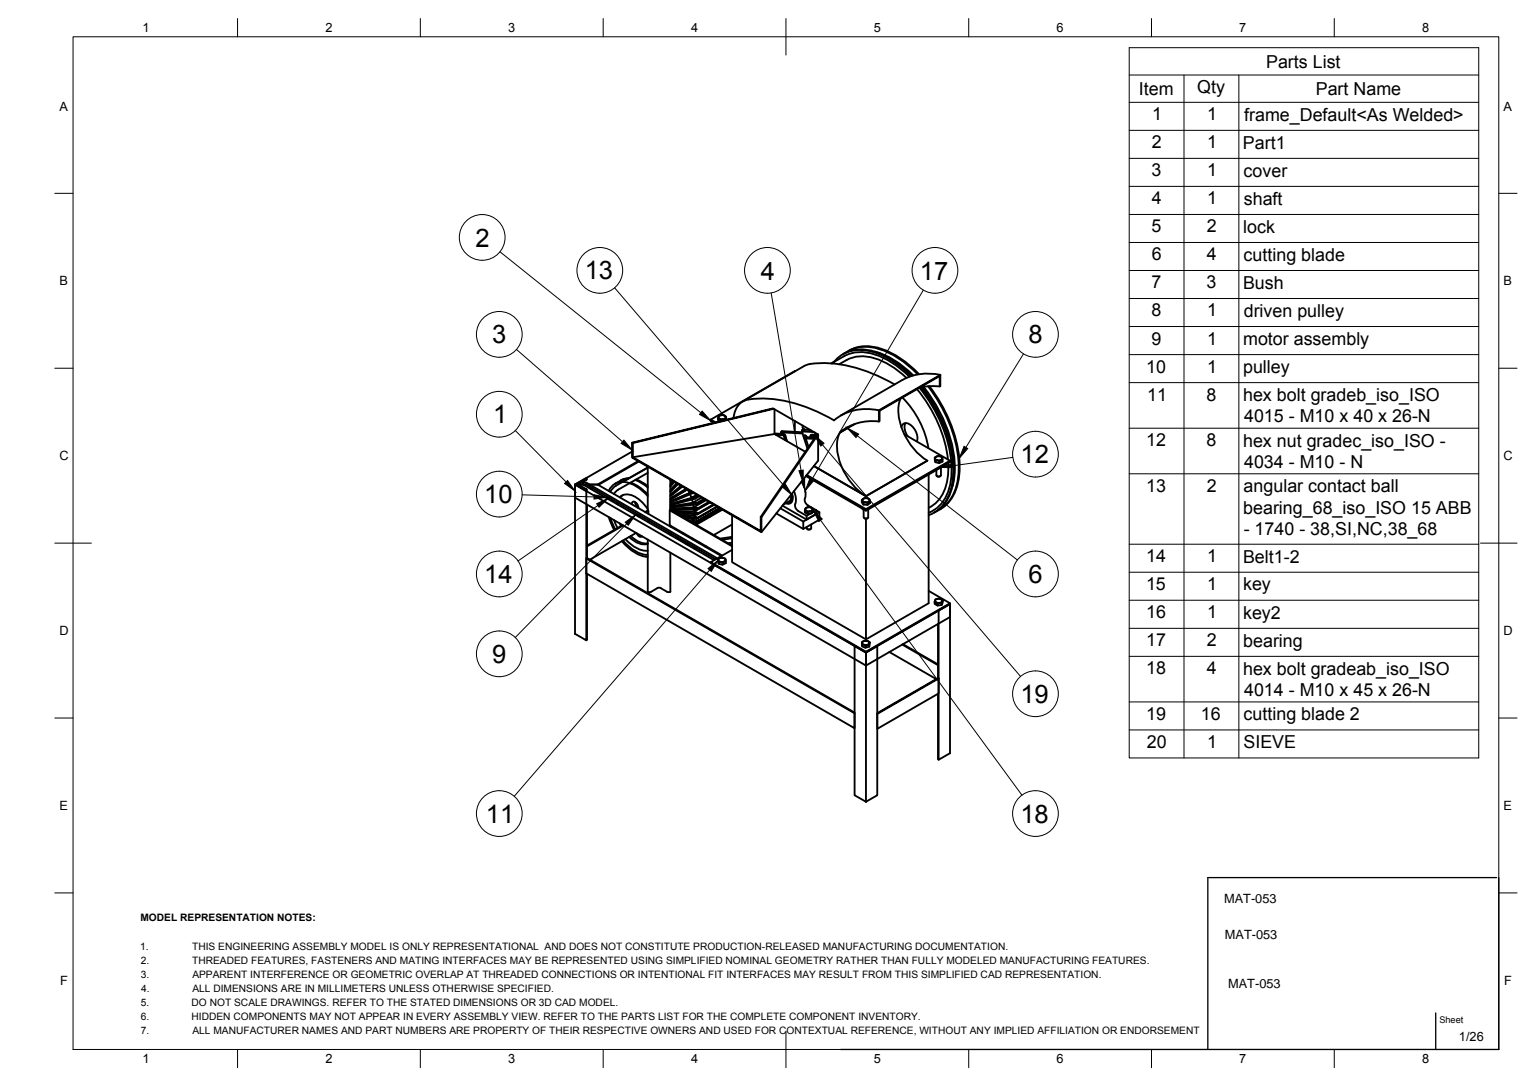
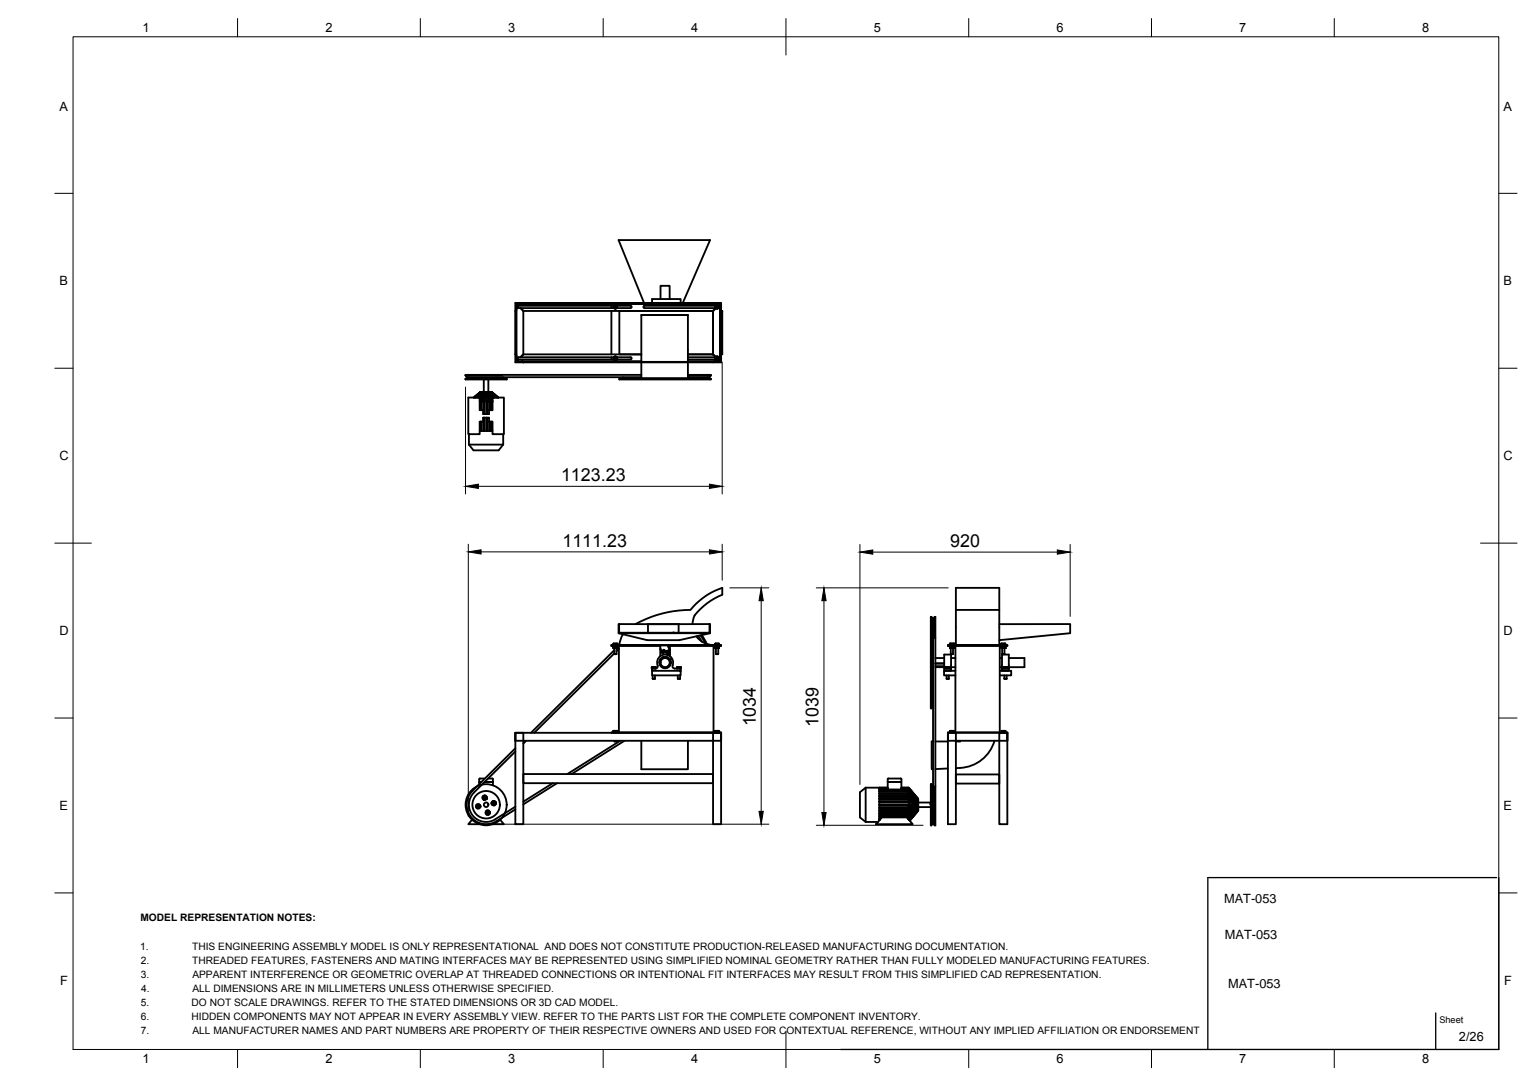
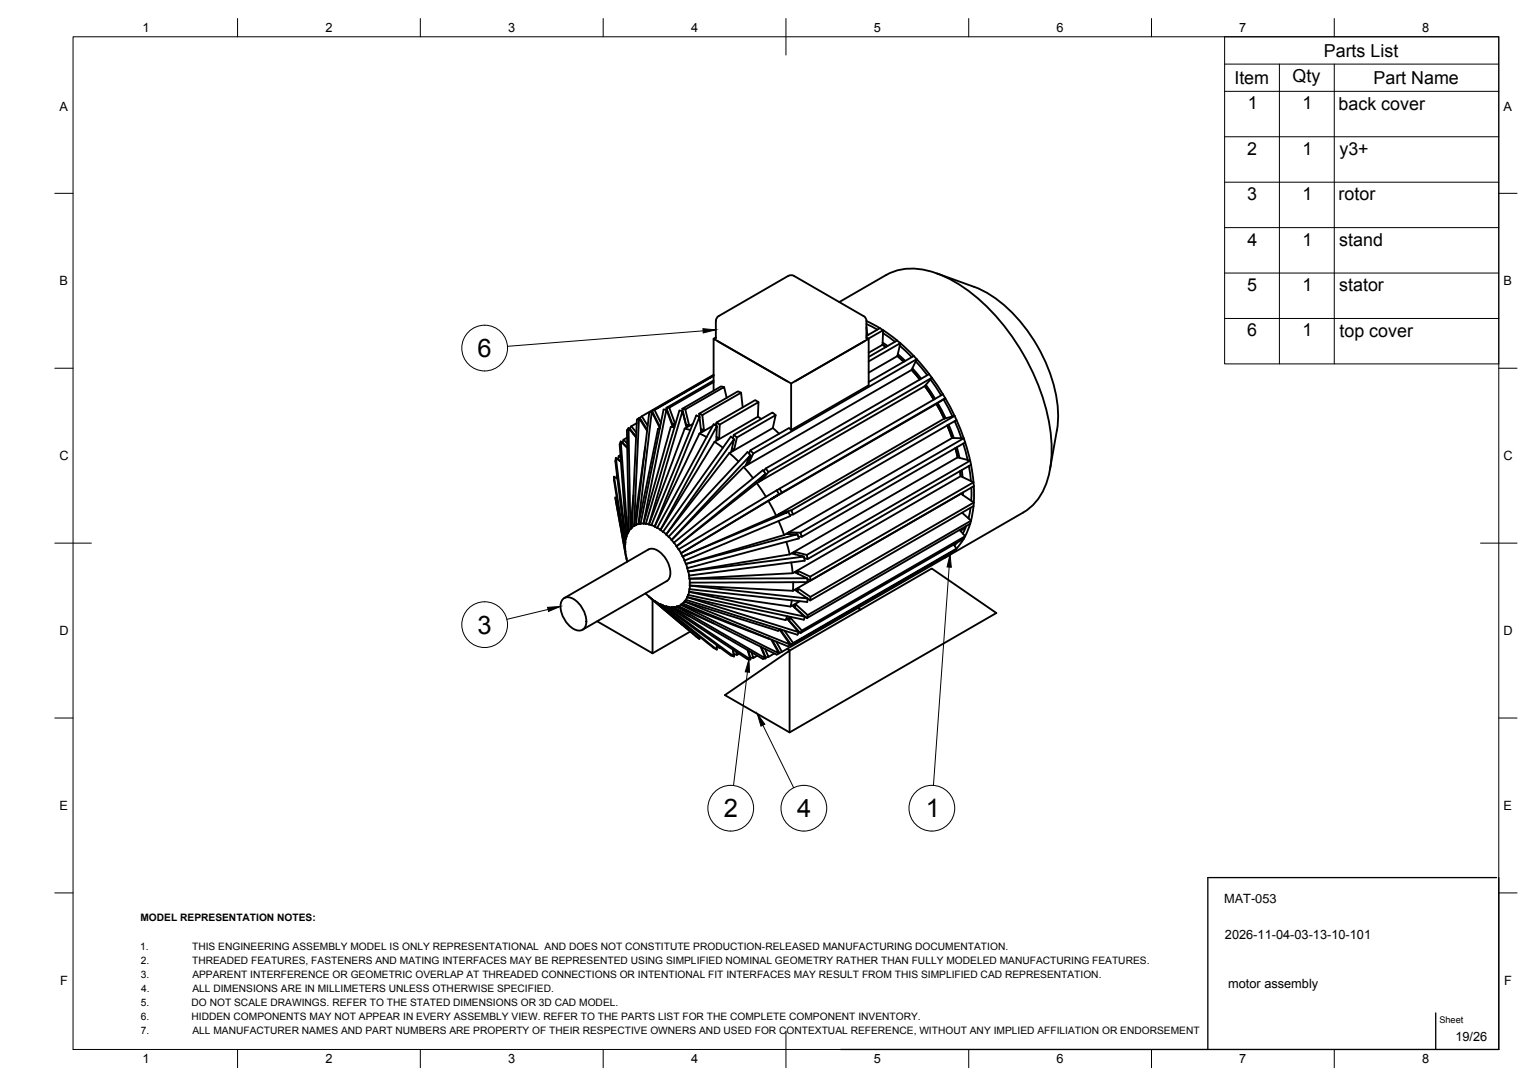
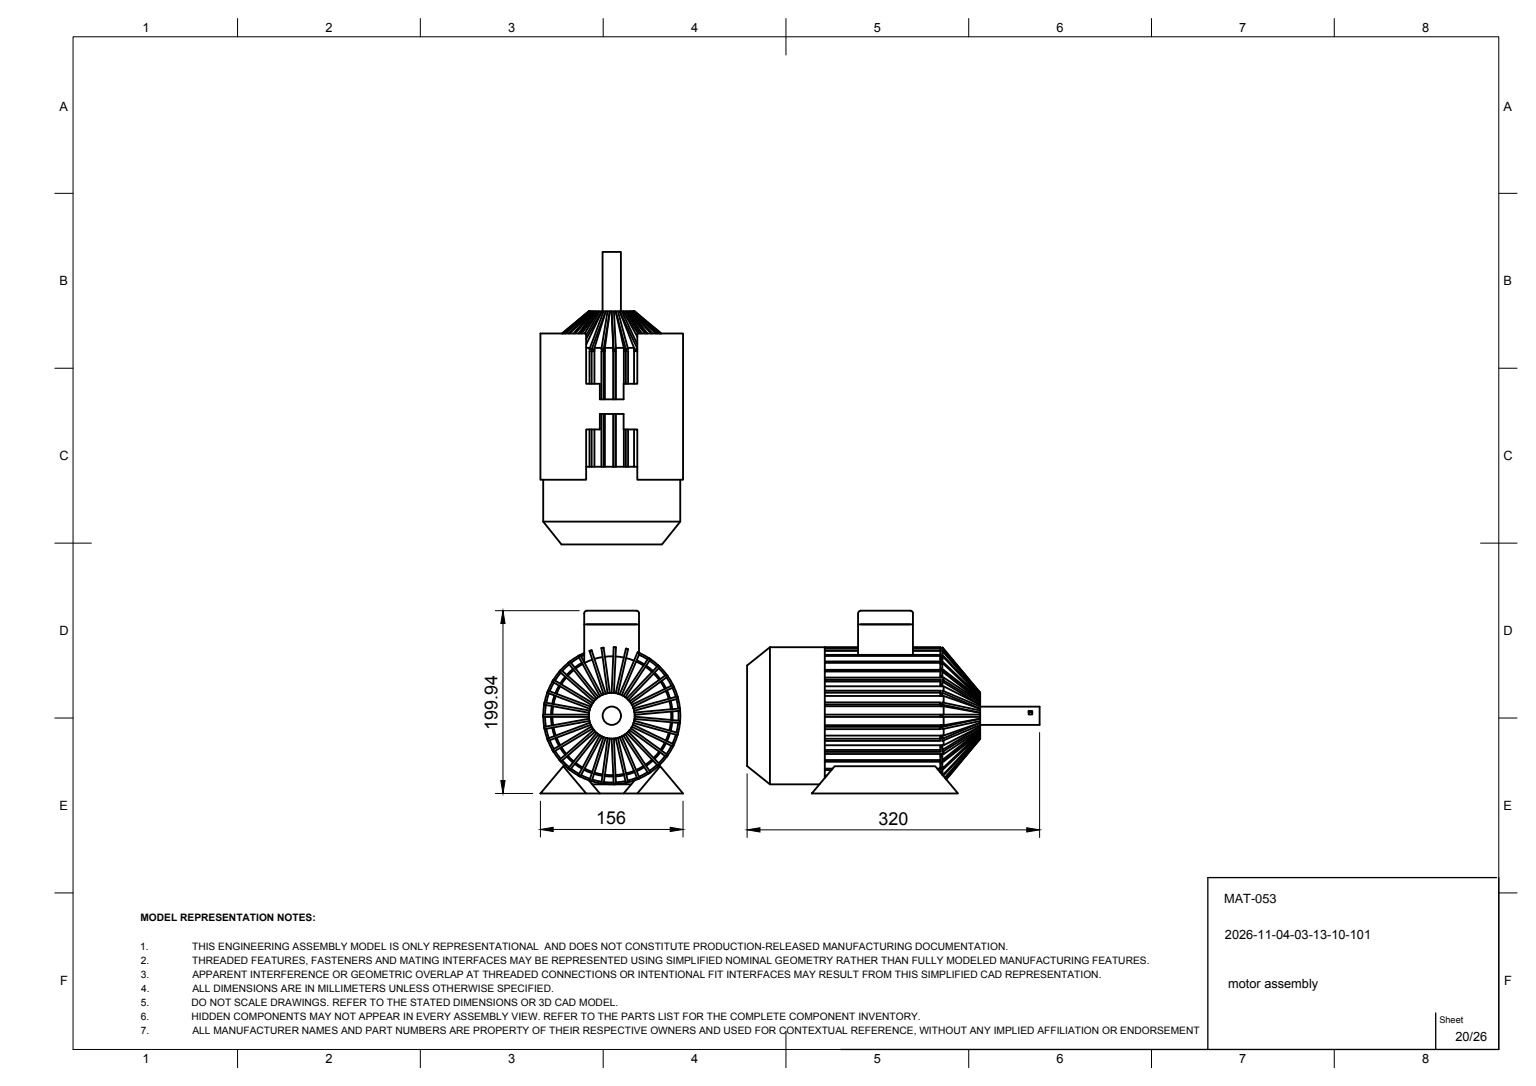
ISO-10303-21;
HEADER;
FILE_DESCRIPTION (('STEP AP214'),
    '1' );
FILE_NAME ('MAT-053',
    '2026-10-10T03:43:58',
    ( '' ),
    ( '' ),
    'SwSTEP 2.0',
    'SolidWorks 2026',
    '' );
FILE_SCHEMA (( 'AUTOMOTIVE_DESIGN' ));
ENDSEC;

DATA;
#1 = CARTESIAN_POINT ( 'NONE',  ( 39.40195752203892710, -170.0000000000000000, -43.11981746542777927 ) ) ;
#2 = ORIENTED_EDGE ( 'NONE', *, *, #57099, .F. ) ;
#3 = EDGE_LOOP ( 'NONE', ( #61802, #31194, #2413, #55543 ) ) ;
#4 = DIRECTION ( 'NONE',  ( 0.000000000000000000, 0.000000000000000000, -1.000000000000000000 ) ) ;
#5 = CARTESIAN_POINT ( 'NONE',  ( -64.61430802170492882, 7.070445451047391749, 170.0000000000000000 ) ) ;
#6 = DIRECTION ( 'NONE',  ( 0.000000000000000000, -1.000000000000000000, 0.000000000000000000 ) ) ;
#7 = CARTESIAN_POINT ( 'NONE',  ( 157.4703587214989113, 58.92748579479261650, -51.12418429913766005 ) ) ;
#8 = CARTESIAN_POINT ( 'NONE',  ( 66.29961816943398389, 13.45804302849872869, 30.55285179693984432 ) ) ;
#9 = VECTOR ( 'NONE', #58697, 1000.000000000000000 ) ;
#10 = ADVANCED_FACE ( 'NONE', ( #11603 ), #16546, .F. ) ;
#11 = CARTESIAN_POINT ( 'NONE',  ( -189.2739965869454579, 107.1373753350176656, -69.83507040438288982 ) ) ;
#12 = EDGE_CURVE ( 'NONE', #54401, #54282, #16885, .T. ) ;
#13 = ORIENTED_EDGE ( 'NONE', *, *, #19324, .T. ) ;
#14 = EDGE_CURVE ( 'NONE', #39203, #23906, #5840, .T. ) ;
#15 = CARTESIAN_POINT ( 'NONE',  ( -95.04120270830171080, 29.25306318840327791, 66.89222559579708616 ) ) ;
#16 = VERTEX_POINT ( 'NONE', #24964 ) ;
#17 = CARTESIAN_POINT ( 'NONE',  ( 0.000000000000000000, 70.00000000000000000, 0.000000000000000000 ) ) ;
#18 = ORIENTED_EDGE ( 'NONE', *, *, #43591, .T. ) ;
#19 = ORIENTED_EDGE ( 'NONE', *, *, #2654, .T. ) ;
#20 = CARTESIAN_POINT ( 'NONE',  ( -124.1095621208148572, 46.52671329146387080, 18.61778521462535352 ) ) ;
#21 = AXIS2_PLACEMENT_3D ( 'NONE', #6201, #49094, #933 ) ;
#22 = CARTESIAN_POINT ( 'NONE',  ( -173.9548930713590380, 88.06040582145359963, 57.70099677511350933 ) ) ;
#23 = CARTESIAN_POINT ( 'NONE',  ( 15.78827728214693416, 6.500811158483328356, 18.17015708224157322 ) ) ;
#24 = ORIENTED_EDGE ( 'NONE', *, *, #58760, .T. ) ;
#25 = CARTESIAN_POINT ( 'NONE',  ( -24.85653282846401879, 8.603185326828743484, 94.99999999999866418 ) ) ;
#26 = CARTESIAN_POINT ( 'NONE',  ( 156.5909039492010209, 56.96742803863246962, 44.40946747225338953 ) ) ;
#27 = CARTESIAN_POINT ( 'NONE',  ( 70.12389542974193546, 15.47520081968151651, 34.86987470614429441 ) ) ;
#28 = DIRECTION ( 'NONE',  ( -1.000000000000000000, -1.850550996349095901E-16, -1.228197773518735191E-20 ) ) ;
#29 = PLANE ( 'NONE',  #12068 ) ;
#30 = DIRECTION ( 'NONE',  ( -0.000000000000000000, 1.000000000000000000, -0.000000000000000000 ) ) ;
#31 = CARTESIAN_POINT ( 'NONE',  ( -23.93880457192868860, 8.479983864459173404, 37.95612845895288956 ) ) ;
#32 = CARTESIAN_POINT ( 'NONE',  ( -142.0084862216822614, 59.34995487985342066, -68.57895708802404044 ) ) ;
#33 = ORIENTED_EDGE ( 'NONE', *, *, #68760, .T. ) ;
#34 = AXIS2_PLACEMENT_3D ( 'NONE', #2299, #49415, #17054 ) ;
#35 = FACE_BOUND ( 'NONE', #6574, .T. ) ;
#36 = CARTESIAN_POINT ( 'NONE',  ( 0.000000000000000000, 0.000000000000000000, 0.000000000000000000 ) ) ;
#37 = CARTESIAN_POINT ( 'NONE',  ( -180.0154536325057677, 96.73346874014741559, 68.13326579958136620 ) ) ;
#38 = CARTESIAN_POINT ( 'NONE',  ( 110.2429982417149432, 28.88204397445230853, -89.61153874658103291 ) ) ;
#39 = CARTESIAN_POINT ( 'NONE',  ( 133.8566784816069344, 41.42467568809808398, 29.51034083899533300 ) ) ;
#40 = CARTESIAN_POINT ( 'NONE',  ( 0.000000000000000000, 0.000000000000000000, 170.0000000000000000 ) ) ;
#41 = DIRECTION ( 'NONE',  ( -1.001915251000354105E-14, 1.000000000000000000, 5.551115123135531297E-17 ) ) ;
#42 = CARTESIAN_POINT ( 'NONE',  ( 110.0000000000000284, 21.42428528562853174, 5.000000000000004441 ) ) ;
#43 = CARTESIAN_POINT ( 'NONE',  ( -78.66644367742111399, 22.32174330031318732, -88.80455181264524356 ) ) ;
#44 = CARTESIAN_POINT ( 'NONE',  ( 70.02892116572940040, 14.40944430928136377, 13.13782541409767646 ) ) ;
#45 = CARTESIAN_POINT ( 'NONE',  ( 161.7048274740120917, 61.01946783654758377, 3.857278696179094801 ) ) ;
#46 = CARTESIAN_POINT ( 'NONE',  ( 92.21252738308859875, 22.47457138983956426, -21.50906452630309929 ) ) ;
#47 = ORIENTED_EDGE ( 'NONE', *, *, #8300, .T. ) ;
#48 = EDGE_CURVE ( 'NONE', #37583, #44986, #40434, .T. ) ;
#49 = CARTESIAN_POINT ( 'NONE',  ( 447.3372781065085633, 399.9999999999998863, 113.5502958579881891 ) ) ;
#50 = ORIENTED_EDGE ( 'NONE', *, *, #39637, .T. ) ;
#51 = CARTESIAN_POINT ( 'NONE',  ( -21.95369412746239846, -11.95973721106846455, 0.000000000000000000 ) ) ;
#52 = ORIENTED_EDGE ( 'NONE', *, *, #19951, .T. ) ;
#53 = CARTESIAN_POINT ( 'NONE',  ( -125.8938041572051105, 46.49392987655495091, 45.61994787315711619 ) ) ;
#54 = CARTESIAN_POINT ( 'NONE',  ( 114.5134543485688710, 32.02763527597250715, 84.62599922377962969 ) ) ;
#55 = CARTESIAN_POINT ( 'NONE',  ( 39.40195752203891999, 9.424259417798147354, -8.775266874964067654 ) ) ;
#56 = CARTESIAN_POINT ( 'NONE',  ( 66.73594759725092729, 13.56641407806656829, -9.859353299932527293 ) ) ;
#57 = AXIS2_PLACEMENT_3D ( 'NONE', #19183, #8994, #35375 ) ;
#58 = CARTESIAN_POINT ( 'NONE',  ( 135.6793972494602656, 43.71805072851429941, -50.81300272974607424 ) ) ;
#59 = PRODUCT_DEFINITION_SHAPE ( 'NONE', 'NONE',  #69636 ) ;
#60 = CARTESIAN_POINT ( 'NONE',  ( 208.3163574534978295, 113.2160455531247152, -90.93580564839912483 ) ) ;
#61 = CYLINDRICAL_SURFACE ( 'NONE', #28597, 10.00000000000000000 ) ;
#62 = CARTESIAN_POINT ( 'NONE',  ( -125.8938041572051389, -170.0000000000000000, -96.10280507916131398 ) ) ;
#63 = ORIENTED_EDGE ( 'NONE', *, *, #15028, .F. ) ;
#64 = ORIENTED_EDGE ( 'NONE', *, *, #47335, .F. ) ;
#65 = EDGE_CURVE ( 'NONE', #33282, #48266, #62999, .T. ) ;
#66 = CARTESIAN_POINT ( 'NONE',  ( 35.66087318222937341, 8.964867769223225480, 57.73931627539139555 ) ) ;
#67 = VECTOR ( 'NONE', #58761, 1000.000000000000000 ) ;
#68 = CARTESIAN_POINT ( 'NONE',  ( 178.1321887506117889, 77.08201292995904907, 83.59636689041089141 ) ) ;
#69 = DIRECTION ( 'NONE',  ( -0.000000000000000000, 1.000000000000000000, -0.000000000000000000 ) ) ;
#70 = EDGE_CURVE ( 'NONE', #25573, #51909, #66497, .T. ) ;
#71 = B_SPLINE_CURVE_WITH_KNOTS ( 'NONE', 3,
 ( #62149, #40352, #67112, #40690, #61801, #51606, #19236, #61465, #13288, #2379, #13619, #2725 ),
 .UNSPECIFIED., .F., .F.,
 ( 4, 2, 2, 2, 2, 4 ),
 ( 0.01013073868447747147, 0.01266158667236432465, 0.01519243466025117784, 0.01645785865419460356, 0.01772328264813802928, 0.02025413063602488073 ),
 .UNSPECIFIED. ) ;
#72 = EDGE_CURVE ( 'NONE', #9244, #1149, #61881, .T. ) ;
#73 = PRODUCT_DEFINITION_CONTEXT ( 'detailed design', #24706, 'design' ) ;
#74 = VECTOR ( 'NONE', #64267, 1000.000000000000000 ) ;
#75 = CARTESIAN_POINT ( 'NONE',  ( 70.16127872101215246, 15.48516972826856097, -94.59315289484993627 ) ) ;
#76 = ORIENTED_EDGE ( 'NONE', *, *, #47792, .F. ) ;
#77 = DIRECTION ( 'NONE',  ( 1.000000000000000000, 0.000000000000000000, -0.000000000000000000 ) ) ;
#78 = CARTESIAN_POINT ( 'NONE',  ( 188.5653887627528036, 88.01608521313129074, -17.48984807395640573 ) ) ;
#79 = CARTESIAN_POINT ( 'NONE',  ( -82.93267503967653909, 23.99263498936122829, -9.597822780125905950 ) ) ;
#80 =( NAMED_UNIT ( * ) PLANE_ANGLE_UNIT ( ) SI_UNIT ( $, .RADIAN. ) );
#81 = CARTESIAN_POINT ( 'NONE',  ( -20.55634918610396866, 36.11269837220808654, 0.000000000000000000 ) ) ;
#82 = CARTESIAN_POINT ( 'NONE',  ( 157.4703587214989398, 58.92748579479258808, 17.56491688178971700 ) ) ;
#83 = LINE ( 'NONE', #53188, #15134 ) ;
#84 = CYLINDRICAL_SURFACE ( 'NONE', #8226, 7.500000000000020428 ) ;
#85 = CARTESIAN_POINT ( 'NONE',  ( 164.6598737201887275, 64.78038692612516058, 61.54778376556991759 ) ) ;
#86 = ORIENTED_EDGE ( 'NONE', *, *, #42856, .F. ) ;
#87 = CARTESIAN_POINT ( 'NONE',  ( -190.6985136298601731, 109.1272424661242582, -95.00000000000133582 ) ) ;
#88 = CARTESIAN_POINT ( 'NONE',  ( 91.11019107624156277, 22.06959540317787827, -37.30231510556647123 ) ) ;
#89 = CARTESIAN_POINT ( 'NONE',  ( 152.8373718734504791, 55.38925997611393370, 69.67201452546140672 ) ) ;
#90 = FACE_OUTER_BOUND ( 'NONE', #51593, .T. ) ;
#91 = CARTESIAN_POINT ( 'NONE',  ( 0.000000000000000000, 0.000000000000000000, 25.00000000000007816 ) ) ;
#92 = CARTESIAN_POINT ( 'NONE',  ( -10.98306470837134796, 8.126405184847016017, 84.49408135793621000 ) ) ;
#93 = ORIENTED_EDGE ( 'NONE', *, *, #10645, .F. ) ;
#94 = EDGE_CURVE ( 'NONE', #10885, #49715, #23914, .T. ) ;
#95 =( NAMED_UNIT ( * ) SI_UNIT ( $, .STERADIAN. ) SOLID_ANGLE_UNIT ( ) );
#96 = DIRECTION ( 'NONE',  ( -0.000000000000000000, -0.000000000000000000, -1.000000000000000000 ) ) ;
#97 = ORIENTED_EDGE ( 'NONE', *, *, #54272, .F. ) ;
#98 = ORIENTED_EDGE ( 'NONE', *, *, #55652, .T. ) ;
#99 = CARTESIAN_POINT ( 'NONE',  ( -67.57266509268163190, 32.54128043381644630, 0.000000000000000000 ) ) ;
#100 = DIRECTION ( 'NONE',  ( -0.000000000000000000, -0.000000000000000000, -1.000000000000000000 ) ) ;
#101 = CARTESIAN_POINT ( 'NONE',  ( 88.52077179907878701, 21.14145351760140557, -62.90458105059150284 ) ) ;
#102 = ORIENTED_EDGE ( 'NONE', *, *, #65193, .F. ) ;
#103 = CARTESIAN_POINT ( 'NONE',  ( -55.05276343752909440, 14.68156374112638929, -77.06087458892358200 ) ) ;
#104 = VECTOR ( 'NONE', #8568, 1000.000000000000000 ) ;
#105 = CARTESIAN_POINT ( 'NONE',  ( 32.29989959354725926, 7.591763852038291738, -13.85219865116375715 ) ) ;
#106 = CARTESIAN_POINT ( 'NONE',  ( 179.4227152810058215, 78.36166152262364903, -51.05095273083168905 ) ) ;
#107 = CARTESIAN_POINT ( 'NONE',  ( 163.7460705099150573, 62.69983247170010543, 94.71987145728411406 ) ) ;
#108 = CARTESIAN_POINT ( 'NONE',  ( 93.85846834761630930, 22.01563781856521018, 35.19885710929750644 ) ) ;
#109 = CIRCLE ( 'NONE', #32707, 5.400000000000001243 ) ;
#110 = ORIENTED_EDGE ( 'NONE', *, *, #20958, .T. ) ;
#111 = VECTOR ( 'NONE', #38454, 1000.000000000000000 ) ;
#112 = VECTOR ( 'NONE', #58293, 1000.000000000000000 ) ;
#113 = CARTESIAN_POINT ( 'NONE',  ( -52.68206656346369954, 15.09776187114412593, -35.59673745022761437 ) ) ;
#114 = CARTESIAN_POINT ( 'NONE',  ( -78.66644367742111399, 23.39876645725287219, 30.41820113967310490 ) ) ;
#115 = CARTESIAN_POINT ( 'NONE',  ( 8.683910719548897816, 7.383368463746306176, 35.09835667283063998 ) ) ;
#116 = DIRECTION ( 'NONE',  ( 0.000000000000000000, 0.000000000000000000, -1.000000000000000000 ) ) ;
#117 = DIRECTION ( 'NONE',  ( 1.000000000000000000, 0.000000000000000000, 0.000000000000000000 ) ) ;
#119 = ORIENTED_EDGE ( 'NONE', *, *, #42370, .F. ) ;
#118 = DIRECTION ( 'NONE',  ( -0.000000000000000000, -0.000000000000000000, -1.000000000000000000 ) ) ;
#120 = ORIENTED_EDGE ( 'NONE', *, *, #64988, .T. ) ;
#121 = ORIENTED_EDGE ( 'NONE', *, *, #21419, .T. ) ;
#122 = CARTESIAN_POINT ( 'NONE',  ( -8.314575874103555364, 6.922894809783093351, -23.57352014148017361 ) ) ;
#123 = CARTESIAN_POINT ( 'NONE',  ( -50.51700111023804851, 13.51182830536852997, 43.81040306015482599 ) ) ;
#124 = CYLINDRICAL_SURFACE ( 'NONE', #1949, 5.000000000000000888 ) ;
#125 = DIRECTION ( 'NONE',  ( 0.000000000000000000, 0.000000000000000000, 1.000000000000000000 ) ) ;
#126 = EDGE_CURVE ( 'NONE', #42836, #57574, #45365, .T. ) ;
#127 = CARTESIAN_POINT ( 'NONE',  ( -38.16652041892307778, 11.81761816422915068, 61.20925241452948740 ) ) ;
#128 = EDGE_CURVE ( 'NONE', #3129, #8050, #2808, .T. ) ;
#129 = CARTESIAN_POINT ( 'NONE',  ( -13.47517652744366856, 8.334971000693553123, -11.11675483260547104 ) ) ;
#130 = CARTESIAN_POINT ( 'NONE',  ( 150.0973882686025433, 52.13852366454154463, -69.06737236800162805 ) ) ;
#131 = CARTESIAN_POINT ( 'NONE',  ( 15.78827728214693416, 6.500811158483328356, -8.674393508222097537 ) ) ;
#132 = ORIENTED_EDGE ( 'NONE', *, *, #17716, .F. ) ;
#133 = EDGE_CURVE ( 'NONE', #13308, #45468, #35156, .T. ) ;
#134 = CARTESIAN_POINT ( 'NONE',  ( -154.7998111145352595, 68.80117179139330119, -47.64861779563037203 ) ) ;
#135 = VERTEX_POINT ( 'NONE', #41824 ) ;
#136 = EDGE_LOOP ( 'NONE', ( #56580, #33322, #40120, #29529 ) ) ;
#137 = CARTESIAN_POINT ( 'NONE',  ( 69.49112875363887554, 15.30845942322122433, -20.16820370593556433 ) ) ;
#138 = EDGE_CURVE ( 'NONE', #47203, #54495, #17035, .T. ) ;
#139 = CARTESIAN_POINT ( 'NONE',  ( -82.93126516400695891, 25.07709093823493873, -48.78959211302295529 ) ) ;
#140 = DIRECTION ( 'NONE',  ( 0.000000000000000000, 0.000000000000000000, 1.000000000000000000 ) ) ;
#141 = CARTESIAN_POINT ( 'NONE',  ( -156.9900125991010498, 72.16580261738670288, 10.78960814776965549 ) ) ;
#142 = CARTESIAN_POINT ( 'NONE',  ( 187.2465631085773907, 85.06582225041681511, -39.42042871992538267 ) ) ;
#143 = CARTESIAN_POINT ( 'NONE',  ( 6.400000000000000355, -9.237604307034018802, 3.355146209984123968E-17 ) ) ;
#144 = CARTESIAN_POINT ( 'NONE',  ( -156.4614183966801022, 71.67647641794694380, 89.09562039624624674 ) ) ;
#145 = VERTEX_POINT ( 'NONE', #21389 ) ;
#146 = EDGE_LOOP ( 'NONE', ( #8104, #20994, #5292, #47649 ) ) ;
#147 = EDGE_LOOP ( 'NONE', ( #11378, #55449, #7164, #22820 ) ) ;
#148 = CARTESIAN_POINT ( 'NONE',  ( -156.0209085498132140, 71.27066046086522988, -19.22534495811094146 ) ) ;
#149 = CARTESIAN_POINT ( 'NONE',  ( 87.02964419696034781, 20.62171628682589386, -89.51066537983909654 ) ) ;
#150 = EDGE_CURVE ( 'NONE', #43731, #18069, #10487, .T. ) ;
#151 = ADVANCED_FACE ( 'NONE', ( #63279 ), #44007, .T. ) ;
#152 = VECTOR ( 'NONE', #5107, 1000.000000000000000 ) ;
#153 = CARTESIAN_POINT ( 'NONE',  ( -33.83558513595455253, 9.996963989836508802, 71.67202419627825805 ) ) ;
#154 = CARTESIAN_POINT ( 'NONE',  ( -150.3791492925491013, 64.92185203933371440, -22.93029560069632211 ) ) ;
#155 = ORIENTED_EDGE ( 'NONE', *, *, #38259, .F. ) ;
#156 = CARTESIAN_POINT ( 'NONE',  ( 187.0788993276711665, 86.37277723143233743, 59.13935664661273250 ) ) ;
#157 = CARTESIAN_POINT ( 'NONE',  ( -155.1302201283146758, 69.09929365814132041, 70.03478143350771745 ) ) ;
#158 = VECTOR ( 'NONE', #16298, 1000.000000000000000 ) ;
#159 = CARTESIAN_POINT ( 'NONE',  ( 16.28382582968306380, 7.523443033994204221, 18.17015708224156612 ) ) ;
#160 = CARTESIAN_POINT ( 'NONE',  ( 104.7147873368644753, 26.40702926859708199, 15.35902160271893813 ) ) ;
#161 = CARTESIAN_POINT ( 'NONE',  ( -124.9927180788553756, 45.90286323198618845, 18.73480619198342367 ) ) ;
#162 = CARTESIAN_POINT ( 'NONE',  ( -444.4229916354184979, 394.6798985497181889, -128.9497041420121093 ) ) ;
#163 = CARTESIAN_POINT ( 'NONE',  ( 21.25987915030395925, 6.737472588634914494, 59.22395766586208055 ) ) ;
#164 = CARTESIAN_POINT ( 'NONE',  ( 46.39999999999999858, 0.000000000000000000, 0.000000000000000000 ) ) ;
#165 = CARTESIAN_POINT ( 'NONE',  ( 8.336882341125875229, 6.376438415325264231, -70.84698747820850429 ) ) ;
#166 = AXIS2_PLACEMENT_3D ( 'NONE', #40198, #13463, #28960 ) ;
#167 = CIRCLE ( 'NONE', #18114, 65.36598343705435354 ) ;
#168 = VERTEX_POINT ( 'NONE', #37218 ) ;
#169 = CARTESIAN_POINT ( 'NONE',  ( 123.4242852856285566, 6.000000000000000000, 0.000000000000000000 ) ) ;
#170 = APPLICATION_PROTOCOL_DEFINITION ( 'draft international standard', 'automotive_design', 1998, #58366 ) ;
#171 = VECTOR ( 'NONE', #36242, 1000.000000000000000 ) ;
#172 = DIRECTION ( 'NONE',  ( -0.000000000000000000, -0.000000000000000000, -1.000000000000000000 ) ) ;
#173 = CARTESIAN_POINT ( 'NONE',  ( 218.0000000000000000, 0.000000000000000000, 0.000000000000000000 ) ) ;
#174 = CARTESIAN_POINT ( 'NONE',  ( 44.34263167748003553, 9.103379693481556956, -75.62813062877941661 ) ) ;
#175 = PLANE ( 'NONE',  #51290 ) ;
#176 = EDGE_LOOP ( 'NONE', ( #13726, #7536, #23044, #10848 ) ) ;
#177 = ORIENTED_EDGE ( 'NONE', *, *, #64499, .T. ) ;
#178 = CARTESIAN_POINT ( 'NONE',  ( -25.48237668717799309, 8.689083390666777262, -11.38912287515594812 ) ) ;
#179 = CARTESIAN_POINT ( 'NONE',  ( 174.1688711713896964, 71.88855623114105242, 93.40745146404465515 ) ) ;
#180 = EDGE_LOOP ( 'NONE', ( #53944, #20596, #29884, #29507 ) ) ;
#181 = ORIENTED_EDGE ( 'NONE', *, *, #66204, .T. ) ;
#182 = CARTESIAN_POINT ( 'NONE',  ( 116.0773578185793582, 31.67580513411752463, 59.21665166914974776 ) ) ;
#183 = ORIENTED_EDGE ( 'NONE', *, *, #3422, .F. ) ;
#184 = CARTESIAN_POINT ( 'NONE',  ( 115.0485321076020568, 32.28990710985444679, 69.73487632334627051 ) ) ;
#185 = LINE ( 'NONE', #21641, #40737 ) ;
#186 = CARTESIAN_POINT ( 'NONE',  ( 140.2058232509808704, 46.59155168125935376, 67.87841396662895477 ) ) ;
#187 = LINE ( 'NONE', #36804, #20712 ) ;
#188 = CARTESIAN_POINT ( 'NONE',  ( -98.46684543088103680, 30.88557736720387936, 44.48182062113936297 ) ) ;
#189 = CARTESIAN_POINT ( 'NONE',  ( 88.98408042523108463, 20.23787745328938570, -50.44636354873872364 ) ) ;
#190 = CARTESIAN_POINT ( 'NONE',  ( -31.11269837220812207, -26.11269837220801193, 0.000000000000000000 ) ) ;
#191 = ORIENTED_EDGE ( 'NONE', *, *, #28368, .T. ) ;
#192 = VERTEX_POINT ( 'NONE', #42509 ) ;
#193 =( BOUNDED_CURVE ( )  B_SPLINE_CURVE ( 3, ( #51309, #3119, #36157, #51647 ),
 .UNSPECIFIED., .F., .F. ) 
 B_SPLINE_CURVE_WITH_KNOTS ( ( 4, 4 ),
 ( 0.3396391817068888930, 0.7435323497954801075 ),
 .UNSPECIFIED. ) 
 CURVE ( )  GEOMETRIC_REPRESENTATION_ITEM ( )  RATIONAL_B_SPLINE_CURVE ( ( 1.000000000000000000, 0.9864519964717846090, 0.9864519964717846090, 1.000000000000000000 ) ) 
 REPRESENTATION_ITEM ( '' )  );
#194 = CARTESIAN_POINT ( 'NONE',  ( 0.000000000000000000, 0.000000000000000000, 43.58025477438756212 ) ) ;
#195 = FACE_BOUND ( 'NONE', #48020, .T. ) ;
#196 = CARTESIAN_POINT ( 'NONE',  ( -9.964117946888929822, -64.24592483216726180, 170.0000000000000000 ) ) ;
#197 = CARTESIAN_POINT ( 'NONE',  ( -165.7690020878297616, 80.74028011998674970, -70.56799682258439077 ) ) ;
#199 = ORIENTED_EDGE ( 'NONE', *, *, #29609, .T. ) ;
#198 = CARTESIAN_POINT ( 'NONE',  ( -142.0251973982164202, 58.08401473564112649, -42.89990999809938188 ) ) ;
#200 = DIRECTION ( 'NONE',  ( -0.000000000000000000, -0.000000000000000000, -1.000000000000000000 ) ) ;
#201 = CIRCLE ( 'NONE', #46254, 65.00000000000000000 ) ;
#202 = ORIENTED_EDGE ( 'NONE', *, *, #20149, .F. ) ;
#203 = AXIS2_PLACEMENT_3D ( 'NONE', #23243, #1076, #59454 ) ;
#204 = LINE ( 'NONE', #41148, #41347 ) ;
#205 = DIRECTION ( 'NONE',  ( 0.000000000000000000, 0.000000000000000000, -1.000000000000000000 ) ) ;
#206 = EDGE_CURVE ( 'NONE', #68800, #69210, #4699, .T. ) ;
#207 = AXIS2_PLACEMENT_3D ( 'NONE', #62081, #45913, #12874 ) ;
#208 = CARTESIAN_POINT ( 'NONE',  ( 79.19345177405116942, 17.01649702043280143, -15.46643930101046038 ) ) ;
#209 = CARTESIAN_POINT ( 'NONE',  ( 93.71772995179813392, 21.96265635001558181, -67.70285364061378175 ) ) ;
#210 = CARTESIAN_POINT ( 'NONE',  ( 60.43099056502398980, 12.08801636090767850, -89.86627097950946563 ) ) ;
#211 = EDGE_CURVE ( 'NONE', #44289, #2530, #5891, .T. ) ;
#212 = CARTESIAN_POINT ( 'NONE',  ( -98.69283175933881580, 30.99524616306738878, 4.570732717346438712 ) ) ;
#213 = CARTESIAN_POINT ( 'NONE',  ( -95.63568360745009045, 29.53168204475774417, -72.84711776369148595 ) ) ;
#214 = ORIENTED_EDGE ( 'NONE', *, *, #67051, .T. ) ;
#215 = ORIENTED_EDGE ( 'NONE', *, *, #11970, .T. ) ;
#216 = AXIS2_PLACEMENT_3D ( 'NONE', #62327, #35605, #30325 ) ;
#217 = ADVANCED_FACE ( 'NONE', ( #3847 ), #69303, .F. ) ;
#218 = CARTESIAN_POINT ( 'NONE',  ( 188.2133404574783242, 86.12414067617878288, -68.22339036842659254 ) ) ;
#219 = VECTOR ( 'NONE', #12666, 1000.000000000000000 ) ;
#220 = DIRECTION ( 'NONE',  ( 0.9639628606958550172, -0.2660368455666687892, 0.000000000000000000 ) ) ;
#221 = DIRECTION ( 'NONE',  ( -0.3930250316539278255, 0.9195277725514487965, 0.000000000000000000 ) ) ;
#222 = LINE ( 'NONE', #22031, #68846 ) ;
#223 = CARTESIAN_POINT ( 'NONE',  ( 23.81581464765719502, -7.603089679099516829, 0.000000000000000000 ) ) ;
#224 = CARTESIAN_POINT ( 'NONE',  ( 79.23200707685336397, 17.02828389812517429, 38.47447533467553171 ) ) ;
#225 = CARTESIAN_POINT ( 'NONE',  ( 90.13282190615606737, 1.839221433318906476E-12, 5.000000000000000000 ) ) ;
#226 = CARTESIAN_POINT ( 'NONE',  ( -124.1007047332777944, 46.52282960291164926, 30.82329275154649295 ) ) ;
#227 = CARTESIAN_POINT ( 'NONE',  ( 211.1200456646897123, 115.5868795682033436, 67.43584021203363932 ) ) ;
#228 = ORIENTED_EDGE ( 'NONE', *, *, #68309, .F. ) ;
#229 = DIRECTION ( 'NONE',  ( 0.000000000000000000, 0.04541273895899431562, -0.9989683093773507050 ) ) ;
#230 = EDGE_LOOP ( 'NONE', ( #67792, #13686 ) ) ;
#231 = CARTESIAN_POINT ( 'NONE',  ( -14.76369756425703983, 7.442560416198673146, -40.03899903455366882 ) ) ;
#232 = CARTESIAN_POINT ( 'NONE',  ( -30.00000000000000355, 26.99999999999999289, 12.00000000000000000 ) ) ;
#233 = CARTESIAN_POINT ( 'NONE',  ( 89.87840278991589571, 21.62393877508911899, 57.29260026085291457 ) ) ;
#234 = EDGE_CURVE ( 'NONE', #1187, #8293, #15089, .T. ) ;
#235 = CARTESIAN_POINT ( 'NONE',  ( 150.0433793199863146, 52.09973307442953683, -17.85989976896762244 ) ) ;
#236 = CARTESIAN_POINT ( 'NONE',  ( 31.96192885395475614, 8.569232728322420556, 11.54728592230744688 ) ) ;
#237 = CARTESIAN_POINT ( 'NONE',  ( -94.77890319529970498, 30.24118571794803145, -69.85920485586603945 ) ) ;
#238 = CARTESIAN_POINT ( 'NONE',  ( -44.00727179482512241, -47.83680621839620528, 170.0000000000000000 ) ) ;
#239 = ORIENTED_EDGE ( 'NONE', *, *, #49975, .T. ) ;
#240 = CARTESIAN_POINT ( 'NONE',  ( -52.69240448066584293, -53.30312580971443026, 41.38025477438755928 ) ) ;
#241 = DIRECTION ( 'NONE',  ( -0.000000000000000000, 1.000000000000000000, -0.000000000000000000 ) ) ;
#242 = VERTEX_POINT ( 'NONE', #53046 ) ;
#243 = CARTESIAN_POINT ( 'NONE',  ( 60.63380853769237433, 13.16344960520422092, 57.04161213523420315 ) ) ;
#244 = PRESENTATION_STYLE_ASSIGNMENT (( #27321 ) ) ;
#245 = CARTESIAN_POINT ( 'NONE',  ( -9.524904342798460988, 8.016391612076530393, 3.461975196507860453 ) ) ;
#246 = B_SPLINE_CURVE_WITH_KNOTS ( 'NONE', 3,
 ( #24990, #25339, #47115, #47446, #36574, #58023, #9495, #14429, #20379, #68579, #26018, #52401, #25686, #36915, #46776, #68907, #62260, #42187, #63654, #14763, #4219, #36227, #52729, #30264, #15462, #41848, #9150, #30605, #9841, #46080, #14077, #8811, #4554, #29912, #62955, #67550, #35539, #52058, #68246, #56993, #8460, #20051, #41504, #51371, #3188, #24647, #19349, #57685, #51713, #46422 ),
 .UNSPECIFIED., .F., .F.,
 ( 4, 2, 2, 2, 2, 2, 2, 2, 2, 2, 2, 2, 2, 2, 2, 2, 2, 2, 2, 2, 2, 2, 2, 2, 4 ),
 ( 0.02688458561150007531, 0.02770990876165290578, 0.02853523191180573973, 0.03018587821211139027, 0.03183652451241704429, 0.03266184766256987476, 0.03348717081272270524, 0.03513781711302831068, 0.03678846341333391612, 0.03761378656348669802, 0.03843910971363948686, 0.03926443286379226877, 0.04008975601394505761, 0.04174040231425062836, 0.04256572546440341026, 0.04339104861455619216, 0.04421637176470897407, 0.04504169491486175597, 0.04586701806501453788, 0.04669234121516731978, 0.04834298751547294604, 0.04916831066562572794, 0.04999363381577851678, 0.05164428011608407365, 0.05329492641638964440 ),
 .UNSPECIFIED. ) ;
#247 = CARTESIAN_POINT ( 'NONE',  ( -51.55432476821989951, -3.384920738951192387, 26.66469104408689006 ) ) ;
#248 = CARTESIAN_POINT ( 'NONE',  ( -3.857727530059799737, 6.665032499723453796, 43.98489318319101926 ) ) ;
#249 = CARTESIAN_POINT ( 'NONE',  ( 53.32245423372616244, -37.19594572654634845, 0.000000000000000000 ) ) ;
#250 = CARTESIAN_POINT ( 'NONE',  ( 92.81046075878417412, 22.69711000191779959, 86.64015653787805604 ) ) ;
#251 = ORIENTED_EDGE ( 'NONE', *, *, #47236, .T. ) ;
#252 = VECTOR ( 'NONE', #36887, 999.9999999999998863 ) ;
#253 = DIRECTION ( 'NONE',  ( -9.989315170677463157E-15, 1.000000000000000000, 4.052314039881817428E-15 ) ) ;
#254 = CARTESIAN_POINT ( 'NONE',  ( 63.74253542338309586, -39.54050679744447194, 170.0000000000000000 ) ) ;
#255 = CARTESIAN_POINT ( 'NONE',  ( -3.364862276288897558, 74.92447999059858432, 0.000000000000000000 ) ) ;
#256 = CARTESIAN_POINT ( 'NONE',  ( -104.1393288135077455, 34.86912007524090029, 72.14469141808412189 ) ) ;
#257 = CONTEXT_DEPENDENT_SHAPE_REPRESENTATION ( #15243, #13690 ) ;
#258 = CARTESIAN_POINT ( 'NONE',  ( -131.6253556217205016, 51.61436399519948282, -47.27706506024894395 ) ) ;
#259 = ORIENTED_EDGE ( 'NONE', *, *, #53036, .T. ) ;
#260 = LINE ( 'NONE', #68864, #29041 ) ;
#261 = VECTOR ( 'NONE', #60433, 1000.000000000000000 ) ;
#262 = B_SPLINE_CURVE_WITH_KNOTS ( 'NONE', 3,
 ( #59638, #61313, #13475, #23684, #67303, #64945, #7519, #45827, #34603, #2920, #19089, #8197, #59303, #16738, #39855, #45475, #23348, #40208, #56375, #13139, #2235, #38197, #11115, #12783, #11452, #571, #34245, #7855, #60962, #44791, #54360, #29302, #28970, #1895, #29646, #32580, #50755, #2576 ),
 .UNSPECIFIED., .F., .F.,
 ( 4, 2, 2, 2, 2, 2, 2, 2, 2, 2, 2, 2, 2, 2, 2, 2, 2, 2, 4 ),
 ( 1.430489624538199204E-17, 0.003908178031105532212, 0.005862267046658249312, 0.007816356062210967279, 0.009770445077763688715, 0.01172453409331640842, 0.01270157860109274485, 0.01367862310886907781, 0.01465566761664541424, 0.01563271212442174721, 0.01660975663219808884, 0.01758680113997443048, 0.01954089015552709294, 0.02051793466330344151, 0.02149497917107979009, 0.02344906818663248377, 0.02540315720218518786, 0.02735724621773788501, 0.03126542424884325155 ),
 .UNSPECIFIED. ) ;
#263 = CARTESIAN_POINT ( 'NONE',  ( -1.088326810997878091, 6.545818265928947888, -19.40564166976581006 ) ) ;
#264 =( NAMED_UNIT ( * ) SI_UNIT ( $, .STERADIAN. ) SOLID_ANGLE_UNIT ( ) );
#265 = VECTOR ( 'NONE', #25443, 1000.000000000000000 ) ;
#266 = CARTESIAN_POINT ( 'NONE',  ( -153.9421172888672231, 68.03407102037994036, 85.85448269280857403 ) ) ;
#267 = CIRCLE ( 'NONE', #18213, 25.00000000000000000 ) ;
#268 = CARTESIAN_POINT ( 'NONE',  ( 141.3445468829085030, 46.13338528906589886, 37.51412908544414648 ) ) ;
#269 = ORIENTED_EDGE ( 'NONE', *, *, #50441, .F. ) ;
#270 = CARTESIAN_POINT ( 'NONE',  ( 0.06730325657897140434, -1.557442666625558525, -8.000000000000000000 ) ) ;
#271 = CARTESIAN_POINT ( 'NONE',  ( 82.73618382051373032, 19.18661415186669217, 16.78260538844248728 ) ) ;
#272 = CARTESIAN_POINT ( 'NONE',  ( 164.4761273435911733, 64.62485394454745347, 7.335242511255203546 ) ) ;
#273 = CARTESIAN_POINT ( 'NONE',  ( -34.39099631177280969, 10.00000000000000000, -33.00000000000000000 ) ) ;
#274 = AXIS2_PLACEMENT_3D ( 'NONE', #4193, #20028, #68878 ) ;
#275 = VERTEX_POINT ( 'NONE', #57999 ) ;
#276 = EDGE_CURVE ( 'NONE', #33643, #59523, #9303, .T. ) ;
#277 = CARTESIAN_POINT ( 'NONE',  ( 174.9099402067542997, 73.96774984027638311, 67.91937322613915740 ) ) ;
#278 = ORIENTED_EDGE ( 'NONE', *, *, #36224, .T. ) ;
#279 = CARTESIAN_POINT ( 'NONE',  ( -104.5730787903383003, 33.96058035148152499, -35.35797728948608665 ) ) ;
#280 = CARTESIAN_POINT ( 'NONE',  ( -20.63749999999999574, 0.000000000000000000, 0.000000000000000000 ) ) ;
#282 = ORIENTED_EDGE ( 'NONE', *, *, #4760, .T. ) ;
#281 = CARTESIAN_POINT ( 'NONE',  ( 150.4542242713869200, 53.63744268572192198, 12.72894179764149847 ) ) ;
#283 = CARTESIAN_POINT ( 'NONE',  ( 157.4703587214989113, 57.65129005721576760, 29.40946747225336466 ) ) ;
#284 = CARTESIAN_POINT ( 'NONE',  ( 0.000000000000000000, 0.000000000000000000, 0.000000000000000000 ) ) ;
#285 = CYLINDRICAL_SURFACE ( 'NONE', #42881, 7.500000000000020428 ) ;
#286 = ORIENTED_EDGE ( 'NONE', *, *, #5924, .T. ) ;
#287 = LINE ( 'NONE', #43194, #50190 ) ;
#288 = EDGE_CURVE ( 'NONE', #56752, #64051, #11518, .T. ) ;
#289 = ADVANCED_FACE ( 'NONE', ( #32988 ), #17141, .F. ) ;
#290 = CYLINDRICAL_SURFACE ( 'NONE', #39876, 21.02500000000000213 ) ;
#291 = CARTESIAN_POINT ( 'NONE',  ( 21.98745393275193294, 71.71550996510526943, 170.0000000000000000 ) ) ;
#292 = CARTESIAN_POINT ( 'NONE',  ( -37.79823708645147917, 10.72197716414928870, -73.64561661794576253 ) ) ;
#293 = ORIENTED_EDGE ( 'NONE', *, *, #14607, .T. ) ;
#294 = ORIENTED_EDGE ( 'NONE', *, *, #30490, .T. ) ;
#295 = VERTEX_POINT ( 'NONE', #1681 ) ;
#296 = VECTOR ( 'NONE', #1863, 1000.000000000000000 ) ;
#297 = EDGE_CURVE ( 'NONE', #67311, #11610, #65085, .T. ) ;
#298 = DIRECTION ( 'NONE',  ( 0.000000000000000000, 1.000000000000000000, 0.000000000000000000 ) ) ;
#299 = DIRECTION ( 'NONE',  ( 1.000000000000000000, 1.024558601614476894E-14, -9.899298618516476860E-15 ) ) ;
#300 = FACE_OUTER_BOUND ( 'NONE', #57072, .T. ) ;
#301 = VECTOR ( 'NONE', #7610, 1000.000000000000000 ) ;
#302 = DIRECTION ( 'NONE',  ( -0.000000000000000000, 1.000000000000000000, -0.000000000000000000 ) ) ;
#303 = CARTESIAN_POINT ( 'NONE',  ( 70.49702515974807682, 14.53327724265703402, 91.86127284075526234 ) ) ;
#304 = FACE_OUTER_BOUND ( 'NONE', #28790, .T. ) ;
#305 = DIRECTION ( 'NONE',  ( 0.000000000000000000, 0.000000000000000000, 1.000000000000000000 ) ) ;
#307 = CYLINDRICAL_SURFACE ( 'NONE', #24291, 7.500000000000013323 ) ;
#306 = AXIS2_PLACEMENT_3D ( 'NONE', #41965, #53186, #58819 ) ;
#308 = VERTEX_POINT ( 'NONE', #33352 ) ;
#309 = LINE ( 'NONE', #37951, #56611 ) ;
#310 = ORIENTED_EDGE ( 'NONE', *, *, #16110, .F. ) ;
#311 = AXIS2_PLACEMENT_3D ( 'NONE', #60560, #44374, #50365 ) ;
#312 = CARTESIAN_POINT ( 'NONE',  ( 211.5066273949820186, 116.1727691518062073, -73.86407362358771422 ) ) ;
#313 = B_SPLINE_CURVE_WITH_KNOTS ( 'NONE', 3,
 ( #22788, #6611, #12241, #1333, #32645, #43534, #50221, #60425, #55133, #1685, #44592, #50913, #45283, #9047, #13622, #19590, #7670, #2728, #34407, #66764, #61804, #18557, #55849, #61471, #62513, #3420, #35784, #41053, #18214, #24879, #2383, #14325, #29453, #29115, #40694, #57233, #40009, #13291, #30495, #29808, #39665, #46316, #50565, #44937 ),
 .UNSPECIFIED., .F., .F.,
 ( 4, 2, 2, 2, 2, 2, 2, 2, 2, 2, 2, 2, 2, 2, 2, 2, 2, 2, 2, 2, 2, 4 ),
 ( 0.02895403260893131964, 0.03071603688922221187, 0.03247804116951310410, 0.03424004544980399634, 0.03600204973009488857, 0.03776405401038577386, 0.03864505615053119569, 0.03952605829067662446, 0.04040706043082205323, 0.04128806257096747506, 0.04216906471111290383, 0.04305006685125832566, 0.04393106899140375443, 0.04481207113154918320, 0.04569307327169461197, 0.04657407541184004074, 0.04745507755198546257, 0.04833607969213089134, 0.05009808397242175582, 0.05186008825271262723, 0.05362209253300349171, 0.05714610109358524842 ),
 .UNSPECIFIED. ) ;
#314 = EDGE_CURVE ( 'NONE', #536, #3478, #33702, .T. ) ;
#315 = DIRECTION ( 'NONE',  ( 0.000000000000000000, 0.000000000000000000, -1.000000000000000000 ) ) ;
#316 = CARTESIAN_POINT ( 'NONE',  ( 63.01563776193091826, -170.0000000000000000, -89.40979201309708913 ) ) ;
#317 = CARTESIAN_POINT ( 'NONE',  ( -124.1095621208148714, 46.52671329146387791, 72.30688639555273767 ) ) ;
#318 = CARTESIAN_POINT ( 'NONE',  ( 22.62427395637551086, 7.823784829753564374, 34.41962451814575275 ) ) ;
#319 = CIRCLE ( 'NONE', #56472, 10.00000000000000178 ) ;
#320 = CARTESIAN_POINT ( 'NONE',  ( 442.3372781065083359, 370.0000000000043201, 108.5502958579838833 ) ) ;
#321 = EDGE_CURVE ( 'NONE', #69231, #19186, #17084, .T. ) ;
#322 = ADVANCED_FACE ( 'NONE', ( #635 ), #43872, .F. ) ;
#323 = DIRECTION ( 'NONE',  ( 0.000000000000000000, 0.000000000000000000, -1.000000000000000000 ) ) ;
#324 = ORIENTED_EDGE ( 'NONE', *, *, #68515, .T. ) ;
#325 = CARTESIAN_POINT ( 'NONE',  ( 65.13282190615461786, 1.839221433318906476E-12, 5.000000000000000000 ) ) ;
#326 = FACE_OUTER_BOUND ( 'NONE', #64859, .T. ) ;
#327 = VERTEX_POINT ( 'NONE', #60057 ) ;
#328 = ORIENTED_EDGE ( 'NONE', *, *, #4703, .T. ) ;
#329 = FACE_OUTER_BOUND ( 'NONE', #61642, .T. ) ;
#330 = CARTESIAN_POINT ( 'NONE',  ( 444.9999999999999432, 225.0000000000000000, -2.000000000000000000 ) ) ;
#331 = CARTESIAN_POINT ( 'NONE',  ( 46.85361596800672146, 10.51535167202354693, 38.39853853478529544 ) ) ;
#332 = CARTESIAN_POINT ( 'NONE',  ( -27.70562707895080123, 9.007984652865424380, 58.03756985863584106 ) ) ;
#333 = CARTESIAN_POINT ( 'NONE',  ( -142.3393481102175713, 58.33014244976924090, 9.152932767281312110 ) ) ;
#334 = ORIENTED_EDGE ( 'NONE', *, *, #37544, .F. ) ;
#335 = ORIENTED_EDGE ( 'NONE', *, *, #3794, .F. ) ;
#336 = CARTESIAN_POINT ( 'NONE',  ( -127.6881387055492354, 48.89937523111242257, 30.83417093567260636 ) ) ;
#337 = ORIENTED_EDGE ( 'NONE', *, *, #57085, .T. ) ;
#338 = CARTESIAN_POINT ( 'NONE',  ( 0.000000000000000000, 6.123233995736767268E-16, -5.000000000000000888 ) ) ;
#339 = CARTESIAN_POINT ( 'NONE',  ( 0.08285530294364991388, 1.570896314703519092, -8.000000000000000000 ) ) ;
#340 = CARTESIAN_POINT ( 'NONE',  ( 55.61382797299289393, 11.07686102552912644, 62.92265474384031876 ) ) ;
#341 = LINE ( 'NONE', #41886, #16088 ) ;
#342 = CARTESIAN_POINT ( 'NONE',  ( -29.96307832726302678, 10.37242130382201921, -89.14992242554669133 ) ) ;
#343 = CARTESIAN_POINT ( 'NONE',  ( -188.8754233303960746, 108.3048424661242137, -95.00000000000133582 ) ) ;
#344 = VECTOR ( 'NONE', #34891, 1000.000000000000000 ) ;
#345 = CARTESIAN_POINT ( 'NONE',  ( 0.000000000000000000, 0.000000000000000000, 380.0000000000000000 ) ) ;
#346 = ORIENTED_EDGE ( 'NONE', *, *, #17053, .T. ) ;
#347 = VERTEX_POINT ( 'NONE', #65712 ) ;
#348 = CARTESIAN_POINT ( 'NONE',  ( 46.76173513940489812, 58.63736118510233553, 0.000000000000000000 ) ) ;
#349 = DIRECTION ( 'NONE',  ( -1.000000000000000000, 0.000000000000000000, 0.000000000000000000 ) ) ;
#350 = VECTOR ( 'NONE', #31052, 1000.000000000000000 ) ;
#351 = CARTESIAN_POINT ( 'NONE',  ( 0.000000000000000000, 0.000000000000000000, 170.0000000000000000 ) ) ;
#352 = DIRECTION ( 'NONE',  ( -0.7071067811865543451, -7.105427357601001070E-15, -0.7071067811865408004 ) ) ;
#353 = CARTESIAN_POINT ( 'NONE',  ( 70.26722489419890394, 14.47234958177329567, 35.33543539248424281 ) ) ;
#354 = VECTOR ( 'NONE', #29148, 1000.000000000000000 ) ;
#355 = ORIENTED_EDGE ( 'NONE', *, *, #33274, .T. ) ;
#356 = EDGE_CURVE ( 'NONE', #53205, #30991, #32306, .T. ) ;
#357 = AXIS2_PLACEMENT_3D ( 'NONE', #51385, #66883, #65837 ) ;
#358 = CARTESIAN_POINT ( 'NONE',  ( 80.30232379693107703, 17.35837133860831472, 6.332652209273762267 ) ) ;
#359 = CARTESIAN_POINT ( 'NONE',  ( -65.13282190615095146, -1.847197903505587038E-12, 5.000000000000000000 ) ) ;
#360 = VECTOR ( 'NONE', #38064, 1000.000000000000000 ) ;
#361 = CARTESIAN_POINT ( 'NONE',  ( -71.97434903038468690, 19.88430675376529067, 34.49547489334918993 ) ) ;
#362 = ORIENTED_EDGE ( 'NONE', *, *, #55841, .F. ) ;
#363 = EDGE_CURVE ( 'NONE', #35105, #14663, #10362, .T. ) ;
#364 = VECTOR ( 'NONE', #18440, 1000.000000000000000 ) ;
#365 = AXIS2_PLACEMENT_3D ( 'NONE', #2334, #1994, #61414 ) ;
#366 = VERTEX_POINT ( 'NONE', #38615 ) ;
#367 = LINE ( 'NONE', #1073, #48782 ) ;
#368 = CARTESIAN_POINT ( 'NONE',  ( -179.5178913137217194, 94.54206947403389449, 69.12039320224292283 ) ) ;
#369 = FACE_OUTER_BOUND ( 'NONE', #27784, .T. ) ;
#370 = ORIENTED_EDGE ( 'NONE', *, *, #14642, .F. ) ;
#371 = CARTESIAN_POINT ( 'NONE',  ( -20.55634918610396866, 31.11269837220809009, 0.000000000000000000 ) ) ;
#372 = ADVANCED_FACE ( 'NONE', ( #59703 ), #54424, .T. ) ;
#373 = EDGE_CURVE ( 'NONE', #61321, #29458, #45223, .T. ) ;
#374 = DIRECTION ( 'NONE',  ( -0.000000000000000000, 1.000000000000000000, -0.000000000000000000 ) ) ;
#375 = CARTESIAN_POINT ( 'NONE',  ( 150.9184679586219033, 52.73111408630721542, 40.56872817287094790 ) ) ;
#376 = CARTESIAN_POINT ( 'NONE',  ( 68.63585058221465829, 15.08566240483130727, 32.32217050974968942 ) ) ;
#377 = FACE_OUTER_BOUND ( 'NONE', #67584, .T. ) ;
#378 = FACE_OUTER_BOUND ( 'NONE', #48491, .T. ) ;
#379 = CYLINDRICAL_SURFACE ( 'NONE', #33876, 5.000000000000170530 ) ;
#380 = EDGE_CURVE ( 'NONE', #35096, #37085, #27704, .T. ) ;
#381 = CARTESIAN_POINT ( 'NONE',  ( -23.95096213915836358, 8.481591526885939203, 38.20520003450658209 ) ) ;
#382 = CARTESIAN_POINT ( 'NONE',  ( -144.7530445311634537, 61.54314312182906122, -74.96293479194935117 ) ) ;
#383 = VERTEX_POINT ( 'NONE', #55130 ) ;
#384 = FACE_BOUND ( 'NONE', #4499, .T. ) ;
#385 = CARTESIAN_POINT ( 'NONE',  ( -2.190131154568200511, 6.589492063460817839, -74.71788358249716566 ) ) ;
#386 = CARTESIAN_POINT ( 'NONE',  ( -179.8926034784145997, 96.58272071140105197, 61.93007157060646506 ) ) ;
#387 = CARTESIAN_POINT ( 'NONE',  ( 0.1317522424472117037, 1.959574484719860621, 8.000000000000000000 ) ) ;
#388 = CARTESIAN_POINT ( 'NONE',  ( -118.9668643994983483, 43.27909474462860828, -39.52642719331304022 ) ) ;
#389 = CARTESIAN_POINT ( 'NONE',  ( -85.66184035008926401, 26.20110535976566268, 13.79000864225666589 ) ) ;
#390 = DIRECTION ( 'NONE',  ( 1.000000000000000000, 0.000000000000000000, 0.000000000000000000 ) ) ;
#391 = CARTESIAN_POINT ( 'NONE',  ( 43.69793136154977020, -27.56441338823224640, 26.66469104408688651 ) ) ;
#392 = CARTESIAN_POINT ( 'NONE',  ( -5.888165822225391643, 7.780336669456525023, -8.823856489658712832 ) ) ;
#393 = CARTESIAN_POINT ( 'NONE',  ( 67.55134213333077753, 13.77030723107740506, 4.475137186144926282 ) ) ;
#394 = CARTESIAN_POINT ( 'NONE',  ( 159.6593397521790791, 59.37286298965126718, 2.877594456964315039 ) ) ;
#395 = CARTESIAN_POINT ( 'NONE',  ( 39.81822037269075309, 9.478622457786777034, -89.30891864635511013 ) ) ;
#396 = ORIENTED_EDGE ( 'NONE', *, *, #36645, .T. ) ;
#397 = AXIS2_PLACEMENT_3D ( 'NONE', #30126, #55451, #24841 ) ;
#398 = CARTESIAN_POINT ( 'NONE',  ( -38.54712373114178092, 11.89174538567466932, 8.428869490921766072 ) ) ;
#399 = ORIENTED_EDGE ( 'NONE', *, *, #56528, .T. ) ;
#400 = LINE ( 'NONE', #38040, #43022 ) ;
#401 = ORIENTED_EDGE ( 'NONE', *, *, #69148, .T. ) ;
#402 = CARTESIAN_POINT ( 'NONE',  ( 85.67165909753201447, 20.15791549876375655, -62.71191053415395089 ) ) ;
#403 = AXIS2_PLACEMENT_3D ( 'NONE', #39353, #38653, #43213 ) ;
#404 = CARTESIAN_POINT ( 'NONE',  ( 110.9260829236403936, 30.30898941444543837, 83.30420403083246583 ) ) ;
#405 = CARTESIAN_POINT ( 'NONE',  ( -142.0084862216822330, 59.34995487985343487, 65.64379586429438973 ) ) ;
#406 = CARTESIAN_POINT ( 'NONE',  ( 70.25990036603482736, 14.47042233282419765, -14.41847716369608001 ) ) ;
#407 = ADVANCED_FACE ( 'NONE', ( #49850 ), #23142, .T. ) ;
#408 = ADVANCED_FACE ( 'NONE', ( #27013 ), #48440, .F. ) ;
#409 = CARTESIAN_POINT ( 'NONE',  ( -31.43908319763710679, 10.61114334766715928, -35.31719736520183517 ) ) ;
#410 = CARTESIAN_POINT ( 'NONE',  ( -53.14657859411972396, 15.21831473227210196, -62.30310801584961666 ) ) ;
#411 = VECTOR ( 'NONE', #777, 999.9999999999998863 ) ;
#412 = CARTESIAN_POINT ( 'NONE',  ( 6.800000000000000711, 0.000000000000000000, 0.000000000000000000 ) ) ;
#413 = EDGE_CURVE ( 'NONE', #65743, #4867, #71, .T. ) ;
#414 = CARTESIAN_POINT ( 'NONE',  ( -118.4106078162223668, 42.93830006159888768, -14.99940221450364319 ) ) ;
#415 = ORIENTED_EDGE ( 'NONE', *, *, #36605, .F. ) ;
#416 = CIRCLE ( 'NONE', #39744, 5.000000000000004441 ) ;
#417 = VERTEX_POINT ( 'NONE', #18553 ) ;
#418 = AXIS2_PLACEMENT_3D ( 'NONE', #49039, #43423, #65240 ) ;
#419 = CARTESIAN_POINT ( 'NONE',  ( 33.31166872005967150, 8.707041209322234465, 59.87445300413067173 ) ) ;
#420 = DIRECTION ( 'NONE',  ( -0.8118923937861950435, -0.5838071093367415143, 0.000000000000000000 ) ) ;
#421 = VECTOR ( 'NONE', #35144, 1000.000000000000000 ) ;
#422 = CARTESIAN_POINT ( 'NONE',  ( -172.3038663181180823, 87.72015621195184565, -7.867406574286301080 ) ) ;
#423 = AXIS2_PLACEMENT_3D ( 'NONE', #15656, #48667, #10364 ) ;
#424 = LINE ( 'NONE', #15226, #9320 ) ;
#425 = ORIENTED_EDGE ( 'NONE', *, *, #19954, .T. ) ;
#426 = CARTESIAN_POINT ( 'NONE',  ( 283.3080539574502268, 21.67699184046404781, 3.763267418054555780 ) ) ;
#427 = CARTESIAN_POINT ( 'NONE',  ( 187.2296622856351860, 86.53808614709454616, -21.18754879403664404 ) ) ;
#428 = CARTESIAN_POINT ( 'NONE',  ( 212.1669304543882788, 119.0398299474539243, 9.162465270872496959 ) ) ;
#429 =( NAMED_UNIT ( * ) SI_UNIT ( $, .STERADIAN. ) SOLID_ANGLE_UNIT ( ) );
#430 = CARTESIAN_POINT ( 'NONE',  ( -20.55634918610403261, 0.000000000000000000, 2.000000000000000000 ) ) ;
#431 = CARTESIAN_POINT ( 'NONE',  ( 111.9975424824652634, 296.0000000000000000, 529.9060149868646477 ) ) ;
#432 = CARTESIAN_POINT ( 'NONE',  ( -149.5074843970971301, 64.17983161892345834, -76.65738112195568021 ) ) ;
#433 = CARTESIAN_POINT ( 'NONE',  ( 105.1691917892558905, 21.96211590856092144, 1.300061720562576406 ) ) ;
#434 = DIRECTION ( 'NONE',  ( 3.687791819402438921E-18, 3.525890001671295931E-18, -1.000000000000000000 ) ) ;
#435 = APPLICATION_CONTEXT ( 'automotive_design' ) ;
#436 = ORIENTED_EDGE ( 'NONE', *, *, #28005, .T. ) ;
#437 = DIRECTION ( 'NONE',  ( 0.000000000000000000, 0.000000000000000000, 1.000000000000000000 ) ) ;
#438 = LINE ( 'NONE', #10639, #37259 ) ;
#439 = CARTESIAN_POINT ( 'NONE',  ( -47.94536219817735656, 13.92422159065987408, 62.21613247434213179 ) ) ;
#440 = DIRECTION ( 'NONE',  ( 0.000000000000000000, 1.000000000000000000, 0.000000000000000000 ) ) ;
#441 = CYLINDRICAL_SURFACE ( 'NONE', #8272, 7.500000000000013323 ) ;
#442 = DIRECTION ( 'NONE',  ( -0.000000000000000000, 1.000000000000000000, -0.000000000000000000 ) ) ;
#443 = B_SPLINE_CURVE_WITH_KNOTS ( 'NONE', 3,
 ( #41840, #54634, #27027, #15107, #63647, #41496, #62947, #36907, #10161, #9488, #16130, #30946, #14755, #4211, #4546, #53400, #25676, #4886, #47438, #68897, #47107, #68570, #47789, #42521, #63298, #15455, #36566, #20724, #31293, #26353, #52719, #58345, #5235, #53749, #63976, #9834, #21078, #15790, #26011, #42179, #37233, #69251, #58684 ),
 .UNSPECIFIED., .F., .F.,
 ( 4, 2, 2, 2, 2, 2, 2, 2, 2, 2, 2, 1, 2, 2, 2, 2, 2, 2, 2, 2, 2, 4 ),
 ( 0.02515559250233022348, 0.02674001423437969566, 0.02753222510040442828, 0.02832443596642916436, 0.02990885769847856715, 0.03149327943052796647, 0.03307770116257736925, 0.03386991202860207412, 0.03466212289462677898, 0.03624654462667613319, 0.03703875549270080336, 0.03783096635872546659, 0.03862317722475013676, 0.03941538809077479999, 0.04099980982282412645, 0.04258423155487345985, 0.04337644242089812308, 0.04416865328692278631, 0.04575307501897205031, 0.04733749675102130738, 0.04892191848307056445, 0.05050634021511982846 ),
 .UNSPECIFIED. ) ;
#444 = EDGE_LOOP ( 'NONE', ( #35988, #44492, #55517, #13641 ) ) ;
#445 = CARTESIAN_POINT ( 'NONE',  ( 62.53328835682435738, 12.56090025569836932, 2.968410348757586803 ) ) ;
#446 = CARTESIAN_POINT ( 'NONE',  ( -58.10608953386396536, 15.52134062643864176, 57.80724698423686903 ) ) ;
#447 = ORIENTED_EDGE ( 'NONE', *, *, #56885, .F. ) ;
#448 = EDGE_LOOP ( 'NONE', ( #53193, #25137, #33362, #38103 ) ) ;
#449 = EDGE_CURVE ( 'NONE', #11991, #8386, #8441, .T. ) ;
#450 = VECTOR ( 'NONE', #55912, 1000.000000000000000 ) ;
#451 = PLANE ( 'NONE',  #68993 ) ;
#452 = LINE ( 'NONE', #27883, #8566 ) ;
#453 = CARTESIAN_POINT ( 'NONE',  ( 91.11019107624153435, 22.06959540317787116, -64.14686569603014732 ) ) ;
#454 = VERTEX_POINT ( 'NONE', #23494 ) ;
#455 = CARTESIAN_POINT ( 'NONE',  ( 15.55634918610400241, -15.55634918610406103, 85.00100000000000477 ) ) ;
#456 = COLOUR_RGB ( '',0.7921568627450980005, 0.8196078431372548767, 0.9333333333333333481 ) ;
#457 = CARTESIAN_POINT ( 'NONE',  ( 35.44781468922820977, 7.928097401423690016, -22.65291149958800432 ) ) ;
#458 = CARTESIAN_POINT ( 'NONE',  ( 173.8576514579035290, 72.97529922124003576, -41.69686196060180094 ) ) ;
#459 = CARTESIAN_POINT ( 'NONE',  ( 158.7623625177564008, 58.66148101564576223, 83.18577911345145992 ) ) ;
#460 = VECTOR ( 'NONE', #45689, 1000.000000000000000 ) ;
#461 = CARTESIAN_POINT ( 'NONE',  ( -4.337405327940998312, -24.62086340933521456, 0.000000000000000000 ) ) ;
#462 = AXIS2_PLACEMENT_3D ( 'NONE', #325, #22133, #54117 ) ;
#463 = EDGE_CURVE ( 'NONE', #12143, #43378, #39662, .T. ) ;
#464 = ORIENTED_EDGE ( 'NONE', *, *, #60521, .F. ) ;
#465 = AXIS2_PLACEMENT_3D ( 'NONE', #65616, #23741, #6150 ) ;
#466 = CARTESIAN_POINT ( 'NONE',  ( -51.34542473642584071, 14.75635007918829800, -49.24053308027907860 ) ) ;
#467 = CIRCLE ( 'NONE', #25205, 10.00000000000000000 ) ;
#468 = DIRECTION ( 'NONE',  ( -0.000000000000000000, -0.000000000000000000, -1.000000000000000000 ) ) ;
#469 = EDGE_CURVE ( 'NONE', #64523, #66077, #7997, .T. ) ;
#470 = CARTESIAN_POINT ( 'NONE',  ( 13.83281508467570653, 7.452090093180185448, 44.77217603759554265 ) ) ;
#471 = LINE ( 'NONE', #21919, #18113 ) ;
#472 = DIRECTION ( 'NONE',  ( -1.000000000000000000, 0.000000000000000000, 0.000000000000000000 ) ) ;
#473 = EDGE_CURVE ( 'NONE', #23927, #8984, #16634, .T. ) ;
#474 = DIRECTION ( 'NONE',  ( 0.000000000000000000, 0.000000000000000000, 1.000000000000000000 ) ) ;
#476 = VERTEX_POINT ( 'NONE', #20615 ) ;
#475 = CARTESIAN_POINT ( 'NONE',  ( -59.42430146430388049, -27.22983999535795618, 41.38025477438755928 ) ) ;
#477 = ORIENTED_EDGE ( 'NONE', *, *, #56695, .T. ) ;
#478 = ORIENTED_EDGE ( 'NONE', *, *, #43254, .F. ) ;
#479 = CARTESIAN_POINT ( 'NONE',  ( -14.32120159453990027, 7.401444311907543039, -19.83056408198577003 ) ) ;
#480 = CARTESIAN_POINT ( 'NONE',  ( -49.11825192196926082, 13.17012322555986970, 42.42977472503392988 ) ) ;
#481 = DIRECTION ( 'NONE',  ( 0.000000000000000000, 0.000000000000000000, 1.000000000000000000 ) ) ;
#482 = FACE_OUTER_BOUND ( 'NONE', #35633, .T. ) ;
#483 = ADVANCED_BREP_SHAPE_REPRESENTATION ( '', ( #63157, #66832 ), #16381 ) ;
#484 = CARTESIAN_POINT ( 'NONE',  ( -31.93169728792083362, 10.69234447276976852, 72.06100499665291181 ) ) ;
#485 = CARTESIAN_POINT ( 'NONE',  ( -15.32584732649904247, 8.506915958926388299, -15.58511460959460315 ) ) ;
#486 = CARTESIAN_POINT ( 'NONE',  ( 152.8430172091323698, 54.14068524174424368, -76.37591427044367265 ) ) ;
#487 = CARTESIAN_POINT ( 'NONE',  ( 16.28371206594635368, 6.516665886438622657, -8.674393508222101090 ) ) ;
#488 = ORIENTED_EDGE ( 'NONE', *, *, #3364, .T. ) ;
#489 = LINE ( 'NONE', #22994, #3698 ) ;
#490 = ORIENTED_EDGE ( 'NONE', *, *, #33090, .F. ) ;
#491 = ORIENTED_EDGE ( 'NONE', *, *, #35579, .F. ) ;
#492 = CARTESIAN_POINT ( 'NONE',  ( -417.6627218934913230, 179.4906275429376308, 113.5502958579881749 ) ) ;
#493 = DIRECTION ( 'NONE',  ( -2.921639538487254261E-16, -1.134144525784205431E-35, -1.000000000000000000 ) ) ;
#494 = FACE_OUTER_BOUND ( 'NONE', #26933, .T. ) ;
#495 = CARTESIAN_POINT ( 'NONE',  ( 110.2429982417149574, 29.99119854320843714, -9.077886975189997543 ) ) ;
#496 = LINE ( 'NONE', #54649, #32650 ) ;
#497 = CARTESIAN_POINT ( 'NONE',  ( 7.533997733928855745, 64.93035244659017735, 43.58025477438756212 ) ) ;
#498 = EDGE_CURVE ( 'NONE', #7475, #40883, #67262, .T. ) ;
#499 = DIRECTION ( 'NONE',  ( 1.000000000000000000, 0.000000000000000000, 0.000000000000000000 ) ) ;
#500 = ORIENTED_EDGE ( 'NONE', *, *, #39553, .F. ) ;
#501 = ORIENTED_EDGE ( 'NONE', *, *, #47379, .F. ) ;
#503 = ORIENTED_EDGE ( 'NONE', *, *, #6828, .T. ) ;
#502 = B_SPLINE_CURVE_WITH_KNOTS ( 'NONE', 3,
 ( #8600, #68036, #40941, #9632, #31090, #57466, #24771, #51838, #62400, #25125, #24434, #68374, #3652, #67689, #40590, #46555, #46208, #58156, #9974, #30049, #19479, #31425, #41631, #52186, #41293, #62751, #57127, #35321, #14553, #52530, #68700, #19136, #2972, #8939, #19836, #9276, #47243, #4353, #56781, #45874, #67345, #51509, #4005 ),
 .UNSPECIFIED., .F., .F.,
 ( 4, 2, 2, 2, 2, 2, 2, 2, 2, 2, 2, 2, 1, 2, 2, 2, 2, 2, 2, 2, 2, 4 ),
 ( 0.02390068823634509954, 0.02538837671117074798, 0.02613222094858357047, 0.02687606518599639643, 0.02836375366082206570, 0.02985144213564773497, 0.03059528637306056092, 0.03133913061047338688, 0.03282681908529903880, 0.03431450756012469072, 0.03580219603495034264, 0.03654604027236316860, 0.03728988450977599456, 0.03803372874718882052, 0.03877757298460164648, 0.04026526145942728452, 0.04175294993425292950, 0.04324063840907856754, 0.04398448264649139350, 0.04472832688390421252, 0.04621601535872984362, 0.04770370383355547472 ),
 .UNSPECIFIED. ) ;
#504 = AXIS2_PLACEMENT_3D ( 'NONE', #27279, #48719, #561 ) ;
#505 = CARTESIAN_POINT ( 'NONE',  ( -9.763294602873864747, 7.024900256480051119, 18.02051675412898391 ) ) ;
#506 = CARTESIAN_POINT ( 'NONE',  ( 36.98541457540711974, 9.120571655722418569, -36.00309299526835360 ) ) ;
#507 = CARTESIAN_POINT ( 'NONE',  ( -38.89042640463648581, 10.93374343663409043, 65.54896640531427465 ) ) ;
#508 = DIRECTION ( 'NONE',  ( 1.000000000000000000, 0.000000000000000000, 0.000000000000000000 ) ) ;
#509 = EDGE_LOOP ( 'NONE', ( #15892, #23987, #55681, #42144 ) ) ;
#510 = VECTOR ( 'NONE', #66224, 1000.000000000000227 ) ;
#511 = DIRECTION ( 'NONE',  ( -1.000000000000000000, 0.000000000000000000, 0.000000000000000000 ) ) ;
#512 = CARTESIAN_POINT ( 'NONE',  ( -153.1121305730337383, 67.29834700374530598, 71.64627490104848562 ) ) ;
#513 =( NAMED_UNIT ( * ) PLANE_ANGLE_UNIT ( ) SI_UNIT ( $, .RADIAN. ) );
#514 = DIRECTION ( 'NONE',  ( 0.000000000000000000, 0.000000000000000000, -1.000000000000000000 ) ) ;
#515 = FACE_OUTER_BOUND ( 'NONE', #61318, .T. ) ;
#516 = CARTESIAN_POINT ( 'NONE',  ( -125.4433371161043311, 46.19736518073187170, 18.77539728269342589 ) ) ;
#517 = CARTESIAN_POINT ( 'NONE',  ( -84.23431294393863311, 24.52078568147203441, -47.66442666584986654 ) ) ;
#518 = CIRCLE ( 'NONE', #7308, 85.31295361348101380 ) ;
#519 = CARTESIAN_POINT ( 'NONE',  ( 23.23895241123074484, 6.853530908437178049, 63.37105988032327986 ) ) ;
#520 = DIRECTION ( 'NONE',  ( -0.000000000000000000, -0.000000000000000000, -1.000000000000000000 ) ) ;
#521 = CARTESIAN_POINT ( 'NONE',  ( 9.827939172326081163, 6.382931149346556587, -65.28444710517328531 ) ) ;
#522 = VECTOR ( 'NONE', #50610, 1000.000000000000000 ) ;
#523 = AXIS2_PLACEMENT_3D ( 'NONE', #9987, #4698, #14905 ) ;
#524 = ORIENTED_EDGE ( 'NONE', *, *, #39838, .T. ) ;
#525 = DIRECTION ( 'NONE',  ( -1.000000000000000000, -0.000000000000000000, -0.000000000000000000 ) ) ;
#526 = ITEM_DEFINED_TRANSFORMATION ( 'NONE', 'NONE', #57915,  #66832 ) ;
#527 = DIRECTION ( 'NONE',  ( 0.000000000000000000, 0.000000000000000000, -1.000000000000000000 ) ) ;
#528 = FACE_OUTER_BOUND ( 'NONE', #60025, .T. ) ;
#529 = CARTESIAN_POINT ( 'NONE',  ( -737.6000277536880958, -694.2189502691660437, 10.00000000000000000 ) ) ;
#530 = CARTESIAN_POINT ( 'NONE',  ( 56.28782924480456984, 12.23883190161850720, -66.71350665837964300 ) ) ;
#531 = ORIENTED_EDGE ( 'NONE', *, *, #31450, .F. ) ;
#532 = ORIENTED_EDGE ( 'NONE', *, *, #61150, .T. ) ;
#533 = LINE ( 'NONE', #52947, #16766 ) ;
#534 = EDGE_CURVE ( 'NONE', #34523, #68707, #2552, .T. ) ;
#535 = CARTESIAN_POINT ( 'NONE',  ( -45.81425895439360829, -46.10914959592906115, 40.00000000000003553 ) ) ;
#536 = VERTEX_POINT ( 'NONE', #20279 ) ;
#537 = ORIENTED_EDGE ( 'NONE', *, *, #20232, .T. ) ;
#538 = EDGE_CURVE ( 'NONE', #52559, #9895, #28349, .T. ) ;
#539 = DIRECTION ( 'NONE',  ( 1.000000000000000000, 0.000000000000000000, 0.000000000000000000 ) ) ;
#540 = CARTESIAN_POINT ( 'NONE',  ( -442.6627218934913230, 1.665334536937734811E-13, 108.5502958579881749 ) ) ;
#541 = ORIENTED_EDGE ( 'NONE', *, *, #47134, .F. ) ;
#542 = CARTESIAN_POINT ( 'NONE',  ( 112.1009898303695138, 30.86414810229296890, 71.23698475841351296 ) ) ;
#543 = CARTESIAN_POINT ( 'NONE',  ( 104.6431565033459492, 27.47282014102828995, -92.10596456002596710 ) ) ;
#544 = CARTESIAN_POINT ( 'NONE',  ( 6.375108774214766072E-14, 31.11269837220806167, 0.000000000000000000 ) ) ;
#545 = CARTESIAN_POINT ( 'NONE',  ( -71.59086462055189770, 19.75139532313338719, -45.11543775482815732 ) ) ;
#546 = CARTESIAN_POINT ( 'NONE',  ( -96.43148989374459745, 29.90755650959363621, 42.74068095059843841 ) ) ;
#547 = LINE ( 'NONE', #52959, #56357 ) ;
#548 = DIRECTION ( 'NONE',  ( 0.000000000000000000, -0.5000000000000013323, -0.8660254037844379305 ) ) ;
#549 = ORIENTED_EDGE ( 'NONE', *, *, #6542, .T. ) ;
#550 = EDGE_LOOP ( 'NONE', ( #10734, #24849 ) ) ;
#551 = CARTESIAN_POINT ( 'NONE',  ( 110.2429982417149290, 28.88204397445231209, -50.92243756565370916 ) ) ;
#552 = AXIS2_PLACEMENT_3D ( 'NONE', #54276, #10682, #49001 ) ;
#553 = CARTESIAN_POINT ( 'NONE',  ( -2.645453300864630819E-14, -15.55634918610403616, 2.000000000000001776 ) ) ;
#554 = EDGE_CURVE ( 'NONE', #23240, #35650, #11353, .T. ) ;
#555 = DIRECTION ( 'NONE',  ( -0.9909497617679352555, 0.1342332658176522697, 2.500042656554811326E-16 ) ) ;
#556 = ADVANCED_FACE ( 'NONE', ( #43363 ), #46664, .F. ) ;
#557 = DIRECTION ( 'NONE',  ( 0.000000000000000000, 1.000000000000000000, -0.000000000000000000 ) ) ;
#558 = VECTOR ( 'NONE', #9205, 1000.000000000000000 ) ;
#560 = ORIENTED_EDGE ( 'NONE', *, *, #67855, .T. ) ;
#559 = CARTESIAN_POINT ( 'NONE',  ( -142.0062637385109667, 58.06920992247430036, -41.76235797465353272 ) ) ;
#561 = DIRECTION ( 'NONE',  ( 0.000000000000000000, 0.000000000000000000, 1.000000000000000000 ) ) ;
#562 = AXIS2_PLACEMENT_3D ( 'NONE', #30602, #57334, #47443 ) ;
#563 = AXIS2_PLACEMENT_3D ( 'NONE', #26561, #16346, #37803 ) ;
#564 = VERTEX_POINT ( 'NONE', #57576 ) ;
#565 = LINE ( 'NONE', #27282, #37965 ) ;
#566 = DIRECTION ( 'NONE',  ( 0.000000000000000000, 0.000000000000000000, 1.000000000000000000 ) ) ;
#567 = CARTESIAN_POINT ( 'NONE',  ( -65.36598343705435354, 0.000000000000000000, 41.38025477438755928 ) ) ;
#568 = VECTOR ( 'NONE', #4706, 1000.000000000000000 ) ;
#569 = CARTESIAN_POINT ( 'NONE',  ( 137.3958226571046737, 43.60243650158411555, -23.30772740699958945 ) ) ;
#570 = CARTESIAN_POINT ( 'NONE',  ( 91.51282003084288874, 21.14522045960329422, -64.45296707595953478 ) ) ;
#571 = CARTESIAN_POINT ( 'NONE',  ( 198.2545923567585930, 97.90679023593582997, 6.013806333985140640 ) ) ;
#572 = AXIS2_PLACEMENT_3D ( 'NONE', #9018, #25882, #35396 ) ;
#573 = CARTESIAN_POINT ( 'NONE',  ( -99.97541017369788108, 31.62502926470688180, 18.32712433046064149 ) ) ;
#574 = DIRECTION ( 'NONE',  ( -0.000000000000000000, -0.000000000000000000, -1.000000000000000000 ) ) ;
#575 = ORIENTED_EDGE ( 'NONE', *, *, #1852, .T. ) ;
#576 = EDGE_LOOP ( 'NONE', ( #32786, #49878, #58567, #41798 ) ) ;
#577 = CARTESIAN_POINT ( 'NONE',  ( 42.03492317486907837, 8.766487167902370814, 30.38697801852312708 ) ) ;
#578 = CARTESIAN_POINT ( 'NONE',  ( -15.55634918610405748, -15.55634918610400774, 85.00100000000000477 ) ) ;
#579 = LINE ( 'NONE', #5503, #875 ) ;
#580 = CARTESIAN_POINT ( 'NONE',  ( 0.000000000000000000, 0.000000000000000000, 0.000000000000000000 ) ) ;
#581 = DIRECTION ( 'NONE',  ( 0.000000000000000000, 0.000000000000000000, 1.000000000000000000 ) ) ;
#582 = CARTESIAN_POINT ( 'NONE',  ( -76.10382222627278281, 22.43453174720078636, -62.40726938075579255 ) ) ;
#583 = CARTESIAN_POINT ( 'NONE',  ( 544.6745185807129701, 190.0000000000000000, 34.73878747406611467 ) ) ;
#584 = CARTESIAN_POINT ( 'NONE',  ( 46.65974587859241041, 10.48396258569371220, -45.07370360866829628 ) ) ;
#585 = CARTESIAN_POINT ( 'NONE',  ( -422.6627218934914936, 399.9999999999998863, -141.4497041420118535 ) ) ;
#586 = ORIENTED_EDGE ( 'NONE', *, *, #6995, .F. ) ;
#587 = CARTESIAN_POINT ( 'NONE',  ( -29.74902699556085039, 10.33856194202127199, 18.18303581849161077 ) ) ;
#588 = EDGE_LOOP ( 'NONE', ( #66796, #38550, #24211, #31113 ) ) ;
#589 = DIRECTION ( 'NONE',  ( 0.000000000000000000, 0.000000000000000000, -1.000000000000000000 ) ) ;
#590 = DIRECTION ( 'NONE',  ( -0.000000000000000000, -0.000000000000000000, 1.000000000000000000 ) ) ;
#591 = LINE ( 'NONE', #22043, #68889 ) ;
#592 = CARTESIAN_POINT ( 'NONE',  ( 151.1607415860635513, 52.90668588398087024, -20.86606007747752400 ) ) ;
#593 = CARTESIAN_POINT ( 'NONE',  ( 3.000000000000002665, 0.000000000000000000, 0.000000000000000000 ) ) ;
#594 = CARTESIAN_POINT ( 'NONE',  ( -4.613603609465552147, 74.86839895266042788, 43.58025477438756923 ) ) ;
#595 = CARTESIAN_POINT ( 'NONE',  ( 107.3013380801408800, 395.0000000000065938, -128.9497041420121093 ) ) ;
#596 = CARTESIAN_POINT ( 'NONE',  ( 208.5494659193436462, 111.7747784805681164, 83.93795935829461996 ) ) ;
#597 = CARTESIAN_POINT ( 'NONE',  ( -58.00979178563854077, 29.32343869649098878, 170.0000000000000000 ) ) ;
#598 = ORIENTED_EDGE ( 'NONE', *, *, #20731, .F. ) ;
#599 = CARTESIAN_POINT ( 'NONE',  ( 60.61895554631705352, 13.15982272268128028, 71.28075859643588785 ) ) ;
#600 = CARTESIAN_POINT ( 'NONE',  ( -7.329206686002009974E-14, -46.66904755831211560, 85.00100000000000477 ) ) ;
#601 = CARTESIAN_POINT ( 'NONE',  ( -8.314488422519705324, 7.931352979988700369, 3.271030448983515804 ) ) ;
#602 = CARTESIAN_POINT ( 'NONE',  ( 41.09759788073309750, 9.651672055033843733, -62.65450869435315440 ) ) ;
#603 = CARTESIAN_POINT ( 'NONE',  ( -2.190131154568196070, 6.589492063460817839, 32.66031877935753869 ) ) ;
#604 = LINE ( 'NONE', #43156, #69293 ) ;
#605 = CARTESIAN_POINT ( 'NONE',  ( 79.14363954553030567, 18.05357752518858661, 91.47790248387103418 ) ) ;
#606 = VECTOR ( 'NONE', #8616, 1000.000000000000000 ) ;
#607 = ORIENTED_EDGE ( 'NONE', *, *, #30585, .F. ) ;
#608 = VECTOR ( 'NONE', #24397, 1000.000000000000000 ) ;
#609 = DIRECTION ( 'NONE',  ( 0.7999999999999942712, 1.038058528024521365E-14, -0.6000000000000077494 ) ) ;
#610 = CARTESIAN_POINT ( 'NONE',  ( 50.57199999999998852, 0.000000000000000000, 5.000000000000000888 ) ) ;
#611 = FACE_OUTER_BOUND ( 'NONE', #10480, .T. ) ;
#612 = CARTESIAN_POINT ( 'NONE',  ( -170.2856292770788968, 85.50720222068218845, -49.16844864926446235 ) ) ;
#613 = EDGE_CURVE ( 'NONE', #67838, #27835, #64835, .T. ) ;
#614 = ITEM_DEFINED_TRANSFORMATION ( 'NONE', 'NONE', #65872,  #66832 ) ;
#615 = CARTESIAN_POINT ( 'NONE',  ( -128.1267916618074594, 49.19573276651588856, -35.23903939184793188 ) ) ;
#616 = ORIENTED_EDGE ( 'NONE', *, *, #58079, .T. ) ;
#618 = DIRECTION ( 'NONE',  ( -0.000000000000000000, 1.000000000000000000, -0.000000000000000000 ) ) ;
#617 = VECTOR ( 'NONE', #33046, 1000.000000000000000 ) ;
#619 = AXIS2_PLACEMENT_3D ( 'NONE', #20593, #9026, #42056 ) ;
#620 = CARTESIAN_POINT ( 'NONE',  ( 0.000000000000000000, 0.000000000000000000, 0.000000000000000000 ) ) ;
#621 =( GEOMETRIC_REPRESENTATION_CONTEXT ( 3 ) GLOBAL_UNCERTAINTY_ASSIGNED_CONTEXT ( ( #45151 ) ) GLOBAL_UNIT_ASSIGNED_CONTEXT ( ( #57453, #30034, #6044 ) ) REPRESENTATION_CONTEXT ( 'NONE', 'WORKASPACE' ) );
#622 = VECTOR ( 'NONE', #43796, 1000.000000000000000 ) ;
#623 = EDGE_CURVE ( 'NONE', #36282, #8304, #15353, .T. ) ;
#624 = CARTESIAN_POINT ( 'NONE',  ( 86.62931800182292363, 19.42108912189599224, -89.51066537983906812 ) ) ;
#625 =( BOUNDED_CURVE ( )  B_SPLINE_CURVE ( 3, ( #39954, #62719, #29065, #46526 ),
 .UNSPECIFIED., .F., .F. ) 
 B_SPLINE_CURVE_WITH_KNOTS ( ( 4, 4 ),
 ( 3.481231835296680899, 3.885125003385272446 ),
 .UNSPECIFIED. ) 
 CURVE ( )  GEOMETRIC_REPRESENTATION_ITEM ( )  RATIONAL_B_SPLINE_CURVE ( ( 1.000000000000000000, 0.9864519964717846090, 0.9864519964717846090, 1.000000000000000000 ) ) 
 REPRESENTATION_ITEM ( '' )  );
#626 = VECTOR ( 'NONE', #27457, 1000.000000000000000 ) ;
#627 = EDGE_CURVE ( 'NONE', #45198, #50879, #47422, .T. ) ;
#628 = DIRECTION ( 'NONE',  ( -0.000000000000000000, -0.000000000000000000, -1.000000000000000000 ) ) ;
#629 = VERTEX_POINT ( 'NONE', #36460 ) ;
#630 = CARTESIAN_POINT ( 'NONE',  ( 0.4973051450695675224, -3.866309095700863896, -8.000000000000000000 ) ) ;
#631 = CARTESIAN_POINT ( 'NONE',  ( 82.94816950786170651, 19.25538918181908343, 16.90648424603243072 ) ) ;
#632 = EDGE_CURVE ( 'NONE', #26921, #4856, #48977, .T. ) ;
#633 = CARTESIAN_POINT ( 'NONE',  ( -100.4347360276019288, 32.97716872911834685, 30.73474136560336234 ) ) ;
#634 = VERTEX_POINT ( 'NONE', #30845 ) ;
#635 = FACE_OUTER_BOUND ( 'NONE', #24714, .T. ) ;
#637 = ORIENTED_EDGE ( 'NONE', *, *, #53348, .T. ) ;
#636 = B_SPLINE_CURVE_WITH_KNOTS ( 'NONE', 3,
 ( #25804, #40931, #40580, #34971, #29685, #46197 ),
 .UNSPECIFIED., .F., .F.,
 ( 4, 2, 4 ),
 ( 1.095770181104900047E-06, 0.03239442681617710901, 0.06478775786217311206 ),
 .UNSPECIFIED. ) ;
#638 = ORIENTED_EDGE ( 'NONE', *, *, #35254, .T. ) ;
#639 = CARTESIAN_POINT ( 'NONE',  ( -75.43044859198180063, 21.11535168543637653, -9.000624265271870428 ) ) ;
#640 = ADVANCED_FACE ( 'NONE', ( #57916 ), #9734, .T. ) ;
#641 = CARTESIAN_POINT ( 'NONE',  ( -24.85653282846401879, 9.618702155736652770, 94.99999999999866418 ) ) ;
#643 = ORIENTED_EDGE ( 'NONE', *, *, #36304, .T. ) ;
#642 = CARTESIAN_POINT ( 'NONE',  ( 154.0281735872262630, 56.28213428456460576, 16.73232576723794907 ) ) ;
#644 = CARTESIAN_POINT ( 'NONE',  ( 164.9534461562628564, 63.71129898458568874, 36.33204052779463922 ) ) ;
#645 = DIRECTION ( 'NONE',  ( -1.000000000000000000, -0.000000000000000000, -0.000000000000000000 ) ) ;
#646 = CARTESIAN_POINT ( 'NONE',  ( 447.3372781065089612, 365.0000000000064233, -146.4497041420121377 ) ) ;
#647 = PRODUCT_DEFINITION_SHAPE ( 'NONE', 'NONE',  #69621 ) ;
#648 = ORIENTED_EDGE ( 'NONE', *, *, #3366, .T. ) ;
#649 = CARTESIAN_POINT ( 'NONE',  ( -144.2298831394396075, 61.12003712726058069, -90.66825305514043976 ) ) ;
#650 = CARTESIAN_POINT ( 'NONE',  ( -35.99432170610150905, 10.38324794858010058, -21.95070075044081648 ) ) ;
#651 = DIRECTION ( 'NONE',  ( -1.000000000000000000, 0.000000000000000000, 0.000000000000000000 ) ) ;
#652 = CARTESIAN_POINT ( 'NONE',  ( -38.69577193929646342, 10.89562623693160148, -71.62007173369499924 ) ) ;
#653 = ORIENTED_EDGE ( 'NONE', *, *, #46286, .F. ) ;
#654 = EDGE_LOOP ( 'NONE', ( #13629, #60048, #33344, #59495 ) ) ;
#655 = CIRCLE ( 'NONE', #60208, 5.000000000000004441 ) ;
#656 = ORIENTED_EDGE ( 'NONE', *, *, #67416, .T. ) ;
#657 = DIRECTION ( 'NONE',  ( 0.000000000000000000, -1.000000000000000000, 0.000000000000000000 ) ) ;
#658 = DIRECTION ( 'NONE',  ( 0.000000000000000000, 1.000000000000000000, 0.000000000000000000 ) ) ;
#659 = VECTOR ( 'NONE', #43417, 1000.000000000000000 ) ;
#660 = AXIS2_PLACEMENT_3D ( 'NONE', #33851, #12745, #56006 ) ;
#661 = DIRECTION ( 'NONE',  ( 0.000000000000000000, -1.000000000000000000, 0.000000000000000000 ) ) ;
#662 = CARTESIAN_POINT ( 'NONE',  ( 8.820885042878503057, -74.43053605947400797, 41.38025477438755928 ) ) ;
#663 = CARTESIAN_POINT ( 'NONE',  ( 69.20492276531108189, 14.19384449732238807, 86.75300155572325878 ) ) ;
#664 = AXIS2_PLACEMENT_3D ( 'NONE', #53715, #65686, #38592 ) ;
#665 = FACE_OUTER_BOUND ( 'NONE', #60065, .T. ) ;
#666 = LINE ( 'NONE', #15804, #31702 ) ;
#667 = CARTESIAN_POINT ( 'NONE',  ( -52.60225734941438702, 15.07707183530729012, 84.41092461975652839 ) ) ;
#668 = AXIS2_PLACEMENT_3D ( 'NONE', #7424, #55591, #18310 ) ;
#670 = LINE ( 'NONE', #22117, #19760 ) ;
#669 = VECTOR ( 'NONE', #8748, 1000.000000000000000 ) ;
#671 = VERTEX_POINT ( 'NONE', #68799 ) ;
#673 = VECTOR ( 'NONE', #25427, 1000.000000000000000 ) ;
#672 = CARTESIAN_POINT ( 'NONE',  ( 36.85262215550149278, -53.56030941157680303, 41.38025477438755928 ) ) ;
#674 = ORIENTED_EDGE ( 'NONE', *, *, #10621, .T. ) ;
#675 = DIRECTION ( 'NONE',  ( 0.000000000000000000, -1.000000000000000000, -0.000000000000000000 ) ) ;
#676 = CARTESIAN_POINT ( 'NONE',  ( 210.9747454890631388, 115.3673079504856105, -66.55747008898767092 ) ) ;
#677 = CARTESIAN_POINT ( 'NONE',  ( 21.98745393275290994, -71.71550996510497100, 170.0000000000000000 ) ) ;
#678 = CARTESIAN_POINT ( 'NONE',  ( 414.4083459183740388, 395.0000000000000568, -113.5207719538772579 ) ) ;
#679 = CARTESIAN_POINT ( 'NONE',  ( -39.55079474733700096, 51.59997227570983114, 43.58025477438756923 ) ) ;
#680 = DIRECTION ( 'NONE',  ( -0.000000000000000000, 1.000000000000000000, -0.000000000000000000 ) ) ;
#681 = CARTESIAN_POINT ( 'NONE',  ( 202.8477687489651373, 103.8400411879524228, 83.10837270847002856 ) ) ;
#682 = DIRECTION ( 'NONE',  ( -0.000000000000000000, -0.000000000000000000, -1.000000000000000000 ) ) ;
#683 = CARTESIAN_POINT ( 'NONE',  ( 164.9540180502650912, 65.02981548735054673, -69.90027363021420115 ) ) ;
#684 = ORIENTED_EDGE ( 'NONE', *, *, #12471, .T. ) ;
#685 = ADVANCED_FACE ( 'NONE', ( #27535 ), #36810, .F. ) ;
#686 = CARTESIAN_POINT ( 'NONE',  ( -28.30427060690108476, 69.40159203110296460, 41.38025477438755928 ) ) ;
#687 = LINE ( 'NONE', #32690, #59969 ) ;
#688 = ORIENTED_EDGE ( 'NONE', *, *, #20639, .F. ) ;
#689 = ORIENTED_EDGE ( 'NONE', *, *, #206, .F. ) ;
#690 = CARTESIAN_POINT ( 'NONE',  ( -86.15441609607631790, 25.31657638323081727, 37.42314418770195772 ) ) ;
#691 = CARTESIAN_POINT ( 'NONE',  ( 157.0357419681844533, 58.58786672900117765, -77.95933384252394660 ) ) ;
#692 = CARTESIAN_POINT ( 'NONE',  ( 46.90170507415073331, 10.52318308703818772, 37.90916503474270627 ) ) ;
#693 = CARTESIAN_POINT ( 'NONE',  ( -26.88245755577922935, 8.887394979218516511, 58.58345839708251646 ) ) ;
#694 = CARTESIAN_POINT ( 'NONE',  ( 131.6189313563687335, 40.08924984825277704, -9.505401706098517423 ) ) ;
#695 = VERTEX_POINT ( 'NONE', #62510 ) ;
#696 = ORIENTED_EDGE ( 'NONE', *, *, #24415, .T. ) ;
#697 = LINE ( 'NONE', #39377, #69339 ) ;
#698 = ORIENTED_EDGE ( 'NONE', *, *, #41061, .T. ) ;
#699 = CARTESIAN_POINT ( 'NONE',  ( 447.3372781065085633, 400.0000000000000568, -116.4497041420118393 ) ) ;
#700 = CYLINDRICAL_SURFACE ( 'NONE', #28223, 65.00000000000000000 ) ;
#701 = CARTESIAN_POINT ( 'NONE',  ( 206.7099580236349823, 109.1417833474364159, 43.94436230140331645 ) ) ;
#702 = CARTESIAN_POINT ( 'NONE',  ( 141.3576134020958932, 47.34559817395930992, 90.83861031058405899 ) ) ;
#703 = CARTESIAN_POINT ( 'NONE',  ( -27.40573813655178270, 9.981056867228259577, -90.17953602832123750 ) ) ;
#704 = EDGE_CURVE ( 'NONE', #58577, #50465, #36961, .T. ) ;
#705 = FACE_OUTER_BOUND ( 'NONE', #37615, .T. ) ;
#706 = AXIS2_PLACEMENT_3D ( 'NONE', #9153, #14435, #51716 ) ;
#707 = B_SPLINE_CURVE_WITH_KNOTS ( 'NONE', 3,
 ( #53839, #38731, #5658, #1443, #27118, #43988 ),
 .UNSPECIFIED., .F., .F.,
 ( 4, 2, 4 ),
 ( 1.095770181099519270E-06, 0.03239442681617710207, 0.06478775786217311206 ),
 .UNSPECIFIED. ) ;
#708 = CARTESIAN_POINT ( 'NONE',  ( -48.00000000000000000, 19.99999999999996447, 0.000000000000000000 ) ) ;
#709 = ORIENTED_EDGE ( 'NONE', *, *, #24458, .T. ) ;
#710 = ORIENTED_EDGE ( 'NONE', *, *, #12281, .T. ) ;
#711 = CARTESIAN_POINT ( 'NONE',  ( 90.13282190615606737, 1.839221433318906476E-12, -5.000000000000000000 ) ) ;
#712 = FACE_OUTER_BOUND ( 'NONE', #13803, .T. ) ;
#713 = AXIS2_PLACEMENT_3D ( 'NONE', #6914, #44550, #24147 ) ;
#714 = CARTESIAN_POINT ( 'NONE',  ( 49.76301652092224970, -41.81676920493044491, 170.0000000000000000 ) ) ;
#715 = CARTESIAN_POINT ( 'NONE',  ( 200.0000000000000000, 2.999999999999969802, -46.99999999999997158 ) ) ;
#716 = EDGE_CURVE ( 'NONE', #67683, #29070, #35781, .T. ) ;
#717 = CARTESIAN_POINT ( 'NONE',  ( 66.08620257826613908, 13.40585338179127106, 44.15986684989842104 ) ) ;
#718 = VECTOR ( 'NONE', #42490, 1000.000000000000227 ) ;
#719 = ORIENTED_EDGE ( 'NONE', *, *, #53021, .T. ) ;
#720 = DIRECTION ( 'NONE',  ( -0.000000000000000000, -0.000000000000000000, -1.000000000000000000 ) ) ;
#721 = CARTESIAN_POINT ( 'NONE',  ( 83.37786665291103816, 18.33670623396830024, 17.14338525297940308 ) ) ;
#722 = ORIENTED_EDGE ( 'NONE', *, *, #59330, .F. ) ;
#723 = CARTESIAN_POINT ( 'NONE',  ( -442.6627218934912662, 394.9999999999998295, 113.5502958579881465 ) ) ;
#724 = ORIENTED_EDGE ( 'NONE', *, *, #31613, .F. ) ;
#725 = ADVANCED_FACE ( 'NONE', ( #30491 ), #68140, .T. ) ;
#726 = ORIENTED_EDGE ( 'NONE', *, *, #5061, .T. ) ;
#727 = DIRECTION ( 'NONE',  ( -0.000000000000000000, -0.000000000000000000, -1.000000000000000000 ) ) ;
#728 = EDGE_CURVE ( 'NONE', #63173, #34225, #68915, .T. ) ;
#729 = CARTESIAN_POINT ( 'NONE',  ( 94.02921784728462740, 22.08005910033071473, 11.61440990420907404 ) ) ;
#730 = FACE_OUTER_BOUND ( 'NONE', #7347, .T. ) ;
#731 = ORIENTED_EDGE ( 'NONE', *, *, #55277, .F. ) ;
#732 = CARTESIAN_POINT ( 'NONE',  ( -445.5916540816263591, 395.0000000000064801, -139.3786363301466906 ) ) ;
#733 = CARTESIAN_POINT ( 'NONE',  ( -2.116120943111210906, -74.98056102853675497, 170.0000000000000000 ) ) ;
#734 = CYLINDRICAL_SURFACE ( 'NONE', #62377, 7.500000000000020428 ) ;
#735 = CARTESIAN_POINT ( 'NONE',  ( -177.5288247523079406, 93.72924674643516596, -36.12611155980226130 ) ) ;
#736 = DIRECTION ( 'NONE',  ( -1.000000000000000000, 0.000000000000000000, 0.000000000000000000 ) ) ;
#737 = CARTESIAN_POINT ( 'NONE',  ( -173.1211646369891355, -170.0000000000000000, -22.86740657428632773 ) ) ;
#738 = DIRECTION ( 'NONE',  ( -1.000000000000000000, 0.000000000000000000, 0.000000000000000000 ) ) ;
#739 = ORIENTED_EDGE ( 'NONE', *, *, #39691, .T. ) ;
#740 = CARTESIAN_POINT ( 'NONE',  ( -56.92000000000000171, -36.09918303830819752, 30.00000000000000000 ) ) ;
#741 = CARTESIAN_POINT ( 'NONE',  ( 0.000000000000000000, 0.000000000000000000, 43.58025477438756212 ) ) ;
#742 = ORIENTED_EDGE ( 'NONE', *, *, #24252, .T. ) ;
#743 = FACE_BOUND ( 'NONE', #56230, .T. ) ;
#744 = CARTESIAN_POINT ( 'NONE',  ( -783.0172411895269988, -622.0000000000060254, 0.000000000000000000 ) ) ;
#745 = CARTESIAN_POINT ( 'NONE',  ( -180.5954680880247167, 97.44843622358462198, 64.52607031460266285 ) ) ;
#746 = CARTESIAN_POINT ( 'NONE',  ( -146.1201263095600211, 62.66021356509621398, -8.772963640185553302 ) ) ;
#747 = LINE ( 'NONE', #64413, #62651 ) ;
#748 = CARTESIAN_POINT ( 'NONE',  ( -86.15466590221106458, 26.40813842494317853, 11.56579973364435787 ) ) ;
#749 = DIRECTION ( 'NONE',  ( -0.000000000000000000, -0.000000000000000000, 1.000000000000000000 ) ) ;
#750 = CARTESIAN_POINT ( 'NONE',  ( 44.99999999999997158, 22.99999999999998579, 0.000000000000000000 ) ) ;
#751 = CARTESIAN_POINT ( 'NONE',  ( -72.43779980922290918, 20.04595627325881324, -92.10289429969509456 ) ) ;
#752 = CARTESIAN_POINT ( 'NONE',  ( 66.08620257826611066, 13.40585338179127106, 17.31531625943474495 ) ) ;
#753 = CARTESIAN_POINT ( 'NONE',  ( 159.2389084450349515, 59.03884018680375334, 17.36706718780300562 ) ) ;
#754 = CARTESIAN_POINT ( 'NONE',  ( 92.95016907945944240, 22.74936990452174967, -20.52150210306960432 ) ) ;
#755 = EDGE_LOOP ( 'NONE', ( #38002, #54803, #6340, #38216 ) ) ;
#756 = AXIS2_PLACEMENT_3D ( 'NONE', #20145, #23779, #63754 ) ;
#757 = DIRECTION ( 'NONE',  ( -1.000000000000000000, -0.000000000000000000, -0.000000000000000000 ) ) ;
#758 = EDGE_LOOP ( 'NONE', ( #20135, #22340, #67146, #6100 ) ) ;
#759 = DIRECTION ( 'NONE',  ( 1.469488203625002396E-16, 2.022576995815139509E-16, 1.000000000000000000 ) ) ;
#760 = FACE_OUTER_BOUND ( 'NONE', #64496, .T. ) ;
#761 = AXIS2_PLACEMENT_3D ( 'NONE', #52678, #36171, #19998 ) ;
#762 = CARTESIAN_POINT ( 'NONE',  ( 116.8402898440648841, 33.18057798316834095, 94.43274024419686441 ) ) ;
#763 = CARTESIAN_POINT ( 'NONE',  ( -149.0764453401866660, 65.13297611514532548, 57.56537183036272864 ) ) ;
#764 = CARTESIAN_POINT ( 'NONE',  ( 70.51484748609222208, 14.53801151001411540, -16.88811832611002117 ) ) ;
#765 = CYLINDRICAL_SURFACE ( 'NONE', #45215, 498.0000000000000000 ) ;
#766 = AXIS2_PLACEMENT_3D ( 'NONE', #19277, #30885, #3455 ) ;
#767 = CARTESIAN_POINT ( 'NONE',  ( -51.34542473642583360, 14.75635007918829622, -76.08508367074277601 ) ) ;
#768 = ADVANCED_FACE ( 'NONE', ( #22611 ), #7498, .F. ) ;
#769 = CARTESIAN_POINT ( 'NONE',  ( -76.57252593202586866, 22.60812157331044148, -89.09011755351514239 ) ) ;
#770 = CARTESIAN_POINT ( 'NONE',  ( -124.1007047332777802, 46.52282960291162084, -22.86580842938086988 ) ) ;
#771 = EDGE_LOOP ( 'NONE', ( #32204, #20972 ) ) ;
#772 = VERTEX_POINT ( 'NONE', #33537 ) ;
#773 = CARTESIAN_POINT ( 'NONE',  ( 32.15284246740099405, 8.588257691344876932, 66.19772994508791442 ) ) ;
#774 = CARTESIAN_POINT ( 'NONE',  ( 174.9042454172879957, 72.57746269938726869, 67.93336458024957381 ) ) ;
#775 = ADVANCED_FACE ( 'NONE', ( #1507 ), #17696, .F. ) ;
#776 = CARTESIAN_POINT ( 'NONE',  ( -165.6397095829521504, 80.60756690931938806, 64.55706535356031850 ) ) ;
#777 = DIRECTION ( 'NONE',  ( 0.7530714660036099684, 0.6579387259397138088, 0.000000000000000000 ) ) ;
#778 = PRODUCT_DEFINITION_CONTEXT ( 'detailed design', #31878, 'design' ) ;
#779 = CARTESIAN_POINT ( 'NONE',  ( 196.9999999999999716, 1.500000000000015321, -1.500000000000015321 ) ) ;
#780 = VERTEX_POINT ( 'NONE', #3099 ) ;
#781 = CARTESIAN_POINT ( 'NONE',  ( 109.7782172510783312, 29.77507867835874222, -50.92243756565370205 ) ) ;
#782 = CARTESIAN_POINT ( 'NONE',  ( -13.47230132170245476, 7.324574289401438065, 69.42015683888705269 ) ) ;
#783 = CARTESIAN_POINT ( 'NONE',  ( 205.5049354810106763, 109.1776577097391225, 2.363170148305743457 ) ) ;
#784 = CARTESIAN_POINT ( 'NONE',  ( -83.06837433973049656, 25.13241508624138376, -90.21674049272554896 ) ) ;
#785 = CARTESIAN_POINT ( 'NONE',  ( 46.50207827473963107, 9.439498081273466568, -18.70419972480020476 ) ) ;
#786 = CARTESIAN_POINT ( 'NONE',  ( 18.66447700095702444, -37.32227186998856894, 13.79046340968177553 ) ) ;
#787 = FACE_BOUND ( 'NONE', #41544, .T. ) ;
#788 = EDGE_CURVE ( 'NONE', #34907, #36914, #33986, .T. ) ;
#789 = CARTESIAN_POINT ( 'NONE',  ( 159.2258951716709987, 60.31399909112332836, 56.44886570136385018 ) ) ;
#790 = EDGE_CURVE ( 'NONE', #8416, #11547, #57246, .T. ) ;
#791 = EDGE_CURVE ( 'NONE', #60292, #33533, #43667, .T. ) ;
#792 = ORIENTED_EDGE ( 'NONE', *, *, #874, .T. ) ;
#793 = DIRECTION ( 'NONE',  ( -1.661094098900087138E-16, 0.6427876096865404731, 0.7660444431189771253 ) ) ;
#794 = LINE ( 'NONE', #10991, #2437 ) ;
#795 = CARTESIAN_POINT ( 'NONE',  ( 412.3372781065085633, 219.4906275429376308, 113.5502958579881749 ) ) ;
#796 = CARTESIAN_POINT ( 'NONE',  ( -783.0172411895269988, -622.0000000000060254, 10.00000000000000000 ) ) ;
#797 = EDGE_CURVE ( 'NONE', #15914, #43922, #8376, .T. ) ;
#798 = CARTESIAN_POINT ( 'NONE',  ( 154.4550750032602195, 55.34393534448155805, 16.93593135338981526 ) ) ;
#799 = CARTESIAN_POINT ( 'NONE',  ( -1.184052349595404507, 7.556339067815312838, 87.80471432908419160 ) ) ;
#800 = VECTOR ( 'NONE', #25987, 1000.000000000000000 ) ;
#801 = ORIENTED_EDGE ( 'NONE', *, *, #53338, .F. ) ;
#802 = CARTESIAN_POINT ( 'NONE',  ( 6.800000000000000711, 0.000000000000000000, 0.000000000000000000 ) ) ;
#803 = DIRECTION ( 'NONE',  ( -0.7071067811865405783, -7.105427357601001070E-15, 0.7071067811865545671 ) ) ;
#804 = ORIENTED_EDGE ( 'NONE', *, *, #57601, .F. ) ;
#805 = VERTEX_POINT ( 'NONE', #29820 ) ;
#806 = DIRECTION ( 'NONE',  ( 1.000000000000000000, 0.000000000000000000, 0.000000000000000000 ) ) ;
#807 = LINE ( 'NONE', #22262, #23012 ) ;
#808 = CARTESIAN_POINT ( 'NONE',  ( 93.32756701508621688, 22.89083686918420568, -66.75542603816978726 ) ) ;
#810 = ORIENTED_EDGE ( 'NONE', *, *, #68485, .F. ) ;
#809 = EDGE_CURVE ( 'NONE', #32676, #18463, #67463, .T. ) ;
#811 = AXIS2_PLACEMENT_3D ( 'NONE', #11235, #38319, #43595 ) ;
#812 = ORIENTED_EDGE ( 'NONE', *, *, #10621, .F. ) ;
#813 = CARTESIAN_POINT ( 'NONE',  ( 0.000000000000000000, 0.000000000000000000, 43.58025477438756212 ) ) ;
#814 = EDGE_CURVE ( 'NONE', #41171, #10653, #16834, .T. ) ;
#816 = EDGE_CURVE ( 'NONE', #58443, #61153, #12692, .T. ) ;
#815 = CARTESIAN_POINT ( 'NONE',  ( 162.6205203824433170, 63.07332653227189212, 42.36688915199772509 ) ) ;
#817 = EDGE_CURVE ( 'NONE', #39831, #41874, #11117, .T. ) ;
#818 = VECTOR ( 'NONE', #14052, 1000.000000000000000 ) ;
#819 = CARTESIAN_POINT ( 'NONE',  ( -156.4966862384868591, 71.70877417666513054, -66.38460535960628306 ) ) ;
#820 = CARTESIAN_POINT ( 'NONE',  ( 70.46579300139244140, 15.56614468937218909, 11.46688215326957305 ) ) ;
#821 = DIRECTION ( 'NONE',  ( 0.000000000000000000, -0.000000000000000000, 1.000000000000000000 ) ) ;
#822 = VECTOR ( 'NONE', #43573, 1000.000000000000114 ) ;
#823 = CARTESIAN_POINT ( 'NONE',  ( 102.7446498997619955, 26.65764321315727514, -17.11449461936757999 ) ) ;
#824 = CARTESIAN_POINT ( 'NONE',  ( -125.8938041572051389, 47.69968343338781125, 72.46449846362081360 ) ) ;
#825 = CARTESIAN_POINT ( 'NONE',  ( 8.478575283864731915, 7.382882227715639623, 39.21115070528450985 ) ) ;
#826 = CYLINDRICAL_SURFACE ( 'NONE', #20311, 5.000000000000004441 ) ;
#827 = DIRECTION ( 'NONE',  ( 0.000000000000000000, -1.000000000000000000, 0.000000000000000000 ) ) ;
#829 = ORIENTED_EDGE ( 'NONE', *, *, #20982, .F. ) ;
#828 = FACE_OUTER_BOUND ( 'NONE', #18462, .T. ) ;
#830 = ORIENTED_EDGE ( 'NONE', *, *, #22808, .F. ) ;
#831 = ORIENTED_EDGE ( 'NONE', *, *, #67075, .T. ) ;
#832 = CARTESIAN_POINT ( 'NONE',  ( -14.55425570676091951, 7.423011834016145727, -12.75193667354853488 ) ) ;
#833 = CARTESIAN_POINT ( 'NONE',  ( -166.2425995121691642, 81.22826102820870631, 94.99999999999866418 ) ) ;
#834 = CARTESIAN_POINT ( 'NONE',  ( 17.98081503251174240, -17.36923402935755689, 0.000000000000000000 ) ) ;
#835 = CARTESIAN_POINT ( 'NONE',  ( 39.40195752203892710, -170.0000000000000000, -96.80891864635512434 ) ) ;
#836 = CARTESIAN_POINT ( 'NONE',  ( -37.07436112751820190, 11.60822760208522375, 69.53422127808219955 ) ) ;
#837 = CARTESIAN_POINT ( 'NONE',  ( -13.92109095214680359, 8.375243258322932149, -20.44991048438748038 ) ) ;
#838 = CARTESIAN_POINT ( 'NONE',  ( -72.21652659655761397, 19.96855882996548459, -73.32001115466152896 ) ) ;
#839 = DIRECTION ( 'NONE',  ( 0.7071067811865475727, 0.000000000000000000, -0.7071067811865475727 ) ) ;
#840 = ORIENTED_EDGE ( 'NONE', *, *, #43108, .F. ) ;
#841 = CARTESIAN_POINT ( 'NONE',  ( 0.000000000000000000, 0.000000000000000000, 85.00000000000000000 ) ) ;
#842 = ORIENTED_EDGE ( 'NONE', *, *, #61547, .F. ) ;
#843 = ORIENTED_EDGE ( 'NONE', *, *, #16764, .T. ) ;
#844 = CARTESIAN_POINT ( 'NONE',  ( 66.07923263163412742, 14.44036440558002532, -23.22621644188427226 ) ) ;
#845 = CARTESIAN_POINT ( 'NONE',  ( 0.06809871960543363578, -7.710219529346616696, 2.645508037661887801 ) ) ;
#846 = CARTESIAN_POINT ( 'NONE',  ( -25.34321324147440180, 9.685523517558388917, 86.98799891496780390 ) ) ;
#847 = CARTESIAN_POINT ( 'NONE',  ( -96.45845418068302024, 29.92035703021965176, -47.26932368623729985 ) ) ;
#849 = CARTESIAN_POINT ( 'NONE',  ( -109.7647482398635361, 36.74843029291206165, 11.72205608543185562 ) ) ;
#848 = VECTOR ( 'NONE', #5552, 1000.000000000000000 ) ;
#850 = CARTESIAN_POINT ( 'NONE',  ( 23.09541709302172308, 6.844586979481588784, 35.80722948394830496 ) ) ;
#851 = CARTESIAN_POINT ( 'NONE',  ( 0.000000000000000000, 0.000000000000000000, 0.000000000000000000 ) ) ;
#852 = ORIENTED_EDGE ( 'NONE', *, *, #43049, .T. ) ;
#853 = ORIENTED_EDGE ( 'NONE', *, *, #16095, .T. ) ;
#854 = ORIENTED_EDGE ( 'NONE', *, *, #55316, .F. ) ;
#855 = AXIS2_PLACEMENT_3D ( 'NONE', #17827, #11841, #44185 ) ;
#856 = EDGE_CURVE ( 'NONE', #15508, #55490, #4805, .T. ) ;
#857 = CARTESIAN_POINT ( 'NONE',  ( -157.0069571479806996, 72.18154199622279066, -15.76883794595808652 ) ) ;
#858 = CARTESIAN_POINT ( 'NONE',  ( 35.44311777160621091, 8.940232499250168274, -36.74501715293298076 ) ) ;
#859 =( REPRESENTATION_RELATIONSHIP ('NONE','NONE', #40274, #60409 ) REPRESENTATION_RELATIONSHIP_WITH_TRANSFORMATION ( #46517 )SHAPE_REPRESENTATION_RELATIONSHIP( ) );
#860 = VECTOR ( 'NONE', #7201, 1000.000000000000000 ) ;
#861 = CARTESIAN_POINT ( 'NONE',  ( -38.93922791710217268, 10.94334660650241986, 64.31909387702090442 ) ) ;
#862 = CARTESIAN_POINT ( 'NONE',  ( 201.5987353083855851, 103.8544727311227405, 56.70899253505132975 ) ) ;
#863 = VERTEX_POINT ( 'NONE', #31892 ) ;
#864 = CARTESIAN_POINT ( 'NONE',  ( 188.4374648754671000, 87.87346242052437617, 62.14831556033239934 ) ) ;
#865 = CARTESIAN_POINT ( 'NONE',  ( -152.9121563765243934, 67.12206067149026012, 71.75184801906829080 ) ) ;
#866 = CARTESIAN_POINT ( 'NONE',  ( -3.253130881186333312, 7.643323950922365384, -48.88322396365997236 ) ) ;
#867 = FILL_AREA_STYLE ('',( #64184 ) ) ;
#868 = DIRECTION ( 'NONE',  ( 0.000000000000000000, 1.000000000000000000, 0.000000000000000000 ) ) ;
#869 = CARTESIAN_POINT ( 'NONE',  ( -444.2280788262714282, 394.7493581867591388, -130.3782898954363532 ) ) ;
#870 = CARTESIAN_POINT ( 'NONE',  ( 22.89234820949994287, 6.832052815347870123, 61.94203120367916426 ) ) ;
#871 = EDGE_CURVE ( 'NONE', #64668, #6453, #9752, .T. ) ;
#872 = LINE ( 'NONE', #58556, #659 ) ;
#873 = CARTESIAN_POINT ( 'NONE',  ( 14.08699529666005823, 6.452200550165255954, -62.55491622521332573 ) ) ;
#874 = EDGE_CURVE ( 'NONE', #69029, #46944, #44509, .T. ) ;
#875 = VECTOR ( 'NONE', #26956, 1000.000000000000000 ) ;
#876 = EDGE_CURVE ( 'NONE', #55579, #9108, #39602, .T. ) ;
#877 = ORIENTED_EDGE ( 'NONE', *, *, #51299, .F. ) ;
#878 = LINE ( 'NONE', #59590, #42830 ) ;
#879 = ITEM_DEFINED_TRANSFORMATION ( 'NONE', 'NONE', #43273,  #66832 ) ;
#880 = CARTESIAN_POINT ( 'NONE',  ( -133.1527834403230486, 51.46311219732124442, -67.35340832687874979 ) ) ;
#881 = CARTESIAN_POINT ( 'NONE',  ( -133.3149301983942223, 51.57857650535022032, -41.29510496815424148 ) ) ;
#882 = DIRECTION ( 'NONE',  ( 0.000000000000000000, 1.000000000000000000, 0.000000000000000000 ) ) ;
#883 = CARTESIAN_POINT ( 'NONE',  ( 57.09527843067915143, 12.40436368789085897, -74.67611128734689885 ) ) ;
#884 = ORIENTED_EDGE ( 'NONE', *, *, #38208, .T. ) ;
#885 = ORIENTED_EDGE ( 'NONE', *, *, #41118, .F. ) ;
#886 = CARTESIAN_POINT ( 'NONE',  ( 0.06730325657375685333, -1.557442666578433776, -8.000000000000000000 ) ) ;
#887 = CARTESIAN_POINT ( 'NONE',  ( 0.000000000000000000, 0.000000000000000000, 170.0000000000000000 ) ) ;
#888 = ORIENTED_EDGE ( 'NONE', *, *, #62836, .F. ) ;
#889 = VERTEX_POINT ( 'NONE', #17803 ) ;
#890 = CARTESIAN_POINT ( 'NONE',  ( 175.5493994043409600, 73.18740965572595769, -38.65758324743049457 ) ) ;
#891 = FACE_OUTER_BOUND ( 'NONE', #1268, .T. ) ;
#892 = ORIENTED_EDGE ( 'NONE', *, *, #45337, .F. ) ;
#893 = DIRECTION ( 'NONE',  ( -0.000000000000000000, 1.000000000000000000, -0.000000000000000000 ) ) ;
#894 = CARTESIAN_POINT ( 'NONE',  ( 138.1901928158493433, 45.29454828899442731, 69.99416493423962038 ) ) ;
#895 = CARTESIAN_POINT ( 'NONE',  ( -72.78737098446266884, 20.16853011470087864, -47.29921101198596745 ) ) ;
#896 = ADVANCED_FACE ( 'NONE', ( #44876 ), #22778, .T. ) ;
#897 = CARTESIAN_POINT ( 'NONE',  ( 0.000000000000000000, 6.000000000000000000, -46.99999999999997158 ) ) ;
#898 = CARTESIAN_POINT ( 'NONE',  ( 15.78827728214693416, 6.500811158483284835, -50.51894409868581448 ) ) ;
#899 = CARTESIAN_POINT ( 'NONE',  ( -51.13576748034041231, 14.70354244225167761, -22.27226429992984080 ) ) ;
#900 = VECTOR ( 'NONE', #4776, 1000.000000000000000 ) ;
#901 = EDGE_CURVE ( 'NONE', #59026, #60171, #23772, .T. ) ;
#902 = VERTEX_POINT ( 'NONE', #49437 ) ;
#903 = VECTOR ( 'NONE', #22935, 1000.000000000000227 ) ;
#904 = PLANE ( 'NONE',  #39037 ) ;
#905 = CARTESIAN_POINT ( 'NONE',  ( -65.00200000000002376, 1.249999999999979350, 170.0000000000000000 ) ) ;
#906 = DIRECTION ( 'NONE',  ( 1.000000000000000000, -0.000000000000000000, -0.000000000000000000 ) ) ;
#907 = AXIS2_PLACEMENT_3D ( 'NONE', #46556, #43247, #32374 ) ;
#908 = CARTESIAN_POINT ( 'NONE',  ( -165.6754884515988522, 79.20562145685592270, -95.00000000000133582 ) ) ;
#910 = VERTEX_POINT ( 'NONE', #6888 ) ;
#909 = CARTESIAN_POINT ( 'NONE',  ( -133.3396229538948887, 51.59616673977242129, 92.77099222264472189 ) ) ;
#911 = CARTESIAN_POINT ( 'NONE',  ( 58.09877917144279280, 12.61383386832654629, 4.783940807170354859 ) ) ;
#912 =( GEOMETRIC_REPRESENTATION_CONTEXT ( 3 ) GLOBAL_UNCERTAINTY_ASSIGNED_CONTEXT ( ( #67666 ) ) GLOBAL_UNIT_ASSIGNED_CONTEXT ( ( #33451, #27807, #26433 ) ) REPRESENTATION_CONTEXT ( 'NONE', 'WORKASPACE' ) );
#913 = VERTEX_POINT ( 'NONE', #44161 ) ;
#914 = CARTESIAN_POINT ( 'NONE',  ( -147.7860806339125190, 62.73248524776226276, 57.75265429496991487 ) ) ;
#915 = DIRECTION ( 'NONE',  ( 0.000000000000000000, 0.000000000000000000, 1.000000000000000000 ) ) ;
#916 = DIRECTION ( 'NONE',  ( 1.261617073437677999E-16, 0.000000000000000000, 1.000000000000000000 ) ) ;
#917 = CARTESIAN_POINT ( 'NONE',  ( 181.5072453427590347, 79.03352099595184654, -24.38050707541595585 ) ) ;
#918 = CARTESIAN_POINT ( 'NONE',  ( 83.37786665291103816, 18.33670623396829313, -9.701165337484269457 ) ) ;
#919 = AXIS2_PLACEMENT_3D ( 'NONE', #25441, #41263, #40910 ) ;
#920 = CARTESIAN_POINT ( 'NONE',  ( 15.55634918610411610, 46.66904755831205875, 85.00100000000000477 ) ) ;
#921 = CARTESIAN_POINT ( 'NONE',  ( 88.99522780200243233, 20.24180937454203999, -63.04501563759147587 ) ) ;
#922 = CARTESIAN_POINT ( 'NONE',  ( -97.85576954355160240, 30.58918648956191078, 17.24970366714013181 ) ) ;
#923 = DIRECTION ( 'NONE',  ( -0.7071067811865463515, 0.000000000000000000, -0.7071067811865487940 ) ) ;
#924 = ORIENTED_EDGE ( 'NONE', *, *, #7720, .F. ) ;
#925 = VERTEX_POINT ( 'NONE', #60704 ) ;
#926 = DIRECTION ( 'NONE',  ( 0.2660368455666687892, 0.9639628606958550172, -0.000000000000000000 ) ) ;
#927 = CARTESIAN_POINT ( 'NONE',  ( 13.37366753069833436, 6.435102282077984626, 30.39700900802003503 ) ) ;
#928 = CARTESIAN_POINT ( 'NONE',  ( 32.06997139192792901, -56.95813133885440749, 41.38025477438755928 ) ) ;
#929 = DIRECTION ( 'NONE',  ( 1.110223024625156540E-16, 1.358505038629840220E-33, 1.000000000000000000 ) ) ;
#930 = PRODUCT_RELATED_PRODUCT_CATEGORY ( 'part', '', ( #65900 ) ) ;
#931 = DIRECTION ( 'NONE',  ( -1.000000000000000000, 0.000000000000000000, 0.000000000000000000 ) ) ;
#932 = CARTESIAN_POINT ( 'NONE',  ( 15.78827728214693060, 7.507518794609573831, 18.17015708224157322 ) ) ;
#933 = DIRECTION ( 'NONE',  ( 0.000000000000000000, 0.000000000000000000, 1.000000000000000000 ) ) ;
#934 = CARTESIAN_POINT ( 'NONE',  ( -119.6801029354225108, 43.71909921132880328, 33.91237456399324657 ) ) ;
#935 = CARTESIAN_POINT ( 'NONE',  ( 160.9069879467681687, 60.37290772564309549, -77.15118032727514219 ) ) ;
#937 = VERTEX_POINT ( 'NONE', #1979 ) ;
#936 = EDGE_CURVE ( 'NONE', #57871, #43209, #58711, .T. ) ;
#938 = CARTESIAN_POINT ( 'NONE',  ( -28.81071653159241563, 10.19258396314333837, 17.90053607095121180 ) ) ;
#939 = EDGE_LOOP ( 'NONE', ( #6618, #33629, #34700, #50943, #34117, #44911, #4182, #50730, #17595 ) ) ;
#940 = CARTESIAN_POINT ( 'NONE',  ( -20.00000000000002842, 3.680555555555560243, 4.000000000000000000 ) ) ;
#941 = EDGE_CURVE ( 'NONE', #52293, #21319, #16043, .T. ) ;
#942 = CARTESIAN_POINT ( 'NONE',  ( -86.05211524933166345, 25.27371147724188916, -95.00000000000133582 ) ) ;
#943 = CARTESIAN_POINT ( 'NONE',  ( 126.4757069339777757, 38.29528077539266206, 35.65345800163305512 ) ) ;
#944 = CARTESIAN_POINT ( 'NONE',  ( 34.45158752686798209, 8.829194381141999060, 16.22471098832457770 ) ) ;
#945 = LINE ( 'NONE', #32946, #35612 ) ;
#946 = CARTESIAN_POINT ( 'NONE',  ( 6.800000000000000711, 0.000000000000000000, 5.000000000000000888 ) ) ;
#947 = CARTESIAN_POINT ( 'NONE',  ( 0.000000000000000000, 70.00000000000000000, 0.000000000000000000 ) ) ;
#948 = CARTESIAN_POINT ( 'NONE',  ( -23.98664764928003734, -23.27925803097926050, 6.893343212288939981 ) ) ;
#949 = DIRECTION ( 'NONE',  ( 0.000000000000000000, 1.000000000000000000, -0.000000000000000000 ) ) ;
#950 = ORIENTED_EDGE ( 'NONE', *, *, #35514, .F. ) ;
#951 = CARTESIAN_POINT ( 'NONE',  ( -18.89790202299212396, 62.20684691518604836, 170.0000000000000000 ) ) ;
#952 = CARTESIAN_POINT ( 'NONE',  ( 55.00000000000000000, 16.00000000000000000, 6.196318915105386793 ) ) ;
#953 = LINE ( 'NONE', #37193, #3939 ) ;
#954 = CARTESIAN_POINT ( 'NONE',  ( 40.38132770291769447, 9.553709436640064112, -62.51267063216231179 ) ) ;
#955 = ADVANCED_FACE ( 'NONE', ( #29059 ), #50502, .F. ) ;
#956 = CARTESIAN_POINT ( 'NONE',  ( -3.868882431147342871, 6.665575841812236391, 31.23930121114426228 ) ) ;
#957 = FACE_OUTER_BOUND ( 'NONE', #48813, .T. ) ;
#958 = VECTOR ( 'NONE', #53885, 1000.000000000000000 ) ;
#959 = CARTESIAN_POINT ( 'NONE',  ( 85.04045433923197095, 19.94575836658696844, 83.56420614133747904 ) ) ;
#960 = EDGE_CURVE ( 'NONE', #18523, #30339, #59867, .T. ) ;
#961 = AXIS2_PLACEMENT_3D ( 'NONE', #39309, #28758, #55474 ) ;
#962 = ADVANCED_FACE ( 'NONE', ( #2322 ), #45219, .F. ) ;
#963 = B_SPLINE_CURVE_WITH_KNOTS ( 'NONE', 3,
 ( #47061, #48411, #15742, #53355, #25961, #243, #10453, #26647, #68849, #54039, #63247, #48081, #47391, #69538, #59335, #11148, #32613, #20672, #11845, #65677, #28373, #38229, #33670, #28732, #18179, #50183, #64975, #1646, #49466, #33324, #23107, #28022, #66038, #1300, #17108, #11483, #54750, #66388, #599, #59671, #32955, #2011, #60731 ),
 .UNSPECIFIED., .F., .F.,
 ( 4, 2, 2, 2, 2, 2, 2, 2, 2, 2, 2, 2, 1, 2, 2, 2, 2, 2, 2, 2, 2, 4 ),
 ( 0.02379577142314830140, 0.02527778373276526672, 0.02601878988757374070, 0.02675979604238221121, 0.02824180835199915571, 0.02972382066161610020, 0.03046482681642458112, 0.03120583297123305858, 0.03268784528085004470, 0.03416985759046703430, 0.03565186990008403778, 0.03639287605489253952, 0.03713388220970104819, 0.03787488836450954993, 0.03861589451931805861, 0.04009790682893510372, 0.04157991913855214883, 0.04306193144816919394, 0.04380293760297770955, 0.04454394375778623905, 0.04602595606740328416, 0.04750796837702032926 ),
 .UNSPECIFIED. ) ;
#964 = VERTEX_POINT ( 'NONE', #11816 ) ;
#965 = CARTESIAN_POINT ( 'NONE',  ( 643.1876992948947418, 1011.457451940551209, 704.5068267248690290 ) ) ;
#966 = DIRECTION ( 'NONE',  ( -1.000000000000000000, 0.000000000000000000, 0.000000000000000000 ) ) ;
#967 = DIRECTION ( 'NONE',  ( 0.000000000000000000, -1.000000000000000000, 0.000000000000000000 ) ) ;
#968 = CARTESIAN_POINT ( 'NONE',  ( -171.0950923142953570, 86.38958441093222973, -49.44577119986571745 ) ) ;
#969 = CIRCLE ( 'NONE', #42531, 0.3000000000000051514 ) ;
#970 = ITEM_DEFINED_TRANSFORMATION ( 'NONE', 'NONE', #20905,  #66832 ) ;
#971 = CARTESIAN_POINT ( 'NONE',  ( -179.1930439439409781, 94.15101626040424776, 87.59719074105936443 ) ) ;
#972 = ORIENTED_EDGE ( 'NONE', *, *, #43163, .F. ) ;
#973 = CARTESIAN_POINT ( 'NONE',  ( -120.1497954511983437, 42.82624472369557367, -47.26276959957558432 ) ) ;
#974 = CARTESIAN_POINT ( 'NONE',  ( -16.20761984364699870, -34.73915265837867850, 13.32819397642333037 ) ) ;
#975 = DIRECTION ( 'NONE',  ( 0.000000000000000000, 1.000000000000000000, -0.000000000000000000 ) ) ;
#976 = CARTESIAN_POINT ( 'NONE',  ( -58.00979178563811445, -29.32343869649178814, 170.0000000000000000 ) ) ;
#977 = B_SPLINE_CURVE_WITH_KNOTS ( 'NONE', 3,
 ( #65120, #65472, #59821, #42946, #10949, #11636, #44346, #64768, #17263, #27827, #54546, #27122, #33110, #17624, #39095, #33807, #59476, #6373, #37680, #53844, #16573, #60179, #26791, #12000, #33474, #60536, #54896, #6720, #5336, #11287, #48217, #28164, #59126, #42 ),
 .UNSPECIFIED., .F., .F.,
 ( 4, 2, 2, 2, 2, 2, 2, 2, 2, 2, 2, 2, 2, 2, 2, 2, 4 ),
 ( 0.01568356594869778006, 0.01666352729433787788, 0.01764348863997797917, 0.01862344998561807699, 0.01960341133125817828, 0.02058337267689827610, 0.02156333402253837739, 0.02254329536817847521, 0.02352325671381857303, 0.02450321805945867432, 0.02548317940509877561, 0.02646314075073887342, 0.02744310209637897124, 0.02842306344201907253, 0.02940302478765917035, 0.03038298613329926817, 0.03136294747893936946 ),
 .UNSPECIFIED. ) ;
#978 = DIRECTION ( 'NONE',  ( -0.000000000000000000, -1.000000000000000000, -0.000000000000000000 ) ) ;
#979 = ORIENTED_EDGE ( 'NONE', *, *, #14468, .F. ) ;
#980 = CARTESIAN_POINT ( 'NONE',  ( 1.219727444046191995E-16, -0.7818963812181061179, -8.000000000000000000 ) ) ;
#981 = CARTESIAN_POINT ( 'NONE',  ( 204.6977192012829789, 106.3443248447423315, -36.32593103262158252 ) ) ;
#982 = CARTESIAN_POINT ( 'NONE',  ( -150.3831389294225289, 66.25266777263973950, 30.76890096360532922 ) ) ;
#983 = LINE ( 'NONE', #36278, #21334 ) ;
#985 = ORIENTED_EDGE ( 'NONE', *, *, #35604, .F. ) ;
#984 = CARTESIAN_POINT ( 'NONE',  ( -5.000000000000073719, -41.66904755831212270, 0.000000000000000000 ) ) ;
#986 = EDGE_CURVE ( 'NONE', #12560, #40674, #59640, .T. ) ;
#987 = CARTESIAN_POINT ( 'NONE',  ( 175.8874477961783782, 74.89984466412605002, 69.08197011996692538 ) ) ;
#988 = VERTEX_POINT ( 'NONE', #32924 ) ;
#989 = VERTEX_POINT ( 'NONE', #6189 ) ;
#990 = CARTESIAN_POINT ( 'NONE',  ( -77.71448999903256549, 21.96089801565736011, -8.316135682572610932 ) ) ;
#991 = CARTESIAN_POINT ( 'NONE',  ( -37.36812455451343595, 11.66407928272600003, -91.89346562232887550 ) ) ;
#993 = ORIENTED_EDGE ( 'NONE', *, *, #35206, .T. ) ;
#992 = LINE ( 'NONE', #5563, #37617 ) ;
#994 = LINE ( 'NONE', #43880, #49914 ) ;
#995 = FACE_OUTER_BOUND ( 'NONE', #20434, .T. ) ;
#996 = CARTESIAN_POINT ( 'NONE',  ( -76.79042791651910704, 22.68960395613479974, -35.34994931789273664 ) ) ;
#997 = ORIENTED_EDGE ( 'NONE', *, *, #9206, .T. ) ;
#998 = CARTESIAN_POINT ( 'NONE',  ( 0.000000000000000000, 0.000000000000000000, 40.00000000000003553 ) ) ;
#999 = CARTESIAN_POINT ( 'NONE',  ( -38.16002576456688899, 10.79155573432543314, -19.31033324421229125 ) ) ;
#1000 = CARTESIAN_POINT ( 'NONE',  ( 151.0569594231044448, 52.83149886109547566, -93.40118860444637505 ) ) ;
#1001 = CARTESIAN_POINT ( 'NONE',  ( -38.55214349681828878, 10.86754840574841907, -72.09035779998554005 ) ) ;
#1002 = CARTESIAN_POINT ( 'NONE',  ( 23.09590709048885770, 7.852755081912512480, 66.06499266665456105 ) ) ;
#1003 = VERTEX_POINT ( 'NONE', #17080 ) ;
#1004 = ORIENTED_EDGE ( 'NONE', *, *, #19047, .F. ) ;
#1005 = ORIENTED_EDGE ( 'NONE', *, *, #14250, .F. ) ;
#1006 = DIRECTION ( 'NONE',  ( -0.000000000000000000, 1.000000000000000000, -0.000000000000000000 ) ) ;
#1007 = VECTOR ( 'NONE', #24608, 1000.000000000000000 ) ;
#1008 = LINE ( 'NONE', #43202, #21889 ) ;
#1009 = EDGE_CURVE ( 'NONE', #57581, #8542, #59993, .T. ) ;
#1010 = FACE_OUTER_BOUND ( 'NONE', #37761, .T. ) ;
#1011 = LINE ( 'NONE', #66095, #27707 ) ;
#1012 = CARTESIAN_POINT ( 'NONE',  ( -4.610955605662443446, -74.80943656680585718, 41.38025477438755928 ) ) ;
#1013 = FACE_OUTER_BOUND ( 'NONE', #13752, .T. ) ;
#1014 = CARTESIAN_POINT ( 'NONE',  ( -128.9786047358387009, 48.55852351614672102, 71.80467742803817544 ) ) ;
#1015 = CARTESIAN_POINT ( 'NONE',  ( -49.02322089375218184, 14.18221587516665494, 86.99932311603028268 ) ) ;
#1016 = EDGE_CURVE ( 'NONE', #28423, #15873, #49084, .T. ) ;
#1017 = CARTESIAN_POINT ( 'NONE',  ( 84.97343609940686804, 18.86260005312945154, 71.37542944298206748 ) ) ;
#1018 = ORIENTED_EDGE ( 'NONE', *, *, #5991, .T. ) ;
#1019 = DIRECTION ( 'NONE',  ( -1.000000000000000000, 0.000000000000000000, 0.000000000000000000 ) ) ;
#1021 = EDGE_LOOP ( 'NONE', ( #20694, #3514, #16394, #42951 ) ) ;
#1020 = EDGE_CURVE ( 'NONE', #49819, #55571, #66006, .T. ) ;
#1022 = CYLINDRICAL_SURFACE ( 'NONE', #19496, 7.500000000000013323 ) ;
#1023 = ORIENTED_EDGE ( 'NONE', *, *, #57399, .T. ) ;
#1024 = CARTESIAN_POINT ( 'NONE',  ( 210.5178985598940073, 114.6803933586780744, -65.93383091898544990 ) ) ;
#1025 = DIRECTION ( 'NONE',  ( -0.000000000000000000, 0.000000000000000000, 1.000000000000000000 ) ) ;
#1026 = CARTESIAN_POINT ( 'NONE',  ( 9.962235950564874543, 64.23203137738424573, 170.0000000000000000 ) ) ;
#1027 = CARTESIAN_POINT ( 'NONE',  ( -36.00055430895446307, 10.38468809415730831, -90.54901991010069651 ) ) ;
#1028 = EDGE_CURVE ( 'NONE', #17268, #36885, #19337, .T. ) ;
#1029 = CARTESIAN_POINT ( 'NONE',  ( 26.99999999999999645, -27.00000000000000355, 12.00000000000000000 ) ) ;
#1030 = CARTESIAN_POINT ( 'NONE',  ( 153.2384531768736338, 54.43344429203624202, -37.41481437027087509 ) ) ;
#1031 = LINE ( 'NONE', #55528, #43434 ) ;
#1032 = EDGE_LOOP ( 'NONE', ( #4642, #65171, #45931, #15526 ) ) ;
#1033 = CARTESIAN_POINT ( 'NONE',  ( 410.0000000000000000, -3.566368924055061292E-16, 174.3129005282752928 ) ) ;
#1034 = DIRECTION ( 'NONE',  ( -1.000000000000000000, 0.000000000000000000, 0.000000000000000000 ) ) ;
#1035 = VERTEX_POINT ( 'NONE', #14260 ) ;
#1036 = CARTESIAN_POINT ( 'NONE',  ( 0.6527133886630180903, -8.860760056385778682, -9.003039949738228742 ) ) ;
#1037 = ORIENTED_EDGE ( 'NONE', *, *, #10644, .F. ) ;
#1038 = CARTESIAN_POINT ( 'NONE',  ( -85.34215807311493052, 24.97769003780924280, 41.34574464142236394 ) ) ;
#1039 = CARTESIAN_POINT ( 'NONE',  ( -29.74902699556085039, 10.33856194202125245, -62.35061595289940328 ) ) ;
#1040 = CARTESIAN_POINT ( 'NONE',  ( 42.03719354205839664, 9.783015072457470040, 44.43989967554949772 ) ) ;
#1041 = CARTESIAN_POINT ( 'NONE',  ( -24.07146903340142785, 8.497560047608724076, 66.02689600193643571 ) ) ;
#1042 = CARTESIAN_POINT ( 'NONE',  ( -149.2910611247328347, 63.99625741915658494, 18.87627064943540134 ) ) ;
#1043 = EDGE_CURVE ( 'NONE', #48718, #23096, #46599, .T. ) ;
#1044 = EDGE_CURVE ( 'NONE', #21376, #7953, #3355, .T. ) ;
#1045 = EDGE_LOOP ( 'NONE', ( #10762, #53811 ) ) ;
#1046 = ORIENTED_EDGE ( 'NONE', *, *, #35292, .F. ) ;
#1047 = CARTESIAN_POINT ( 'NONE',  ( 31.11269837220803325, -15.55634918610409656, 2.000000000000001776 ) ) ;
#1048 = ORIENTED_EDGE ( 'NONE', *, *, #61066, .T. ) ;
#1049 = CARTESIAN_POINT ( 'NONE',  ( 157.4703587214989113, 58.92748579479258808, -24.27963370867398396 ) ) ;
#1050 = DIRECTION ( 'NONE',  ( 0.000000000000000000, 0.000000000000000000, 1.000000000000000000 ) ) ;
#1051 = CARTESIAN_POINT ( 'NONE',  ( 63.01563776193091826, 12.67277567978498176, 56.65751152968497451 ) ) ;
#1052 = CARTESIAN_POINT ( 'NONE',  ( -0.9897066053608937208, 7.549089325901769065, 61.36437911206027707 ) ) ;
#1053 = LINE ( 'NONE', #32712, #68406 ) ;
#1054 = CARTESIAN_POINT ( 'NONE',  ( 32.12337157895397866, -170.0000000000000000, -95.00000000000133582 ) ) ;
#1055 = EDGE_LOOP ( 'NONE', ( #53256, #11888, #11752, #31216 ) ) ;
#1056 = CYLINDRICAL_SURFACE ( 'NONE', #3184, 5.000000000000018652 ) ;
#1057 = ORIENTED_EDGE ( 'NONE', *, *, #9172, .F. ) ;
#1058 = VECTOR ( 'NONE', #1739, 1000.000000000000000 ) ;
#1059 = ORIENTED_EDGE ( 'NONE', *, *, #35607, .F. ) ;
#1060 = FACE_OUTER_BOUND ( 'NONE', #18651, .T. ) ;
#1061 = DIRECTION ( 'NONE',  ( 0.000000000000000000, 0.000000000000000000, 1.000000000000000000 ) ) ;
#1062 = FACE_OUTER_BOUND ( 'NONE', #64312, .T. ) ;
#1063 = CARTESIAN_POINT ( 'NONE',  ( 134.7720294983483029, 43.15885542353191084, 17.62355008800678746 ) ) ;
#1064 = CARTESIAN_POINT ( 'NONE',  ( 9.068001575458771057, -57.63052812422861138, 27.58472369369409094 ) ) ;
#1065 = CIRCLE ( 'NONE', #56102, 243.4957430088094839 ) ;
#1066 = ORIENTED_EDGE ( 'NONE', *, *, #15157, .T. ) ;
#1067 = DIRECTION ( 'NONE',  ( 0.000000000000000000, 1.000000000000000000, 0.000000000000000000 ) ) ;
#1068 = EDGE_LOOP ( 'NONE', ( #54688, #23963, #14484, #64716 ) ) ;
#1069 = CARTESIAN_POINT ( 'NONE',  ( -75.43044859198180063, 21.11535168543638363, 44.68847691565546398 ) ) ;
#1070 = ORIENTED_EDGE ( 'NONE', *, *, #17625, .F. ) ;
#1071 = DIRECTION ( 'NONE',  ( 1.000000000000000000, 0.000000000000000000, 0.000000000000000000 ) ) ;
#1072 = EDGE_LOOP ( 'NONE', ( #4972, #45772, #7897, #719 ) ) ;
#1073 = CARTESIAN_POINT ( 'NONE',  ( -31.90315521289150524, 56.64813493366005304, 41.38025477438755928 ) ) ;
#1074 = CIRCLE ( 'NONE', #13440, 25.12245591505646303 ) ;
#1075 = CARTESIAN_POINT ( 'NONE',  ( 94.07616572255075482, 22.09777530676769075, 9.343156713767100996 ) ) ;
#1076 = DIRECTION ( 'NONE',  ( 0.000000000000000000, 0.000000000000000000, 1.000000000000000000 ) ) ;
#1077 = ORIENTED_EDGE ( 'NONE', *, *, #16773, .T. ) ;
#1078 = CARTESIAN_POINT ( 'NONE',  ( -447.6627218934918346, 392.9289321881408910, -141.4497041420121661 ) ) ;
#1079 = CARTESIAN_POINT ( 'NONE',  ( -4.999999999999936939, 36.11269837220805812, 85.00100000000000477 ) ) ;
#1080 = CARTESIAN_POINT ( 'NONE',  ( 33.46033188299907835, 8.722678254080106441, 32.83038915614411479 ) ) ;
#1081 = CARTESIAN_POINT ( 'NONE',  ( -176.3763474213711504, 92.36993073950279154, -48.98273591874998800 ) ) ;
#1082 = CARTESIAN_POINT ( 'NONE',  ( -128.7810612886106014, 48.42424427998343361, -22.49492442257137270 ) ) ;
#1083 = LINE ( 'NONE', #49599, #33421 ) ;
#1084 = CYLINDRICAL_SURFACE ( 'NONE', #16978, 5.000000000000004441 ) ;
#1085 = VERTEX_POINT ( 'NONE', #8291 ) ;
#1086 = LINE ( 'NONE', #49961, #626 ) ;
#1087 = CARTESIAN_POINT ( 'NONE',  ( -51.66904755831212981, -15.55634918610397222, 0.000000000000000000 ) ) ;
#1088 = B_SPLINE_CURVE_WITH_KNOTS ( 'NONE', 3,
 ( #39692, #51297, #61148, #29140, #22816, #34436 ),
 .UNSPECIFIED., .F., .F.,
 ( 4, 2, 4 ),
 ( 1.095770181107971388E-06, 0.03239442681617708819, 0.06478775786217308430 ),
 .UNSPECIFIED. ) ;
#1089 = ORIENTED_EDGE ( 'NONE', *, *, #65531, .F. ) ;
#1090 = VECTOR ( 'NONE', #39346, 1000.000000000000000 ) ;
#1091 = FACE_BOUND ( 'NONE', #30911, .T. ) ;
#1092 = CARTESIAN_POINT ( 'NONE',  ( -6.851003965218987801, 6.829052369041587411, -77.21532479566432983 ) ) ;
#1093 = CARTESIAN_POINT ( 'NONE',  ( -177.1381400275771796, 93.26609858452819424, 58.81773603299666320 ) ) ;
#1094 = DIRECTION ( 'NONE',  ( -1.000000000000000000, 0.000000000000000000, 0.000000000000000000 ) ) ;
#1095 = CARTESIAN_POINT ( 'NONE',  ( -124.7710763417278486, 46.96042092553523162, -49.83267132162298196 ) ) ;
#1096 = DIRECTION ( 'NONE',  ( -0.5877852522924686962, -0.8090169943749506709, 2.500042656554809354E-16 ) ) ;
#1097 = DIRECTION ( 'NONE',  ( 1.000000000000000000, 0.000000000000000000, 0.000000000000000000 ) ) ;
#1098 = DIRECTION ( 'NONE',  ( -4.906538933386759377E-15, 0.7071067811865474617, 0.7071067811865474617 ) ) ;
#1099 = CARTESIAN_POINT ( 'NONE',  ( -75.76780310373240468, 21.23838321961104469, -89.37419894888229521 ) ) ;
#1100 = EDGE_CURVE ( 'NONE', #68856, #49636, #25515, .T. ) ;
#1101 = CARTESIAN_POINT ( 'NONE',  ( -7.825402957745081878, 7.899365992529270741, 30.11558103944718923 ) ) ;
#1102 = CARTESIAN_POINT ( 'NONE',  ( 116.0773578185793440, 31.67580513411751753, 5.527550488222392033 ) ) ;
#1103 = CARTESIAN_POINT ( 'NONE',  ( 86.62931800182292363, 20.48449268398422163, -8.977013608448025650 ) ) ;
#1104 = VERTEX_POINT ( 'NONE', #35367 ) ;
#1105 = CARTESIAN_POINT ( 'NONE',  ( -20.63749999999999929, 2.574819895207310592E-15, 21.02500000000000213 ) ) ;
#1106 = ORIENTED_EDGE ( 'NONE', *, *, #20088, .F. ) ;
#1107 = CARTESIAN_POINT ( 'NONE',  ( -443.8115333961470128, 394.8687311169578606, 93.62756966056487329 ) ) ;
#1108 = B_SPLINE_CURVE_WITH_KNOTS ( 'NONE', 3,
 ( #42123, #58294, #5180, #69193, #63582, #31920, #4829, #39199, #65944, #31569, #21019, #64265, #60640, #53349, #55003, #38486, #48074, #12457, #6484, #53005, #21350, #20664, #33917, #58630, #63923, #10446, #49720, #38851, #36853, #42798, #16073, #10112, #4493, #42464, #11746, #68841, #1549, #26301, #47385, #47730, #60295, #27932, #54657, #15735, #33226 ),
 .UNSPECIFIED., .F., .F.,
 ( 4, 2, 2, 2, 2, 2, 2, 2, 1, 2, 2, 2, 2, 2, 2, 2, 2, 2, 2, 2, 2, 2, 4 ),
 ( 0.000000000000000000, 0.001470449819620711336, 0.002205674729431056705, 0.002940899639241401856, 0.004411349458862072644, 0.005881799278482742997, 0.007352249098103413351, 0.008087474007913748528, 0.008822698917724084572, 0.009557923827534418881, 0.01029314873734475319, 0.01176359855696538191, 0.01249882346677569887, 0.01323404837658601410, 0.01470449819620668792, 0.01543972310601701009, 0.01617494801582733052, 0.01764539783544796792, 0.01911584765506860531, 0.01985107256487892574, 0.02058629747468924617, 0.02205674729430989051, 0.02352719711393053484 ),
 .UNSPECIFIED. ) ;
#1109 = CIRCLE ( 'NONE', #48227, 21.99999999999998579 ) ;
#1110 = CARTESIAN_POINT ( 'NONE',  ( 81.76212856587197564, 18.87332718082994987, -75.87751552093126861 ) ) ;
#1111 = CARTESIAN_POINT ( 'NONE',  ( 117.5606386312644247, 33.54431188492876714, 92.48088064648997886 ) ) ;
#1112 = CYLINDRICAL_SURFACE ( 'NONE', #66073, 7.500000000000020428 ) ;
#1113 = EDGE_CURVE ( 'NONE', #57471, #44581, #10986, .T. ) ;
#1114 = CARTESIAN_POINT ( 'NONE',  ( 65.41496713438823463, 13.24164235279043744, -9.253839073797927028 ) ) ;
#1116 = CARTESIAN_POINT ( 'NONE',  ( -29.74902699556085039, 10.33856194202125245, -35.50606536243572009 ) ) ;
#1115 = AXIS2_PLACEMENT_3D ( 'NONE', #49664, #60929, #1492 ) ;
#1117 = CARTESIAN_POINT ( 'NONE',  ( -125.8938041572051105, 46.49392987655492959, -23.06915330777029638 ) ) ;
#1118 = CARTESIAN_POINT ( 'NONE',  ( 109.9975424824652634, 296.0000000000000000, 529.9060149868646477 ) ) ;
#1119 = CARTESIAN_POINT ( 'NONE',  ( -190.6985136298601731, 109.1272424661242582, -73.40678087856149148 ) ) ;
#1120 = ORIENTED_EDGE ( 'NONE', *, *, #63162, .F. ) ;
#1121 = ORIENTED_EDGE ( 'NONE', *, *, #19516, .T. ) ;
#1122 = LINE ( 'NONE', #17650, #64641 ) ;
#1123 = LINE ( 'NONE', #12371, #41190 ) ;
#1124 = DIRECTION ( 'NONE',  ( -0.3513748240813305279, -0.9362348706397417564, 5.102127870520021228E-18 ) ) ;
#1125 = CARTESIAN_POINT ( 'NONE',  ( -165.7140086129057011, 80.68381997492575408, 63.95079900650693361 ) ) ;
#1126 = LINE ( 'NONE', #65145, #9413 ) ;
#1127 = ADVANCED_FACE ( 'NONE', ( #53591 ), #52006, .T. ) ;
#1128 = DIRECTION ( 'NONE',  ( -1.000000000000000000, 1.232595164407830946E-32, 7.703719777548943412E-34 ) ) ;
#1129 = ORIENTED_EDGE ( 'NONE', *, *, #8619, .F. ) ;
#1130 = CARTESIAN_POINT ( 'NONE',  ( 104.4006536356073980, 27.36759527624478139, -48.15181421002847628 ) ) ;
#1131 = CARTESIAN_POINT ( 'NONE',  ( 188.2091813586561102, 87.61952156613880049, -14.52189767635950091 ) ) ;
#1132 = CARTESIAN_POINT ( 'NONE',  ( -84.96580414052108665, 24.82184094495578108, -11.69303817377454635 ) ) ;
#1133 = CARTESIAN_POINT ( 'NONE',  ( -447.6627218934914367, 399.9999999999998863, -136.4497041420118251 ) ) ;
#1134 = CARTESIAN_POINT ( 'NONE',  ( 46.42281973867195433, 9.426811321855149473, -13.62602333367861007 ) ) ;
#1135 = CARTESIAN_POINT ( 'NONE',  ( 207.8675797643809915, 110.7908513421271977, -10.17102767663917540 ) ) ;
#1136 = FACE_BOUND ( 'NONE', #24883, .T. ) ;
#1137 = CARTESIAN_POINT ( 'NONE',  ( 157.9121974517528599, 59.27335488206246339, 56.25401806271705141 ) ) ;
#1138 = ORIENTED_EDGE ( 'NONE', *, *, #24887, .T. ) ;
#1139 = DIRECTION ( 'NONE',  ( -0.000000000000000000, -1.000000000000000000, 0.000000000000000000 ) ) ;
#1140 = CARTESIAN_POINT ( 'NONE',  ( 93.08073375333745503, 22.79826000593201485, -47.15458855754309297 ) ) ;
#1141 = LINE ( 'NONE', #39137, #57724 ) ;
#1142 = CARTESIAN_POINT ( 'NONE',  ( -180.6209674222602075, 97.47999311542515954, 11.31048516350536381 ) ) ;
#1143 = CYLINDRICAL_SURFACE ( 'NONE', #35228, 65.36598343705435354 ) ;
#1144 = CONICAL_SURFACE ( 'NONE', #55059, 65.00000000000000000, 0.7853981633974497223 ) ;
#1145 = DIRECTION ( 'NONE',  ( -0.000000000000000000, -0.7071067811865474617, 0.7071067811865474617 ) ) ;
#1146 = VERTEX_POINT ( 'NONE', #15293 ) ;
#1147 = CARTESIAN_POINT ( 'NONE',  ( 55.51547041749727640, 11.05727559334830090, 10.22624786746376735 ) ) ;
#1148 = CARTESIAN_POINT ( 'NONE',  ( -1.666933348992581942, 64.97862212458815634, 40.00000000000003553 ) ) ;
#1149 = VERTEX_POINT ( 'NONE', #58195 ) ;
#1150 = EDGE_LOOP ( 'NONE', ( #20877, #65074, #12430, #64337 ) ) ;
#1151 = CARTESIAN_POINT ( 'NONE',  ( 0.000000000000000000, -6.928203230275503444, 4.000000000000010658 ) ) ;
#1152 = CARTESIAN_POINT ( 'NONE',  ( -28.30427060690011132, -69.40159203110334829, 41.38025477438755928 ) ) ;
#1153 = CARTESIAN_POINT ( 'NONE',  ( 89.20981392318256553, 21.38519354635262459, -63.11988782574987056 ) ) ;
#1154 = ORIENTED_EDGE ( 'NONE', *, *, #54505, .F. ) ;
#1155 = ORIENTED_EDGE ( 'NONE', *, *, #59225, .F. ) ;
#1156 = CARTESIAN_POINT ( 'NONE',  ( -41.50537345350635121, -50.04124777106354571, 3.061616997868437868E-16 ) ) ;
#1157 = CARTESIAN_POINT ( 'NONE',  ( 164.9540180502650912, 65.02981548735056094, 37.47792873164053873 ) ) ;
#1158 = AXIS2_PLACEMENT_3D ( 'NONE', #24010, #19073, #25057 ) ;
#1159 = CARTESIAN_POINT ( 'NONE',  ( 104.4006536356074264, 27.36759527624477073, 5.537286970898872340 ) ) ;
#1160 = DIRECTION ( 'NONE',  ( 1.232595164407830946E-32, 1.000000000000000000, 3.469446951953615421E-17 ) ) ;
#1161 = CARTESIAN_POINT ( 'NONE',  ( 1.667562369266827327, 64.99262834925669097, 170.0000000000000000 ) ) ;
#1162 = EDGE_CURVE ( 'NONE', #19726, #7734, #16319, .T. ) ;
#1164 = EDGE_CURVE ( 'NONE', #53174, #39681, #69076, .T. ) ;
#1163 = CARTESIAN_POINT ( 'NONE',  ( 106.6181401479172308, 28.34160787025143335, -10.00766880435194217 ) ) ;
#1165 = DIRECTION ( 'NONE',  ( 0.000000000000000000, 0.000000000000000000, -1.000000000000000000 ) ) ;
#1166 = CARTESIAN_POINT ( 'NONE',  ( -130.2071229607962550, 50.62285182196875155, -9.415733337548060078 ) ) ;
#1167 = CARTESIAN_POINT ( 'NONE',  ( -155.8069098289708165, 71.07457338077841769, -91.92448083599751385 ) ) ;
#1168 = CARTESIAN_POINT ( 'NONE',  ( 70.34686579112866411, -18.11777090454118877, 41.38025477438755928 ) ) ;
#1169 = CARTESIAN_POINT ( 'NONE',  ( 92.91022130985207639, 21.66059330820416307, 94.99999999999866418 ) ) ;
#1171 = ORIENTED_EDGE ( 'NONE', *, *, #16376, .T. ) ;
#1170 = CARTESIAN_POINT ( 'NONE',  ( -190.6985136298601731, 109.1272424661242582, 87.66052266422059347 ) ) ;
#1172 = VERTEX_POINT ( 'NONE', #37776 ) ;
#1173 = VECTOR ( 'NONE', #25176, 1000.000000000000000 ) ;
#1174 = VERTEX_POINT ( 'NONE', #20912 ) ;
#1175 = CARTESIAN_POINT ( 'NONE',  ( -12.39701069459754201, 7.231688578592713412, -22.03915780541799663 ) ) ;
#1176 = CARTESIAN_POINT ( 'NONE',  ( -48.04019567818504299, 12.91272349839804434, 40.48869681787067520 ) ) ;
#1177 = CARTESIAN_POINT ( 'NONE',  ( 10.55634918610400419, -10.55634918610406281, 2.000000000000001776 ) ) ;
#1178 = LINE ( 'NONE', #22633, #24273 ) ;
#1179 = ADVANCED_FACE ( 'NONE', ( #58526 ), #31810, .F. ) ;
#1180 = CARTESIAN_POINT ( 'NONE',  ( -34.74563762132953570, 11.17960945723135602, 71.29720797180668512 ) ) ;
#1181 = EDGE_CURVE ( 'NONE', #67595, #55797, #53243, .T. ) ;
#1182 = CARTESIAN_POINT ( 'NONE',  ( 47.70222499156757578, 57.81185381817647340, 41.38025477438755928 ) ) ;
#1183 = CARTESIAN_POINT ( 'NONE',  ( -75.01314391403411719, 20.96328762434828263, -76.02809170986127185 ) ) ;
#1184 = CARTESIAN_POINT ( 'NONE',  ( 19.54475376904848005, 6.649964688461121654, -9.678301494481228673 ) ) ;
#1185 = ORIENTED_EDGE ( 'NONE', *, *, #50012, .T. ) ;
#1186 = FACE_BOUND ( 'NONE', #2757, .T. ) ;
#1187 = VERTEX_POINT ( 'NONE', #69435 ) ;
#1188 = EDGE_LOOP ( 'NONE', ( #37725, #12945, #49340, #52870, #24655, #3201, #47835, #3664 ) ) ;
#1189 = CARTESIAN_POINT ( 'NONE',  ( -143.8756912989387047, 60.83492035645719653, 16.33554224011767175 ) ) ;
#1190 = SURFACE_STYLE_FILL_AREA ( #60284 ) ;
#1191 = CARTESIAN_POINT ( 'NONE',  ( -28.32971103059306373, 10.11911997875206204, 84.57276817772938671 ) ) ;
#1192 = EDGE_CURVE ( 'NONE', #19369, #63634, #42702, .T. ) ;
#1193 = VECTOR ( 'NONE', #59745, 1000.000000000000000 ) ;
#1194 = CARTESIAN_POINT ( 'NONE',  ( -95.52163045714284806, 29.47808868198299237, -45.77603188274618873 ) ) ;
#1195 = CARTESIAN_POINT ( 'NONE',  ( -109.7290872258107015, 36.72869630780159156, 10.15525318343610728 ) ) ;
#1196 = CARTESIAN_POINT ( 'NONE',  ( 15.29912143387263690, 7.491799981865499447, -50.51894409868582159 ) ) ;
#1197 = DIRECTION ( 'NONE',  ( -0.000000000000000000, -0.000000000000000000, -1.000000000000000000 ) ) ;
#1198 = VERTEX_POINT ( 'NONE', #53931 ) ;
#1199 = ORIENTED_EDGE ( 'NONE', *, *, #5184, .F. ) ;
#1200 = ORIENTED_EDGE ( 'NONE', *, *, #38790, .T. ) ;
#1201 = DIRECTION ( 'NONE',  ( -0.5773502691896255090, -0.5773502691896258421, 0.5773502691896258421 ) ) ;
#1202 = DIRECTION ( 'NONE',  ( 0.000000000000000000, 1.000000000000000000, -0.000000000000000000 ) ) ;
#1203 = DIRECTION ( 'NONE',  ( -1.000000000000000000, 0.000000000000000000, 0.000000000000000000 ) ) ;
#1204 = CARTESIAN_POINT ( 'NONE',  ( 59.29597493004737885, 11.84030339376940510, -9.845320537704525421 ) ) ;
#1205 = ADVANCED_FACE ( 'NONE', ( #15972 ), #37421, .F. ) ;
#1206 = CARTESIAN_POINT ( 'NONE',  ( -47.56463531432804359, 12.80077789972090230, 38.30749179624960021 ) ) ;
#1207 = ADVANCED_FACE ( 'NONE', ( #57854, #55337, #28257, #1186, #27560 ), #44439, .F. ) ;
#1208 = CARTESIAN_POINT ( 'NONE',  ( 197.1975259970231775, 98.19639476549650681, 63.87880983231196552 ) ) ;
#1209 = EDGE_CURVE ( 'NONE', #16807, #23774, #1533, .T. ) ;
#1210 = ORIENTED_EDGE ( 'NONE', *, *, #24253, .T. ) ;
#1211 = CARTESIAN_POINT ( 'NONE',  ( 39.40195752203892710, -170.0000000000000000, -8.775266874964069430 ) ) ;
#1212 = CARTESIAN_POINT ( 'NONE',  ( -150.3898662070192245, 64.92828409760430475, 72.56537183036274996 ) ) ;
#1213 = CARTESIAN_POINT ( 'NONE',  ( -177.2385321673936858, 68.86478131554719084, 177.4362760962257539 ) ) ;
#1214 = CARTESIAN_POINT ( 'NONE',  ( -5.417282889646088506, 7.753782747238989970, -35.81092865362596456 ) ) ;
#1215 = LINE ( 'NONE', #65590, #12769 ) ;
#1216 = CARTESIAN_POINT ( 'NONE',  ( -165.7447522913192586, 79.27610653780159566, -94.42765512978321851 ) ) ;
#1217 = FACE_OUTER_BOUND ( 'NONE', #47662, .T. ) ;
#1218 = FACE_BOUND ( 'NONE', #61286, .T. ) ;
#1219 = CARTESIAN_POINT ( 'NONE',  ( 5.799999999999999822, 0.000000000000000000, 0.000000000000000000 ) ) ;
#1220 = CARTESIAN_POINT ( 'NONE',  ( 9.416656162223560500, 6.380306691996769253, -65.89949783066536781 ) ) ;
#1221 = ORIENTED_EDGE ( 'NONE', *, *, #61362, .T. ) ;
#1222 = CARTESIAN_POINT ( 'NONE',  ( 2.337278106504167230, 395.0000000000000000, -341.4497041420117966 ) ) ;
#1223 = AXIS2_PLACEMENT_3D ( 'NONE', #64449, #31748, #54221 ) ;
#1224 = CARTESIAN_POINT ( 'NONE',  ( -128.1219934350341703, 47.97781708504715681, -62.08223023690383258 ) ) ;
#1225 = FACE_OUTER_BOUND ( 'NONE', #13546, .T. ) ;
#1226 = CARTESIAN_POINT ( 'NONE',  ( -31.11269837220801193, 31.11269837220812207, 2.000000000000001776 ) ) ;
#1227 = CARTESIAN_POINT ( 'NONE',  ( 59.94652978725887493, 13.01168383647461724, -63.21766814124692502 ) ) ;
#1228 = ORIENTED_EDGE ( 'NONE', *, *, #39925, .F. ) ;
#1229 = PRESENTATION_LAYER_ASSIGNMENT (  '', '', ( #61878 ) ) ;
#1230 = ORIENTED_EDGE ( 'NONE', *, *, #60967, .T. ) ;
#1231 = LINE ( 'NONE', #29025, #57253 ) ;
#1232 = CARTESIAN_POINT ( 'NONE',  ( 182.3693118667488875, 79.91269779363329917, 83.08661189630149124 ) ) ;
#1233 = EDGE_LOOP ( 'NONE', ( #15909, #46873 ) ) ;
#1234 = AXIS2_PLACEMENT_3D ( 'NONE', #59286, #59624, #6531 ) ;
#1235 = VERTEX_POINT ( 'NONE', #11731 ) ;
#1236 = CARTESIAN_POINT ( 'NONE',  ( 174.1364721914477229, 71.85829564941445824, -46.56446820418197774 ) ) ;
#1237 = LINE ( 'NONE', #11423, #47052 ) ;
#1238 = ORIENTED_EDGE ( 'NONE', *, *, #47800, .F. ) ;
#1239 = DIRECTION ( 'NONE',  ( 0.7071067811865474617, -0.7071067811865474617, -0.000000000000000000 ) ) ;
#1240 = DIRECTION ( 'NONE',  ( -0.1342332658176667304, 0.9909497617679331460, 0.000000000000000000 ) ) ;
#1241 = CARTESIAN_POINT ( 'NONE',  ( -75.01314391403410298, 20.96328762434827908, -49.18354111939758155 ) ) ;
#1242 = VECTOR ( 'NONE', #52232, 1000.000000000000000 ) ;
#1243 = CARTESIAN_POINT ( 'NONE',  ( -25.87147652227456263, 70.00000000000000000, 129.5802547743875550 ) ) ;
#1244 = CARTESIAN_POINT ( 'NONE',  ( 86.62931800182292363, 19.42108912189597092, -35.82156419891171595 ) ) ;
#1245 = CARTESIAN_POINT ( 'NONE',  ( -50.14523569787234436, 14.45648954445650247, -21.56493559798800774 ) ) ;
#1246 = EDGE_CURVE ( 'NONE', #2785, #21253, #66340, .T. ) ;
#1247 = ORIENTED_EDGE ( 'NONE', *, *, #46850, .F. ) ;
#1249 = ADVANCED_FACE ( 'NONE', ( #66278 ), #33203, .F. ) ;
#1248 = FACE_OUTER_BOUND ( 'NONE', #33448, .T. ) ;
#1250 = FACE_BOUND ( 'NONE', #49319, .T. ) ;
#1251 = CARTESIAN_POINT ( 'NONE',  ( -143.3980294393558950, 60.45217072626394383, -46.67054387122288261 ) ) ;
#1252 = CARTESIAN_POINT ( 'NONE',  ( -167.6524579626394598, 82.69702609844095775, -74.19494829241439504 ) ) ;
#1254 = VERTEX_POINT ( 'NONE', #27212 ) ;
#1253 = CARTESIAN_POINT ( 'NONE',  ( -121.5946276578746534, 43.72760306970064192, 85.65620857137692212 ) ) ;
#1255 = CARTESIAN_POINT ( 'NONE',  ( 56.94505604581133440, 12.37336791557970450, 6.057149477580686003 ) ) ;
#1256 = ORIENTED_EDGE ( 'NONE', *, *, #41395, .F. ) ;
#1257 = CARTESIAN_POINT ( 'NONE',  ( -132.9409505933031710, 51.31241517713430511, 35.50028265355906143 ) ) ;
#1258 = CARTESIAN_POINT ( 'NONE',  ( 14.59045944429412600, 20.30070179093326743, 0.000000000000000000 ) ) ;
#1259 = FACE_OUTER_BOUND ( 'NONE', #14240, .T. ) ;
#1260 = EDGE_CURVE ( 'NONE', #42425, #65549, #28621, .T. ) ;
#1261 = DIRECTION ( 'NONE',  ( 0.000000000000000000, 0.000000000000000000, 1.000000000000000000 ) ) ;
#1262 = EDGE_CURVE ( 'NONE', #23524, #39998, #319, .T. ) ;
#1263 = CARTESIAN_POINT ( 'NONE',  ( 81.74909803672915132, 17.81295302817861526, -22.19359623302083051 ) ) ;
#1264 = DIRECTION ( 'NONE',  ( -3.081487911019579554E-32, -1.000000000000000000, -3.469446951953612956E-17 ) ) ;
#1265 = CARTESIAN_POINT ( 'NONE',  ( 88.28780346671263146, 19.99350429399657614, -77.48438020982086982 ) ) ;
#1266 = DIRECTION ( 'NONE',  ( -0.000000000000000000, -0.000000000000000000, 1.000000000000000000 ) ) ;
#1267 = CARTESIAN_POINT ( 'NONE',  ( 427.4999999999999432, 207.5000000000000284, 20.00000000000000000 ) ) ;
#1268 = EDGE_LOOP ( 'NONE', ( #11768, #41933, #16549, #1900 ) ) ;
#1269 = ORIENTED_EDGE ( 'NONE', *, *, #19129, .T. ) ;
#1270 = EDGE_CURVE ( 'NONE', #30832, #4530, #489, .T. ) ;
#1271 = VECTOR ( 'NONE', #7727, 1000.000000000000000 ) ;
#1272 = CARTESIAN_POINT ( 'NONE',  ( 60.58000000000000540, -36.09918303830819752, 15.41169613715280562 ) ) ;
#1273 = DIRECTION ( 'NONE',  ( -0.000000000000000000, 1.000000000000000000, -0.000000000000000000 ) ) ;
#1274 = FACE_OUTER_BOUND ( 'NONE', #43238, .T. ) ;
#1275 = LINE ( 'NONE', #22730, #301 ) ;
#1276 = CARTESIAN_POINT ( 'NONE',  ( 210.6584452238135157, 116.7138338345753823, -48.40461618372044938 ) ) ;
#1277 = AXIS2_PLACEMENT_3D ( 'NONE', #30478, #35064, #25562 ) ;
#1278 = CARTESIAN_POINT ( 'NONE',  ( 18.66447740837935854, 37.32227262710744498, 13.79046412339527805 ) ) ;
#1279 = CARTESIAN_POINT ( 'NONE',  ( -109.6660553119434951, 36.69391917620598775, 66.19210472742473428 ) ) ;
#1280 = CARTESIAN_POINT ( 'NONE',  ( -27.70005010046225991, 9.007417901453015574, -36.31107217152676014 ) ) ;
#1281 = CARTESIAN_POINT ( 'NONE',  ( -26.00000000000000000, 0.000000000000000000, -2.818925648462311923E-15 ) ) ;
#1282 = PRODUCT_DEFINITION_SHAPE ( 'NONE', 'NONE',  #69573 ) ;
#1283 = EDGE_LOOP ( 'NONE', ( #47982, #4355, #44982, #36285 ) ) ;
#1284 = LINE ( 'NONE', #28007, #53475 ) ;
#1285 = EDGE_LOOP ( 'NONE', ( #47174, #10231, #18565, #33399, #41316, #43548, #36520, #6805, #23132 ) ) ;
#1286 = AXIS2_PLACEMENT_3D ( 'NONE', #32056, #27454, #22537 ) ;
#1287 = AXIS2_PLACEMENT_3D ( 'NONE', #68840, #30886, #67483 ) ;
#1288 = CARTESIAN_POINT ( 'NONE',  ( -10.23867141318106455, 7.059827648235818209, -50.03618833735410476 ) ) ;
#1289 = DIRECTION ( 'NONE',  ( 1.000000000000000000, 0.000000000000000000, -0.000000000000000000 ) ) ;
#1290 = LINE ( 'NONE', #61422, #65606 ) ;
#1291 = CARTESIAN_POINT ( 'NONE',  ( 132.9557829392755082, 42.05591979570418459, 29.55064835711428017 ) ) ;
#1292 = CARTESIAN_POINT ( 'NONE',  ( 35.65622260226242446, 8.964590916200316784, 17.07156420890763115 ) ) ;
#1293 = DIRECTION ( 'NONE',  ( 1.000000000000000000, -0.000000000000000000, 0.000000000000000000 ) ) ;
#1294 = PLANE ( 'NONE',  #9088 ) ;
#1295 = ADVANCED_FACE ( 'NONE', ( #22639 ), #18070, .T. ) ;
#1296 = ADVANCED_FACE ( 'NONE', ( #39520 ), #6806, .T. ) ;
#1297 = CARTESIAN_POINT ( 'NONE',  ( 63.01563776193091826, 13.70579113808094895, 29.81296093922127710 ) ) ;
#1298 = CARTESIAN_POINT ( 'NONE',  ( -29.72794928047597551, -29.28418875150963174, 13.79046340968179329 ) ) ;
#1299 = ORIENTED_EDGE ( 'NONE', *, *, #69235, .F. ) ;
#1300 = CARTESIAN_POINT ( 'NONE',  ( 58.46823952472682606, 12.69204591816735572, 70.14181518529996140 ) ) ;
#1301 = CARTESIAN_POINT ( 'NONE',  ( 329.1355598199468204, 190.0000000000000000, -129.5087625010780812 ) ) ;
#1303 = EDGE_CURVE ( 'NONE', #59205, #889, #60969, .T. ) ;
#1302 = CARTESIAN_POINT ( 'NONE',  ( -13.77312480593388777, 8.361845410302541026, 6.195500647299365227 ) ) ;
#1304 = CARTESIAN_POINT ( 'NONE',  ( 284.9999364138627129, -21.99998554860538391, -0.3278620034596229083 ) ) ;
#1305 = CARTESIAN_POINT ( 'NONE',  ( 19.62566184736102315, -15.48655536434847413, 0.000000000000000000 ) ) ;
#1306 = CARTESIAN_POINT ( 'NONE',  ( 80.27480108964937244, 18.40368268764104442, 86.90318297740122944 ) ) ;
#1307 = EDGE_LOOP ( 'NONE', ( #35299, #10153, #10005, #63339 ) ) ;
#1308 = CARTESIAN_POINT ( 'NONE',  ( 403.0071894358310374, 610.4960000259681010, 569.0068267248719849 ) ) ;
#1309 = CARTESIAN_POINT ( 'NONE',  ( -125.8938041572051389, 47.69968343338778993, 57.46449846362076386 ) ) ;
#1310 = CARTESIAN_POINT ( 'NONE',  ( -132.2352756077771687, 50.81350938245626025, 7.262685974171482428 ) ) ;
#1311 = CARTESIAN_POINT ( 'NONE',  ( -169.1116812882276008, 84.24296059722693997, -35.85782011543879122 ) ) ;
#1312 = CARTESIAN_POINT ( 'NONE',  ( -130.2071229607962550, 50.62285182196873734, -36.26028392801173084 ) ) ;
#1313 = VERTEX_POINT ( 'NONE', #43729 ) ;
#1314 = CARTESIAN_POINT ( 'NONE',  ( -118.6849742182705114, 41.92701402439732306, -40.32728246622576052 ) ) ;
#1315 = PLANE ( 'NONE',  #1532 ) ;
#1316 = DIRECTION ( 'NONE',  ( -0.000000000000000000, 1.000000000000000000, -0.000000000000000000 ) ) ;
#1317 = DIRECTION ( 'NONE',  ( -0.000000000000000000, 1.000000000000000000, -0.000000000000000000 ) ) ;
#1318 = DIRECTION ( 'NONE',  ( -0.000000000000000000, -0.000000000000000000, -1.000000000000000000 ) ) ;
#1319 = ORIENTED_EDGE ( 'NONE', *, *, #24301, .T. ) ;
#1320 = CARTESIAN_POINT ( 'NONE',  ( -60.95805269991219433, 17.39401718769329719, 6.342651992393583349 ) ) ;
#1321 = CARTESIAN_POINT ( 'NONE',  ( 199.7255144154429161, 99.76581417577205002, -49.45988108201962774 ) ) ;
#1322 = CARTESIAN_POINT ( 'NONE',  ( -95.63694837622348643, 30.64472169584718841, 41.50935696543631082 ) ) ;
#1323 = TOROIDAL_SURFACE ( 'NONE', #20399, 22.50000000000000000, 1.500000000000000444 ) ;
#1324 = CARTESIAN_POINT ( 'NONE',  ( 20.74093720376649941, 6.709541214524366026, -48.67227202248968609 ) ) ;
#1325 = AXIS2_PLACEMENT_3D ( 'NONE', #67107, #4108, #14995 ) ;
#1327 = ORIENTED_EDGE ( 'NONE', *, *, #10704, .T. ) ;
#1326 = PLANE ( 'NONE',  #5078 ) ;
#1328 = CARTESIAN_POINT ( 'NONE',  ( -42.36049017605959932, 61.90437280228238137, 170.0000000000000000 ) ) ;
#1329 = EDGE_LOOP ( 'NONE', ( #45469, #25042, #63712, #61696 ) ) ;
#1330 = AXIS2_PLACEMENT_3D ( 'NONE', #4044, #15288, #14591 ) ;
#1331 = PRESENTATION_LAYER_ASSIGNMENT (  '', '', ( #52978 ) ) ;
#1332 = VERTEX_POINT ( 'NONE', #12794 ) ;
#1334 = EDGE_CURVE ( 'NONE', #10029, #21805, #48601, .T. ) ;
#1333 = CARTESIAN_POINT ( 'NONE',  ( 179.4227152810058215, 78.36166152262364903, 29.48269904055934276 ) ) ;
#1336 = DIRECTION ( 'NONE',  ( 1.000000000000000000, 0.000000000000000000, 0.000000000000000000 ) ) ;
#1335 = VECTOR ( 'NONE', #46755, 1000.000000000000000 ) ;
#1338 = EDGE_LOOP ( 'NONE', ( #14531, #35591, #15625, #48133 ) ) ;
#1337 = CARTESIAN_POINT ( 'NONE',  ( -8.314488422519703548, 7.931352979988683494, -77.26262132240753999 ) ) ;
#1339 = CARTESIAN_POINT ( 'NONE',  ( 158.3595886390532428, 58.34525996025801220, 29.44919521104816340 ) ) ;
#1340 = CLOSED_SHELL ( 'NONE', ( #64564, #36434, #25846, #2769, #31042, #6717, #35413, #19813, #9481, #33980, #26616, #20112, #10478, #20014, #64798, #13207, #41216, #44725, #21120, #61014, #59716, #10226, #39239, #31844, #27146, #58887, #58375, #11492, #48120, #25762, #35077, #24104 ) ) ;
#1341 = DIRECTION ( 'NONE',  ( -1.000000000000000000, 0.000000000000000000, 0.000000000000000000 ) ) ;
#1342 = CARTESIAN_POINT ( 'NONE',  ( 112.3013380801408658, 400.0000000000066507, -123.9497041420121235 ) ) ;
#1343 = EDGE_LOOP ( 'NONE', ( #19373, #43322, #68066, #46993 ) ) ;
#1344 = DIRECTION ( 'NONE',  ( -0.000000000000000000, -0.000000000000000000, -1.000000000000000000 ) ) ;
#1345 = ADVANCED_FACE ( 'NONE', ( #65205 ), #27915, .T. ) ;
#1346 = DIRECTION ( 'NONE',  ( 1.000000000000000000, -0.000000000000000000, 0.000000000000000000 ) ) ;
#1347 = CARTESIAN_POINT ( 'NONE',  ( 110.7167338301704120, 30.21148223254619225, 44.61121420573734753 ) ) ;
#1348 = CYLINDRICAL_SURFACE ( 'NONE', #27998, 7.500000000000013323 ) ;
#1349 = EDGE_CURVE ( 'NONE', #50750, #8416, #55694, .T. ) ;
#1350 = CARTESIAN_POINT ( 'NONE',  ( 22.51798020284706325, 7.817376421459703018, 61.03934684355338192 ) ) ;
#1351 = ORIENTED_EDGE ( 'NONE', *, *, #50161, .T. ) ;
#1352 = EDGE_CURVE ( 'NONE', #21613, #62663, #64860, .T. ) ;
#1353 = ORIENTED_EDGE ( 'NONE', *, *, #66788, .F. ) ;
#1354 = ORIENTED_EDGE ( 'NONE', *, *, #2252, .T. ) ;
#1355 = CARTESIAN_POINT ( 'NONE',  ( 209.2403607860319426, 112.7852583139808189, -91.53499439785448999 ) ) ;
#1356 = CARTESIAN_POINT ( 'NONE',  ( -48.85180024597538306, 13.10609030261107932, 87.27526625388559012 ) ) ;
#1357 = DIRECTION ( 'NONE',  ( 0.000000000000000000, 0.000000000000000000, -1.000000000000000000 ) ) ;
#1358 = CARTESIAN_POINT ( 'NONE',  ( 49.99999999999998579, -19.99999999999996447, 2.000000000000015543 ) ) ;
#1359 = CARTESIAN_POINT ( 'NONE',  ( -103.4984104302275938, 33.40397788071886254, 84.30186542324130983 ) ) ;
#1360 = CARTESIAN_POINT ( 'NONE',  ( 64.38365952014046911, -38.46744580544211800, 0.000000000000000000 ) ) ;
#1361 = DIRECTION ( 'NONE',  ( 0.000000000000000000, 0.000000000000000000, 1.000000000000000000 ) ) ;
#1362 = CARTESIAN_POINT ( 'NONE',  ( -74.79539698934964065, 21.95498232236883496, -22.19923502380404301 ) ) ;
#1363 = CARTESIAN_POINT ( 'NONE',  ( 80.73012746365746750, 17.49169339352361519, 68.71435551237969719 ) ) ;
#1364 = ORIENTED_EDGE ( 'NONE', *, *, #65796, .F. ) ;
#1365 = CARTESIAN_POINT ( 'NONE',  ( 32.28603806442400526, 7.590310383548731110, 34.99384699948907240 ) ) ;
#1366 = CARTESIAN_POINT ( 'NONE',  ( 187.5325688887157867, 85.37769363979907666, 40.67676355286661050 ) ) ;
#1367 = B_SPLINE_CURVE_WITH_KNOTS ( 'NONE', 3,
 ( #22102, #64670, #38274, #43542, #60435, #59720 ),
 .UNSPECIFIED., .F., .F.,
 ( 4, 2, 4 ),
 ( 0.03218934490037923812, 0.06469832469447826806, 0.09720730448857729800 ),
 .UNSPECIFIED. ) ;
#1368 = DIRECTION ( 'NONE',  ( 0.000000000000000000, 0.000000000000000000, -1.000000000000000000 ) ) ;
#1369 = LINE ( 'NONE', #21772, #32585 ) ;
#1370 = CARTESIAN_POINT ( 'NONE',  ( -119.6801029354224966, 43.71909921132878907, 60.75692515445694397 ) ) ;
#1371 = CARTESIAN_POINT ( 'NONE',  ( -48.56549579811110817, 13.03742088415616429, 14.76862391130607932 ) ) ;
#1372 = CIRCLE ( 'NONE', #41799, 65.36598343705435354 ) ;
#1373 = CARTESIAN_POINT ( 'NONE',  ( 0.08285530295198803574, 1.570896314769985702, -8.000000000000000000 ) ) ;
#1374 = CARTESIAN_POINT ( 'NONE',  ( 163.5944155533005642, 63.88379440759431560, -74.80571809177408227 ) ) ;
#1375 = ORIENTED_EDGE ( 'NONE', *, *, #58489, .F. ) ;
#1376 = CARTESIAN_POINT ( 'NONE',  ( 24.36509522348982060, 70.94296747916789059, 170.0000000000000000 ) ) ;
#1377 = FACE_OUTER_BOUND ( 'NONE', #3277, .T. ) ;
#1378 = ORIENTED_EDGE ( 'NONE', *, *, #27790, .F. ) ;
#1379 = DIRECTION ( 'NONE',  ( -0.000000000000000000, -0.000000000000000000, -1.000000000000000000 ) ) ;
#1380 = EDGE_CURVE ( 'NONE', #42777, #60210, #17354, .T. ) ;
#1381 = EDGE_LOOP ( 'NONE', ( #20943, #1491, #51722, #43619 ) ) ;
#1382 = CARTESIAN_POINT ( 'NONE',  ( -83.51052366780673708, 24.22613130369188994, 43.64917403576246357 ) ) ;
#1383 = CARTESIAN_POINT ( 'NONE',  ( 154.6530827109543509, 56.75509330623211923, -63.51432978475487801 ) ) ;
#1384 = CARTESIAN_POINT ( 'NONE',  ( 60.62939143133407072, 12.13148391928978143, -50.34764057611634058 ) ) ;
#1385 = B_SPLINE_CURVE_WITH_KNOTS ( 'NONE', 3,
 ( #22950, #28571, #54595, #2196, #50023, #28212, #65519, #12396, #49659, #18715, #23994, #60232, #1488, #23308, #40167, #1857, #61275, #18020, #44756, #61624, #29268, #39820, #6419, #49311, #27873, #17674, #44394, #17314, #39471, #45087, #38785, #12045, #34565, #7816, #65881, #39139, #13099, #66573, #56007, #60923, #12746, #34207, #62311, #9194 ),
 .UNSPECIFIED., .F., .F.,
 ( 4, 2, 2, 2, 2, 2, 2, 2, 2, 2, 2, 2, 2, 2, 2, 2, 2, 2, 2, 2, 2, 4 ),
 ( 1.387778780781445676E-17, 0.004120577325733650390, 0.006180865988600449563, 0.008241154651467248737, 0.01030144331433404878, 0.01133158764576740543, 0.01236173197720076035, 0.01339187630863411874, 0.01442202064006747365, 0.01545216497150083031, 0.01648230930293418522, 0.01699738146865086355, 0.01751245363436754535, 0.01854259796580088465, 0.01957274229723423090, 0.02060288662866757020, 0.02266317529153428004, 0.02472346395440098640, 0.02678375261726769971, 0.02781389694870106330, 0.02884404128013443036, 0.03296461860586798881 ),
 .UNSPECIFIED. ) ;
#1386 = AXIS2_PLACEMENT_3D ( 'NONE', #23783, #34697, #56132 ) ;
#1387 = CARTESIAN_POINT ( 'NONE',  ( -26.50364027666004674, 8.832969329054167318, 58.89264053224560769 ) ) ;
#1388 = ORIENTED_EDGE ( 'NONE', *, *, #34429, .T. ) ;
#1389 = EDGE_LOOP ( 'NONE', ( #46759, #58270, #47068, #8834 ) ) ;
#1390 = CARTESIAN_POINT ( 'NONE',  ( -55.05276343752908730, 15.72344139423347720, -8.371773407996169425 ) ) ;
#1391 = ORIENTED_EDGE ( 'NONE', *, *, #21130, .F. ) ;
#1392 = CARTESIAN_POINT ( 'NONE',  ( 34.45158752686798209, 8.829194381142000836, -10.61983960213909306 ) ) ;
#1393 = CARTESIAN_POINT ( 'NONE',  ( 181.0840389613909736, 78.60582251573003987, 2.464043515047718458 ) ) ;
#1394 =( NAMED_UNIT ( * ) SI_UNIT ( $, .STERADIAN. ) SOLID_ANGLE_UNIT ( ) );
#1395 = CARTESIAN_POINT ( 'NONE',  ( -0.3255842968951683236, 7.525381170773409956, 64.95241148711420465 ) ) ;
#1396 = B_SPLINE_CURVE_WITH_KNOTS ( 'NONE', 3,
 ( #47744, #20002, #42479, #31253, #4844, #63599, #41797, #42135, #57973, #47397, #36175, #25284, #4167, #68855, #69208, #36867, #15409, #9789, #14713, #20680, #9443, #63937, #25968, #62908, #57634, #58307, #10124, #30900, #52681, #35834, #52349, #25634, #36517, #53018, #30549, #21032, #4506, #47067, #68528, #31581, #46369, #9101, #26314, #30214, #63255, #67848, #14381, #20332, #15063, #62568 ),
 .UNSPECIFIED., .F., .F.,
 ( 4, 2, 2, 2, 2, 2, 2, 2, 2, 2, 2, 2, 2, 2, 2, 2, 2, 2, 2, 2, 2, 2, 2, 2, 4 ),
 ( 0.02688458561150008225, 0.02770990876165288150, 0.02853523191180568075, 0.03018587821211126537, 0.03183652451241685000, 0.03266184766256963190, 0.03348717081272241380, 0.03513781711302799149, 0.03678846341333356917, 0.03761378656348635108, 0.03843910971363913298, 0.03926443286379191488, 0.04008975601394469679, 0.04174040231425028141, 0.04256572546440307719, 0.04339104861455587991, 0.04421637176470867570, 0.04504169491486147148, 0.04586701806501427420, 0.04669234121516707692, 0.04834298751547272399, 0.04916831066562551977, 0.04999363381577832249, 0.05164428011608399038, 0.05329492641638964440 ),
 .UNSPECIFIED. ) ;
#1397 = CARTESIAN_POINT ( 'NONE',  ( 198.3712756463373239, 99.67211044168692524, -93.48022478442567262 ) ) ;
#1398 = PLANE ( 'NONE',  #59758 ) ;
#1399 = ORIENTED_EDGE ( 'NONE', *, *, #17201, .T. ) ;
#1400 = CARTESIAN_POINT ( 'NONE',  ( 8.000000000000000000, 3.115336682267017210, -0.3193931313915070458 ) ) ;
#1401 = ORIENTED_EDGE ( 'NONE', *, *, #67407, .F. ) ;
#1402 = EDGE_LOOP ( 'NONE', ( #21473, #51203 ) ) ;
#1403 = FACE_OUTER_BOUND ( 'NONE', #22851, .T. ) ;
#1404 = DIRECTION ( 'NONE',  ( -0.000000000000000000, -0.000000000000000000, 1.000000000000000000 ) ) ;
#1405 = CARTESIAN_POINT ( 'NONE',  ( 442.3372781065085633, 399.9999999999998863, 103.5502958579881891 ) ) ;
#1406 = CARTESIAN_POINT ( 'NONE',  ( 133.8566784816069060, 42.60093787723655367, 17.66579024853170310 ) ) ;
#1407 = LINE ( 'NONE', #55564, #7161 ) ;
#1408 = VERTEX_POINT ( 'NONE', #33562 ) ;
#1409 = ADVANCED_FACE ( 'NONE', ( #62002 ), #51117, .T. ) ;
#1410 = CARTESIAN_POINT ( 'NONE',  ( 80.16939877002758408, 17.31693935407229645, 14.20996114281630618 ) ) ;
#1411 = EDGE_CURVE ( 'NONE', #51862, #23473, #29508, .T. ) ;
#1412 = ORIENTED_EDGE ( 'NONE', *, *, #13505, .F. ) ;
#1413 = CARTESIAN_POINT ( 'NONE',  ( 209.9518228411288874, 0.000000000000000000, 31.43423095485942298 ) ) ;
#1414 = ORIENTED_EDGE ( 'NONE', *, *, #50736, .T. ) ;
#1415 = EDGE_CURVE ( 'NONE', #10004, #63684, #40901, .T. ) ;
#1416 = CARTESIAN_POINT ( 'NONE',  ( 0.000000000000000000, 35.26862320190615208, -9.999999999999998224 ) ) ;
#1417 = AXIS2_PLACEMENT_3D ( 'NONE', #30152, #18895, #57567 ) ;
#1418 = EDGE_LOOP ( 'NONE', ( #66100, #12328, #6607, #20703 ) ) ;
#1419 = CARTESIAN_POINT ( 'NONE',  ( -144.7571537022063524, 60.25265659240449168, -74.96618912951997515 ) ) ;
#1420 = CARTESIAN_POINT ( 'NONE',  ( 10.55634918610400419, -15.55634918610406103, 85.00100000000000477 ) ) ;
#1421 = DIRECTION ( 'NONE',  ( -0.000000000000000000, 1.000000000000000000, -0.000000000000000000 ) ) ;
#1422 = VECTOR ( 'NONE', #58262, 1000.000000000000000 ) ;
#1423 = VERTEX_POINT ( 'NONE', #51467 ) ;
#1424 = PLANE ( 'NONE',  #7615 ) ;
#1425 = AXIS2_PLACEMENT_3D ( 'NONE', #25627, #58986, #15401 ) ;
#1426 = CARTESIAN_POINT ( 'NONE',  ( 66.21212819542179773, 14.47309682125277774, 84.20943056763468348 ) ) ;
#1427 = CARTESIAN_POINT ( 'NONE',  ( 35.65622260226241735, 8.964590916200318560, 43.91611479937130724 ) ) ;
#1428 = CARTESIAN_POINT ( 'NONE',  ( -175.9944734395087096, 91.92390745845766276, -35.27130985876561198 ) ) ;
#1429 = DIRECTION ( 'NONE',  ( -0.000000000000000000, 1.000000000000000000, -0.000000000000000000 ) ) ;
#1430 = AXIS2_PLACEMENT_3D ( 'NONE', #24335, #67253, #13759 ) ;
#1431 = DIRECTION ( 'NONE',  ( 0.000000000000000000, 1.000000000000000000, 0.000000000000000000 ) ) ;
#1432 = EDGE_CURVE ( 'NONE', #52541, #47772, #5936, .T. ) ;
#1433 = CARTESIAN_POINT ( 'NONE',  ( 128.0848616812662613, 38.04676222636083338, -65.55253114271090453 ) ) ;
#1434 = ORIENTED_EDGE ( 'NONE', *, *, #24309, .T. ) ;
#1435 = CARTESIAN_POINT ( 'NONE',  ( 134.7708899521910553, 43.15864772107688907, -77.81547585753226315 ) ) ;
#1437 = EDGE_CURVE ( 'NONE', #20980, #32549, #4275, .T. ) ;
#1436 = CARTESIAN_POINT ( 'NONE',  ( -142.8492950481058870, 60.01492924994601452, -72.62007504265284297 ) ) ;
#1438 = ORIENTED_EDGE ( 'NONE', *, *, #9221, .F. ) ;
#1439 = AXIS2_PLACEMENT_3D ( 'NONE', #31545, #574, #22025 ) ;
#1440 = CARTESIAN_POINT ( 'NONE',  ( 8.000000000000007105, 249.8719672152120381, 94.99999999999866418 ) ) ;
#1441 = CARTESIAN_POINT ( 'NONE',  ( -0.7174461528505768904, 6.532311451815526304, -67.35691283117644446 ) ) ;
#1442 = CARTESIAN_POINT ( 'NONE',  ( -176.3856149167964986, 92.38076834121979175, 71.93273640432624916 ) ) ;
#1443 = CARTESIAN_POINT ( 'NONE',  ( 32.23328773803155656, 26.50150638838968931, 13.79046340968178441 ) ) ;
#1444 = DIRECTION ( 'NONE',  ( -1.000000000000000000, 0.000000000000000000, 0.000000000000000000 ) ) ;
#1445 = CARTESIAN_POINT ( 'NONE',  ( -5.183193881612057297, 7.740932022135017299, 44.63904903171023619 ) ) ;
#1446 = DIRECTION ( 'NONE',  ( 1.000000000000000000, 0.000000000000000000, 0.000000000000000000 ) ) ;
#1447 = CYLINDRICAL_SURFACE ( 'NONE', #33698, 65.36598343705435354 ) ;
#1448 = CARTESIAN_POINT ( 'NONE',  ( -5.417282889646089394, 7.753782747238989081, -8.966378063162283141 ) ) ;
#1449 = CARTESIAN_POINT ( 'NONE',  ( -11.79249160485393766, 8.191429102467035150, 43.98525602679245594 ) ) ;
#1450 = CARTESIAN_POINT ( 'NONE',  ( 114.6632852039171127, 30.98120524556723510, 4.202855321170513747 ) ) ;
#1451 = CARTESIAN_POINT ( 'NONE',  ( -20.55634918610405748, -15.55634918610400774, 0.000000000000000000 ) ) ;
#1452 = ORIENTED_EDGE ( 'NONE', *, *, #49262, .F. ) ;
#1453 = DIRECTION ( 'NONE',  ( -1.000000000000000000, -0.000000000000000000, -0.000000000000000000 ) ) ;
#1454 = VERTEX_POINT ( 'NONE', #29656 ) ;
#1455 = CARTESIAN_POINT ( 'NONE',  ( 0.000000000000000000, 0.000000000000000000, 170.0000000000000000 ) ) ;
#1456 = CARTESIAN_POINT ( 'NONE',  ( 79.39764314491563368, 18.13166883367086157, -72.17018488364679740 ) ) ;
#1457 = CARTESIAN_POINT ( 'NONE',  ( 103.0076904570972687, 26.76944391674850365, 92.80592866474482605 ) ) ;
#1458 = DIRECTION ( 'NONE',  ( -1.000000000000000000, -0.000000000000000000, -0.000000000000000000 ) ) ;
#1459 = DIRECTION ( 'NONE',  ( 0.000000000000000000, -1.000000000000000000, 0.000000000000000000 ) ) ;
#1460 = CARTESIAN_POINT ( 'NONE',  ( -23.93933407965395688, 9.495050561681672718, -42.32159819572655124 ) ) ;
#1461 = FACE_OUTER_BOUND ( 'NONE', #63718, .T. ) ;
#1462 = CARTESIAN_POINT ( 'NONE',  ( 89.99999999999998579, 0.000000000000000000, 7.000000000000000000 ) ) ;
#1463 = DIRECTION ( 'NONE',  ( 0.000000000000000000, -1.000000000000000000, 0.000000000000000000 ) ) ;
#1464 = ORIENTED_EDGE ( 'NONE', *, *, #14554, .T. ) ;
#1465 = ORIENTED_EDGE ( 'NONE', *, *, #37162, .F. ) ;
#1466 = CARTESIAN_POINT ( 'NONE',  ( 32.30062460741315533, 8.603096374765343057, 61.83302680985992339 ) ) ;
#1467 = CARTESIAN_POINT ( 'NONE',  ( 41.66904755831212981, 15.55634918610394379, 0.000000000000000000 ) ) ;
#1468 = CARTESIAN_POINT ( 'NONE',  ( 39.81840452174282774, 8.463718892264783022, -89.30891864635512434 ) ) ;
#1469 = SURFACE_SIDE_STYLE ('',( #55275 ) ) ;
#1470 = CARTESIAN_POINT ( 'NONE',  ( -167.1619226259398943, 82.18315278115414912, -19.92833628696023496 ) ) ;
#1471 = DIRECTION ( 'NONE',  ( -0.000000000000000000, 1.000000000000000000, -0.000000000000000000 ) ) ;
#1472 = ORIENTED_EDGE ( 'NONE', *, *, #33458, .F. ) ;
#1473 = CARTESIAN_POINT ( 'NONE',  ( 103.1534365798308386, 26.83148826706846535, -40.92239761178424118 ) ) ;
#1474 = CARTESIAN_POINT ( 'NONE',  ( 23.28809538736928175, 7.864824219997535337, -42.52675217981989420 ) ) ;
#1475 = CARTESIAN_POINT ( 'NONE',  ( -85.10774223992955001, 24.88053943842882276, -19.62096145546114911 ) ) ;
#1476 = CARTESIAN_POINT ( 'NONE',  ( -84.63218004431101349, 25.77252883085057533, -91.73812189727786404 ) ) ;
#1477 = LINE ( 'NONE', #29259, #53207 ) ;
#1478 = CARTESIAN_POINT ( 'NONE',  ( 210.5178985598939789, 114.6803933586780602, -12.24472973805804976 ) ) ;
#1479 = FACE_BOUND ( 'NONE', #66534, .T. ) ;
#1480 = CARTESIAN_POINT ( 'NONE',  ( -56.02358673658414290, 14.94347049174937503, -50.16887940659524503 ) ) ;
#1481 = AXIS2_PLACEMENT_3D ( 'NONE', #48092, #69551, #32624 ) ;
#1482 = ORIENTED_EDGE ( 'NONE', *, *, #22147, .F. ) ;
#1483 = CARTESIAN_POINT ( 'NONE',  ( 0.000000000000000000, 0.000000000000000000, 0.000000000000000000 ) ) ;
#1484 = DIRECTION ( 'NONE',  ( 0.000000000000000000, -1.000000000000000000, 0.000000000000000000 ) ) ;
#1485 = AXIS2_PLACEMENT_3D ( 'NONE', #851, #39193, #44812 ) ;
#1486 = LINE ( 'NONE', #22948, #64439 ) ;
#1487 = DIRECTION ( 'NONE',  ( -0.000000000000000000, 1.000000000000000000, -0.000000000000000000 ) ) ;
#1488 = CARTESIAN_POINT ( 'NONE',  ( 211.1046732743772338, 117.3965485104337176, 67.46095300389731619 ) ) ;
#1489 = CARTESIAN_POINT ( 'NONE',  ( -8.000000000000000000, 4.618802153516996079, -0.7145311798163263006 ) ) ;
#1490 = EDGE_CURVE ( 'NONE', #21376, #25377, #62094, .T. ) ;
#1491 = ORIENTED_EDGE ( 'NONE', *, *, #22147, .T. ) ;
#1492 = DIRECTION ( 'NONE',  ( -1.000000000000000000, 0.000000000000000000, 0.000000000000000000 ) ) ;
#1493 = CARTESIAN_POINT ( 'NONE',  ( 410.0000000000000000, 0.000000000000000000, 380.0000000000000000 ) ) ;
#1494 = ADVANCED_FACE ( 'NONE', ( #31724 ), #63402, .T. ) ;
#1495 = ORIENTED_EDGE ( 'NONE', *, *, #45979, .F. ) ;
#1496 = ORIENTED_EDGE ( 'NONE', *, *, #11332, .F. ) ;
#1497 = LINE ( 'NONE', #6064, #10599 ) ;
#1498 = CARTESIAN_POINT ( 'NONE',  ( -61.76386578474846800, 17.63453064612499688, -19.25649393556963318 ) ) ;
#1499 = EDGE_CURVE ( 'NONE', #64497, #58120, #57102, .T. ) ;
#1500 = CARTESIAN_POINT ( 'NONE',  ( 103.0103829243729052, 25.67737053862328267, 39.16093723846415742 ) ) ;
#1501 = ORIENTED_EDGE ( 'NONE', *, *, #10704, .F. ) ;
#1502 = EDGE_CURVE ( 'NONE', #68705, #58537, #3752, .T. ) ;
#1503 = EDGE_LOOP ( 'NONE', ( #64737, #47138, #56812, #9323 ) ) ;
#1504 = DIRECTION ( 'NONE',  ( -1.000000000000000000, 0.000000000000000000, 0.000000000000000000 ) ) ;
#1505 = CARTESIAN_POINT ( 'NONE',  ( 163.1370549780984334, 63.50181104276889243, 31.97058753488886396 ) ) ;
#1506 = CARTESIAN_POINT ( 'NONE',  ( 69.36122620657974380, 14.23458312296499528, 94.99999999999866418 ) ) ;
#1507 = FACE_OUTER_BOUND ( 'NONE', #30878, .T. ) ;
#1508 = CARTESIAN_POINT ( 'NONE',  ( -173.1211646369891639, 87.12891641440852197, -88.40105834567665966 ) ) ;
#1509 = CARTESIAN_POINT ( 'NONE',  ( 107.0447263249841541, 28.53200276018955961, -9.789778272522351443 ) ) ;
#1510 = CARTESIAN_POINT ( 'NONE',  ( -48.58011387679029269, 14.07568064779664319, 7.175827997749510523 ) ) ;
#1511 = CIRCLE ( 'NONE', #41934, 25.12245591505646303 ) ;
#1512 = DIRECTION ( 'NONE',  ( -1.000000000000000000, 0.000000000000000000, 0.000000000000000000 ) ) ;
#1514 = EDGE_CURVE ( 'NONE', #4893, #19257, #13498, .T. ) ;
#1513 = CARTESIAN_POINT ( 'NONE',  ( -156.9402586331177361, 72.11962769956262775, -95.00000000000133582 ) ) ;
#1515 = DIRECTION ( 'NONE',  ( 0.000000000000000000, 1.000000000000000000, -0.000000000000000000 ) ) ;
#1516 = CARTESIAN_POINT ( 'NONE',  ( 81.80451556658140078, 17.83033755654336261, 85.12011702748436903 ) ) ;
#1518 = ORIENTED_EDGE ( 'NONE', *, *, #63162, .T. ) ;
#1517 = DIRECTION ( 'NONE',  ( 0.000000000000000000, -0.000000000000000000, -1.000000000000000000 ) ) ;
#1519 = ORIENTED_EDGE ( 'NONE', *, *, #52020, .T. ) ;
#1520 = ORIENTED_EDGE ( 'NONE', *, *, #37790, .F. ) ;
#1521 = VECTOR ( 'NONE', #55884, 1000.000000000000000 ) ;
#1522 = CARTESIAN_POINT ( 'NONE',  ( -13.78709718204646961, 7.352743657744182926, -20.65034025157325459 ) ) ;
#1523 = CARTESIAN_POINT ( 'NONE',  ( -165.6128944859384831, 80.58007050464003385, 92.14767930188499179 ) ) ;
#1524 = CARTESIAN_POINT ( 'NONE',  ( -54.08504625707234936, 14.42374043447188114, -8.418564600962227473 ) ) ;
#1525 = CARTESIAN_POINT ( 'NONE',  ( 102.7571040248400891, 25.57023079238897267, -16.05041636952068274 ) ) ;
#1526 = CARTESIAN_POINT ( 'NONE',  ( -56.73868929054669508, 16.18382781951277849, -35.40422542096111869 ) ) ;
#1527 = VECTOR ( 'NONE', #25037, 1000.000000000000000 ) ;
#1528 = FACE_OUTER_BOUND ( 'NONE', #26038, .T. ) ;
#1529 = LINE ( 'NONE', #55690, #24184 ) ;
#1530 = CARTESIAN_POINT ( 'NONE',  ( 21.88606409348644277, 6.772455198693825729, -20.54785372844966318 ) ) ;
#1531 = EDGE_LOOP ( 'NONE', ( #47811, #17635, #2209 ) ) ;
#1532 = AXIS2_PLACEMENT_3D ( 'NONE', #12569, #6939, #17848 ) ;
#1533 = LINE ( 'NONE', #38469, #44099 ) ;
#1534 = ORIENTED_EDGE ( 'NONE', *, *, #38769, .T. ) ;
#1535 = VERTEX_POINT ( 'NONE', #23523 ) ;
#1536 = CARTESIAN_POINT ( 'NONE',  ( 3.000000000000006217, 0.000000000000000000, 0.000000000000000000 ) ) ;
#1537 = CARTESIAN_POINT ( 'NONE',  ( -55.48176214950256480, 15.83928188623576894, -88.91464852580686795 ) ) ;
#1538 = VECTOR ( 'NONE', #21960, 1000.000000000000000 ) ;
#1539 = CARTESIAN_POINT ( 'NONE',  ( -29.85611858039614219, 10.35537958803110925, 84.06752208004112958 ) ) ;
#1540 = CARTESIAN_POINT ( 'NONE',  ( -1.734723475976807094E-15, 9.237604307034022355, -8.785468820183664818 ) ) ;
#1541 = CARTESIAN_POINT ( 'NONE',  ( -422.6627218934913230, 399.9999999999997726, 108.5502958579881891 ) ) ;
#1542 = CARTESIAN_POINT ( 'NONE',  ( 20.89850557012451659, -13.94239061780404043, 0.000000000000000000 ) ) ;
#1543 = CARTESIAN_POINT ( 'NONE',  ( 0.000000000000000000, -26.09918303830819397, 0.000000000000000000 ) ) ;
#1544 = ORIENTED_EDGE ( 'NONE', *, *, #54272, .T. ) ;
#1545 = ORIENTED_EDGE ( 'NONE', *, *, #39490, .T. ) ;
#1546 = EDGE_LOOP ( 'NONE', ( #41839, #52195, #39224, #64714 ) ) ;
#1547 = LINE ( 'NONE', #6482, #48398 ) ;
#1548 = CARTESIAN_POINT ( 'NONE',  ( -11.14445507968272153, 7.129894202659276203, 4.040923808319601740 ) ) ;
#1549 = CARTESIAN_POINT ( 'NONE',  ( 35.44781468922820267, 7.928097401423682911, -76.34201268051539557 ) ) ;
#1550 = CARTESIAN_POINT ( 'NONE',  ( 61.33627421985471528, 12.28939706835343770, -9.062593789058455584 ) ) ;
#1551 = B_SPLINE_CURVE_WITH_KNOTS ( 'NONE', 3,
 ( #13741, #33813, #35196, #7076, #67235, #55256, #17634, #1814, #55609, #19019, #3200, #2501, #17987, #60542, #45050, #2160, #66535, #34172, #7780, #8120, #34526, #55968, #12356, #28535, #7439, #28891, #50677, #40470, #45755, #39431, #23612, #34864, #40133, #49983, #23270, #44717 ),
 .UNSPECIFIED., .F., .F.,
 ( 4, 2, 2, 2, 2, 2, 2, 2, 2, 2, 2, 2, 2, 2, 2, 2, 2, 4 ),
 ( 1.551583845779545699E-17, 0.001548367318450172845, 0.003096734636900330077, 0.004645101955350487526, 0.006193469273800644541, 0.007741836592250802423, 0.008516020251475891339, 0.009290203910700981990, 0.01083857122915114247, 0.01238693854760130643, 0.01393530586605147038, 0.01548367318450163087, 0.01703204050295179309, 0.01858040782140195704, 0.02012877513985211406, 0.02167714245830226760, 0.02322550977675242809, 0.02477387709520258510 ),
 .UNSPECIFIED. ) ;
#1552 = UNCERTAINTY_MEASURE_WITH_UNIT (LENGTH_MEASURE( 1.000000000000000082E-05 ), #45317, 'distance_accuracy_value', 'NONE');
#1553 = CARTESIAN_POINT ( 'NONE',  ( -47.55235941796723154, 12.79790236059689512, 38.05499662510656123 ) ) ;
#1554 = DIRECTION ( 'NONE',  ( 0.000000000000000000, -1.000000000000000000, 0.000000000000000000 ) ) ;
#1555 = VERTEX_POINT ( 'NONE', #50942 ) ;
#1556 = CARTESIAN_POINT ( 'NONE',  ( -56.73868929054668087, 16.18382781951278204, -62.24877601142479477 ) ) ;
#1557 = CARTESIAN_POINT ( 'NONE',  ( 199.3764173596862292, 100.9540560740992134, -75.98014011034484838 ) ) ;
#1558 = EDGE_CURVE ( 'NONE', #28403, #51848, #17535, .T. ) ;
#1559 = CARTESIAN_POINT ( 'NONE',  ( -4.502148936856956496, 7.704491846230412833, -36.17659697066419255 ) ) ;
#1560 = CARTESIAN_POINT ( 'NONE',  ( 108.3906473026530080, 28.03385344351497466, 17.54929269514099133 ) ) ;
#1561 = CARTESIAN_POINT ( 'NONE',  ( -167.1534554062404538, 80.72263015867910951, 16.02705747859470264 ) ) ;
#1562 = DIRECTION ( 'NONE',  ( -1.393823445737823288E-16, 0.7660444431189770143, 0.6427876096865403621 ) ) ;
#1563 = FACE_BOUND ( 'NONE', #48077, .T. ) ;
#1564 = DIRECTION ( 'NONE',  ( 0.000000000000000000, 0.000000000000000000, 1.000000000000000000 ) ) ;
#1565 = MECHANICAL_DESIGN_GEOMETRIC_PRESENTATION_REPRESENTATION (  '', ( #34171 ), #59945 ) ;
#1566 = EDGE_LOOP ( 'NONE', ( #36926, #54120, #31121, #55593 ) ) ;
#1567 = CARTESIAN_POINT ( 'NONE',  ( -51.84164840787185113, 39.21024726209461875, 40.00000000000003553 ) ) ;
#1568 = PLANE ( 'NONE',  #65557 ) ;
#1569 = CARTESIAN_POINT ( 'NONE',  ( 26.99999999999999645, 0.000000000000000000, 15.00000000000000000 ) ) ;
#1570 = CARTESIAN_POINT ( 'NONE',  ( 46.85206196242845778, 9.495795933269487676, -70.95794390456796918 ) ) ;
#1571 = CARTESIAN_POINT ( 'NONE',  ( 0.000000000000000000, 0.000000000000000000, 41.38025477438755928 ) ) ;
#1572 = VERTEX_POINT ( 'NONE', #44260 ) ;
#1573 = AXIS2_PLACEMENT_3D ( 'NONE', #37705, #53531, #59155 ) ;
#1574 = ORIENTED_EDGE ( 'NONE', *, *, #43551, .F. ) ;
#1575 = CYLINDRICAL_SURFACE ( 'NONE', #59147, 7.500000000000013323 ) ;
#1576 = VECTOR ( 'NONE', #39227, 1000.000000000000000 ) ;
#1577 = CARTESIAN_POINT ( 'NONE',  ( 188.4662191759685470, 86.40293565635343498, 89.15863815613664656 ) ) ;
#1578 = EDGE_CURVE ( 'NONE', #62965, #28360, #26074, .T. ) ;
#1579 = EDGE_LOOP ( 'NONE', ( #58682, #202, #19140, #26203 ) ) ;
#1580 = VERTEX_POINT ( 'NONE', #18236 ) ;
#1581 = VECTOR ( 'NONE', #15769, 1000.000000000000000 ) ;
#1582 = DIRECTION ( 'NONE',  ( -0.000000000000000000, -1.000000000000000000, -0.000000000000000000 ) ) ;
#1583 = CARTESIAN_POINT ( 'NONE',  ( 151.6178224291901699, 54.48737267587419097, 41.60651290194002883 ) ) ;
#1584 = DIRECTION ( 'NONE',  ( -0.000000000000000000, -0.000000000000000000, -1.000000000000000000 ) ) ;
#1585 = EDGE_LOOP ( 'NONE', ( #52041, #42802, #63554, #14608 ) ) ;
#1586 = CARTESIAN_POINT ( 'NONE',  ( 55.46196446482127840, -34.59309596431295120, 6.377659838150088165E-18 ) ) ;
#1587 = LINE ( 'NONE', #12150, #22150 ) ;
#1588 = CARTESIAN_POINT ( 'NONE',  ( -12.50012419267789454, 70.00000000000000000, -27.27172336262650987 ) ) ;
#1589 = CIRCLE ( 'NONE', #19567, 4.999999999999997335 ) ;
#1590 = ADVANCED_FACE ( 'NONE', ( #39693 ), #61149, .F. ) ;
#1591 = LINE ( 'NONE', #17777, #28115 ) ;
#1592 = LINE ( 'NONE', #44135, #22665 ) ;
#1593 = CARTESIAN_POINT ( 'NONE',  ( -190.4968431727839118, 108.8425311198514720, 34.24491274770363702 ) ) ;
#1594 = VERTEX_POINT ( 'NONE', #29141 ) ;
#1595 = DIRECTION ( 'NONE',  ( 0.000000000000000000, 1.000000000000000000, 0.000000000000000000 ) ) ;
#1596 = CARTESIAN_POINT ( 'NONE',  ( -73.81801970646054656, 21.60231032711191190, 16.80100356717971977 ) ) ;
#1597 = EDGE_CURVE ( 'NONE', #58006, #60940, #60454, .T. ) ;
#1598 = FACE_OUTER_BOUND ( 'NONE', #21651, .T. ) ;
#1599 = DIRECTION ( 'NONE',  ( 0.000000000000000000, 1.000000000000000000, 0.000000000000000000 ) ) ;
#1601 = ORIENTED_EDGE ( 'NONE', *, *, #1028, .F. ) ;
#1600 = CARTESIAN_POINT ( 'NONE',  ( -130.5004577019969076, 49.60245395521563694, 85.88294129194291315 ) ) ;
#1602 = CARTESIAN_POINT ( 'NONE',  ( 82.14449817946437804, 17.93919511903895980, -37.30520553978547582 ) ) ;
#1603 = EDGE_CURVE ( 'NONE', #4848, #2387, #65577, .T. ) ;
#1604 = ADVANCED_FACE ( 'NONE', ( #63911 ), #11468, .F. ) ;
#1605 = ORIENTED_EDGE ( 'NONE', *, *, #40738, .T. ) ;
#1606 = CARTESIAN_POINT ( 'NONE',  ( -147.3641864666714412, 62.38213854487950982, 57.86459567537096405 ) ) ;
#1607 = CARTESIAN_POINT ( 'NONE',  ( 82.95856197793163744, 19.25847567427441120, 30.65358330111253338 ) ) ;
#1608 = CARTESIAN_POINT ( 'NONE',  ( 15.55634918610397399, -26.11269837220809364, 2.000000000000001776 ) ) ;
#1609 = CARTESIAN_POINT ( 'NONE',  ( 91.12448333640237763, 22.07449368110502519, 31.18905971957590495 ) ) ;
#1610 = CARTESIAN_POINT ( 'NONE',  ( 138.5721691894143817, 44.34516164557648921, -22.53138726545303427 ) ) ;
#1611 = DIRECTION ( 'NONE',  ( 0.000000000000000000, 0.000000000000000000, -1.000000000000000000 ) ) ;
#1612 = CARTESIAN_POINT ( 'NONE',  ( 88.30010642107258434, 19.99780058782974379, -62.85061619352340045 ) ) ;
#1613 = VECTOR ( 'NONE', #727, 1000.000000000000000 ) ;
#1614 = CARTESIAN_POINT ( 'NONE',  ( -33.00964028082890422, -25.52799247005623329, 13.79046412380261799 ) ) ;
#1615 = CARTESIAN_POINT ( 'NONE',  ( -54.56685407443679736, 15.59259313022787907, 45.31732777293115078 ) ) ;
#1616 = ORIENTED_EDGE ( 'NONE', *, *, #7716, .T. ) ;
#1617 = VERTEX_POINT ( 'NONE', #5168 ) ;
#1618 =( GEOMETRIC_REPRESENTATION_CONTEXT ( 3 ) GLOBAL_UNCERTAINTY_ASSIGNED_CONTEXT ( ( #3629 ) ) GLOBAL_UNIT_ASSIGNED_CONTEXT ( ( #16852, #59753, #22487 ) ) REPRESENTATION_CONTEXT ( 'NONE', 'WORKASPACE' ) );
#1619 = CARTESIAN_POINT ( 'NONE',  ( 46.42281973867196143, 9.426811321855154802, 40.06307784724872789 ) ) ;
#1620 = CARTESIAN_POINT ( 'NONE',  ( 10.55634918610411432, 51.66904755831205875, 85.00100000000000477 ) ) ;
#1621 = CARTESIAN_POINT ( 'NONE',  ( 0.000000000000000000, 200.0000000000000000, 0.000000000000000000 ) ) ;
#1622 = DIRECTION ( 'NONE',  ( -1.000000000000000000, 0.000000000000000000, 0.000000000000000000 ) ) ;
#1623 = VECTOR ( 'NONE', #26735, 1000.000000000000000 ) ;
#1624 = CARTESIAN_POINT ( 'NONE',  ( 212.0779786303465926, 118.9010947973413437, -45.20355168328251239 ) ) ;
#1625 = CARTESIAN_POINT ( 'NONE',  ( -72.35078170365746075, 21.08176362823952843, -73.51264129435554651 ) ) ;
#1626 = CARTESIAN_POINT ( 'NONE',  ( 16.78635691501517613, 6.000000000000000000, -4.435653166495499455 ) ) ;
#1627 = CARTESIAN_POINT ( 'NONE',  ( -25.50312845906834980, 8.692070753302672870, -47.40798146362784848 ) ) ;
#1628 = CARTESIAN_POINT ( 'NONE',  ( 162.0835148203876770, 61.32844276806159911, -76.40136503387930134 ) ) ;
#1629 = ORIENTED_EDGE ( 'NONE', *, *, #37145, .F. ) ;
#1631 = CARTESIAN_POINT ( 'NONE',  ( -24.95010104166214404, 9.631487977190600347, 14.64071932601358128 ) ) ;
#1630 = VECTOR ( 'NONE', #25226, 1000.000000000000000 ) ;
#1632 = ORIENTED_EDGE ( 'NONE', *, *, #41608, .F. ) ;
#1633 = PLANE ( 'NONE',  #28492 ) ;
#1634 = VECTOR ( 'NONE', #40606, 1000.000000000000114 ) ;
#1635 = LINE ( 'NONE', #12540, #16170 ) ;
#1636 = CARTESIAN_POINT ( 'NONE',  ( -85.09761763353363051, 24.87634954265997322, 68.62969091966090218 ) ) ;
#1637 = CARTESIAN_POINT ( 'NONE',  ( 55.46196446482078812, 34.59309596431376121, 43.58025477438756212 ) ) ;
#1638 = CARTESIAN_POINT ( 'NONE',  ( 108.3842135503130777, -21.48302731199173721, -4.742990268296093603 ) ) ;
#1639 = CARTESIAN_POINT ( 'NONE',  ( 127.7121523762017858, -170.0000000000000000, 94.99999999999866418 ) ) ;
#1640 = DIRECTION ( 'NONE',  ( 1.850371928290090422E-16, -1.000000000000000000, -1.110223024625156171E-16 ) ) ;
#1641 = CARTESIAN_POINT ( 'NONE',  ( -190.6985136298601731, 109.1272424661242582, -95.00000000000133582 ) ) ;
#1642 = CARTESIAN_POINT ( 'NONE',  ( 212.1739865054640006, 117.1950576737078791, 91.03382279583313164 ) ) ;
#1643 = CARTESIAN_POINT ( 'NONE',  ( 133.8566784816069628, 41.42467568809806977, -36.02331093239566684 ) ) ;
#1645 = ORIENTED_EDGE ( 'NONE', *, *, #47561, .T. ) ;
#1644 = ADVANCED_FACE ( 'NONE', ( #6203 ), #36842, .F. ) ;
#1646 = CARTESIAN_POINT ( 'NONE',  ( 55.99998955208977236, 12.18058389017405396, 66.82069825596038015 ) ) ;
#1647 = DIRECTION ( 'NONE',  ( -0.9749279121818227312, -0.2225209339563184729, 2.500042656554810833E-16 ) ) ;
#1648 = FACE_OUTER_BOUND ( 'NONE', #49556, .T. ) ;
#1649 = DIRECTION ( 'NONE',  ( -1.000000000000000000, 0.000000000000000000, 0.000000000000000000 ) ) ;
#1650 = DIRECTION ( 'NONE',  ( 0.000000000000000000, 0.000000000000000000, -1.000000000000000000 ) ) ;
#1651 = DIRECTION ( 'NONE',  ( 1.000000000000000000, 0.000000000000000000, 0.000000000000000000 ) ) ;
#1652 = EDGE_CURVE ( 'NONE', #46890, #13975, #15383, .T. ) ;
#1653 = ORIENTED_EDGE ( 'NONE', *, *, #26539, .T. ) ;
#1654 = CARTESIAN_POINT ( 'NONE',  ( 613.4340796539316898, 724.2365977282739777, 681.7781431858762744 ) ) ;
#1655 = CARTESIAN_POINT ( 'NONE',  ( 0.000000000000000000, 0.000000000000000000, 0.000000000000000000 ) ) ;
#1656 = CARTESIAN_POINT ( 'NONE',  ( 31.11269837220800127, -31.11269837220812562, 2.000000000000001776 ) ) ;
#1657 = DIRECTION ( 'NONE',  ( 0.000000000000000000, -0.000000000000000000, -1.000000000000000000 ) ) ;
#1658 = CONTEXT_DEPENDENT_SHAPE_REPRESENTATION ( #66106, #4178 ) ;
#1659 = CARTESIAN_POINT ( 'NONE',  ( -165.6291901388946997, 79.15850773921177108, 92.52324537314119368 ) ) ;
#1660 = ORIENTED_EDGE ( 'NONE', *, *, #34022, .F. ) ;
#1661 = CARTESIAN_POINT ( 'NONE',  ( -119.6995109608661352, 42.54844499216734022, -46.64985785500188342 ) ) ;
#1662 = DIRECTION ( 'NONE',  ( -0.000000000000000000, -1.000000000000000000, -0.000000000000000000 ) ) ;
#1663 = ADVANCED_FACE ( 'NONE', ( #69520, #10102 ), #63570, .F. ) ;
#1664 = FACE_OUTER_BOUND ( 'NONE', #11943, .T. ) ;
#1665 = CARTESIAN_POINT ( 'NONE',  ( -6.840165690716690783, 7.836465889224639270, -77.21372475586606754 ) ) ;
#1666 = EDGE_CURVE ( 'NONE', #1887, #55194, #16064, .T. ) ;
#1667 = CARTESIAN_POINT ( 'NONE',  ( -21.44923269555038203, 47.00251555413245796, 26.66469066592269144 ) ) ;
#1668 = EDGE_CURVE ( 'NONE', #2382, #69500, #27304, .T. ) ;
#1669 = ORIENTED_EDGE ( 'NONE', *, *, #37017, .F. ) ;
#1670 = CARTESIAN_POINT ( 'NONE',  ( -56.01329802674224112, 15.98369420723829570, 3.518770225379651784 ) ) ;
#1671 = CARTESIAN_POINT ( 'NONE',  ( -21.27554331372999741, 61.43430442924864820, 41.38025477438755928 ) ) ;
#1672 = AXIS2_PLACEMENT_3D ( 'NONE', #56432, #23047, #8255 ) ;
#1673 = CARTESIAN_POINT ( 'NONE',  ( -99.10674985723791508, 32.31836975419496838, 31.20713615476282143 ) ) ;
#1674 = EDGE_CURVE ( 'NONE', #9968, #27957, #11131, .T. ) ;
#1675 = CARTESIAN_POINT ( 'NONE',  ( 19.11168290073779019, 6.629794975642859356, -36.29099477203722302 ) ) ;
#1676 = AXIS2_PLACEMENT_3D ( 'NONE', #6098, #53928, #48643 ) ;
#1677 = AXIS2_PLACEMENT_3D ( 'NONE', #24509, #41705, #67758 ) ;
#1679 = ORIENTED_EDGE ( 'NONE', *, *, #16264, .F. ) ;
#1678 = LINE ( 'NONE', #60760, #6233 ) ;
#1680 = VECTOR ( 'NONE', #34096, 1000.000000000000000 ) ;
#1681 = CARTESIAN_POINT ( 'NONE',  ( 311.9975424824652350, 172.0000000000000284, 354.1673509436691347 ) ) ;
#1682 = AXIS2_PLACEMENT_3D ( 'NONE', #36378, #26165, #16299 ) ;
#1683 = ORIENTED_EDGE ( 'NONE', *, *, #47236, .F. ) ;
#1684 = ORIENTED_EDGE ( 'NONE', *, *, #9687, .F. ) ;
#1685 = CARTESIAN_POINT ( 'NONE',  ( 175.8947993867356843, 74.90689716047907609, 31.37274126135447716 ) ) ;
#1686 = CIRCLE ( 'NONE', #47705, 2.999999999999999112 ) ;
#1687 = ADVANCED_FACE ( 'NONE', ( #31557 ), #48747, .F. ) ;
#1688 = CARTESIAN_POINT ( 'NONE',  ( -38.07133317494998437, 11.79914672408466458, -92.97776376164446788 ) ) ;
#1690 = ORIENTED_EDGE ( 'NONE', *, *, #44656, .F. ) ;
#1689 = DIRECTION ( 'NONE',  ( 0.000000000000000000, 0.000000000000000000, -1.000000000000000000 ) ) ;
#1691 = CARTESIAN_POINT ( 'NONE',  ( -14.79841479960649053, 20.14961338137236524, 0.000000000000000000 ) ) ;
#1692 = CARTESIAN_POINT ( 'NONE',  ( 0.000000000000000000, 0.000000000000000000, 170.0000000000000000 ) ) ;
#1693 = ADVANCED_FACE ( 'NONE', ( #50514 ), #28004, .F. ) ;
#1694 = EDGE_CURVE ( 'NONE', #53100, #28536, #21713, .T. ) ;
#1695 = DIRECTION ( 'NONE',  ( 0.000000000000000000, 0.000000000000000000, 1.000000000000000000 ) ) ;
#1696 = ORIENTED_EDGE ( 'NONE', *, *, #44720, .F. ) ;
#1697 = DIRECTION ( 'NONE',  ( 0.000000000000000000, 0.000000000000000000, -1.000000000000000000 ) ) ;
#1698 = CARTESIAN_POINT ( 'NONE',  ( -33.37566357177428955, 9.916833145467590427, -23.23467432567402824 ) ) ;
#1699 = CARTESIAN_POINT ( 'NONE',  ( 157.4703587214989113, 57.65129005721575339, -89.81328548006499091 ) ) ;
#1700 = CARTESIAN_POINT ( 'NONE',  ( -128.9843070188472609, 49.78011598923032466, 4.426543353926868818 ) ) ;
#1701 = CARTESIAN_POINT ( 'NONE',  ( 22.51849650178394668, 7.817407610814552044, 67.67805970500643298 ) ) ;
#1702 = ORIENTED_EDGE ( 'NONE', *, *, #53762, .T. ) ;
#1703 = B_SPLINE_CURVE_WITH_KNOTS ( 'NONE', 3,
 ( #20258, #36791, #32534, #68776, #26570, #53964, #47665, #16005, #41716, #48008, #10726, #4426, #48337, #32200, #5794, #31848, #5455, #53280, #64196, #14972, #21628, #64548, #36439, #69471, #57892, #25891, #31177, #47321, #52940, #20592, #15330, #58232, #10048, #31505, #21290, #42737, #27952, #48683, #39561, #21975, #17760, #17394, #61010, #38869 ),
 .UNSPECIFIED., .F., .F.,
 ( 4, 2, 2, 2, 2, 2, 2, 2, 2, 2, 2, 2, 2, 2, 2, 2, 2, 2, 2, 2, 2, 4 ),
 ( 0.000000000000000000, 0.003518733725596350382, 0.004398417156995416619, 0.005278100588394483289, 0.007037467451192677345, 0.007917150882591761363, 0.008796834313990845380, 0.01055620117678905678, 0.01231556803958726992, 0.01319525147098637476, 0.01407493490238548133, 0.01495461833378458789, 0.01583430176518369620, 0.01671398519658279930, 0.01759366862798190934, 0.01935303549078008084, 0.02111240235357825928, 0.02199208578497731728, 0.02287176921637638222, 0.02463113607917447739, 0.02639050294197256910, 0.02814986980477066428 ),
 .UNSPECIFIED. ) ;
#1704 = ORIENTED_EDGE ( 'NONE', *, *, #46368, .T. ) ;
#1705 = ORIENTED_EDGE ( 'NONE', *, *, #28112, .T. ) ;
#1706 = CARTESIAN_POINT ( 'NONE',  ( 205.3819056893079278, 107.2819694648321303, -90.01503221354890627 ) ) ;
#1707 = CARTESIAN_POINT ( 'NONE',  ( -109.7686203588201010, 37.90089348911612888, 11.66623203320282975 ) ) ;
#1708 = LINE ( 'NONE', #34768, #38008 ) ;
#1709 = CARTESIAN_POINT ( 'NONE',  ( 200.0000000000000000, 0.000000000000000000, -46.99999999999997158 ) ) ;
#1710 = DIRECTION ( 'NONE',  ( -0.000000000000000000, -0.000000000000000000, 1.000000000000000000 ) ) ;
#1711 = CARTESIAN_POINT ( 'NONE',  ( -146.1260528621668016, 61.36307454672303408, 31.51035454738589792 ) ) ;
#1712 = CARTESIAN_POINT ( 'NONE',  ( -130.6002960060537248, 49.67125682092490280, 59.10497990830987192 ) ) ;
#1713 = CARTESIAN_POINT ( 'NONE',  ( -71.22896441287285541, 20.69091426169410752, -16.76999692228343974 ) ) ;
#1714 = VERTEX_POINT ( 'NONE', #60375 ) ;
#1715 = CARTESIAN_POINT ( 'NONE',  ( 83.37786665291103816, 18.33670623396829313, 70.83248643390679433 ) ) ;
#1716 = ORIENTED_EDGE ( 'NONE', *, *, #22252, .T. ) ;
#1717 = AXIS2_PLACEMENT_3D ( 'NONE', #66276, #45132, #30005 ) ;
#1718 = CARTESIAN_POINT ( 'NONE',  ( 33.44983424733138122, 7.709709042132400825, 42.00358695764388983 ) ) ;
#1719 = DIRECTION ( 'NONE',  ( 0.000000000000000000, 0.000000000000000000, 1.000000000000000000 ) ) ;
#1720 = EDGE_LOOP ( 'NONE', ( #58958, #10654, #36258, #10054 ) ) ;
#1721 = CARTESIAN_POINT ( 'NONE',  ( -6.183861102004804070E-16, 9.237604307034020579, -9.500000000000000000 ) ) ;
#1722 = CARTESIAN_POINT ( 'NONE',  ( -17.50000000000000000, 207.5000000000000284, 0.000000000000000000 ) ) ;
#1724 = LINE ( 'NONE', #12275, #14687 ) ;
#1723 = AXIS2_PLACEMENT_3D ( 'NONE', #47192, #4301, #14500 ) ;
#1725 = CARTESIAN_POINT ( 'NONE',  ( -125.4463376280758098, 47.40387005565909107, 57.47446237482950693 ) ) ;
#1726 = CARTESIAN_POINT ( 'NONE',  ( -47.60396279792519181, 12.80997843568596295, 9.966546515805026374 ) ) ;
#1727 = CARTESIAN_POINT ( 'NONE',  ( 150.8925291903903485, 52.71218673668933974, -47.26666548743844487 ) ) ;
#1729 = DIRECTION ( 'NONE',  ( -0.000000000000000000, -0.000000000000000000, -1.000000000000000000 ) ) ;
#1728 = AXIS2_PLACEMENT_3D ( 'NONE', #2173, #23628, #35212 ) ;
#1730 = AXIS2_PLACEMENT_3D ( 'NONE', #16357, #31849, #58564 ) ;
#1731 = ORIENTED_EDGE ( 'NONE', *, *, #59531, .F. ) ;
#1732 = CARTESIAN_POINT ( 'NONE',  ( 209.9999999999999716, 192.0000000000000000, 72.99999999999998579 ) ) ;
#1733 = CARTESIAN_POINT ( 'NONE',  ( -65.36598343705435354, 0.000000000000000000, 41.38025477438755928 ) ) ;
#1734 = VERTEX_POINT ( 'NONE', #23450 ) ;
#1735 = CARTESIAN_POINT ( 'NONE',  ( 63.01563776193091826, -170.0000000000000000, 64.15751152968499582 ) ) ;
#1736 = CARTESIAN_POINT ( 'NONE',  ( -20.16272189348855903, 400.0000000000064801, 321.0502958579853043 ) ) ;
#1737 = DIRECTION ( 'NONE',  ( -0.000000000000000000, 1.000000000000000000, -0.000000000000000000 ) ) ;
#1738 = ORIENTED_EDGE ( 'NONE', *, *, #8963, .F. ) ;
#1739 = DIRECTION ( 'NONE',  ( -1.000000000000000000, -0.000000000000000000, -0.000000000000000000 ) ) ;
#1740 = VECTOR ( 'NONE', #65545, 1000.000000000000000 ) ;
#1741 = CARTESIAN_POINT ( 'NONE',  ( 152.1381498073141358, 54.87048121475574192, -75.76501768209521970 ) ) ;
#1742 = CARTESIAN_POINT ( 'NONE',  ( 43.96421756700841144, 10.06386361114660488, 31.44109886963873635 ) ) ;
#1743 = CARTESIAN_POINT ( 'NONE',  ( -24.70354720400823112, 8.582324684301861240, 67.89677931424583335 ) ) ;
#1744 = B_SPLINE_CURVE_WITH_KNOTS ( 'NONE', 3,
 ( #15560, #52825, #20142, #58123, #31054, #9939, #26801, #52498, #48228, #64084, #10961, #47541, #58792, #26111, #21181, #26460, #31728, #4648, #20829, #41594, #69005, #42288, #25781, #47208, #64427, #63751, #4317, #58449, #42627, #10267, #63052, #53162, #15896, #37340, #16238, #32428, #37690, #57779, #59138, #53855, #46876, #68667, #68340 ),
 .UNSPECIFIED., .F., .F.,
 ( 4, 2, 2, 2, 2, 2, 2, 2, 1, 2, 2, 2, 2, 2, 2, 2, 2, 2, 2, 2, 2, 4 ),
 ( 3.469446951953614189E-18, 0.001466285743483490599, 0.002199428615225229935, 0.002932571486966969922, 0.004398857230450423442, 0.005865142973933877395, 0.007331428717417331348, 0.008064571589159075238, 0.008797714460900817393, 0.009530857332642563018, 0.01026400020438430691, 0.01173028594786779469, 0.01319657169135128420, 0.01466285743483477372, 0.01539600030657651934, 0.01612914317831826497, 0.01759542892180175969, 0.01906171466528525787, 0.01979485753702700523, 0.02052800040876874912, 0.02199428615225222997, 0.02346057189573570734 ),
 .UNSPECIFIED. ) ;
#1745 = EDGE_CURVE ( 'NONE', #50582, #41326, #16091, .T. ) ;
#1746 = EDGE_LOOP ( 'NONE', ( #27404, #16430, #22724, #24439 ) ) ;
#1747 = ORIENTED_EDGE ( 'NONE', *, *, #14153, .F. ) ;
#1748 = DIRECTION ( 'NONE',  ( 0.000000000000000000, -1.000000000000000000, 0.000000000000000000 ) ) ;
#1749 = ORIENTED_EDGE ( 'NONE', *, *, #35351, .F. ) ;
#1750 = CARTESIAN_POINT ( 'NONE',  ( 432.4999999999999432, -18.06806526123148160, 378.0000000000000000 ) ) ;
#1751 = CARTESIAN_POINT ( 'NONE',  ( -53.09243148547984248, -24.18057212396687206, 27.58472315868180402 ) ) ;
#1752 = FILL_AREA_STYLE ('',( #65780 ) ) ;
#1753 = CARTESIAN_POINT ( 'NONE',  ( 140.9255869758567030, 47.06171785931592666, 88.16863402254999471 ) ) ;
#1754 = B_SPLINE_CURVE_WITH_KNOTS ( 'NONE', 3,
 ( #19820, #14871, #13503, #35655, #3984, #51486, #45500, #19461, #30026, #41611, #2600, #41273, #67328, #63067, #13840, #36339, #25455, #57791, #40920, #8919, #35992, #3295, #66985, #24060, #18777, #31072, #40233, #62380, #8227, #67665, #40570, #57447, #29674, #61681, #34959, #62021, #62731, #56403, #51136, #2952, #46536, #14196, #20158 ),
 .UNSPECIFIED., .F., .F.,
 ( 4, 2, 2, 2, 2, 2, 2, 2, 2, 2, 2, 2, 1, 2, 2, 2, 2, 2, 2, 2, 2, 4 ),
 ( 0.02362927190606133043, 0.02510248541563190466, 0.02583909217041719872, 0.02657569892520248930, 0.02804891243477306007, 0.02952212594434362736, 0.03025873269912889713, 0.03099533945391416689, 0.03246855296348473419, 0.03394176647305530842, 0.03541497998262588265, 0.03615158673741118711, 0.03688819349219649157, 0.03762480024698179604, 0.03836140700176710744, 0.03983462051133768167, 0.04130783402090825590, 0.04278104753047883013, 0.04351765428526413459, 0.04425426104004942518, 0.04572747454962002023, 0.04720068805919060834 ),
 .UNSPECIFIED. ) ;
#1755 = EDGE_CURVE ( 'NONE', #52438, #42077, #26195, .T. ) ;
#1756 = CARTESIAN_POINT ( 'NONE',  ( -190.6985136298601731, 109.1272424661242582, -95.00000000000133582 ) ) ;
#1757 = CARTESIAN_POINT ( 'NONE',  ( -25.87147652227456263, 70.00000000000000000, 129.5802547743875550 ) ) ;
#1758 = ORIENTED_EDGE ( 'NONE', *, *, #20251, .T. ) ;
#1759 = ADVANCED_FACE ( 'NONE', ( #12190 ), #60716, .F. ) ;
#1760 = LINE ( 'NONE', #39734, #62732 ) ;
#1761 = EDGE_CURVE ( 'NONE', #54242, #40885, #49448, .T. ) ;
#1762 = ORIENTED_EDGE ( 'NONE', *, *, #15857, .T. ) ;
#1763 = CARTESIAN_POINT ( 'NONE',  ( 164.0158927577712689, 62.92463143894076438, -20.47931855560399939 ) ) ;
#1764 = DIRECTION ( 'NONE',  ( 0.000000000000000000, 0.000000000000000000, 1.000000000000000000 ) ) ;
#1765 = LINE ( 'NONE', #12662, #64488 ) ;
#1766 = FACE_OUTER_BOUND ( 'NONE', #21460, .T. ) ;
#1767 = DIRECTION ( 'NONE',  ( 1.000000000000000000, 0.000000000000000000, -0.000000000000000000 ) ) ;
#1768 = EDGE_CURVE ( 'NONE', #27095, #38528, #55793, .T. ) ;
#1769 = ORIENTED_EDGE ( 'NONE', *, *, #50561, .T. ) ;
#1770 = ORIENTED_EDGE ( 'NONE', *, *, #13048, .F. ) ;
#1771 = CARTESIAN_POINT ( 'NONE',  ( 9.827939172326081163, 6.382931149346556587, 42.09375525668145457 ) ) ;
#1772 = ORIENTED_EDGE ( 'NONE', *, *, #31156, .T. ) ;
#1773 = CONICAL_SURFACE ( 'NONE', #21987, 74.95140232871122521, 0.8777644062502172329 ) ;
#1774 = CARTESIAN_POINT ( 'NONE',  ( 63.98689050258324329, 13.93365232918668006, 71.61000602743803256 ) ) ;
#1775 = DIRECTION ( 'NONE',  ( -0.000000000000000000, -0.000000000000000000, -1.000000000000000000 ) ) ;
#1776 = CIRCLE ( 'NONE', #53407, 5.000000000000170530 ) ;
#1777 = ORIENTED_EDGE ( 'NONE', *, *, #26829, .F. ) ;
#1778 = CARTESIAN_POINT ( 'NONE',  ( -142.9728934044261734, 58.82891228489261692, -72.87700524141401104 ) ) ;
#1779 = CARTESIAN_POINT ( 'NONE',  ( 92.21267147730743829, 21.40196534721318500, 15.39891977708759008 ) ) ;
#1780 = EDGE_CURVE ( 'NONE', #45155, #31339, #43825, .T. ) ;
#1781 = DIRECTION ( 'NONE',  ( -0.8160245890732938934, -0.5780171883497599028, 0.000000000000000000 ) ) ;
#1782 = CIRCLE ( 'NONE', #53411, 65.00000000000000000 ) ;
#1783 = AXIS2_PLACEMENT_3D ( 'NONE', #7114, #56339, #29267 ) ;
#1784 = VERTEX_POINT ( 'NONE', #38561 ) ;
#1785 = AXIS2_PLACEMENT_3D ( 'NONE', #57977, #31583, #20336 ) ;
#1786 = EDGE_CURVE ( 'NONE', #2896, #55220, #18505, .T. ) ;
#1787 = CARTESIAN_POINT ( 'NONE',  ( -447.6627218934913230, 399.9999999999997726, 83.55029585798818914 ) ) ;
#1788 = AXIS2_PLACEMENT_3D ( 'NONE', #24721, #40533, #2565 ) ;
#1789 = CARTESIAN_POINT ( 'NONE',  ( 62.71085615297809568, 13.63476094311646492, 83.50115473030093938 ) ) ;
#1790 = LINE ( 'NONE', #17961, #25329 ) ;
#1791 = AXIS2_PLACEMENT_3D ( 'NONE', #65034, #34080, #59734 ) ;
#1792 = CARTESIAN_POINT ( 'NONE',  ( -180.0094637318086939, 96.72611451757710199, -45.19277143581986422 ) ) ;
#1793 = CARTESIAN_POINT ( 'NONE',  ( -180.5668408223793904, 97.41302302526328560, -95.00000000000133582 ) ) ;
#1794 = CARTESIAN_POINT ( 'NONE',  ( 156.5909039492009640, 56.96742803863245541, 71.25401806271710825 ) ) ;
#1795 =( REPRESENTATION_RELATIONSHIP ('NONE','NONE', #40274, #64096 ) REPRESENTATION_RELATIONSHIP_WITH_TRANSFORMATION ( #45259 )SHAPE_REPRESENTATION_RELATIONSHIP( ) );
#1796 = CARTESIAN_POINT ( 'NONE',  ( 127.2397149628677937, 37.56999625068102233, -66.79971066083803066 ) ) ;
#1797 = EDGE_LOOP ( 'NONE', ( #65731, #29293 ) ) ;
#1798 = CARTESIAN_POINT ( 'NONE',  ( 141.3036441389950539, 47.31002705502925920, -71.40782174165585161 ) ) ;
#1799 = CARTESIAN_POINT ( 'NONE',  ( -85.35521056349260505, 26.07297753498038873, 94.99999999999866418 ) ) ;
#1800 = ORIENTED_EDGE ( 'NONE', *, *, #68219, .F. ) ;
#1801 = CARTESIAN_POINT ( 'NONE',  ( -150.5993571094983281, 66.43939758484179947, -49.73612197178368177 ) ) ;
#1802 = CARTESIAN_POINT ( 'NONE',  ( -2.874437057892789138, 6.618922960888051321, -75.41744632663154846 ) ) ;
#1803 = CARTESIAN_POINT ( 'NONE',  ( -38.69449158134467837, 11.92067517118077014, 35.75389334926249063 ) ) ;
#1804 = DIRECTION ( 'NONE',  ( 0.000000000000000000, -1.000000000000000000, 0.000000000000000000 ) ) ;
#1805 = CARTESIAN_POINT ( 'NONE',  ( -173.1211646369891355, 87.12891641440857882, -49.71195716475001092 ) ) ;
#1806 = LINE ( 'NONE', #55245, #35511 ) ;
#1807 = CARTESIAN_POINT ( 'NONE',  ( -14.96764630465879797, 7.461781624211967667, -94.16342404306476510 ) ) ;
#1808 = FACE_OUTER_BOUND ( 'NONE', #63947, .T. ) ;
#1809 = CARTESIAN_POINT ( 'NONE',  ( -7.486743542469090684, -64.58150799671139453, 0.000000000000000000 ) ) ;
#1810 = CARTESIAN_POINT ( 'NONE',  ( 0.000000000000000000, 190.0000000000000000, 159.3522585083728700 ) ) ;
#1811 = CARTESIAN_POINT ( 'NONE',  ( 164.8471526211111211, 63.62172173173269130, 11.44683124855694523 ) ) ;
#1812 = CARTESIAN_POINT ( 'NONE',  ( 188.9999999999999432, 190.0000000000000000, 380.0000000000000000 ) ) ;
#1813 = ORIENTED_EDGE ( 'NONE', *, *, #39226, .T. ) ;
#1814 = CARTESIAN_POINT ( 'NONE',  ( -97.88021438939453844, 31.71889184683102059, -36.42215870048158166 ) ) ;
#1815 = ORIENTED_EDGE ( 'NONE', *, *, #68701, .T. ) ;
#1816 = DIRECTION ( 'NONE',  ( -0.9639628606958550172, 0.2660368455666687892, 0.000000000000000000 ) ) ;
#1817 = CARTESIAN_POINT ( 'NONE',  ( 80.15818551272217007, 18.36718314243333694, -66.34257447059830781 ) ) ;
#1818 = CARTESIAN_POINT ( 'NONE',  ( -5.767955557622883589E-14, -26.11269837220806522, 2.000000000000001776 ) ) ;
#1819 = DIRECTION ( 'NONE',  ( 0.000000000000000000, 0.000000000000000000, 1.000000000000000000 ) ) ;
#1820 = CARTESIAN_POINT ( 'NONE',  ( 69.72313848477159581, -27.50266661387038170, 41.38025477438755928 ) ) ;
#1821 = FACE_OUTER_BOUND ( 'NONE', #57597, .T. ) ;
#1822 = DIRECTION ( 'NONE',  ( -0.000000000000000000, -0.000000000000000000, -1.000000000000000000 ) ) ;
#1823 = CARTESIAN_POINT ( 'NONE',  ( -118.3948752128398922, 42.92869324237092599, -15.27178645307563798 ) ) ;
#1824 = ORIENTED_EDGE ( 'NONE', *, *, #5705, .T. ) ;
#1825 = EDGE_LOOP ( 'NONE', ( #14686, #30540, #26848, #56419 ) ) ;
#1826 = EDGE_CURVE ( 'NONE', #31701, #24549, #49803, .T. ) ;
#1827 = CARTESIAN_POINT ( 'NONE',  ( 445.3372781065085633, 177.8591479523844612, -111.4497041420119388 ) ) ;
#1828 = CARTESIAN_POINT ( 'NONE',  ( 174.1364721914476661, 71.85829564941441561, 60.81373415767276924 ) ) ;
#1829 = DIRECTION ( 'NONE',  ( -1.000000000000000000, 0.000000000000000000, 0.000000000000000000 ) ) ;
#1830 = AXIS2_PLACEMENT_3D ( 'NONE', #9232, #40890, #24728 ) ;
#1831 = CARTESIAN_POINT ( 'NONE',  ( -165.6215009671260816, 80.58889799860445180, 65.48035359524065768 ) ) ;
#1832 = ADVANCED_FACE ( 'NONE', ( #65660 ), #28357, .T. ) ;
#1833 = CARTESIAN_POINT ( 'NONE',  ( -168.1811549361196967, 83.25427431521136157, -21.01567069218833694 ) ) ;
#1834 = AXIS2_PLACEMENT_3D ( 'NONE', #63579, #5178, #9774 ) ;
#1835 = CARTESIAN_POINT ( 'NONE',  ( -27.00000000000000355, -27.00000000000000355, 15.00000000000000000 ) ) ;
#1836 = VERTEX_POINT ( 'NONE', #54735 ) ;
#1837 = CARTESIAN_POINT ( 'NONE',  ( 94.06416612695406343, 23.16920323269611970, 11.38599088637463019 ) ) ;
#1838 = VECTOR ( 'NONE', #46198, 1000.000000000000000 ) ;
#1839 = VECTOR ( 'NONE', #27527, 1000.000000000000000 ) ;
#1840 = CARTESIAN_POINT ( 'NONE',  ( -190.6985136298601731, 109.1272424661242582, 94.99999999999866418 ) ) ;
#1841 = CARTESIAN_POINT ( 'NONE',  ( -12.99999999999999645, 0.000000000000000000, -33.00000000000000000 ) ) ;
#1842 = CARTESIAN_POINT ( 'NONE',  ( -173.1211646369891355, -170.0000000000000000, 11.47714401617735902 ) ) ;
#1843 = CARTESIAN_POINT ( 'NONE',  ( 212.1535111375854683, 117.1635556319084657, -16.15046538589425751 ) ) ;
#1844 = FACE_BOUND ( 'NONE', #16370, .T. ) ;
#1845 = AXIS2_PLACEMENT_3D ( 'NONE', #66045, #55461, #67418 ) ;
#1846 = CARTESIAN_POINT ( 'NONE',  ( -62.48965350618343706, 16.80247907725181378, -41.71376395946558091 ) ) ;
#1847 = EDGE_CURVE ( 'NONE', #43438, #48157, #42746, .T. ) ;
#1848 = VECTOR ( 'NONE', #11811, 1000.000000000000000 ) ;
#1849 = AXIS2_PLACEMENT_3D ( 'NONE', #48486, #323, #32687 ) ;
#1850 = EDGE_CURVE ( 'NONE', #58197, #53112, #45577, .T. ) ;
#1851 = ORIENTED_EDGE ( 'NONE', *, *, #49528, .F. ) ;
#1852 = EDGE_CURVE ( 'NONE', #67175, #45635, #9379, .T. ) ;
#1853 = DIRECTION ( 'NONE',  ( -1.000000000000000000, 0.000000000000000000, 0.000000000000000000 ) ) ;
#1854 = CARTESIAN_POINT ( 'NONE',  ( -17.50000000000002842, -18.06806526123148160, 380.0000000000000000 ) ) ;
#1855 = CARTESIAN_POINT ( 'NONE',  ( -47.60266343315662851, 13.84328785304053966, 65.66110071374279755 ) ) ;
#1856 = CARTESIAN_POINT ( 'NONE',  ( -177.5100621450479252, 93.70693725195826573, 5.377500373651478149 ) ) ;
#1857 = CARTESIAN_POINT ( 'NONE',  ( 211.7357196141372242, 118.3691710715567211, 66.16139203830061888 ) ) ;
#1858 = CARTESIAN_POINT ( 'NONE',  ( 83.37786665291105237, 18.33670623396829669, -63.39026651841162163 ) ) ;
#1859 = VERTEX_POINT ( 'NONE', #41000 ) ;
#1860 = LINE ( 'NONE', #18024, #9010 ) ;
#1861 = CARTESIAN_POINT ( 'NONE',  ( 0.000000000000000000, 0.000000000000000000, 10.00000000000000000 ) ) ;
#1862 = ORIENTED_EDGE ( 'NONE', *, *, #67850, .F. ) ;
#1863 = DIRECTION ( 'NONE',  ( 0.000000000000000000, -1.000000000000000000, 0.000000000000000000 ) ) ;
#1864 = ORIENTED_EDGE ( 'NONE', *, *, #9538, .T. ) ;
#1865 = CARTESIAN_POINT ( 'NONE',  ( 41.49663191311347532, 50.03028622612080767, 170.0000000000000000 ) ) ;
#1866 = CARTESIAN_POINT ( 'NONE',  ( -62.06231780744543869, 17.72446026058425517, -13.19249544724704037 ) ) ;
#1867 = FACE_OUTER_BOUND ( 'NONE', #43871, .T. ) ;
#1868 = ORIENTED_EDGE ( 'NONE', *, *, #4757, .T. ) ;
#1869 = EDGE_LOOP ( 'NONE', ( #22751, #69273, #8707 ) ) ;
#1870 = DIRECTION ( 'NONE',  ( -0.000000000000000000, 1.000000000000000000, -0.000000000000000000 ) ) ;
#1871 = DIRECTION ( 'NONE',  ( 0.9510565162951545304, -0.3090169943749447312, 5.102127870520021228E-18 ) ) ;
#1872 = CARTESIAN_POINT ( 'NONE',  ( -155.5977325361978103, 70.88311713755700794, -64.77305499973000735 ) ) ;
#1873 = CARTESIAN_POINT ( 'NONE',  ( 67.93154431625912082, 14.90489441944787252, 4.782582000548346812 ) ) ;
#1874 = LINE ( 'NONE', #65182, #66878 ) ;
#1875 = ORIENTED_EDGE ( 'NONE', *, *, #20675, .F. ) ;
#1876 = EDGE_CURVE ( 'NONE', #59383, #13453, #2673, .T. ) ;
#1877 = PRODUCT_DEFINITION_SHAPE ( 'NONE', 'NONE',  #58964 ) ;
#1878 =( NAMED_UNIT ( * ) PLANE_ANGLE_UNIT ( ) SI_UNIT ( $, .RADIAN. ) );
#1879 = CIRCLE ( 'NONE', #29940, 1.500000000000001332 ) ;
#1880 = CARTESIAN_POINT ( 'NONE',  ( -53.31111153860250340, -37.18770477615797176, 40.00000000000003553 ) ) ;
#1881 = CARTESIAN_POINT ( 'NONE',  ( -133.0921934900200370, 52.65587531157186874, -13.44671944861685908 ) ) ;
#1882 = CARTESIAN_POINT ( 'NONE',  ( 447.3372781065085633, 217.8591479523844612, -111.4497041420119388 ) ) ;
#1883 = DIRECTION ( 'NONE',  ( 0.000000000000000000, 0.000000000000000000, -1.000000000000000000 ) ) ;
#1884 = CARTESIAN_POINT ( 'NONE',  ( 15.68296563925591514, -63.09411298019745828, 41.38025477438755928 ) ) ;
#1886 = ORIENTED_EDGE ( 'NONE', *, *, #48178, .F. ) ;
#1885 = PLANE ( 'NONE',  #60224 ) ;
#1887 = VERTEX_POINT ( 'NONE', #41685 ) ;
#1888 = VECTOR ( 'NONE', #8941, 1000.000000000000000 ) ;
#1889 = EDGE_LOOP ( 'NONE', ( #31139, #2749, #9487, #15334 ) ) ;
#1890 = CARTESIAN_POINT ( 'NONE',  ( 0.1306530452038070222, -5.952467836904146381, 5.690023276062398772 ) ) ;
#1891 = FACE_OUTER_BOUND ( 'NONE', #33481, .T. ) ;
#1892 = CARTESIAN_POINT ( 'NONE',  ( -48.04019567818505010, 12.91272349839804789, -13.20040436305664855 ) ) ;
#1893 = CARTESIAN_POINT ( 'NONE',  ( 102.7425154123292543, 25.56407025871219574, -16.81959381298093348 ) ) ;
#1894 = CARTESIAN_POINT ( 'NONE',  ( 41.66904755831210849, -9.150666335777657423E-14, 85.00100000000000477 ) ) ;
#1895 = CARTESIAN_POINT ( 'NONE',  ( 201.5903370237274714, 102.1785392640257868, 3.023677376802185179 ) ) ;
#1896 = CARTESIAN_POINT ( 'NONE',  ( 197.9945392102239055, 99.19564887483076632, 87.01074304022465356 ) ) ;
#1897 = DIRECTION ( 'NONE',  ( -1.000000000000000000, 0.000000000000000000, 0.000000000000000000 ) ) ;
#1898 = CARTESIAN_POINT ( 'NONE',  ( -78.19460645047365688, 22.14203592077027594, -76.96000122218154615 ) ) ;
#1899 = CARTESIAN_POINT ( 'NONE',  ( -13.47680110791657881, 7.324966777230639714, 32.66010570199217256 ) ) ;
#1900 = ORIENTED_EDGE ( 'NONE', *, *, #46935, .F. ) ;
#1901 = AXIS2_PLACEMENT_3D ( 'NONE', #15705, #25241, #62867 ) ;
#1902 = DIRECTION ( 'NONE',  ( 0.000000000000000000, 0.000000000000000000, -1.000000000000000000 ) ) ;
#1903 = ORIENTED_EDGE ( 'NONE', *, *, #43501, .F. ) ;
#1904 = ORIENTED_EDGE ( 'NONE', *, *, #36060, .T. ) ;
#1905 = DIRECTION ( 'NONE',  ( 0.000000000000000000, 0.000000000000000000, 1.000000000000000000 ) ) ;
#1906 = CARTESIAN_POINT ( 'NONE',  ( 60.74750367560238828, -24.13405452624855130, 6.377659838150107425E-18 ) ) ;
#1907 = CARTESIAN_POINT ( 'NONE',  ( -38.73578281104377652, 11.92878435305931539, 89.64055695031605353 ) ) ;
#1908 = CARTESIAN_POINT ( 'NONE',  ( 69.72313848477159581, -27.50266661387038170, 41.38025477438755928 ) ) ;
#1909 = EDGE_CURVE ( 'NONE', #62027, #63672, #20228, .T. ) ;
#1910 = CARTESIAN_POINT ( 'NONE',  ( -3.306248862503413655, 500.0000000000000000, -51.64566090791306863 ) ) ;
#1911 = DIRECTION ( 'NONE',  ( 0.000000000000000000, 0.000000000000000000, 1.000000000000000000 ) ) ;
#1912 = CARTESIAN_POINT ( 'NONE',  ( 110.2429982417149574, -170.0000000000000000, -50.92243756565370916 ) ) ;
#1913 = VERTEX_POINT ( 'NONE', #62456 ) ;
#1914 = VERTEX_POINT ( 'NONE', #24823 ) ;
#1915 = EDGE_CURVE ( 'NONE', #26889, #39680, #35031, .T. ) ;
#1916 = ORIENTED_EDGE ( 'NONE', *, *, #8825, .T. ) ;
#1917 = LINE ( 'NONE', #33223, #50699 ) ;
#1918 = CARTESIAN_POINT ( 'NONE',  ( 112.3013380801408658, 388.0000000000065938, -123.9497041420121235 ) ) ;
#1919 = LINE ( 'NONE', #23373, #50231 ) ;
#1920 = EDGE_CURVE ( 'NONE', #25401, #25095, #25945, .T. ) ;
#1921 = PLANE ( 'NONE',  #11654 ) ;
#1922 = EDGE_CURVE ( 'NONE', #13453, #38828, #44149, .T. ) ;
#1923 = FACE_OUTER_BOUND ( 'NONE', #44162, .T. ) ;
#1924 = CARTESIAN_POINT ( 'NONE',  ( 197.3064269725219617, 98.33232022113060111, 64.86617095098992536 ) ) ;
#1925 = ORIENTED_EDGE ( 'NONE', *, *, #34314, .T. ) ;
#1926 = CARTESIAN_POINT ( 'NONE',  ( -55.05276343752909440, 15.72344139423347364, -62.06087458892354647 ) ) ;
#1927 = CARTESIAN_POINT ( 'NONE',  ( 198.2588776805010298, 99.52972231602372233, -74.52680556020536073 ) ) ;
#1928 = DIRECTION ( 'NONE',  ( 1.000000000000000000, 2.261926634819711547E-29, -9.860761315262647568E-31 ) ) ;
#1929 = CARTESIAN_POINT ( 'NONE',  ( -2.873329055852805514, 7.626065826870670250, -48.57246868976042720 ) ) ;
#1930 = CARTESIAN_POINT ( 'NONE',  ( 109.7774723066848281, 28.66666416591278477, 2.766663615273642574 ) ) ;
#1931 = CARTESIAN_POINT ( 'NONE',  ( -170.0785278435570547, 83.80419503909187995, -89.03350163840394771 ) ) ;
#1932 = CYLINDRICAL_SURFACE ( 'NONE', #27329, 65.36598343705435354 ) ;
#1933 = FACE_BOUND ( 'NONE', #29391, .T. ) ;
#1934 = CARTESIAN_POINT ( 'NONE',  ( -189.2641795714223178, 107.1238410236401677, 91.36523946422995834 ) ) ;
#1935 = AXIS2_PLACEMENT_3D ( 'NONE', #55616, #50350, #54908 ) ;
#1936 = EDGE_CURVE ( 'NONE', #11965, #32966, #17681, .T. ) ;
#1937 = ORIENTED_EDGE ( 'NONE', *, *, #57039, .T. ) ;
#1938 = VECTOR ( 'NONE', #46028, 1000.000000000000000 ) ;
#1939 = CARTESIAN_POINT ( 'NONE',  ( 276.6934359423128740, 21.67676124233544499, 3.764605836381906379 ) ) ;
#1940 = CARTESIAN_POINT ( 'NONE',  ( -133.3392045760936355, 51.59583146030202983, -70.31251124416750997 ) ) ;
#1941 = CARTESIAN_POINT ( 'NONE',  ( 133.8566784816069628, 41.42467568809806977, -62.86786152285933582 ) ) ;
#1942 = CARTESIAN_POINT ( 'NONE',  ( 50.97490815085634352, 6.000000000000000000, -46.68900338898716029 ) ) ;
#1943 = CARTESIAN_POINT ( 'NONE',  ( -0.2727178028659107967, 2.936090700955778964E-15, -23.97499999999999787 ) ) ;
#1944 = AXIS2_PLACEMENT_3D ( 'NONE', #14779, #57012, #9163 ) ;
#1945 = ORIENTED_EDGE ( 'NONE', *, *, #538, .F. ) ;
#1946 = CARTESIAN_POINT ( 'NONE',  ( 110.0000000000000284, -21.42428528562853174, -5.000000000000004441 ) ) ;
#1947 = CARTESIAN_POINT ( 'NONE',  ( 188.3602976857901865, 86.28604666859746430, 92.35901500848406442 ) ) ;
#1948 = ORIENTED_EDGE ( 'NONE', *, *, #5686, .T. ) ;
#1949 = AXIS2_PLACEMENT_3D ( 'NONE', #32493, #31802, #6093 ) ;
#1950 = ORIENTED_EDGE ( 'NONE', *, *, #16118, .F. ) ;
#1951 = CARTESIAN_POINT ( 'NONE',  ( 175.8855729601531550, 73.50624012737691260, -49.15246532231710574 ) ) ;
#1952 = CARTESIAN_POINT ( 'NONE',  ( 149.9683128897950155, 53.28564708287392193, 37.43972384951239718 ) ) ;
#1953 = DIRECTION ( 'NONE',  ( -0.000000000000000000, -0.000000000000000000, 1.000000000000000000 ) ) ;
#1954 = ORIENTED_EDGE ( 'NONE', *, *, #17726, .F. ) ;
#1955 = CYLINDRICAL_SURFACE ( 'NONE', #41330, 7.500000000000013323 ) ;
#1956 = CARTESIAN_POINT ( 'NONE',  ( -175.1920326508033270, 89.46239303019292777, 4.256113626765591462 ) ) ;
#1957 = CARTESIAN_POINT ( 'NONE',  ( -71.41745561414268195, 19.69148172991712542, -40.62644917380843168 ) ) ;
#1958 = CARTESIAN_POINT ( 'NONE',  ( -102.2801239173131194, -170.0000000000000000, 18.67452391595144334 ) ) ;
#1959 = CARTESIAN_POINT ( 'NONE',  ( -30.94745021534356155, 10.53010394565407459, -8.472646774738157305 ) ) ;
#1960 = CARTESIAN_POINT ( 'NONE',  ( -189.2346268516247676, 107.0830361517165130, 38.63455055429937346 ) ) ;
#1961 = EDGE_LOOP ( 'NONE', ( #40526, #24326, #2830, #6923 ) ) ;
#1962 = CARTESIAN_POINT ( 'NONE',  ( -2.368959188627906887, 24.88750755625416744, 0.000000000000000000 ) ) ;
#1963 = CARTESIAN_POINT ( 'NONE',  ( -75.65611349188962720, 22.26947559308019464, 4.200113054923877876 ) ) ;
#1964 = CARTESIAN_POINT ( 'NONE',  ( 46.84183314611287585, 9.494161546644493299, -42.14055136037359972 ) ) ;
#1965 = CARTESIAN_POINT ( 'NONE',  ( 45.69927128652683734, 36.58596684574255420, -74.30072871347310581 ) ) ;
#1967 = ORIENTED_EDGE ( 'NONE', *, *, #20792, .F. ) ;
#1966 = CARTESIAN_POINT ( 'NONE',  ( -189.8133172329396814, 107.8858115918112901, 94.99999999999866418 ) ) ;
#1968 = CARTESIAN_POINT ( 'NONE',  ( 80.17205177205136124, 17.31791394718354482, -47.14471772045799014 ) ) ;
#1969 = VERTEX_POINT ( 'NONE', #10026 ) ;
#1970 = CARTESIAN_POINT ( 'NONE',  ( -145.3279998500303520, 60.71393190715793509, 58.83337766670971547 ) ) ;
#1971 = VECTOR ( 'NONE', #42579, 1000.000000000000227 ) ;
#1972 = CARTESIAN_POINT ( 'NONE',  ( 80.73462811483979351, 18.54763808182592300, 32.54810887579326817 ) ) ;
#1973 = DIRECTION ( 'NONE',  ( -0.000000000000000000, -0.000000000000000000, 1.000000000000000000 ) ) ;
#1974 = PLANE ( 'NONE',  #39498 ) ;
#1975 = CARTESIAN_POINT ( 'NONE',  ( -119.2982054035570769, 42.30181775808004119, 61.38488466982619940 ) ) ;
#1976 = VECTOR ( 'NONE', #23288, 1000.000000000000000 ) ;
#1977 = CARTESIAN_POINT ( 'NONE',  ( 43.35536254672136636, 9.973606330917816010, 4.191193481081563199 ) ) ;
#1978 = CARTESIAN_POINT ( 'NONE',  ( -180.0094637318086370, 96.72611451757705936, -18.34822084535621300 ) ) ;
#1979 = CARTESIAN_POINT ( 'NONE',  ( 0.1285234777254253835, 24.99966963213046611, 0.000000000000000000 ) ) ;
#1980 = ORIENTED_EDGE ( 'NONE', *, *, #53959, .F. ) ;
#1981 = ORIENTED_EDGE ( 'NONE', *, *, #63831, .F. ) ;
#1982 = AXIS2_PLACEMENT_3D ( 'NONE', #37710, #69378, #69021 ) ;
#1983 = B_SPLINE_CURVE_WITH_KNOTS ( 'NONE', 3,
 ( #43560, #49173, #65032, #65387, #16830, #38946, #1014, #22464, #17174, #11909, #49526, #63991, #5251, #26710, #48141, #21420, #42863, #64333, #10866, #13316, #66448, #28437, #28799, #13649, #17534, #6984, #55161, #8027, #40382, #7343, #39006, #55515, #50590, #49889, #60450, #1712, #2411, #45666, #35103, #67144, #12266, #56558, #18235, #66098, #23174, #50941 ),
 .UNSPECIFIED., .F., .F.,
 ( 4, 2, 2, 2, 2, 2, 2, 2, 2, 2, 2, 2, 2, 2, 2, 2, 2, 2, 2, 2, 2, 2, 4 ),
 ( 0.000000000000000000, 0.001615199098318991942, 0.003230398196637983884, 0.004037997745797491239, 0.004845597294956999028, 0.006460796393275994656, 0.007268395942435511986, 0.008075995491595029316, 0.009691194589914013668, 0.01049879413907353967, 0.01130639368823306568, 0.01211399323739259168, 0.01292159278655211595, 0.01453679188487112459, 0.01615199098319013496, 0.01695959053234963321, 0.01776719008150913146, 0.01938238917982806203, 0.02099758827814698914, 0.02180518782730647698, 0.02261278737646596829, 0.02422798647478494050, 0.02584318557310391617 ),
 .UNSPECIFIED. ) ;
#1984 = CARTESIAN_POINT ( 'NONE',  ( 43.97326221476412655, 9.047815246749992824, 43.37997826269698010 ) ) ;
#1985 = CARTESIAN_POINT ( 'NONE',  ( 197.3059626281005592, 96.72682679064189415, -15.67053974981288000 ) ) ;
#1986 = LINE ( 'NONE', #30100, #9912 ) ;
#1987 = CARTESIAN_POINT ( 'NONE',  ( 144.4165763529819344, -26.99999999999998224, 108.9999999999999858 ) ) ;
#1988 = MECHANICAL_DESIGN_GEOMETRIC_PRESENTATION_REPRESENTATION (  '', ( #14333 ), #912 ) ;
#1989 = CARTESIAN_POINT ( 'NONE',  ( 181.0840389613909736, -170.0000000000000000, -78.06960825634331513 ) ) ;
#1990 = CARTESIAN_POINT ( 'NONE',  ( -76.78104518372332166, 22.68568622761702969, -76.73470982633753579 ) ) ;
#1991 = CIRCLE ( 'NONE', #26677, 243.4957430088094839 ) ;
#1992 = CARTESIAN_POINT ( 'NONE',  ( -102.2801239173131052, 32.78103895658058065, 72.36362509687883460 ) ) ;
#1993 = CARTESIAN_POINT ( 'NONE',  ( -25.81763596640061209, 8.735969132042866292, -47.78813171631949785 ) ) ;
#1994 = DIRECTION ( 'NONE',  ( -0.000000000000000000, -0.000000000000000000, 1.000000000000000000 ) ) ;
#1995 = ORIENTED_EDGE ( 'NONE', *, *, #35814, .T. ) ;
#1996 = EDGE_CURVE ( 'NONE', #60543, #5635, #11609, .T. ) ;
#1997 = ORIENTED_EDGE ( 'NONE', *, *, #12232, .T. ) ;
#1999 = VECTOR ( 'NONE', #221, 1000.000000000000114 ) ;
#1998 = PLANE ( 'NONE',  #19559 ) ;
#2000 = CARTESIAN_POINT ( 'NONE',  ( 15.78827728214693416, -170.0000000000000000, -96.70804527961315955 ) ) ;
#2001 = DIRECTION ( 'NONE',  ( -0.000000000000000000, 0.000000000000000000, 1.000000000000000000 ) ) ;
#2002 = CARTESIAN_POINT ( 'NONE',  ( 126.4219470349616188, 38.26519385429183018, 38.03294307216089720 ) ) ;
#2003 = CARTESIAN_POINT ( 'NONE',  ( 107.4937869665630359, -21.56868463414005177, -4.338918127843130357 ) ) ;
#2004 = DIRECTION ( 'NONE',  ( 0.000000000000000000, 0.000000000000000000, 1.000000000000000000 ) ) ;
#2005 = EDGE_CURVE ( 'NONE', #64974, #46266, #58883, .T. ) ;
#2006 = CARTESIAN_POINT ( 'NONE',  ( -98.67557579989349392, 32.10670856967971076, -22.26450473806611541 ) ) ;
#2007 = CARTESIAN_POINT ( 'NONE',  ( 39.40195752203892710, 8.409560354027384221, 71.75838489642698903 ) ) ;
#2008 = CARTESIAN_POINT ( 'NONE',  ( 313.9975424824652350, 172.0000000000000284, 418.0000000000000000 ) ) ;
#2009 = DIRECTION ( 'NONE',  ( 0.000000000000000000, 0.000000000000000000, 1.000000000000000000 ) ) ;
#2010 = EDGE_LOOP ( 'NONE', ( #40359, #25395, #54246, #10560 ) ) ;
#2011 = CARTESIAN_POINT ( 'NONE',  ( 62.52762183777206673, 13.59210632617624803, 71.65751152968498161 ) ) ;
#2012 = CARTESIAN_POINT ( 'NONE',  ( 188.9999999999999432, 0.000000000000000000, 380.0000000000000000 ) ) ;
#2013 = CARTESIAN_POINT ( 'NONE',  ( -15.07533778868020313, 8.482826962130836534, 12.70726733519779827 ) ) ;
#2014 = CARTESIAN_POINT ( 'NONE',  ( 169.9999999999999716, -6.319444444444440201, 4.000000000000000000 ) ) ;
#2015 = DIRECTION ( 'NONE',  ( -1.000000000000000000, -0.000000000000000000, -0.000000000000000000 ) ) ;
#2016 = CARTESIAN_POINT ( 'NONE',  ( 132.9557829392755082, 42.05591979570419880, -24.13845282381304003 ) ) ;
#2017 = EDGE_CURVE ( 'NONE', #53513, #46954, #10698, .T. ) ;
#2018 = VERTEX_POINT ( 'NONE', #25866 ) ;
#2019 = APPLICATION_PROTOCOL_DEFINITION ( 'draft international standard', 'automotive_design', 1998, #28708 ) ;
#2020 = CARTESIAN_POINT ( 'NONE',  ( 10.55634918610411432, 46.66904755831205875, 85.00100000000000477 ) ) ;
#2021 = DIRECTION ( 'NONE',  ( -1.000000000000000000, 0.000000000000000000, 0.000000000000000000 ) ) ;
#2022 = CARTESIAN_POINT ( 'NONE',  ( 0.7145311798163268557, -9.237604307034018802, 5.946466066724412554E-16 ) ) ;
#2023 = CARTESIAN_POINT ( 'NONE',  ( -175.2564835000419805, 89.53548519733848821, 84.80368869902895312 ) ) ;
#2024 = ORIENTED_EDGE ( 'NONE', *, *, #65884, .F. ) ;
#2025 = FACE_OUTER_BOUND ( 'NONE', #12896, .T. ) ;
#2026 = VECTOR ( 'NONE', #28313, 1000.000000000000000 ) ;
#2027 = B_SPLINE_CURVE_WITH_KNOTS ( 'NONE', 3,
 ( #27187, #31785, #68718, #15950, #37745, #48618, #25834, #37395, #59190, #37061, #47262, #63457, #58499, #26164, #47596, #69054, #38447, #34222, #6441, #28949, #17695, #59535, #2214, #27534, #44772, #22610, #11352, #64834, #59884, #66249, #12762, #7131, #819, #60247, #33176, #28592, #1872, #49677, #65180, #44055, #18040, #60943, #11703, #12065, #33870, #55666, #23328, #39492 ),
 .UNSPECIFIED., .F., .F.,
 ( 4, 2, 2, 2, 2, 2, 2, 2, 2, 2, 2, 2, 2, 2, 2, 2, 2, 2, 2, 2, 2, 2, 2, 4 ),
 ( 0.02698595842317763963, 0.02784423243973405820, 0.02870250645629048025, 0.03041905448940328272, 0.03127732850595967007, 0.03213560252251606436, 0.03385215055562883907, 0.03471042457218519173, 0.03556869858874154439, 0.03728524662185422889, 0.03814352063841059542, 0.03900179465496696196, 0.03986006867152332850, 0.04071834268807969504, 0.04157661670463606157, 0.04243489072119242811, 0.04415143875430510567, 0.04500971277086143058, 0.04586798678741776936, 0.04758453482053040529, 0.04930108285364304122, 0.05101763088675567714, 0.05273417891986832001, 0.05445072695298095594 ),
 .UNSPECIFIED. ) ;
#2028 = LINE ( 'NONE', #13271, #49296 ) ;
#2029 = CARTESIAN_POINT ( 'NONE',  ( -0.9897066053608880587, 7.549089325901770842, -72.85837384025812469 ) ) ;
#2030 = VECTOR ( 'NONE', #4341, 1000.000000000000227 ) ;
#2031 = CARTESIAN_POINT ( 'NONE',  ( 50.03867889673313130, 42.05760816978183669, 41.38025477438755928 ) ) ;
#2032 = ORIENTED_EDGE ( 'NONE', *, *, #30523, .F. ) ;
#2033 = CARTESIAN_POINT ( 'NONE',  ( 163.6472217856825466, 63.92779681097861300, -93.03927632148491966 ) ) ;
#2034 = CARTESIAN_POINT ( 'NONE',  ( 197.2197025888162329, 96.62026035493822462, -44.48619938706712418 ) ) ;
#2035 = VECTOR ( 'NONE', #52358, 1000.000000000000000 ) ;
#2036 = CARTESIAN_POINT ( 'NONE',  ( -5.066666666666671759, 0.000000000000000000, -11.86666666666666536 ) ) ;
#2037 = DIRECTION ( 'NONE',  ( 1.000000000000000000, 0.000000000000000000, -0.000000000000000000 ) ) ;
#2038 = CIRCLE ( 'NONE', #53667, 25.00000000000000355 ) ;
#2040 = VERTEX_POINT ( 'NONE', #64870 ) ;
#2039 = DIRECTION ( 'NONE',  ( 1.000000000000000000, 0.000000000000000000, 0.000000000000000000 ) ) ;
#2041 = CARTESIAN_POINT ( 'NONE',  ( 63.01563776193091826, 12.67277567978498176, 29.81296093922127710 ) ) ;
#2042 = VERTEX_POINT ( 'NONE', #47293 ) ;
#2043 = ORIENTED_EDGE ( 'NONE', *, *, #42498, .F. ) ;
#2044 = AXIS2_PLACEMENT_3D ( 'NONE', #60547, #2852, #1819 ) ;
#2045 = CARTESIAN_POINT ( 'NONE',  ( -73.79615177260652104, 20.52570924097571492, -10.04630520512574599 ) ) ;
#2046 = DIRECTION ( 'NONE',  ( -1.000000000000000000, 0.000000000000000000, 0.000000000000000000 ) ) ;
#2048 = ORIENTED_EDGE ( 'NONE', *, *, #27631, .F. ) ;
#2047 = CARTESIAN_POINT ( 'NONE',  ( 0.000000000000000000, 190.0000000000000000, -2.000000000000000000 ) ) ;
#2049 = DIRECTION ( 'NONE',  ( 1.000000000000000000, 0.000000000000000000, 0.000000000000000000 ) ) ;
#2050 = LINE ( 'NONE', #45644, #44193 ) ;
#2051 = CARTESIAN_POINT ( 'NONE',  ( -74.39861643904069410, 21.81123504700007487, -36.44343603524747266 ) ) ;
#2052 = VERTEX_POINT ( 'NONE', #36760 ) ;
#2053 = EDGE_CURVE ( 'NONE', #43634, #38637, #20566, .T. ) ;
#2054 = CARTESIAN_POINT ( 'NONE',  ( 175.5371852679042775, 74.56478031408204288, -92.34861066285949960 ) ) ;
#2055 = EDGE_CURVE ( 'NONE', #23050, #32357, #4146, .T. ) ;
#2056 = CARTESIAN_POINT ( 'NONE',  ( 138.1901928158493433, 45.29454828899442731, 43.14961434377592298 ) ) ;
#2057 = CARTESIAN_POINT ( 'NONE',  ( -178.2448732545370831, 94.58403736950705820, 43.81829304766783650 ) ) ;
#2058 = CARTESIAN_POINT ( 'NONE',  ( 132.0249343950657135, 41.49728247212333088, 71.18673643823439079 ) ) ;
#2059 = CARTESIAN_POINT ( 'NONE',  ( 19.11382977197791533, 7.636807742668411336, 71.09960622632753768 ) ) ;
#2060 = VERTEX_POINT ( 'NONE', #27925 ) ;
#2061 = ORIENTED_EDGE ( 'NONE', *, *, #33182, .T. ) ;
#2062 = ORIENTED_EDGE ( 'NONE', *, *, #21925, .T. ) ;
#2063 = CARTESIAN_POINT ( 'NONE',  ( 109.9975424824652634, 18.08738615523480675, 402.4289050101931480 ) ) ;
#2064 = CARTESIAN_POINT ( 'NONE',  ( -59.94154301275570162, 45.09516516490385385, 43.58025477438756212 ) ) ;
#2065 = CARTESIAN_POINT ( 'NONE',  ( 78.57571471437144339, 0.000000000000000000, -30.00000000000000355 ) ) ;
#2066 = CARTESIAN_POINT ( 'NONE',  ( -94.85325982401134581, 29.16540057079190262, 92.80390509532465160 ) ) ;
#2067 = CARTESIAN_POINT ( 'NONE',  ( -142.0251973982164770, 58.08401473564112649, 37.63374177329165349 ) ) ;
#2068 = ADVANCED_FACE ( 'NONE', ( #27572 ), #28452, .T. ) ;
#2069 = CARTESIAN_POINT ( 'NONE',  ( 0.000000000000000000, 0.000000000000000000, 8.000000000000000000 ) ) ;
#2070 = CARTESIAN_POINT ( 'NONE',  ( -78.19438069111006939, 23.21811806230638098, -23.27090004125422240 ) ) ;
#2071 = ORIENTED_EDGE ( 'NONE', *, *, #14595, .T. ) ;
#2072 = CARTESIAN_POINT ( 'NONE',  ( 82.94943325692331371, 18.19803534719805782, 57.51694778251922457 ) ) ;
#2073 = EDGE_CURVE ( 'NONE', #52786, #23236, #40804, .T. ) ;
#2074 = VERTEX_POINT ( 'NONE', #55348 ) ;
#2075 = VECTOR ( 'NONE', #8776, 1000.000000000000227 ) ;
#2076 = CARTESIAN_POINT ( 'NONE',  ( 31.99894129856763314, 7.561773404408285160, 36.18667756713777806 ) ) ;
#2077 = DIRECTION ( 'NONE',  ( -0.000000000000000000, -0.000000000000000000, -1.000000000000000000 ) ) ;
#2078 = VERTEX_POINT ( 'NONE', #44452 ) ;
#2079 = CARTESIAN_POINT ( 'NONE',  ( 0.000000000000000000, 70.00000000000000000, 0.000000000000000000 ) ) ;
#2080 = DIRECTION ( 'NONE',  ( -1.000000000000000000, 0.000000000000000000, 0.000000000000000000 ) ) ;
#2081 = VECTOR ( 'NONE', #29184, 1000.000000000000114 ) ;
#2082 = DIRECTION ( 'NONE',  ( -0.9009688679024155933, -0.4338837391175656699, 0.000000000000000000 ) ) ;
#2083 = DIRECTION ( 'NONE',  ( -0.000000000000000000, 1.000000000000000000, -0.000000000000000000 ) ) ;
#2084 = EDGE_CURVE ( 'NONE', #40853, #60572, #12105, .T. ) ;
#2085 = CARTESIAN_POINT ( 'NONE',  ( 73.79471914489741380, -13.39176710989671726, 0.000000000000000000 ) ) ;
#2086 = CIRCLE ( 'NONE', #66164, 246.3582898394606957 ) ;
#2087 = CARTESIAN_POINT ( 'NONE',  ( 162.0862735437574713, 62.63196145447158614, -76.39940893092133933 ) ) ;
#2088 = ORIENTED_EDGE ( 'NONE', *, *, #49767, .F. ) ;
#2089 = B_SPLINE_CURVE_WITH_KNOTS ( 'NONE', 3,
 ( #49248, #16899, #65454, #54881, #66511, #60164, #1081, #44328, #22533, #28149, #66172, #18303, #28511, #39761, #1792, #17962, #54171, #11272, #39411, #12682, #65815, #34148, #11983, #55584, #28869, #17609, #38718, #5993, #22885, #39075, #43972, #22187, #17248, #33454, #50320, #735, #49596, #2138, #1428, #48892, #32741, #43627, #38360, #59805 ),
 .UNSPECIFIED., .F., .F.,
 ( 4, 2, 2, 2, 2, 2, 2, 2, 2, 2, 2, 2, 2, 2, 2, 2, 2, 2, 2, 2, 2, 4 ),
 ( 0.02908143158676660886, 0.03095422299093871649, 0.03282701439511082064, 0.03469980579928292480, 0.03657259720345503590, 0.03844538860762714005, 0.04031818001179924421, 0.04125457571388527200, 0.04219097141597129980, 0.04312736711805732759, 0.04359556496910033108, 0.04406376282014333456, 0.04500015852222933460, 0.04593655422431534852, 0.04687294992640135549, 0.04780934562848735553, 0.04968213703265940417, 0.05155492843683144588, 0.05342771984100349453, 0.05530051124517554317, 0.05717330264934758488, 0.05904609405351963353 ),
 .UNSPECIFIED. ) ;
#2090 = PLANE ( 'NONE',  #24134 ) ;
#2091 = CARTESIAN_POINT ( 'NONE',  ( 15.78827728214693416, 6.500811158483322139, -89.20804527961313113 ) ) ;
#2092 = ORIENTED_EDGE ( 'NONE', *, *, #5568, .T. ) ;
#2093 = CARTESIAN_POINT ( 'NONE',  ( 4.000000000000011546, -6.928203230275505220, -9.500000000000000000 ) ) ;
#2094 = LINE ( 'NONE', #44643, #47644 ) ;
#2095 = DIRECTION ( 'NONE',  ( 0.000000000000000000, 0.000000000000000000, 1.000000000000000000 ) ) ;
#2096 = ORIENTED_EDGE ( 'NONE', *, *, #47172, .F. ) ;
#2097 = DIRECTION ( 'NONE',  ( -1.000000000000000000, 0.000000000000000000, 0.000000000000000000 ) ) ;
#2098 = CARTESIAN_POINT ( 'NONE',  ( 151.8005253678162489, 54.62151558044536159, -75.40480181429586537 ) ) ;
#2099 = CARTESIAN_POINT ( 'NONE',  ( -34.74312654625183683, 10.15703162223800859, 30.97899339878855329 ) ) ;
#2100 = CARTESIAN_POINT ( 'NONE',  ( 141.0804878838241336, 45.96076546397620888, -41.43773930307789044 ) ) ;
#2101 = EDGE_CURVE ( 'NONE', #34582, #25022, #49713, .T. ) ;
#2102 = ORIENTED_EDGE ( 'NONE', *, *, #62336, .T. ) ;
#2103 = EDGE_CURVE ( 'NONE', #5375, #39717, #50083, .T. ) ;
#2104 = EDGE_CURVE ( 'NONE', #69562, #64513, #40275, .T. ) ;
#2105 = ADVANCED_FACE ( 'NONE', ( #14188 ), #35648, .F. ) ;
#2106 = DIRECTION ( 'NONE',  ( 0.000000000000000000, -1.000000000000000000, 0.000000000000000000 ) ) ;
#2107 = ORIENTED_EDGE ( 'NONE', *, *, #62169, .F. ) ;
#2108 = CARTESIAN_POINT ( 'NONE',  ( 424.8372781065087906, 400.0000000000067075, -123.9497041420121235 ) ) ;
#2109 = DIRECTION ( 'NONE',  ( 1.000000000000000000, -0.000000000000000000, 0.000000000000000000 ) ) ;
#2110 = CARTESIAN_POINT ( 'NONE',  ( 15.68296563925591514, -63.09411298019745828, 170.0000000000000000 ) ) ;
#2111 = CARTESIAN_POINT ( 'NONE',  ( 140.6568134119880824, 46.88581307642903795, 87.51626415052055563 ) ) ;
#2112 = CARTESIAN_POINT ( 'NONE',  ( -25.64812644094277871, 9.728246071458697131, -91.73551276297135360 ) ) ;
#2113 = DIRECTION ( 'NONE',  ( -0.000000000000000000, -0.000000000000000000, -1.000000000000000000 ) ) ;
#2114 = ORIENTED_EDGE ( 'NONE', *, *, #3365, .T. ) ;
#2115 = CARTESIAN_POINT ( 'NONE',  ( 109.9975424824652634, 296.0000000000000000, 529.9060149868646477 ) ) ;
#2116 = DIRECTION ( 'NONE',  ( 1.000000000000000000, 0.000000000000000000, 0.000000000000000000 ) ) ;
#2117 = DIRECTION ( 'NONE',  ( 0.4338837391175656699, -0.9009688679024155933, 2.500042656554809847E-16 ) ) ;
#2118 = CARTESIAN_POINT ( 'NONE',  ( 34.76618902119740540, 54.93755186520760958, 170.0000000000000000 ) ) ;
#2119 = CARTESIAN_POINT ( 'NONE',  ( 309.8720357909272707, 172.0000000000000284, 536.6193948016162949 ) ) ;
#2120 = VERTEX_POINT ( 'NONE', #13833 ) ;
#2121 = CARTESIAN_POINT ( 'NONE',  ( 163.1313205310725039, 63.49733392291058465, -11.85377922317074528 ) ) ;
#2122 = CARTESIAN_POINT ( 'NONE',  ( 8.670103207226933506, 6.377073801252349128, 35.10160029233258427 ) ) ;
#2123 = EDGE_LOOP ( 'NONE', ( #65423, #20110, #20744, #32328 ) ) ;
#2124 = CARTESIAN_POINT ( 'NONE',  ( 65.62985354949972816, 14.32996029952553485, 71.19137513351442692 ) ) ;
#2125 = CARTESIAN_POINT ( 'NONE',  ( 126.9829467593605301, 37.42601351122073083, -94.18273480071589177 ) ) ;
#2126 = VECTOR ( 'NONE', #628, 1000.000000000000000 ) ;
#2127 = ORIENTED_EDGE ( 'NONE', *, *, #52497, .F. ) ;
#2128 = CARTESIAN_POINT ( 'NONE',  ( 163.1370549780984049, 63.50181104276887822, -48.56306423650217852 ) ) ;
#2129 = DIRECTION ( 'NONE',  ( 0.000000000000000000, 0.000000000000000000, -1.000000000000000000 ) ) ;
#2130 =( GEOMETRIC_REPRESENTATION_CONTEXT ( 3 ) GLOBAL_UNCERTAINTY_ASSIGNED_CONTEXT ( ( #8581 ) ) GLOBAL_UNIT_ASSIGNED_CONTEXT ( ( #28794, #2407, #61144 ) ) REPRESENTATION_CONTEXT ( 'NONE', 'WORKASPACE' ) );
#2131 = CARTESIAN_POINT ( 'NONE',  ( 159.6725804802005939, 59.38339663535511193, -36.44073469567691603 ) ) ;
#2132 = ORIENTED_EDGE ( 'NONE', *, *, #52864, .T. ) ;
#2133 = CARTESIAN_POINT ( 'NONE',  ( -95.20053778133910782, 30.43887292928076604, 8.646733277597450140 ) ) ;
#2134 = B_SPLINE_CURVE_WITH_KNOTS ( 'NONE', 3,
 ( #66414, #27348, #48787, #982, #60415, #22430, #38609, #60051, #11873, #46657, #40001, #40683, #24535, #68134, #61458, #14315, #29796, #9038, #29442, #50904, #8350, #45971, #61793, #35774, #18548, #8698, #35420, #13614, #67436, #19581, #30485, #56520, #66755, #57223, #50556, #35070, #45274, #51935, #13281, #41040, #30153, #3751, #62142, #51262, #67784, #2374, #23832, #25223 ),
 .UNSPECIFIED., .F., .F.,
 ( 4, 2, 2, 2, 2, 2, 2, 2, 2, 2, 2, 2, 2, 2, 2, 2, 2, 2, 2, 2, 2, 2, 2, 4 ),
 ( 0.02698595842317764310, 0.02784423243973403739, 0.02870250645629042821, 0.03041905448940312312, 0.03127732850595946884, 0.03213560252251581456, 0.03385215055562851294, 0.03471042457218486560, 0.03556869858874121132, 0.03728524662185391664, 0.03814352063841026236, 0.03900179465496660114, 0.03986006867152294686, 0.04071834268807929258, 0.04157661670463563830, 0.04243489072119198402, 0.04415143875430466158, 0.04500971277086100730, 0.04586798678741735302, 0.04758453482053006528, 0.04930108285364277754, 0.05101763088675548286, 0.05273417891986818817, 0.05445072695298090043 ),
 .UNSPECIFIED. ) ;
#2135 = DIRECTION ( 'NONE',  ( 0.000000000000000000, 0.000000000000000000, 1.000000000000000000 ) ) ;
#2136 = ADVANCED_FACE ( 'NONE', ( #46888 ), #35297, .F. ) ;
#2137 = CARTESIAN_POINT ( 'NONE',  ( 31.95163392065794739, 8.568192436298495807, 36.42221770829554117 ) ) ;
#2138 = CARTESIAN_POINT ( 'NONE',  ( -176.3856149167966407, 92.38076834121984859, -35.44546595752847651 ) ) ;
#2139 = CARTESIAN_POINT ( 'NONE',  ( -44.29440389294402536, -17.09499999999999886, 0.000000000000000000 ) ) ;
#2140 = CARTESIAN_POINT ( 'NONE',  ( 152.8558173410469294, 54.14978343559392471, 69.68634218349458820 ) ) ;
#2141 = CARTESIAN_POINT ( 'NONE',  ( 128.4224537826253822, 38.23837035195744960, -65.17599223679393106 ) ) ;
#2142 = ORIENTED_EDGE ( 'NONE', *, *, #4964, .F. ) ;
#2143 = CARTESIAN_POINT ( 'NONE',  ( 140.4769819293526893, 46.76840769395180786, -73.90161371371723931 ) ) ;
#2144 = LINE ( 'NONE', #35537, #4043 ) ;
#2145 = EDGE_LOOP ( 'NONE', ( #5278, #8405, #51535 ) ) ;
#2146 = CARTESIAN_POINT ( 'NONE',  ( -154.7826623253029936, 70.14150242829518334, -47.64975679370859751 ) ) ;
#2147 = CARTESIAN_POINT ( 'NONE',  ( -442.6627218934916641, 394.9999999999954525, 103.5502958579924808 ) ) ;
#2148 = CARTESIAN_POINT ( 'NONE',  ( -33.38294402636582703, 10.93918551420889607, 44.97681826711176001 ) ) ;
#2149 = CARTESIAN_POINT ( 'NONE',  ( -167.9889421625799741, 81.59140042431236850, -47.70137618540091040 ) ) ;
#2150 = CARTESIAN_POINT ( 'NONE',  ( 19.62566184736079578, 15.48655536434876900, 0.000000000000000000 ) ) ;
#2151 = FACE_OUTER_BOUND ( 'NONE', #2415, .T. ) ;
#2152 = CARTESIAN_POINT ( 'NONE',  ( -48.57297291660697880, 13.03920345822339044, -73.36987217233711078 ) ) ;
#2153 = ADVANCED_FACE ( 'NONE', ( #50772 ), #39873, .F. ) ;
#2154 = CARTESIAN_POINT ( 'NONE',  ( 208.5889601154909201, 111.8333159387241835, -50.25120141670069529 ) ) ;
#2155 = EDGE_CURVE ( 'NONE', #64382, #37468, #14528, .T. ) ;
#2156 = PLANE ( 'NONE',  #68079 ) ;
#2158 = ADVANCED_FACE ( 'NONE', ( #31404 ), #64092, .F. ) ;
#2157 = CARTESIAN_POINT ( 'NONE',  ( 164.9559213734325169, 63.71338633026442722, 10.60842315000168234 ) ) ;
#2159 = ORIENTED_EDGE ( 'NONE', *, *, #27779, .F. ) ;
#2160 = CARTESIAN_POINT ( 'NONE',  ( -95.21085197937820510, 30.44372064875429373, -39.95763492157845320 ) ) ;
#2161 = ORIENTED_EDGE ( 'NONE', *, *, #63382, .T. ) ;
#2162 = LINE ( 'NONE', #13743, #57665 ) ;
#2163 = EDGE_CURVE ( 'NONE', #30662, #53211, #9601, .T. ) ;
#2164 = CARTESIAN_POINT ( 'NONE',  ( 0.000000000000000000, 0.000000000000000000, -5.000000000000000888 ) ) ;
#2165 = CARTESIAN_POINT ( 'NONE',  ( 45.34143264614439772, 9.256465810451185661, 59.67216321036798377 ) ) ;
#2166 = CARTESIAN_POINT ( 'NONE',  ( -12.50000000000002842, 207.5000000000000284, 378.0000000000000000 ) ) ;
#2167 = DIRECTION ( 'NONE',  ( 0.000000000000000000, 0.000000000000000000, 1.000000000000000000 ) ) ;
#2168 = LINE ( 'NONE', #45410, #29903 ) ;
#2169 = DIRECTION ( 'NONE',  ( -0.7071067811865474617, -0.000000000000000000, -0.7071067811865474617 ) ) ;
#2170 = FACE_BOUND ( 'NONE', #11561, .T. ) ;
#2171 = VERTEX_POINT ( 'NONE', #48575 ) ;
#2172 = EDGE_LOOP ( 'NONE', ( #17537, #12775, #56513, #41341 ) ) ;
#2173 = CARTESIAN_POINT ( 'NONE',  ( 63.01563776193091826, -170.0000000000000000, 64.15751152968499582 ) ) ;
#2174 = CARTESIAN_POINT ( 'NONE',  ( 173.5837434292114096, 71.34409607026155697, 63.36509229591028003 ) ) ;
#2175 = LINE ( 'NONE', #18695, #68256 ) ;
#2176 = CARTESIAN_POINT ( 'NONE',  ( 108.3753929817421096, 29.13179266688723956, 71.23489859707926541 ) ) ;
#2177 = CARTESIAN_POINT ( 'NONE',  ( -167.6524579626395166, 82.69702609844094354, -20.50584711148702510 ) ) ;
#2178 = AXIS2_PLACEMENT_3D ( 'NONE', #46569, #25483, #26158 ) ;
#2179 = DIRECTION ( 'NONE',  ( 0.000000000000000000, 0.000000000000000000, -1.000000000000000000 ) ) ;
#2180 = ORIENTED_EDGE ( 'NONE', *, *, #21990, .T. ) ;
#2181 = ADVANCED_FACE ( 'NONE', ( #53171 ), #4657, .F. ) ;
#2182 = EDGE_CURVE ( 'NONE', #46584, #55490, #14866, .T. ) ;
#2183 =( GEOMETRIC_REPRESENTATION_CONTEXT ( 3 ) GLOBAL_UNCERTAINTY_ASSIGNED_CONTEXT ( ( #2954 ) ) GLOBAL_UNIT_ASSIGNED_CONTEXT ( ( #13188, #10650, #95 ) ) REPRESENTATION_CONTEXT ( 'NONE', 'WORKASPACE' ) );
#2184 = CARTESIAN_POINT ( 'NONE',  ( 104.7227067006896561, 27.50728936118535373, -48.52285352452530276 ) ) ;
#2185 = CARTESIAN_POINT ( 'NONE',  ( -8.314575874103551811, 6.922894809783093351, 56.96013162991087597 ) ) ;
#2186 = CARTESIAN_POINT ( 'NONE',  ( -86.06489347855099936, 25.27905598459107139, -17.02718089029554704 ) ) ;
#2187 = DIRECTION ( 'NONE',  ( -1.000000000000000000, 0.000000000000000000, 0.000000000000000000 ) ) ;
#2188 = DIRECTION ( 'NONE',  ( -1.000000000000000000, 0.000000000000000000, 0.000000000000000000 ) ) ;
#2189 = FACE_BOUND ( 'NONE', #62448, .T. ) ;
#2190 = EDGE_CURVE ( 'NONE', #41640, #36722, #58803, .T. ) ;
#2191 = ORIENTED_EDGE ( 'NONE', *, *, #45440, .F. ) ;
#2192 = DIRECTION ( 'NONE',  ( -1.000000000000000000, 0.000000000000000000, 0.000000000000000000 ) ) ;
#2193 = DIRECTION ( 'NONE',  ( -0.000000000000000000, -0.000000000000000000, 1.000000000000000000 ) ) ;
#2194 = CARTESIAN_POINT ( 'NONE',  ( 0.000000000000000000, 0.000000000000000000, 133.5802547743875550 ) ) ;
#2195 = DIRECTION ( 'NONE',  ( 0.000000000000000000, 0.000000000000000000, 1.000000000000000000 ) ) ;
#2196 = CARTESIAN_POINT ( 'NONE',  ( 207.4610690199662031, 111.9701171077052066, 70.53645963308595412 ) ) ;
#2197 = AXIS2_PLACEMENT_3D ( 'NONE', #57678, #3864, #3179 ) ;
#2198 = CARTESIAN_POINT ( 'NONE',  ( 82.34195123877069022, 18.00239921638039675, -64.00762485161624227 ) ) ;
#2199 = ORIENTED_EDGE ( 'NONE', *, *, #61849, .F. ) ;
#2200 = CARTESIAN_POINT ( 'NONE',  ( 0.000000000000000000, 0.000000000000000000, 0.000000000000000000 ) ) ;
#2201 = CARTESIAN_POINT ( 'NONE',  ( -4.680456609903988152, -6.535341423375606418, -9.483111142572225205 ) ) ;
#2202 = ORIENTED_EDGE ( 'NONE', *, *, #5625, .T. ) ;
#2203 = DIRECTION ( 'NONE',  ( 0.000000000000000000, -0.000000000000000000, 1.000000000000000000 ) ) ;
#2204 = VERTEX_POINT ( 'NONE', #69369 ) ;
#2205 = CARTESIAN_POINT ( 'NONE',  ( -83.51052366780672287, 24.22613130369187218, -63.72902832609224077 ) ) ;
#2206 = CARTESIAN_POINT ( 'NONE',  ( -56.96436614829622158, 16.24647150911285465, -23.12810583680024479 ) ) ;
#2207 = DIRECTION ( 'NONE',  ( 0.000000000000000000, 0.000000000000000000, 1.000000000000000000 ) ) ;
#2208 = APPLICATION_CONTEXT ( 'automotive_design' ) ;
#2209 = ORIENTED_EDGE ( 'NONE', *, *, #12961, .T. ) ;
#2210 = VERTEX_POINT ( 'NONE', #64435 ) ;
#2211 = CARTESIAN_POINT ( 'NONE',  ( 45.76405797021009647, 10.34101216371941945, 68.23763830739490288 ) ) ;
#2212 = AXIS2_PLACEMENT_3D ( 'NONE', #15468, #36921, #58360 ) ;
#2213 = LINE ( 'NONE', #32821, #63921 ) ;
#2214 = CARTESIAN_POINT ( 'NONE',  ( -156.7435307435793845, 71.93726016406964163, -71.14971855428032654 ) ) ;
#2215 = CARTESIAN_POINT ( 'NONE',  ( 66.73467315386238852, 14.60276727483218728, 16.99948571587159307 ) ) ;
#2216 = ORIENTED_EDGE ( 'NONE', *, *, #20941, .T. ) ;
#2217 = PRESENTATION_STYLE_ASSIGNMENT (( #34229 ) ) ;
#2218 = ADVANCED_FACE ( 'NONE', ( #5683 ), #9947, .F. ) ;
#2219 = CARTESIAN_POINT ( 'NONE',  ( -47.80251179448168131, 13.89045662648309154, 12.95678486719901912 ) ) ;
#2220 = CARTESIAN_POINT ( 'NONE',  ( -130.5904357464317513, 50.88938808445628581, -9.701552378028926782 ) ) ;
#2221 = CARTESIAN_POINT ( 'NONE',  ( -154.4602569667544856, 69.84957963938288117, -90.35317075896763583 ) ) ;
#2222 = CARTESIAN_POINT ( 'NONE',  ( 116.0773578185793724, 31.67580513411751753, -21.31700010224128050 ) ) ;
#2223 = B_SPLINE_CURVE_WITH_KNOTS ( 'NONE', 3,
 ( #69474, #64199, #16008, #53634, #43772, #37124, #17039, #58566, #49042, #31852, #69122, #53285, #37459, #883, #11773, #11074, #21631, #58916, #27251, #43078, #5458, #48340, #10731, #48011, #16360, #59262, #20950, #48686, #530, #43426, #64904, #38508, #38156, #59595, #11415, #59953, #34293, #1227, #38872, #60315, #6849, #12481, #18454 ),
 .UNSPECIFIED., .F., .F.,
 ( 4, 2, 2, 2, 2, 2, 2, 2, 2, 2, 2, 2, 1, 2, 2, 2, 2, 2, 2, 2, 2, 4 ),
 ( 0.02379577142314830487, 0.02527778373276535345, 0.02601878988757387254, 0.02675979604238239162, 0.02824180835199942979, 0.02972382066161646449, 0.03046482681642496276, 0.03120583297123346103, 0.03268784528085046104, 0.03416985759046747145, 0.03565186990008447493, 0.03639287605489297667, 0.03713388220970148534, 0.03787488836450998708, 0.03861589451931848882, 0.04009790682893545760, 0.04157991913855242638, 0.04306193144816939516, 0.04380293760297787609, 0.04454394375778636395, 0.04602595606740334661, 0.04750796837702032926 ),
 .UNSPECIFIED. ) ;
#2224 = VECTOR ( 'NONE', #64142, 1000.000000000000000 ) ;
#2225 = CARTESIAN_POINT ( 'NONE',  ( 85.37210774275131087, 18.99570166535387727, 83.50014660744342621 ) ) ;
#2227 = VERTEX_POINT ( 'NONE', #53524 ) ;
#2226 = CARTESIAN_POINT ( 'NONE',  ( -180.5668408223793904, -170.0000000000000000, -95.00000000000133582 ) ) ;
#2228 = ORIENTED_EDGE ( 'NONE', *, *, #33111, .F. ) ;
#2229 = AXIS2_PLACEMENT_3D ( 'NONE', #66577, #8161, #56011 ) ;
#2230 = ORIENTED_EDGE ( 'NONE', *, *, #34718, .T. ) ;
#2231 = DIRECTION ( 'NONE',  ( 0.000000000000000000, -1.000000000000000000, 0.000000000000000000 ) ) ;
#2232 = CARTESIAN_POINT ( 'NONE',  ( 181.0840389613909736, 80.03940679743416808, 2.464043515047717570 ) ) ;
#2233 = CARTESIAN_POINT ( 'NONE',  ( -132.6811329440527061, -170.0000000000000000, 94.99999999999866418 ) ) ;
#2234 = CARTESIAN_POINT ( 'NONE',  ( 105.4375968828853729, 26.72149058755202944, -10.81446374568332125 ) ) ;
#2235 = CARTESIAN_POINT ( 'NONE',  ( 197.2197025888162045, 96.62026035493816778, 9.202901793860229773 ) ) ;
#2236 = EDGE_CURVE ( 'NONE', #53211, #61781, #59915, .T. ) ;
#2237 = CARTESIAN_POINT ( 'NONE',  ( 202.3256005306661223, 104.8219372317010141, 83.25897611976662915 ) ) ;
#2238 = DIRECTION ( 'NONE',  ( -0.000000000000000000, -0.000000000000000000, 1.000000000000000000 ) ) ;
#2239 = CARTESIAN_POINT ( 'NONE',  ( -72.78737098446268305, 20.16853011470087864, -74.14376160244967195 ) ) ;
#2240 = CARTESIAN_POINT ( 'NONE',  ( -14.92903005859421128, 7.458185427130750611, 40.03400615406091134 ) ) ;
#2241 = ORIENTED_EDGE ( 'NONE', *, *, #35604, .T. ) ;
#2242 = CARTESIAN_POINT ( 'NONE',  ( 12.68603346975295132, 7.427591953486040843, -9.341698521599035132 ) ) ;
#2243 = VERTEX_POINT ( 'NONE', #47217 ) ;
#2244 = ADVANCED_FACE ( 'NONE', ( #10616 ), #59149, .F. ) ;
#2245 = ORIENTED_EDGE ( 'NONE', *, *, #24861, .F. ) ;
#2246 = EDGE_CURVE ( 'NONE', #31208, #26272, #51977, .T. ) ;
#2247 = CARTESIAN_POINT ( 'NONE',  ( 66.30230369578302430, 14.49551544185123753, -23.12206507395049826 ) ) ;
#2248 = CARTESIAN_POINT ( 'NONE',  ( 186.0827296088606886, 85.28826835108064586, -64.97338836740433976 ) ) ;
#2249 = CARTESIAN_POINT ( 'NONE',  ( -37.70624945308918541, 11.72883674540529242, 87.27307330636284632 ) ) ;
#2250 = AXIS2_PLACEMENT_3D ( 'NONE', #44344, #38734, #56292 ) ;
#2251 = DIRECTION ( 'NONE',  ( 0.000000000000000000, 0.9989683093773507050, 0.04541273895899305274 ) ) ;
#2252 = EDGE_CURVE ( 'NONE', #18701, #68876, #20486, .T. ) ;
#2253 = DIRECTION ( 'NONE',  ( 0.000000000000000000, 0.000000000000000000, -1.000000000000000000 ) ) ;
#2254 = LINE ( 'NONE', #24051, #2264 ) ;
#2255 = CARTESIAN_POINT ( 'NONE',  ( 139.1306635769909690, 45.89653412152168244, -22.01677782650911652 ) ) ;
#2256 = EDGE_LOOP ( 'NONE', ( #42855, #11599, #67261, #3883 ) ) ;
#2257 = ORIENTED_EDGE ( 'NONE', *, *, #26764, .T. ) ;
#2258 = PLANE ( 'NONE',  #31609 ) ;
#2259 = CARTESIAN_POINT ( 'NONE',  ( -14.94265033805045562, 7.459411036484909552, 8.355115657452357070 ) ) ;
#2260 = DIRECTION ( 'NONE',  ( 0.000000000000000000, 1.000000000000000000, 0.000000000000000000 ) ) ;
#2261 = DIRECTION ( 'NONE',  ( -0.7071067811865483499, 8.659560562354925463E-17, -0.7071067811865467956 ) ) ;
#2262 = UNCERTAINTY_MEASURE_WITH_UNIT (LENGTH_MEASURE( 1.000000000000000082E-05 ), #25461, 'distance_accuracy_value', 'NONE');
#2263 = CARTESIAN_POINT ( 'NONE',  ( -188.6739852773920347, 108.2139733222100517, 40.12819175787510062 ) ) ;
#2264 = VECTOR ( 'NONE', #28628, 1000.000000000000000 ) ;
#2265 = CARTESIAN_POINT ( 'NONE',  ( -46.66904755831212981, -15.55634918610397222, 0.000000000000000000 ) ) ;
#2266 = ORIENTED_EDGE ( 'NONE', *, *, #53514, .T. ) ;
#2267 = CARTESIAN_POINT ( 'NONE',  ( -102.2801239173131194, -170.0000000000000000, 64.86362509687882039 ) ) ;
#2268 = CARTESIAN_POINT ( 'NONE',  ( -61.77164219855452387, 17.63686644795249236, -66.19097850481081480 ) ) ;
#2269 = CARTESIAN_POINT ( 'NONE',  ( 199.2049631873263138, 100.7347227143600037, -65.55741041441223160 ) ) ;
#2270 = DIRECTION ( 'NONE',  ( 1.000000000000000000, 2.261926634819711547E-29, -9.860761315262647568E-31 ) ) ;
#2271 = FACE_OUTER_BOUND ( 'NONE', #44764, .T. ) ;
#2272 = DIRECTION ( 'NONE',  ( 0.000000000000000000, 0.000000000000000000, 1.000000000000000000 ) ) ;
#2273 = LINE ( 'NONE', #23023, #26383 ) ;
#2274 = CARTESIAN_POINT ( 'NONE',  ( 0.000000000000000000, 0.000000000000000000, 0.000000000000000000 ) ) ;
#2276 = EDGE_CURVE ( 'NONE', #17473, #12095, #34441, .T. ) ;
#2275 = FACE_BOUND ( 'NONE', #51080, .T. ) ;
#2277 = DIRECTION ( 'NONE',  ( -1.000000000000000000, 0.000000000000000000, 0.000000000000000000 ) ) ;
#2278 = CARTESIAN_POINT ( 'NONE',  ( -4.725257700476002576, 6.708862164351558910, 71.29377542245961763 ) ) ;
#2279 = ORIENTED_EDGE ( 'NONE', *, *, #15630, .F. ) ;
#2280 = CARTESIAN_POINT ( 'NONE',  ( 278.3860478234813058, 21.48288568141374455, -4.743631494308814034 ) ) ;
#2281 = CARTESIAN_POINT ( 'NONE',  ( -125.8938041572051105, 46.49392987655492959, -76.75825448869764500 ) ) ;
#2282 = CARTESIAN_POINT ( 'NONE',  ( 183.2136430849847955, 6.000000000000000000, -41.68900338898720292 ) ) ;
#2283 = CARTESIAN_POINT ( 'NONE',  ( 0.000000000000000000, 0.000000000000000000, -9.474599999999998801 ) ) ;
#2284 = AXIS2_PLACEMENT_3D ( 'NONE', #40684, #4107, #3755 ) ;
#2285 = DIRECTION ( 'NONE',  ( 0.5407162030609372616, -0.6444004775717706579, -0.5407162030609374836 ) ) ;
#2286 = VERTEX_POINT ( 'NONE', #66207 ) ;
#2287 = CARTESIAN_POINT ( 'NONE',  ( -190.6985136298601731, 109.1272424661242582, 7.126870892829554549 ) ) ;
#2288 = DIRECTION ( 'NONE',  ( -0.000000000000000000, 0.000000000000000000, 1.000000000000000000 ) ) ;
#2289 = EDGE_LOOP ( 'NONE', ( #44687, #20070, #18258, #6680 ) ) ;
#2290 = ORIENTED_EDGE ( 'NONE', *, *, #17551, .F. ) ;
#2291 = PLANE ( 'NONE',  #63395 ) ;
#2292 = CARTESIAN_POINT ( 'NONE',  ( 154.0281735872262061, 56.28213428456460576, 43.57687635770160739 ) ) ;
#2293 = CARTESIAN_POINT ( 'NONE',  ( 427.4999999999999432, 207.5000000000000284, 0.000000000000000000 ) ) ;
#2294 = VERTEX_POINT ( 'NONE', #16593 ) ;
#2295 = DIRECTION ( 'NONE',  ( -1.000000000000000000, 0.000000000000000000, 0.000000000000000000 ) ) ;
#2296 = CARTESIAN_POINT ( 'NONE',  ( 445.3372781065086201, 177.8591479523844612, 78.55029585798806124 ) ) ;
#2297 = CARTESIAN_POINT ( 'NONE',  ( 44.99999999999995737, -25.00000000000000000, 1.999999999999984457 ) ) ;
#2298 = AXIS2_PLACEMENT_3D ( 'NONE', #8382, #19975, #61496 ) ;
#2299 = CARTESIAN_POINT ( 'NONE',  ( 259.4165763529819060, 225.8585178651493948, 138.9999999999999716 ) ) ;
#2300 = CARTESIAN_POINT ( 'NONE',  ( 87.11228333101213650, 19.58587579906928511, -35.82156419891172305 ) ) ;
#2301 = CARTESIAN_POINT ( 'NONE',  ( 141.2470358420065395, 46.06959063280891797, 11.47092469016289407 ) ) ;
#2302 = EDGE_CURVE ( 'NONE', #1174, #36237, #24878, .T. ) ;
#2303 = EDGE_CURVE ( 'NONE', #6058, #28877, #22222, .T. ) ;
#2304 = VERTEX_POINT ( 'NONE', #12717 ) ;
#2305 = CARTESIAN_POINT ( 'NONE',  ( 113.8748103246145007, 30.59837980920002209, -36.84266853766591510 ) ) ;
#2306 = EDGE_CURVE ( 'NONE', #4870, #42101, #55269, .T. ) ;
#2307 = CARTESIAN_POINT ( 'NONE',  ( -77.71801202538874520, 23.03755222122951452, 18.52846565512617971 ) ) ;
#2308 = CARTESIAN_POINT ( 'NONE',  ( 40.38414441725700499, 8.538832720399529563, -35.66810678251472666 ) ) ;
#2309 = DIRECTION ( 'NONE',  ( 0.4738686624729966379, 0.8805955318567391110, 0.000000000000000000 ) ) ;
#2311 = ORIENTED_EDGE ( 'NONE', *, *, #31125, .T. ) ;
#2310 = CARTESIAN_POINT ( 'NONE',  ( -119.1443287577880739, 42.20738984040679043, 88.47138527478010417 ) ) ;
#2312 = CARTESIAN_POINT ( 'NONE',  ( 79.19345177405118363, 17.01649702043280143, -42.31098989147414358 ) ) ;
#2313 = CIRCLE ( 'NONE', #61839, 21.99999999999998579 ) ;
#2314 = ORIENTED_EDGE ( 'NONE', *, *, #36138, .T. ) ;
#2315 = CARTESIAN_POINT ( 'NONE',  ( -146.5268141329886191, 61.69196909035591148, 71.95141080427552538 ) ) ;
#2316 = CARTESIAN_POINT ( 'NONE',  ( 83.38619203015943526, 19.39783821526630447, 30.43258577136558074 ) ) ;
#2317 = CARTESIAN_POINT ( 'NONE',  ( 14.99999999999997158, 0.000000000000000000, -0.000000000000000000 ) ) ;
#2318 = CARTESIAN_POINT ( 'NONE',  ( 188.4389256074244372, 86.37278721358589451, -15.38304180145345867 ) ) ;
#2319 = CARTESIAN_POINT ( 'NONE',  ( 139.2921620648436942, 44.80435067172500396, -21.86958038675194871 ) ) ;
#2320 = CARTESIAN_POINT ( 'NONE',  ( 39.40195752203892710, 9.424259417798131366, 3.069283715499574239 ) ) ;
#2321 = CARTESIAN_POINT ( 'NONE',  ( 16.62903674119167263, 7.535646975941353354, -89.24366362108607120 ) ) ;
#2322 = FACE_OUTER_BOUND ( 'NONE', #39212, .T. ) ;
#2323 = ORIENTED_EDGE ( 'NONE', *, *, #38041, .F. ) ;
#2324 = EDGE_CURVE ( 'NONE', #66023, #3025, #33490, .T. ) ;
#2325 = ORIENTED_EDGE ( 'NONE', *, *, #51865, .F. ) ;
#2326 = EDGE_CURVE ( 'NONE', #19391, #30922, #18475, .T. ) ;
#2327 = CARTESIAN_POINT ( 'NONE',  ( 107.0471828278920441, 27.43080724084231647, 70.75761023996984989 ) ) ;
#2328 = CARTESIAN_POINT ( 'NONE',  ( 164.4615316623334991, 63.29763980349832764, 61.02503964407276982 ) ) ;
#2329 = CARTESIAN_POINT ( 'NONE',  ( -189.9638655956219964, 108.0957249433520673, 62.03588848252969967 ) ) ;
#2330 = DIRECTION ( 'NONE',  ( -0.000000000000000000, 1.000000000000000000, -0.000000000000000000 ) ) ;
#2331 = PLANE ( 'NONE',  #41598 ) ;
#2332 = CARTESIAN_POINT ( 'NONE',  ( -108.6909373351217027, 36.15835109565442451, 60.93927029289248765 ) ) ;
#2333 = PLANE ( 'NONE',  #1386 ) ;
#2334 = CARTESIAN_POINT ( 'NONE',  ( 0.000000000000000000, 0.000000000000000000, 2.500000000000030198 ) ) ;
#2335 = ORIENTED_EDGE ( 'NONE', *, *, #23615, .F. ) ;
#2336 = VERTEX_POINT ( 'NONE', #32777 ) ;
#2337 = ORIENTED_EDGE ( 'NONE', *, *, #28584, .T. ) ;
#2338 = DIRECTION ( 'NONE',  ( 0.9216045519012663334, 0.000000000000000000, -0.3881301971180111110 ) ) ;
#2339 = CARTESIAN_POINT ( 'NONE',  ( -71.16326860233392892, 19.60396142827894295, 91.85506027016724317 ) ) ;
#2340 = CARTESIAN_POINT ( 'NONE',  ( 427.4999999999999432, -17.50000000000000000, 1.999999999999998224 ) ) ;
#2341 = B_SPLINE_CURVE_WITH_KNOTS ( 'NONE', 3,
 ( #56471, #55786, #30099, #35025, #29396, #2327, #13567, #56125, #46605, #68086, #61404, #50849, #24484, #19886, #45922, #41344, #19179, #62796, #7944, #8646, #13229, #40633, #3360, #8989, #2667, #34343, #24818, #46255, #40298, #40992, #45222, #18496, #24128, #67733, #7608, #62450, #66701, #39951, #14264, #35724, #57174, #30436, #29062, #50506 ),
 .UNSPECIFIED., .F., .F.,
 ( 4, 2, 2, 2, 2, 2, 2, 2, 2, 2, 2, 2, 2, 2, 2, 2, 2, 2, 2, 2, 2, 4 ),
 ( 0.000000000000000000, 0.001533942663855623412, 0.003067885327711246824, 0.004601827991566870453, 0.005368799323494680316, 0.006135770655422489311, 0.007669713319278136793, 0.008436684651205958799, 0.009203655983133782539, 0.01073759864698937277, 0.01150456997891716876, 0.01227154131084496475, 0.01303851264277275900, 0.01380548397470055325, 0.01533942663855618338, 0.01687336930241181004, 0.01840731196626744018, 0.01994125463012307031, 0.02070822596205088018, 0.02147519729397868657, 0.02300913995783433405, 0.02454308262168998500 ),
 .UNSPECIFIED. ) ;
#2342 = LINE ( 'NONE', #66717, #52285 ) ;
#2343 = CARTESIAN_POINT ( 'NONE',  ( -78.66644367742111399, 23.39876645725286153, -61.96000122218157458 ) ) ;
#2344 = LINE ( 'NONE', #17101, #4229 ) ;
#2345 = VECTOR ( 'NONE', #16431, 1000.000000000000000 ) ;
#2346 = CARTESIAN_POINT ( 'NONE',  ( -95.88693721180811735, 30.76307528361166632, -11.74052076892611218 ) ) ;
#2347 = CARTESIAN_POINT ( 'NONE',  ( 37.70762885381311236, 8.195134395012278361, 71.56854745327594003 ) ) ;
#2348 = CARTESIAN_POINT ( 'NONE',  ( 32.05329076859800352, 7.567153360545789909, 89.56790089374254649 ) ) ;
#2349 = CIRCLE ( 'NONE', #4590, 8.000000000000000000 ) ;
#2350 = SHAPE_REPRESENTATION_RELATIONSHIP ( 'NONE' , 'NONE' ,  #2894, #64275 ) ;
#2351 = ORIENTED_EDGE ( 'NONE', *, *, #40585, .F. ) ;
#2352 = CARTESIAN_POINT ( 'NONE',  ( -5.401648928593171028, 6.744888135494087500, -35.80373528830617857 ) ) ;
#2353 = CARTESIAN_POINT ( 'NONE',  ( -59.94154301275507635, -45.09516516490467808, 170.0000000000000000 ) ) ;
#2354 = CARTESIAN_POINT ( 'NONE',  ( -189.3111515777349894, 107.1887855376296841, -41.02269173539261260 ) ) ;
#2355 = CARTESIAN_POINT ( 'NONE',  ( -65.36598343705435354, 0.000000000000000000, 41.38025477438755928 ) ) ;
#2356 = LINE ( 'NONE', #23808, #45615 ) ;
#2357 = CARTESIAN_POINT ( 'NONE',  ( 217.9999999999999716, 126.6235316737731580, 94.99999999999866418 ) ) ;
#2358 = CARTESIAN_POINT ( 'NONE',  ( 127.4669243510812890, 38.85312661085428232, -12.71959053557455022 ) ) ;
#2359 = ORIENTED_EDGE ( 'NONE', *, *, #8756, .T. ) ;
#2360 = CARTESIAN_POINT ( 'NONE',  ( 537.6413221127930910, 951.2720944765814011, 735.5068267248718712 ) ) ;
#2361 = VECTOR ( 'NONE', #29823, 1000.000000000000000 ) ;
#2362 = CARTESIAN_POINT ( 'NONE',  ( -189.3111515777350462, 107.1887855376297125, -14.17814114492894184 ) ) ;
#2363 = CARTESIAN_POINT ( 'NONE',  ( -34.74023699876256899, 11.17830703027882855, -49.56910944950720932 ) ) ;
#2364 = CARTESIAN_POINT ( 'NONE',  ( -72.57286576968782299, -18.73210786364450442, 41.38025477438755928 ) ) ;
#2365 = CARTESIAN_POINT ( 'NONE',  ( -166.2425995121691642, 79.78465616981384301, 94.99999999999866418 ) ) ;
#2366 = ORIENTED_EDGE ( 'NONE', *, *, #19208, .F. ) ;
#2367 = CARTESIAN_POINT ( 'NONE',  ( -119.2982054035571338, 42.30181775808006961, -45.99331769202854758 ) ) ;
#2368 = DIRECTION ( 'NONE',  ( -0.000000000000000000, 0.000000000000000000, 1.000000000000000000 ) ) ;
#2369 = CARTESIAN_POINT ( 'NONE',  ( -0.5178428571329644070, 7.532057582089303871, -68.05658183845606857 ) ) ;
#2370 = CARTESIAN_POINT ( 'NONE',  ( 164.9466788279801790, 65.02358717534978894, 91.30755230343568485 ) ) ;
#2371 = EDGE_LOOP ( 'NONE', ( #59908, #20323, #39063, #20263 ) ) ;
#2372 = CARTESIAN_POINT ( 'NONE',  ( 164.4555644730588710, 64.60768971797665472, -94.57351069396484888 ) ) ;
#2373 = DIRECTION ( 'NONE',  ( 1.000000000000000000, 0.000000000000000000, 0.000000000000000000 ) ) ;
#2374 = CARTESIAN_POINT ( 'NONE',  ( -150.3850953947692233, 66.25368649589884740, 45.68226874722795827 ) ) ;
#2375 = CARTESIAN_POINT ( 'NONE',  ( 19.10216788411013411, 6.629360741291161041, -49.75156701922125535 ) ) ;
#2377 = ORIENTED_EDGE ( 'NONE', *, *, #20334, .T. ) ;
#2376 = CARTESIAN_POINT ( 'NONE',  ( 115.7612476187723871, 32.64200929566223408, 15.36962448049462182 ) ) ;
#2378 = B_SPLINE_CURVE_WITH_KNOTS ( 'NONE', 3,
 ( #44626, #17897, #61154, #8032, #56216, #49894, #34082, #45315, #55882, #22821, #60457, #12271, #1718, #61831, #2760, #18588, #33733, #12977, #12620, #23181, #7699, #7349, #40045, #39352, #34443, #2076, #55520, #1365, #65746, #28805, #6990, #24225, #45672, #29146, #67149, #50595, #50253, #18938, #40387, #34779, #2416, #39011, #13655, #23871, #60795 ),
 .UNSPECIFIED., .F., .F.,
 ( 4, 2, 2, 2, 2, 2, 2, 2, 1, 2, 2, 2, 2, 2, 2, 2, 2, 2, 2, 2, 2, 2, 4 ),
 ( 0.000000000000000000, 0.001470449819620651055, 0.002205674729430986882, 0.002940899639241323360, 0.004411349458861975499, 0.005881799278482627638, 0.007352249098103279777, 0.008087474007913614954, 0.008822698917723949263, 0.009557923827534283573, 0.01029314873734461962, 0.01176359855696526915, 0.01249882346677560346, 0.01323404837658594298, 0.01470449819620661507, 0.01543972310601695805, 0.01617494801582729930, 0.01764539783544796098, 0.01911584765506862613, 0.01985107256487894656, 0.02058629747468926699, 0.02205674729430991132, 0.02352719711393055912 ),
 .UNSPECIFIED. ) ;
#2379 = CARTESIAN_POINT ( 'NONE',  ( -1.000020675113008961, 7.549072000771346325, -93.38318693586774089 ) ) ;
#2380 = EDGE_CURVE ( 'NONE', #27926, #37383, #54205, .T. ) ;
#2381 = VERTEX_POINT ( 'NONE', #22569 ) ;
#2382 = VERTEX_POINT ( 'NONE', #6028 ) ;
#2383 = CARTESIAN_POINT ( 'NONE',  ( 174.2468109002382448, 73.34092405459588804, 39.90336194450533469 ) ) ;
#2384 = ADVANCED_FACE ( 'NONE', ( #38397 ), #59837, .F. ) ;
#2385 = CARTESIAN_POINT ( 'NONE',  ( 21.44031696305384571, 6.747195267824409370, -64.90930529496827717 ) ) ;
#2387 = VERTEX_POINT ( 'NONE', #18333 ) ;
#2386 = DIRECTION ( 'NONE',  ( 1.000000000000000000, 0.000000000000000000, 0.000000000000000000 ) ) ;
#2388 = CYLINDRICAL_SURFACE ( 'NONE', #7245, 7.500000000000013323 ) ;
#2389 = ADVANCED_FACE ( 'NONE', ( #2170, #50353, #34538 ), #24324, .F. ) ;
#2390 = CARTESIAN_POINT ( 'NONE',  ( -23.95089599695169014, 9.496585844566148182, 37.22793919491487458 ) ) ;
#2391 = FACE_BOUND ( 'NONE', #20555, .T. ) ;
#2392 = VERTEX_POINT ( 'NONE', #7790 ) ;
#2393 = VECTOR ( 'NONE', #37049, 1000.000000000000000 ) ;
#2394 = CARTESIAN_POINT ( 'NONE',  ( 204.6977192012829505, 108.0580384837234931, -78.17048162308530834 ) ) ;
#2395 = VECTOR ( 'NONE', #42182, 1000.000000000000000 ) ;
#2396 = MECHANICAL_DESIGN_GEOMETRIC_PRESENTATION_REPRESENTATION (  '', ( #32715 ), #59658 ) ;
#2397 = CARTESIAN_POINT ( 'NONE',  ( 136.7507824285649178, 44.38599729999916121, 43.93330792897594250 ) ) ;
#2398 = CARTESIAN_POINT ( 'NONE',  ( 6.400000000000000355, -4.618802153517011178, 8.000000000000000000 ) ) ;
#2399 = CARTESIAN_POINT ( 'NONE',  ( 0.000000000000000000, 0.000000000000000000, 0.000000000000000000 ) ) ;
#2400 = CARTESIAN_POINT ( 'NONE',  ( 22.15926701483429895, 7.796117250416237709, 68.32426611714438991 ) ) ;
#2401 = EDGE_CURVE ( 'NONE', #58133, #49065, #24667, .T. ) ;
#2402 = VERTEX_POINT ( 'NONE', #56664 ) ;
#2403 = VERTEX_POINT ( 'NONE', #29243 ) ;
#2404 = VERTEX_POINT ( 'NONE', #13411 ) ;
#2405 = STYLED_ITEM ( 'NONE', ( #35553 ), #16744 ) ;
#2406 = DIRECTION ( 'NONE',  ( -4.270088556250601699E-16, -0.000000000000000000, -1.000000000000000000 ) ) ;
#2407 =( NAMED_UNIT ( * ) PLANE_ANGLE_UNIT ( ) SI_UNIT ( $, .RADIAN. ) );
#2408 = CARTESIAN_POINT ( 'NONE',  ( -34.51918258780364823, 10.11719938103012417, -49.65991457455191238 ) ) ;
#2409 = DIRECTION ( 'NONE',  ( 0.000000000000000000, -0.000000000000000000, 1.000000000000000000 ) ) ;
#2410 = CARTESIAN_POINT ( 'NONE',  ( -149.5074843970971301, 64.17983161892345834, 30.72082123989904900 ) ) ;
#2411 = CARTESIAN_POINT ( 'NONE',  ( -130.2196570250629577, 49.40815211106350091, 58.81961367888054326 ) ) ;
#2412 = CARTESIAN_POINT ( 'NONE',  ( -62.20000168511805327, 17.76605013184458315, 93.80264320643617282 ) ) ;
#2413 = ORIENTED_EDGE ( 'NONE', *, *, #24190, .F. ) ;
#2414 = DIRECTION ( 'NONE',  ( 0.000000000000000000, 1.000000000000000000, -0.000000000000000000 ) ) ;
#2415 = EDGE_LOOP ( 'NONE', ( #22354, #8411, #56637, #13834 ) ) ;
#2416 = CARTESIAN_POINT ( 'NONE',  ( 36.99625334683020839, 8.108440754877200618, 30.29321116345249720 ) ) ;
#2417 = CARTESIAN_POINT ( 'NONE',  ( 84.74089592029041285, 19.84571403269345424, 56.79428774094038346 ) ) ;
#2418 = CARTESIAN_POINT ( 'NONE',  ( 181.5127080940606845, 79.03904173130082711, 44.30859410551142474 ) ) ;
#2419 = CARTESIAN_POINT ( 'NONE',  ( 20.79325243092023001, -13.87950479462515396, 0.000000000000000000 ) ) ;
#2420 = DIRECTION ( 'NONE',  ( 0.000000000000000000, 0.000000000000000000, 1.000000000000000000 ) ) ;
#2421 = CARTESIAN_POINT ( 'NONE',  ( -118.3918229753715252, 42.92682904595257298, 64.45486351284331761 ) ) ;
#2422 = CARTESIAN_POINT ( 'NONE',  ( -11.13714165684777768, 8.138643170880698108, -49.65174624528041392 ) ) ;
#2423 = PLANE ( 'NONE',  #28142 ) ;
#2424 = ORIENTED_EDGE ( 'NONE', *, *, #44709, .F. ) ;
#2425 = CARTESIAN_POINT ( 'NONE',  ( -104.3671396759760910, 33.85343629185614134, -88.98748543686591006 ) ) ;
#2426 = CARTESIAN_POINT ( 'NONE',  ( 15.55634918610400241, -15.55634918610406103, 0.000000000000000000 ) ) ;
#2427 = ORIENTED_EDGE ( 'NONE', *, *, #48014, .T. ) ;
#2428 = CARTESIAN_POINT ( 'NONE',  ( -60.00000000000000000, 0.000000000000000000, -10.00000000000000000 ) ) ;
#2429 = CARTESIAN_POINT ( 'NONE',  ( -59.58556642339447507, 16.99097764963621060, 70.65714236767303191 ) ) ;
#2430 = LINE ( 'NONE', #50964, #30805 ) ;
#2431 = EDGE_LOOP ( 'NONE', ( #44600, #48576 ) ) ;
#2432 = FACE_OUTER_BOUND ( 'NONE', #59132, .T. ) ;
#2433 = CARTESIAN_POINT ( 'NONE',  ( 151.6178224291901131, 54.48737267587417676, -65.77168945991468263 ) ) ;
#2434 = CARTESIAN_POINT ( 'NONE',  ( -33.37566357177431087, 9.916833145467597532, 30.45442685525332038 ) ) ;
#2435 = CARTESIAN_POINT ( 'NONE',  ( 140.4897729434289886, 45.57634363643750675, -39.98413189135570889 ) ) ;
#2436 = EDGE_LOOP ( 'NONE', ( #28978, #59934, #27975, #24956 ) ) ;
#2437 = VECTOR ( 'NONE', #32455, 1000.000000000000000 ) ;
#2438 = CARTESIAN_POINT ( 'NONE',  ( -120.4586945679390482, 43.01762219615311267, 43.31108851025778250 ) ) ;
#2439 = ORIENTED_EDGE ( 'NONE', *, *, #13053, .F. ) ;
#2440 = CARTESIAN_POINT ( 'NONE',  ( 36.98541457540711264, 9.120571655722415016, -9.158542404804654424 ) ) ;
#2441 = PLANE ( 'NONE',  #40587 ) ;
#2442 = VECTOR ( 'NONE', #25225, 1000.000000000000000 ) ;
#2443 = CARTESIAN_POINT ( 'NONE',  ( -1.095583923122879888, 7.553030873957006897, 14.09065126040307270 ) ) ;
#2444 = EDGE_CURVE ( 'NONE', #13950, #58737, #55978, .T. ) ;
#2445 = CARTESIAN_POINT ( 'NONE',  ( 126.8687677780346093, 38.51583040706892547, 93.44669519883952091 ) ) ;
#2446 = PRODUCT_DEFINITION_SHAPE ( 'NONE', 'NONE',  #69600 ) ;
#2447 = CYLINDRICAL_SURFACE ( 'NONE', #33618, 25.00000000000000711 ) ;
#2448 = AXIS2_PLACEMENT_3D ( 'NONE', #61221, #56632, #34153 ) ;
#2450 = AXIS2_PLACEMENT_3D ( 'NONE', #32714, #5964, #27425 ) ;
#2449 = DIRECTION ( 'NONE',  ( 1.000000000000000000, -0.000000000000000000, 0.000000000000000000 ) ) ;
#2451 = DIRECTION ( 'NONE',  ( -0.000000000000000000, -1.000000000000000000, -0.000000000000000000 ) ) ;
#2452 = ORIENTED_EDGE ( 'NONE', *, *, #16743, .T. ) ;
#2453 = CARTESIAN_POINT ( 'NONE',  ( 0.000000000000000000, -2.000000000000000000, 380.0000000000000000 ) ) ;
#2454 = FACE_OUTER_BOUND ( 'NONE', #34954, .T. ) ;
#2455 = CARTESIAN_POINT ( 'NONE',  ( 67.92995549349548412, 13.86623459444475337, 58.47094168735598174 ) ) ;
#2456 = CARTESIAN_POINT ( 'NONE',  ( 138.2204650371259049, 44.12203217345472694, -64.24952538475335473 ) ) ;
#2457 = FACE_OUTER_BOUND ( 'NONE', #58163, .T. ) ;
#2458 = VECTOR ( 'NONE', #56262, 1000.000000000000000 ) ;
#2459 = ORIENTED_EDGE ( 'NONE', *, *, #31851, .T. ) ;
#2460 = EDGE_CURVE ( 'NONE', #11779, #61489, #23625, .T. ) ;
#2461 = CARTESIAN_POINT ( 'NONE',  ( -35.00000000000000000, -35.00000000000000000, 2.000000000000000000 ) ) ;
#2462 = EDGE_CURVE ( 'NONE', #66935, #36885, #51734, .T. ) ;
#2463 = CARTESIAN_POINT ( 'NONE',  ( 8.336882341125877005, 6.376438415325264231, 36.53121488364622138 ) ) ;
#2464 = EDGE_LOOP ( 'NONE', ( #43968, #36978, #53446, #55906, #66488, #18902, #35917 ) ) ;
#2465 = LINE ( 'NONE', #61884, #68216 ) ;
#2466 = LINE ( 'NONE', #23918, #19606 ) ;
#2467 = ORIENTED_EDGE ( 'NONE', *, *, #66746, .T. ) ;
#2468 = CARTESIAN_POINT ( 'NONE',  ( 157.4703587214989113, 58.92748579479260229, -36.12418429913763163 ) ) ;
#2469 = EDGE_CURVE ( 'NONE', #68633, #48880, #31068, .T. ) ;
#2470 = PLANE ( 'NONE',  #7800 ) ;
#2471 = CARTESIAN_POINT ( 'NONE',  ( -25.87147652227456263, 70.00000000000000000, 77.58025477438755502 ) ) ;
#2472 = CARTESIAN_POINT ( 'NONE',  ( 0.000000000000000000, 0.000000000000000000, 40.00000000000003553 ) ) ;
#2473 = ORIENTED_EDGE ( 'NONE', *, *, #43442, .T. ) ;
#2474 = CARTESIAN_POINT ( 'NONE',  ( -97.86516199987804043, 31.71158167298306907, 5.092746270469413972 ) ) ;
#2475 = CARTESIAN_POINT ( 'NONE',  ( 70.47378276567178546, 15.56829108688369345, 91.86182244508080430 ) ) ;
#2476 = CARTESIAN_POINT ( 'NONE',  ( 157.4703587214989113, 57.65129005721576760, 29.40946747225336466 ) ) ;
#2477 = CARTESIAN_POINT ( 'NONE',  ( 79.18180043629683951, 18.06526831600449157, -17.49560269492410924 ) ) ;
#2478 = CARTESIAN_POINT ( 'NONE',  ( -131.6508182719823594, 50.40277850441007246, -20.40230296405928101 ) ) ;
#2479 = CARTESIAN_POINT ( 'NONE',  ( -149.5074843970971301, 64.17983161892347255, -88.50193171241930656 ) ) ;
#2480 = CARTESIAN_POINT ( 'NONE',  ( 126.8947007444828614, 37.37669340849691224, -73.16922649445019999 ) ) ;
#2481 = EDGE_CURVE ( 'NONE', #65549, #11659, #47136, .T. ) ;
#2482 = EDGE_LOOP ( 'NONE', ( #8029, #97, #20347, #42967 ) ) ;
#2483 = CARTESIAN_POINT ( 'NONE',  ( -3.816391647148975608E-14, -9.237604307034022355, -0.7145311798163346273 ) ) ;
#2484 = CYLINDRICAL_SURFACE ( 'NONE', #43335, 7.500000000000020428 ) ;
#2485 = ORIENTED_EDGE ( 'NONE', *, *, #16200, .T. ) ;
#2486 = EDGE_CURVE ( 'NONE', #45063, #30339, #20404, .T. ) ;
#2487 = ADVANCED_FACE ( 'NONE', ( #5266 ), #48156, .T. ) ;
#2488 = DIRECTION ( 'NONE',  ( 0.000000000000000000, 0.000000000000000000, 1.000000000000000000 ) ) ;
#2489 = CARTESIAN_POINT ( 'NONE',  ( 3.319543390096045155, -7.321065037175443990, -0.01688885742777720272 ) ) ;
#2490 = PLANE ( 'NONE',  #35776 ) ;
#2491 = VECTOR ( 'NONE', #11976, 1000.000000000000114 ) ;
#2492 = DIRECTION ( 'NONE',  ( 0.000000000000000000, -1.000000000000000000, 0.000000000000000000 ) ) ;
#2493 = CARTESIAN_POINT ( 'NONE',  ( -8.252323494751598432, 6.918840298267292965, -89.10717191287119476 ) ) ;
#2494 = CARTESIAN_POINT ( 'NONE',  ( -51.78153763344965910, 13.82841714689605084, -76.32711335290281340 ) ) ;
#2495 = CARTESIAN_POINT ( 'NONE',  ( -1.328627985309863258, 7.561890325089884790, -19.82887340779442198 ) ) ;
#2497 = CARTESIAN_POINT ( 'NONE',  ( -7.825402957745085430, 7.899365992529246761, 45.11558103944722120 ) ) ;
#2496 = VECTOR ( 'NONE', #42537, 1000.000000000000000 ) ;
#2498 = VECTOR ( 'NONE', #34813, 1000.000000000000000 ) ;
#2499 = DIRECTION ( 'NONE',  ( -1.000000000000000000, 0.000000000000000000, 0.000000000000000000 ) ) ;
#2500 = ORIENTED_EDGE ( 'NONE', *, *, #27204, .T. ) ;
#2501 = CARTESIAN_POINT ( 'NONE',  ( -96.02159028238557426, 30.82695531378849552, -38.37423410059079032 ) ) ;
#2502 = ORIENTED_EDGE ( 'NONE', *, *, #48803, .F. ) ;
#2503 = DIRECTION ( 'NONE',  ( 1.387778780781446169E-16, -1.000000000000000000, -3.469446951953615421E-17 ) ) ;
#2504 = CIRCLE ( 'NONE', #11457, 66.50000000000000000 ) ;
#2505 = CARTESIAN_POINT ( 'NONE',  ( 41.33434189587760699, 9.684413566891869607, -9.024336741280105656 ) ) ;
#2506 = CARTESIAN_POINT ( 'NONE',  ( 46.41758729921143356, 9.425975226414241348, 61.59540596826231962 ) ) ;
#2507 = LINE ( 'NONE', #49989, #5388 ) ;
#2508 = DIRECTION ( 'NONE',  ( 1.000000000000000000, 0.000000000000000000, 0.000000000000000000 ) ) ;
#2509 = VECTOR ( 'NONE', #66846, 1000.000000000000000 ) ;
#2510 = CARTESIAN_POINT ( 'NONE',  ( 432.4999999999999432, -17.50000000000000000, 1.999999999999998224 ) ) ;
#2511 = DIRECTION ( 'NONE',  ( 1.000000000000000000, 0.000000000000000000, -0.000000000000000000 ) ) ;
#2512 = CARTESIAN_POINT ( 'NONE',  ( -169.8791831685531122, 83.59058982490286382, 71.94396900893276836 ) ) ;
#2513 = ORIENTED_EDGE ( 'NONE', *, *, #2918, .F. ) ;
#2514 = EDGE_LOOP ( 'NONE', ( #42301, #32097, #17830, #68201, #41419, #24026, #6192, #42764, #12951 ) ) ;
#2515 = LINE ( 'NONE', #29246, #19698 ) ;
#2516 = CARTESIAN_POINT ( 'NONE',  ( 41.49663191311417165, -50.03028622612021792, 40.00000000000003553 ) ) ;
#2517 = CARTESIAN_POINT ( 'NONE',  ( -5.000000000000073719, -41.66904755831212270, 85.00100000000000477 ) ) ;
#2518 = CARTESIAN_POINT ( 'NONE',  ( 102.7938674513918613, 26.67851209377771227, 64.96700818474666050 ) ) ;
#2519 = FACE_OUTER_BOUND ( 'NONE', #35690, .T. ) ;
#2520 = CARTESIAN_POINT ( 'NONE',  ( 58.09877917144281412, 12.61383386832655518, -22.06060978329331235 ) ) ;
#2521 = ORIENTED_EDGE ( 'NONE', *, *, #2569, .T. ) ;
#2522 = CARTESIAN_POINT ( 'NONE',  ( -3.120068508582665157, -41.61225602822255354, 13.79046340968177553 ) ) ;
#2523 = CARTESIAN_POINT ( 'NONE',  ( -14.55390976651257162, 7.422979442794212623, 61.13778679154074780 ) ) ;
#2524 = CARTESIAN_POINT ( 'NONE',  ( -84.23431294393863311, 24.52078568147205218, -20.81987607538617624 ) ) ;
#2525 = CARTESIAN_POINT ( 'NONE',  ( 7.484861546145032740, 64.56761454192837846, 170.0000000000000000 ) ) ;
#2526 = CARTESIAN_POINT ( 'NONE',  ( 212.1707951106656935, 117.1901534358505899, -16.32344178605950091 ) ) ;
#2527 = ADVANCED_FACE ( 'NONE', ( #21112 ), #68930, .T. ) ;
#2528 = CARTESIAN_POINT ( 'NONE',  ( 9.229352927370984006, 6.379222623903515021, -93.04627149865262936 ) ) ;
#2529 = EDGE_CURVE ( 'NONE', #48794, #67246, #9433, .T. ) ;
#2530 = VERTEX_POINT ( 'NONE', #64348 ) ;
#2531 = DIRECTION ( 'NONE',  ( -1.000000000000000000, 0.000000000000000000, 0.000000000000000000 ) ) ;
#2532 = CARTESIAN_POINT ( 'NONE',  ( -417.6627218934913799, 399.9999999999998295, -111.4497041420118251 ) ) ;
#2533 = CIRCLE ( 'NONE', #56453, 30.00000000000000000 ) ;
#2534 = CARTESIAN_POINT ( 'NONE',  ( 31.91383250562746099, 8.564461488296995384, -69.47600483345588884 ) ) ;
#2535 = FACE_OUTER_BOUND ( 'NONE', #48112, .T. ) ;
#2536 = CARTESIAN_POINT ( 'NONE',  ( -444.4229916354184979, 394.6798985497181320, 96.05029585798874336 ) ) ;
#2537 = CARTESIAN_POINT ( 'NONE',  ( 82.14449817946434962, 17.93919511903895980, -64.14975613024911638 ) ) ;
#2538 = ORIENTED_EDGE ( 'NONE', *, *, #32611, .T. ) ;
#2540 = ADVANCED_FACE ( 'NONE', ( #63328 ), #42214, .F. ) ;
#2539 = CARTESIAN_POINT ( 'NONE',  ( -5.767955557622883589E-14, -31.11269837220806878, 0.000000000000000000 ) ) ;
#2541 = CARTESIAN_POINT ( 'NONE',  ( 197.1979149960397706, 98.19687999752001417, -44.16128514133923488 ) ) ;
#2542 = EDGE_LOOP ( 'NONE', ( #55637, #55611, #67408, #62699 ) ) ;
#2543 = CIRCLE ( 'NONE', #21607, 25.00000000000395772 ) ;
#2544 = EDGE_CURVE ( 'NONE', #45063, #35721, #38639, .T. ) ;
#2545 = LINE ( 'NONE', #8521, #51988 ) ;
#2546 = ORIENTED_EDGE ( 'NONE', *, *, #59775, .T. ) ;
#2547 = LINE ( 'NONE', #40867, #69041 ) ;
#2548 = CARTESIAN_POINT ( 'NONE',  ( -59.95412189755936794, 17.09836075175410031, -21.56948105266851812 ) ) ;
#2549 = CARTESIAN_POINT ( 'NONE',  ( -35.00000000000000000, 225.0000000000000000, 2.000000000000000000 ) ) ;
#2550 = ORIENTED_EDGE ( 'NONE', *, *, #27368, .F. ) ;
#2551 = EDGE_CURVE ( 'NONE', #35639, #58973, #65437, .T. ) ;
#2552 = CIRCLE ( 'NONE', #39606, 5.000000000000004441 ) ;
#2553 = ORIENTED_EDGE ( 'NONE', *, *, #4045, .F. ) ;
#2554 = CARTESIAN_POINT ( 'NONE',  ( 45.35621884287174055, 10.27694987765648449, 59.67183030682132738 ) ) ;
#2555 = DIRECTION ( 'NONE',  ( 1.000000000000000000, 0.000000000000000000, 0.000000000000000000 ) ) ;
#2556 = EDGE_CURVE ( 'NONE', #10732, #61153, #15137, .T. ) ;
#2557 = CARTESIAN_POINT ( 'NONE',  ( 21.88606409348644277, 6.772455198693823952, 6.296696862013998697 ) ) ;
#2558 = B_SPLINE_CURVE_WITH_KNOTS ( 'NONE', 3,
 ( #36675, #58126, #50510, #31395, #4651, #30359, #47546, #45226, #20832, #66704, #65484, #44006, #53858, #27138, #53166, #33128, #26463, #17277, #58452, #21516, #764, #31731, #6386, #43656, #59143, #406, #4999, #64782, #59489, #42630, #32431, #22563, #37693, #48231, #21863, #56, #5675, #22218, #1114, #48571, #53518, #64430, #65134 ),
 .UNSPECIFIED., .F., .F.,
 ( 4, 2, 2, 2, 2, 2, 2, 2, 2, 2, 2, 2, 1, 2, 2, 2, 2, 2, 2, 2, 2, 4 ),
 ( 0.02371951416048007424, 0.02520633211177539593, 0.02594974108742303595, 0.02669315006307067598, 0.02817996801436595949, 0.02966678596566124648, 0.03041019494130889345, 0.03115360391695653694, 0.03264042186825182740, 0.03412723981954712132, 0.03561405777084241525, 0.03635746674649006221, 0.03710087572213770918, 0.03784428469778534920, 0.03858769367343299617, 0.04007451162472830397, 0.04156132957602360484, 0.04304814752731890570, 0.04379155650296656654, 0.04453496547861421351, 0.04602178342990952131, 0.04750860138120482218 ),
 .UNSPECIFIED. ) ;
#2559 = EDGE_LOOP ( 'NONE', ( #62181, #13017, #69406, #67367 ) ) ;
#2560 = FILL_AREA_STYLE_COLOUR ( '', #18851 ) ;
#2561 = CARTESIAN_POINT ( 'NONE',  ( -48.34250119710923599, 14.01879126850789348, 7.613551659782504366 ) ) ;
#2562 = CARTESIAN_POINT ( 'NONE',  ( -132.2161740628506266, 52.03204870034953444, -19.61185874996504452 ) ) ;
#2563 = CARTESIAN_POINT ( 'NONE',  ( 117.7411475730015553, 32.50808475802735131, -17.12051833154609426 ) ) ;
#2564 = LINE ( 'NONE', #55321, #48891 ) ;
#2566 = ORIENTED_EDGE ( 'NONE', *, *, #63693, .F. ) ;
#2565 = DIRECTION ( 'NONE',  ( 1.000000000000000000, -9.109522253334613014E-16, 0.000000000000000000 ) ) ;
#2567 = ORIENTED_EDGE ( 'NONE', *, *, #16266, .F. ) ;
#2568 = EDGE_CURVE ( 'NONE', #37758, #24336, #57705, .T. ) ;
#2569 = EDGE_CURVE ( 'NONE', #13609, #53396, #62064, .T. ) ;
#2570 = ORIENTED_EDGE ( 'NONE', *, *, #11979, .T. ) ;
#2571 = CARTESIAN_POINT ( 'NONE',  ( 46.84183314611289006, 9.494161546644502181, 11.54854982055374535 ) ) ;
#2572 = CARTESIAN_POINT ( 'NONE',  ( -179.9869519326159946, 96.69839571505836773, 88.97430052463283801 ) ) ;
#2573 = CARTESIAN_POINT ( 'NONE',  ( -48.32993240732256623, 12.98137013984324639, -12.50980678800987000 ) ) ;
#2574 = CARTESIAN_POINT ( 'NONE',  ( 102.7551177910568470, 25.56939188780867767, -17.07542069066059298 ) ) ;
#2575 = EDGE_CURVE ( 'NONE', #49581, #11859, #45372, .T. ) ;
#2576 = CARTESIAN_POINT ( 'NONE',  ( 204.6977192012829789, 106.3443248447423599, 2.363170148305747009 ) ) ;
#2577 = CARTESIAN_POINT ( 'NONE',  ( 211.4199041905045249, 117.8812456326728721, 87.06571698777939616 ) ) ;
#2578 = LINE ( 'NONE', #60620, #48950 ) ;
#2579 = FACE_OUTER_BOUND ( 'NONE', #67824, .T. ) ;
#2580 = CARTESIAN_POINT ( 'NONE',  ( -13.78709718204646428, 7.352743657744177597, 33.03876092935409758 ) ) ;
#2581 = ORIENTED_EDGE ( 'NONE', *, *, #47265, .T. ) ;
#2582 = CARTESIAN_POINT ( 'NONE',  ( 8.336237313193160858, 7.382629160459395656, -15.19676915959678709 ) ) ;
#2583 = ORIENTED_EDGE ( 'NONE', *, *, #50107, .F. ) ;
#2584 = ORIENTED_EDGE ( 'NONE', *, *, #47172, .T. ) ;
#2585 = CARTESIAN_POINT ( 'NONE',  ( -146.1140637052938587, 62.65471088530799904, 4.672121997598104315 ) ) ;
#2586 = CARTESIAN_POINT ( 'NONE',  ( 124.4094311749753814, 190.0000000000000000, -91.28179539054374914 ) ) ;
#2587 = CARTESIAN_POINT ( 'NONE',  ( -38.93057666883864698, 11.96714560916617742, 90.92290394697204192 ) ) ;
#2588 = CARTESIAN_POINT ( 'NONE',  ( -99.31850058233801803, 31.30166762705811223, -35.62007679328529974 ) ) ;
#2589 = AXIS2_PLACEMENT_3D ( 'NONE', #56553, #52313, #9067 ) ;
#2590 = CARTESIAN_POINT ( 'NONE',  ( 41.66904755831210849, 4.999999999999909406, 2.000000000000001776 ) ) ;
#2591 = LINE ( 'NONE', #61331, #12397 ) ;
#2592 = DIRECTION ( 'NONE',  ( -1.000000000000000000, 0.000000000000000000, 0.000000000000000000 ) ) ;
#2593 = VERTEX_POINT ( 'NONE', #21779 ) ;
#2594 = ORIENTED_EDGE ( 'NONE', *, *, #1303, .F. ) ;
#2595 = VECTOR ( 'NONE', #6924, 1000.000000000000000 ) ;
#2596 = DIRECTION ( 'NONE',  ( -2.168404344971009361E-16, 0.000000000000000000, 1.000000000000000000 ) ) ;
#2597 = CARTESIAN_POINT ( 'NONE',  ( 422.4999999999999432, -17.50000000000000000, 20.00000000000000000 ) ) ;
#2598 = CARTESIAN_POINT ( 'NONE',  ( 0.6543471694412384965, 8.859816792613651515, -0.4964154566687983272 ) ) ;
#2599 = VECTOR ( 'NONE', #20855, 1000.000000000000000 ) ;
#2600 = CARTESIAN_POINT ( 'NONE',  ( -26.50364027666005029, 8.832969329054181529, -75.33011242007280828 ) ) ;
#2601 = AXIS2_PLACEMENT_3D ( 'NONE', #24393, #62712, #45834 ) ;
#2602 = CARTESIAN_POINT ( 'NONE',  ( -47.60396279792516339, 12.80997843568594874, 36.81109710626871134 ) ) ;
#2603 = CARTESIAN_POINT ( 'NONE',  ( 10.13846145460683523, 6.385368868491637429, 15.62687571206995329 ) ) ;
#2604 = ORIENTED_EDGE ( 'NONE', *, *, #10155, .T. ) ;
#2605 = CARTESIAN_POINT ( 'NONE',  ( 44.34689728705971845, 10.12166135033765002, -64.30425762756091501 ) ) ;
#2606 = CARTESIAN_POINT ( 'NONE',  ( -59.95412189755936083, 17.09836075175411807, -75.25858223359590227 ) ) ;
#2607 = CARTESIAN_POINT ( 'NONE',  ( 197.9843579228224542, 99.18296459057403069, -67.31460967885617208 ) ) ;
#2608 = CARTESIAN_POINT ( 'NONE',  ( 275.6615829231344037, -21.85840048673442126, -2.507220999339073053 ) ) ;
#2609 = CARTESIAN_POINT ( 'NONE',  ( 109.3047266816501377, 28.44977739115299187, 2.810780713438274070 ) ) ;
#2610 = CARTESIAN_POINT ( 'NONE',  ( -169.3420190433745063, 83.01791327558585465, -89.40959992967984249 ) ) ;
#2611 = PLANE ( 'NONE',  #12739 ) ;
#2612 = CARTESIAN_POINT ( 'NONE',  ( -137.3060924980642596, 138.4631249211268482, 10.00000000000000000 ) ) ;
#2613 = EDGE_CURVE ( 'NONE', #65931, #57935, #59366, .T. ) ;
#2614 = CARTESIAN_POINT ( 'NONE',  ( 264.4165763529819628, 225.8585178651493948, 128.9999999999999716 ) ) ;
#2615 = VERTEX_POINT ( 'NONE', #44275 ) ;
#2616 = DIRECTION ( 'NONE',  ( -0.7071067811865474617, 0.7071067811865474617, -0.000000000000000000 ) ) ;
#2617 = CARTESIAN_POINT ( 'NONE',  ( 150.2193536046551969, 53.46717047532150957, 61.81829156147041715 ) ) ;
#2618 = CARTESIAN_POINT ( 'NONE',  ( -12.50000000000000000, -17.50000000000000000, 1.999999999999998224 ) ) ;
#2619 = LINE ( 'NONE', #39563, #860 ) ;
#2620 = LINE ( 'NONE', #24085, #58061 ) ;
#2621 = ORIENTED_EDGE ( 'NONE', *, *, #25957, .T. ) ;
#2623 = ADVANCED_FACE ( 'NONE', ( #38664 ), #5943, .F. ) ;
#2622 = DIRECTION ( 'NONE',  ( 1.000000000000000000, 0.000000000000000000, 0.000000000000000000 ) ) ;
#2624 = CARTESIAN_POINT ( 'NONE',  ( -452.6627218934912662, 364.9999999999998863, 113.5502958579877912 ) ) ;
#2625 = ORIENTED_EDGE ( 'NONE', *, *, #31517, .T. ) ;
#2626 = VERTEX_POINT ( 'NONE', #43227 ) ;
#2627 = AXIS2_PLACEMENT_3D ( 'NONE', #18525, #51577, #23805 ) ;
#2628 = PLANE ( 'NONE',  #6078 ) ;
#2629 = PLANE ( 'NONE',  #1672 ) ;
#2630 = ADVANCED_FACE ( 'NONE', ( #17556 ), #16849, .F. ) ;
#2631 = DIRECTION ( 'NONE',  ( -1.000000000000000000, 0.000000000000000000, 0.000000000000000000 ) ) ;
#2632 = ORIENTED_EDGE ( 'NONE', *, *, #31478, .F. ) ;
#2633 = DIRECTION ( 'NONE',  ( 0.000000000000000000, -0.000000000000000000, -1.000000000000000000 ) ) ;
#2634 = EDGE_CURVE ( 'NONE', #39735, #19572, #687, .T. ) ;
#2635 = CARTESIAN_POINT ( 'NONE',  ( -34.29440389294403246, 17.09499999999999886, 0.000000000000000000 ) ) ;
#2636 = CARTESIAN_POINT ( 'NONE',  ( -4.081377963939790909, 6.676029627840591729, 4.267774825659859772 ) ) ;
#2637 = PRESENTATION_LAYER_ASSIGNMENT (  '', '', ( #65548 ) ) ;
#2638 = CARTESIAN_POINT ( 'NONE',  ( 55.51528220483959331, 12.08323518953686104, -42.98226798348757427 ) ) ;
#2639 = CARTESIAN_POINT ( 'NONE',  ( 11.70038220502452297, -40.05515866293553984, 13.79046340968177553 ) ) ;
#2640 = CARTESIAN_POINT ( 'NONE',  ( 150.7492521598543078, 52.60853770899247905, 87.25043900936348962 ) ) ;
#2641 = AXIS2_PLACEMENT_3D ( 'NONE', #67736, #19535, #40994 ) ;
#2642 = CARTESIAN_POINT ( 'NONE',  ( 136.1310312718401576, 42.81430973242785853, 17.32757056502941495 ) ) ;
#2643 = AXIS2_PLACEMENT_3D ( 'NONE', #60950, #23670, #66257 ) ;
#2644 = ORIENTED_EDGE ( 'NONE', *, *, #1262, .F. ) ;
#2645 = PLANE ( 'NONE',  #51441 ) ;
#2646 = CIRCLE ( 'NONE', #56567, 60.00000000000000000 ) ;
#2647 = CARTESIAN_POINT ( 'NONE',  ( -76.78104518372332166, 22.68568622761702969, 3.798941945053491143 ) ) ;
#2648 = FACE_BOUND ( 'NONE', #8178, .T. ) ;
#2649 = FACE_OUTER_BOUND ( 'NONE', #33605, .T. ) ;
#2651 = VERTEX_POINT ( 'NONE', #22484 ) ;
#2650 = CARTESIAN_POINT ( 'NONE',  ( -149.5074843970971017, 64.17983161892347255, -34.81283053149196149 ) ) ;
#2652 = CARTESIAN_POINT ( 'NONE',  ( -12.71198166530289342, -21.52685583500284139, 0.000000000000000000 ) ) ;
#2653 = VECTOR ( 'NONE', #5003, 1000.000000000000114 ) ;
#2654 = EDGE_CURVE ( 'NONE', #33368, #44925, #15052, .T. ) ;
#2655 = ORIENTED_EDGE ( 'NONE', *, *, #23784, .F. ) ;
#2656 = DIRECTION ( 'NONE',  ( 0.000000000000000000, 0.000000000000000000, 1.000000000000000000 ) ) ;
#2657 = CARTESIAN_POINT ( 'NONE',  ( 84.26390409839190454, 19.68678207880321906, 44.34546724818678598 ) ) ;
#2658 = CARTESIAN_POINT ( 'NONE',  ( 0.000000000000000000, 0.000000000000000000, 41.38025477438755928 ) ) ;
#2659 = EDGE_CURVE ( 'NONE', #40482, #29355, #17910, .T. ) ;
#2660 = DIRECTION ( 'NONE',  ( -0.000000000000000000, -0.000000000000000000, -1.000000000000000000 ) ) ;
#2661 = CARTESIAN_POINT ( 'NONE',  ( -125.0023254877051215, 45.90912477771774292, 57.50388153796715329 ) ) ;
#2662 = CARTESIAN_POINT ( 'NONE',  ( -125.8938041572051389, -170.0000000000000000, 38.11994787315708777 ) ) ;
#2663 = CARTESIAN_POINT ( 'NONE',  ( 19.76786553127199042, 7.667850394326512387, -90.33727694201498082 ) ) ;
#2664 = CARTESIAN_POINT ( 'NONE',  ( -48.34500911884043006, 14.01939034823941910, 41.18154736179070596 ) ) ;
#2665 = ORIENTED_EDGE ( 'NONE', *, *, #60967, .F. ) ;
#2666 = EDGE_LOOP ( 'NONE', ( #64992, #17344, #63519, #7045 ) ) ;
#2667 = CARTESIAN_POINT ( 'NONE',  ( 102.7551177910568470, 25.56939188780867056, 63.45823108073047081 ) ) ;
#2668 = LINE ( 'NONE', #50507, #54840 ) ;
#2669 = CARTESIAN_POINT ( 'NONE',  ( 8.000000000000001776, 0.000000000000000000, -9.500000000000000000 ) ) ;
#2670 = LINE ( 'NONE', #30103, #1173 ) ;
#2671 = DIRECTION ( 'NONE',  ( -0.000000000000000000, -1.000000000000000000, -0.000000000000000000 ) ) ;
#2672 = CARTESIAN_POINT ( 'NONE',  ( -29.04258984626623175, 9.210213971636685315, -49.92821304749501365 ) ) ;
#2673 = LINE ( 'NONE', #25526, #4850 ) ;
#2674 = ORIENTED_EDGE ( 'NONE', *, *, #30840, .F. ) ;
#2675 = ORIENTED_EDGE ( 'NONE', *, *, #59329, .T. ) ;
#2676 = EDGE_LOOP ( 'NONE', ( #13530, #3406, #22223, #37378, #48877, #45798, #46771, #41194, #5341 ) ) ;
#2677 = CARTESIAN_POINT ( 'NONE',  ( -7.825402957745083654, 6.891034867348166060, -50.41807073194384259 ) ) ;
#2678 = CARTESIAN_POINT ( 'NONE',  ( -79.92369693322969226, 22.80368560911615816, 84.18822230409878671 ) ) ;
#2679 = CARTESIAN_POINT ( 'NONE',  ( -8.000000000000000000, 1.572549600175622730, -9.431055444744870897 ) ) ;
#2680 = CARTESIAN_POINT ( 'NONE',  ( 70.26722489419891815, 14.47234958177329212, -45.19821637890682808 ) ) ;
#2681 = LINE ( 'NONE', #55439, #22046 ) ;
#2682 = CARTESIAN_POINT ( 'NONE',  ( -61.77164219855452387, 17.63686644795249236, 41.18722385704388955 ) ) ;
#2683 = CARTESIAN_POINT ( 'NONE',  ( -94.83091526606385457, 30.26550147229322363, -16.68601127600661371 ) ) ;
#2684 = PRODUCT_DEFINITION ( 'UNKNOWN', '', #8623, #54214 ) ;
#2685 = VECTOR ( 'NONE', #29942, 1000.000000000000000 ) ;
#2686 = FACE_OUTER_BOUND ( 'NONE', #48013, .T. ) ;
#2687 = CARTESIAN_POINT ( 'NONE',  ( 111.9975424824652634, 0.000000000000000000, 256.6193948016162381 ) ) ;
#2688 = CARTESIAN_POINT ( 'NONE',  ( -190.6985136298602015, 109.1272424661243434, -91.34903848884556510 ) ) ;
#2689 = ORIENTED_EDGE ( 'NONE', *, *, #47335, .T. ) ;
#2690 = CARTESIAN_POINT ( 'NONE',  ( -5.871577929436018195, 6.771181646175758573, -35.66018690998220819 ) ) ;
#2691 = DIRECTION ( 'NONE',  ( 0.000000000000000000, -0.000000000000000000, 1.000000000000000000 ) ) ;
#2692 = CARTESIAN_POINT ( 'NONE',  ( 2.699999999999990408, 0.000000000000000000, 0.000000000000000000 ) ) ;
#2693 = CIRCLE ( 'NONE', #30760, 24.99999999999985434 ) ;
#2694 = CARTESIAN_POINT ( 'NONE',  ( -78.66644367742109978, 22.32174330031318732, -50.11545063171791270 ) ) ;
#2696 = EDGE_CURVE ( 'NONE', #22856, #4959, #22574, .T. ) ;
#2695 = CARTESIAN_POINT ( 'NONE',  ( 283.9728608271481107, -21.78879854653021297, -3.053399776244554609 ) ) ;
#2697 = CARTESIAN_POINT ( 'NONE',  ( -108.6909373351217170, 36.15835109565441741, -73.28348265942591411 ) ) ;
#2698 = AXIS2_PLACEMENT_3D ( 'NONE', #27431, #33074, #22512 ) ;
#2699 = CARTESIAN_POINT ( 'NONE',  ( 131.6115093721024891, 41.25402743071401801, -23.83854876421534996 ) ) ;
#2700 = ADVANCED_FACE ( 'NONE', ( #39025 ), #49904, .T. ) ;
#2701 = VECTOR ( 'NONE', #8433, 1000.000000000000000 ) ;
#2702 = ORIENTED_EDGE ( 'NONE', *, *, #58656, .F. ) ;
#2704 = VECTOR ( 'NONE', #14100, 999.9999999999998863 ) ;
#2703 = SHAPE_DEFINITION_REPRESENTATION ( #64721, #45199 ) ;
#2705 = PLANE ( 'NONE',  #8270 ) ;
#2706 = CARTESIAN_POINT ( 'NONE',  ( -37.93379515072632557, 11.77251734620211643, -46.60018604761813066 ) ) ;
#2707 = FACE_OUTER_BOUND ( 'NONE', #53949, .T. ) ;
#2708 = CARTESIAN_POINT ( 'NONE',  ( 204.6977192012829789, -170.0000000000000000, 9.863170148305760776 ) ) ;
#2709 = ORIENTED_EDGE ( 'NONE', *, *, #35169, .F. ) ;
#2710 = CARTESIAN_POINT ( 'NONE',  ( 129.1310456962235094, 39.80382822048398594, 4.321560090366997287 ) ) ;
#2711 = CARTESIAN_POINT ( 'NONE',  ( -144.9287131874382055, 60.39056348581543432, -9.508616525343073889 ) ) ;
#2712 = CARTESIAN_POINT ( 'NONE',  ( 199.7286177451876199, 101.4075663537892211, 4.226501175219063100 ) ) ;
#2713 = EDGE_LOOP ( 'NONE', ( #26660, #62305, #27434, #31457 ) ) ;
#2714 = ADVANCED_FACE ( 'NONE', ( #37969 ), #53779, .T. ) ;
#2715 = CARTESIAN_POINT ( 'NONE',  ( 150.0309095590486663, 53.33084854625626292, 91.62168867483059387 ) ) ;
#2716 = ORIENTED_EDGE ( 'NONE', *, *, #45081, .F. ) ;
#2717 = CARTESIAN_POINT ( 'NONE',  ( 204.6977192012829789, 108.0580384837234931, 71.05227132923315025 ) ) ;
#2718 = DIRECTION ( 'NONE',  ( 1.000000000000000000, 0.000000000000000000, 0.000000000000000000 ) ) ;
#2719 = ADVANCED_FACE ( 'NONE', ( #1377 ), #48841, .F. ) ;
#2720 = LINE ( 'NONE', #3072, #17293 ) ;
#2721 = CARTESIAN_POINT ( 'NONE',  ( 23.28869764673362042, 6.856674305776598644, -42.53058434114498709 ) ) ;
#2722 = CARTESIAN_POINT ( 'NONE',  ( 84.73231936899556160, 18.78199960571076943, 3.095663364362381653 ) ) ;
#2724 = ORIENTED_EDGE ( 'NONE', *, *, #21371, .T. ) ;
#2723 = LINE ( 'NONE', #35425, #51095 ) ;
#2725 = CARTESIAN_POINT ( 'NONE',  ( -0.4996266546846081513, 7.531422798935177632, -95.00000000000133582 ) ) ;
#2726 = ORIENTED_EDGE ( 'NONE', *, *, #15157, .F. ) ;
#2727 = ORIENTED_EDGE ( 'NONE', *, *, #23656, .F. ) ;
#2728 = CARTESIAN_POINT ( 'NONE',  ( 173.9457771591584958, 73.05793967547529633, 34.48989055565348139 ) ) ;
#2729 = VECTOR ( 'NONE', #44518, 1000.000000000000000 ) ;
#2730 = CARTESIAN_POINT ( 'NONE',  ( -34.14504207561676452, 11.07284558078377579, -89.50818587954944405 ) ) ;
#2732 = ORIENTED_EDGE ( 'NONE', *, *, #31234, .T. ) ;
#2731 = CARTESIAN_POINT ( 'NONE',  ( -14.92860730136983527, 8.468845235798742266, -72.18242109116805239 ) ) ;
#2733 = CARTESIAN_POINT ( 'NONE',  ( -95.09829086201085602, 30.39089736475074943, 89.52221081825875615 ) ) ;
#2734 = CARTESIAN_POINT ( 'NONE',  ( -24.03640295269299898, 9.507963273819770578, 36.48715109637453224 ) ) ;
#2735 = FACE_BOUND ( 'NONE', #45270, .T. ) ;
#2736 = VECTOR ( 'NONE', #37672, 1000.000000000000000 ) ;
#2737 = VERTEX_POINT ( 'NONE', #59750 ) ;
#2738 = CARTESIAN_POINT ( 'NONE',  ( 174.6490316376289513, 73.72059609105147615, -93.55543838724517514 ) ) ;
#2739 = VECTOR ( 'NONE', #26466, 1000.000000000000000 ) ;
#2740 = AXIS2_PLACEMENT_3D ( 'NONE', #51849, #29706, #19145 ) ;
#2741 = CARTESIAN_POINT ( 'NONE',  ( 141.2361973397653401, 47.26569015399785911, 38.37501290123390874 ) ) ;
#2742 = B_SPLINE_CURVE_WITH_KNOTS ( 'NONE', 3,
 ( #61198, #28488, #45360, #12314, #6333, #17939, #49578, #18284, #23568, #22861, #34482, #60842, #65431, #7033, #49935, #66150, #13021, #11960 ),
 .UNSPECIFIED., .F., .F.,
 ( 4, 2, 2, 2, 2, 2, 2, 2, 4 ),
 ( 0.000000000000000000, 0.001486129123402290652, 0.002972258246804581304, 0.004458387370206871522, 0.005944516493609162608, 0.007430645617011453694, 0.008916774740413743044, 0.01040290386381603413, 0.01188903298721832522 ),
 .UNSPECIFIED. ) ;
#2743 = DIRECTION ( 'NONE',  ( -1.000000000000000000, 0.000000000000000000, 0.000000000000000000 ) ) ;
#2744 = AXIS2_PLACEMENT_3D ( 'NONE', #62058, #62417, #30069 ) ;
#2745 = CARTESIAN_POINT ( 'NONE',  ( 129.4887940973039804, 40.01039828304092794, 69.97058656504017904 ) ) ;
#2746 = CARTESIAN_POINT ( 'NONE',  ( -61.34830047412111043, 62.92641549729705019, 73.58025477438758344 ) ) ;
#2747 = ORIENTED_EDGE ( 'NONE', *, *, #46120, .F. ) ;
#2748 = ORIENTED_EDGE ( 'NONE', *, *, #4984, .T. ) ;
#2749 = ORIENTED_EDGE ( 'NONE', *, *, #60610, .F. ) ;
#2750 = DIRECTION ( 'NONE',  ( 0.000000000000000000, 0.5000000000000009992, 0.8660254037844380415 ) ) ;
#2751 = CARTESIAN_POINT ( 'NONE',  ( 444.9999999999999432, -35.00000000000000000, 380.0000000000000000 ) ) ;
#2752 = FACE_OUTER_BOUND ( 'NONE', #52532, .T. ) ;
#2753 = DIRECTION ( 'NONE',  ( 0.7530714660036195163, -0.6579387259397027066, 0.000000000000000000 ) ) ;
#2754 = CARTESIAN_POINT ( 'NONE',  ( -41.50537345350708307, 50.04124777106294886, 170.0000000000000000 ) ) ;
#2755 = FACE_BOUND ( 'NONE', #28802, .T. ) ;
#2756 = CARTESIAN_POINT ( 'NONE',  ( -71.86568654225717978, 20.91200104397924164, -18.94308595472579881 ) ) ;
#2757 = EDGE_LOOP ( 'NONE', ( #15220, #28245 ) ) ;
#2758 = CARTESIAN_POINT ( 'NONE',  ( -104.5740066103012254, 35.09687312794776659, 30.87461852538474005 ) ) ;
#2759 = ORIENTED_EDGE ( 'NONE', *, *, #7249, .T. ) ;
#2760 = CARTESIAN_POINT ( 'NONE',  ( 32.90878072717891456, 7.653588083204844850, 41.17538734954451485 ) ) ;
#2761 =( NAMED_UNIT ( * ) PLANE_ANGLE_UNIT ( ) SI_UNIT ( $, .RADIAN. ) );
#2762 = EDGE_LOOP ( 'NONE', ( #38333, #62039 ) ) ;
#2763 = CARTESIAN_POINT ( 'NONE',  ( 186.6118452967672283, 84.37814701615440072, 41.90269769157806934 ) ) ;
#2764 = FACE_OUTER_BOUND ( 'NONE', #14655, .T. ) ;
#2765 = CARTESIAN_POINT ( 'NONE',  ( 112.3013380801407095, 388.0000000000077307, 91.05029585798746439 ) ) ;
#2766 = CARTESIAN_POINT ( 'NONE',  ( 38.42384008295177722, 8.283891555743471358, 18.02114195686916176 ) ) ;
#2767 = CARTESIAN_POINT ( 'NONE',  ( -13.79190010541702627, 8.363435739308560102, -38.34741394315791752 ) ) ;
#2768 = CARTESIAN_POINT ( 'NONE',  ( 152.1190604254709910, 53.60705199010333644, -48.88494239191637547 ) ) ;
#2769 = ADVANCED_FACE ( 'NONE', ( #66123 ), #11563, .F. ) ;
#2770 = ORIENTED_EDGE ( 'NONE', *, *, #33124, .F. ) ;
#2771 = CARTESIAN_POINT ( 'NONE',  ( -452.6627218934912094, 399.9999999999998295, 113.5502958579882602 ) ) ;
#2772 = CARTESIAN_POINT ( 'NONE',  ( -156.9252506979472344, 70.73559306219775067, -16.61248648017295082 ) ) ;
#2773 = ORIENTED_EDGE ( 'NONE', *, *, #39637, .F. ) ;
#2774 = CARTESIAN_POINT ( 'NONE',  ( 444.9999999999999432, 225.0000000000000000, 2.000000000000000000 ) ) ;
#2775 = CARTESIAN_POINT ( 'NONE',  ( -62.41727141396690826, 17.83188754031766976, 66.14490890585253169 ) ) ;
#2776 = CYLINDRICAL_SURFACE ( 'NONE', #37568, 7.500000000000020428 ) ;
#2777 = ORIENTED_EDGE ( 'NONE', *, *, #40056, .F. ) ;
#2778 = CARTESIAN_POINT ( 'NONE',  ( 40.81683821231161602, -8.677580169988223346, 13.79046340968177731 ) ) ;
#2780 = EDGE_CURVE ( 'NONE', #47684, #28536, #39364, .T. ) ;
#2779 = CARTESIAN_POINT ( 'NONE',  ( 155.7167524447090727, 57.56687707799949294, -63.16317902508508553 ) ) ;
#2781 = CARTESIAN_POINT ( 'NONE',  ( -96.02415295709705845, 29.71480036090586907, -19.81432279787944140 ) ) ;
#2782 = CARTESIAN_POINT ( 'NONE',  ( 136.9934874058118055, 43.35050367224292955, -36.69511880788390812 ) ) ;
#2783 = VECTOR ( 'NONE', #29904, 1000.000000000000000 ) ;
#2784 = ADVANCED_FACE ( 'NONE', ( #326 ), #64702, .F. ) ;
#2785 = VERTEX_POINT ( 'NONE', #27754 ) ;
#2786 = EDGE_CURVE ( 'NONE', #2737, #32221, #49196, .T. ) ;
#2787 = DIRECTION ( 'NONE',  ( 1.000000000000000000, 0.000000000000000000, 0.000000000000000000 ) ) ;
#2788 = CARTESIAN_POINT ( 'NONE',  ( -56.55682214211910974, -14.31196067865754173, 27.58472315868180402 ) ) ;
#2789 = CARTESIAN_POINT ( 'NONE',  ( -31.11269837220801193, 31.11269837220812207, 2.000000000000001776 ) ) ;
#2790 = ORIENTED_EDGE ( 'NONE', *, *, #64406, .T. ) ;
#2791 = CARTESIAN_POINT ( 'NONE',  ( -452.6627218934913230, 399.9999999999997726, 78.55029585798818914 ) ) ;
#2792 = CARTESIAN_POINT ( 'NONE',  ( 186.2722199822850655, 84.01218714714246971, 15.40014518578409763 ) ) ;
#2793 = AXIS2_PLACEMENT_3D ( 'NONE', #21535, #48592, #64454 ) ;
#2794 = CARTESIAN_POINT ( 'NONE',  ( 126.4418792563097327, 38.27634703522673476, 89.51384704393026936 ) ) ;
#2795 = LINE ( 'NONE', #34812, #43672 ) ;
#2796 = VECTOR ( 'NONE', #29277, 1000.000000000000000 ) ;
#2797 = CARTESIAN_POINT ( 'NONE',  ( -50.00000000000001421, -20.00000000000000355, 2.000000000000015543 ) ) ;
#2798 = VECTOR ( 'NONE', #35005, 1000.000000000000000 ) ;
#2799 = ADVANCED_FACE ( 'NONE', ( #20237 ), #8332, .T. ) ;
#2800 = CARTESIAN_POINT ( 'NONE',  ( -124.9927180788553756, 45.90286323198616003, -61.79884557940761880 ) ) ;
#2801 = VERTEX_POINT ( 'NONE', #4074 ) ;
#2802 = CARTESIAN_POINT ( 'NONE',  ( 204.6977192012829789, -170.0000000000000000, -90.01503221354893469 ) ) ;
#2803 = CARTESIAN_POINT ( 'NONE',  ( 15.55634918610411610, 46.66904755831205875, 0.000000000000000000 ) ) ;
#2804 = CARTESIAN_POINT ( 'NONE',  ( 68.63487067129264574, 14.04635751989140502, 69.14883297453368982 ) ) ;
#2805 = CARTESIAN_POINT ( 'NONE',  ( 134.7708899521910837, 43.15864772107691749, 2.718175913858767778 ) ) ;
#2806 = CARTESIAN_POINT ( 'NONE',  ( 10.06749493632391967, 74.32123213259514216, 43.58025477438756212 ) ) ;
#2807 = ORIENTED_EDGE ( 'NONE', *, *, #46761, .T. ) ;
#2808 = LINE ( 'NONE', #13704, #47364 ) ;
#2809 = CYLINDRICAL_SURFACE ( 'NONE', #65443, 245.3095347406802773 ) ;
#2810 = ORIENTED_EDGE ( 'NONE', *, *, #43574, .F. ) ;
#2811 = CARTESIAN_POINT ( 'NONE',  ( 69.49112875363887554, 15.30845942322119591, 60.36544806545548880 ) ) ;
#2812 = CARTESIAN_POINT ( 'NONE',  ( 140.6983622512872785, 45.71183921003505191, 93.79223251056832567 ) ) ;
#2813 = ORIENTED_EDGE ( 'NONE', *, *, #33035, .F. ) ;
#2814 = CARTESIAN_POINT ( 'NONE',  ( 164.8444104055694481, 64.93678790243657772, -45.02061212871966944 ) ) ;
#2815 = DIRECTION ( 'NONE',  ( 1.000000000000000000, 0.000000000000000000, 0.000000000000000000 ) ) ;
#2816 = PLANE ( 'NONE',  #19313 ) ;
#2817 = CARTESIAN_POINT ( 'NONE',  ( 160.9069879467681119, 60.37290772564306707, -50.30662973681143768 ) ) ;
#2818 = ORIENTED_EDGE ( 'NONE', *, *, #1514, .F. ) ;
#2819 = CARTESIAN_POINT ( 'NONE',  ( -35.00000000000000000, -35.00000000000000000, 2.000000000000000000 ) ) ;
#2820 = FACE_OUTER_BOUND ( 'NONE', #53008, .T. ) ;
#2821 = DIRECTION ( 'NONE',  ( 0.000000000000000000, -1.000000000000000000, -0.000000000000000000 ) ) ;
#2822 = VECTOR ( 'NONE', #54617, 1000.000000000000000 ) ;
#2823 = CARTESIAN_POINT ( 'NONE',  ( 79.22872707466395070, 18.07970189365807201, -15.23444678155258103 ) ) ;
#2824 = CARTESIAN_POINT ( 'NONE',  ( -176.7403177620948895, 92.79785224917912956, -89.32883995899774732 ) ) ;
#2825 = CARTESIAN_POINT ( 'NONE',  ( -143.1937182229694656, 59.00378877849532699, -91.94668305751585535 ) ) ;
#2826 = CARTESIAN_POINT ( 'NONE',  ( 126.3541873520044305, 37.07520218256171773, -70.86737662479835365 ) ) ;
#2827 = ORIENTED_EDGE ( 'NONE', *, *, #13092, .F. ) ;
#2828 = CARTESIAN_POINT ( 'NONE',  ( -96.02159028238558847, 30.82695531378847775, 69.00396826126393535 ) ) ;
#2829 = CARTESIAN_POINT ( 'NONE',  ( -52.69240448066660321, 53.30312580971368419, 41.38025477438755928 ) ) ;
#2830 = ORIENTED_EDGE ( 'NONE', *, *, #17150, .T. ) ;
#2831 = AXIS2_PLACEMENT_3D ( 'NONE', #67732, #19884, #29741 ) ;
#2832 = CARTESIAN_POINT ( 'NONE',  ( -153.6946616617039183, 69.16142959008689672, -48.55193879071696017 ) ) ;
#2833 = PLANE ( 'NONE',  #68014 ) ;
#2834 = VECTOR ( 'NONE', #1264, 1000.000000000000000 ) ;
#2835 = AXIS2_PLACEMENT_3D ( 'NONE', #39813, #25639, #30556 ) ;
#2836 = DIRECTION ( 'NONE',  ( -1.000000000000000000, 0.000000000000000000, 0.000000000000000000 ) ) ;
#2837 = EDGE_CURVE ( 'NONE', #34252, #12488, #63161, .T. ) ;
#2838 = CARTESIAN_POINT ( 'NONE',  ( 412.3372781065085633, 219.4906275429376308, 111.5502958579881749 ) ) ;
#2839 = CARTESIAN_POINT ( 'NONE',  ( 183.2136430849848239, 0.000000000000000000, -14.43565316649556074 ) ) ;
#2840 =( GEOMETRIC_REPRESENTATION_CONTEXT ( 3 ) GLOBAL_UNCERTAINTY_ASSIGNED_CONTEXT ( ( #34628 ) ) GLOBAL_UNIT_ASSIGNED_CONTEXT ( ( #27587, #26214, #43758 ) ) REPRESENTATION_CONTEXT ( 'NONE', 'WORKASPACE' ) );
#2841 = CARTESIAN_POINT ( 'NONE',  ( -51.13073217147961458, 13.66490163179657635, -63.16339902663095529 ) ) ;
#2842 = CARTESIAN_POINT ( 'NONE',  ( 205.5004956747122264, 107.4493581495447785, -51.29378026339399810 ) ) ;
#2843 = CARTESIAN_POINT ( 'NONE',  ( 173.7246046907419839, 71.47482343504563573, 11.43823586838169426 ) ) ;
#2844 = CARTESIAN_POINT ( 'NONE',  ( -58.33245019990697244, 15.58496056636070293, 17.73516165329973759 ) ) ;
#2845 = VERTEX_POINT ( 'NONE', #14956 ) ;
#2847 = AXIS2_PLACEMENT_3D ( 'NONE', #55235, #19692, #19004 ) ;
#2846 = DIRECTION ( 'NONE',  ( 1.000000000000000000, 0.000000000000000000, 0.000000000000000000 ) ) ;
#2848 = ORIENTED_EDGE ( 'NONE', *, *, #52436, .F. ) ;
#2849 = CARTESIAN_POINT ( 'NONE',  ( 103.5839822277949764, 25.92130892112108853, -66.80704105902555057 ) ) ;
#2850 = CARTESIAN_POINT ( 'NONE',  ( 45.35146934743632841, 10.27620685439442028, -11.68218203743552586 ) ) ;
#2851 = CARTESIAN_POINT ( 'NONE',  ( 46.76970795284344717, 9.482505412758895247, 65.72351425996377827 ) ) ;
#2852 = DIRECTION ( 'NONE',  ( -0.000000000000000000, 1.000000000000000000, -0.000000000000000000 ) ) ;
#2853 = DIRECTION ( 'NONE',  ( -0.000000000000000000, -0.000000000000000000, -1.000000000000000000 ) ) ;
#2854 = CARTESIAN_POINT ( 'NONE',  ( 0.000000000000000000, 0.000000000000000000, 40.82842712474622004 ) ) ;
#2855 = CARTESIAN_POINT ( 'NONE',  ( 59.12362561977391096, 12.83186343420200970, -90.44545082695854887 ) ) ;
#2856 = CARTESIAN_POINT ( 'NONE',  ( -166.7068579965636843, 80.26142964949320913, 61.27046711184852512 ) ) ;
#2857 = VERTEX_POINT ( 'NONE', #66811 ) ;
#2858 = EDGE_LOOP ( 'NONE', ( #46250, #47296, #53615, #9063 ) ) ;
#2860 = ADVANCED_FACE ( 'NONE', ( #52591 ), #57538, .F. ) ;
#2859 = PLANE ( 'NONE',  #68017 ) ;
#2861 = DIRECTION ( 'NONE',  ( 1.000000000000000000, 0.000000000000000000, 0.000000000000000000 ) ) ;
#2862 = CARTESIAN_POINT ( 'NONE',  ( 177.7960900018544521, 75.34533826015461955, -10.13599328491967277 ) ) ;
#2863 = CARTESIAN_POINT ( 'NONE',  ( 102.7446498997619813, 26.65764321315729646, 63.41915715202346604 ) ) ;
#2864 = CARTESIAN_POINT ( 'NONE',  ( -20.55634918610403261, 5.000000000000028422, 85.00100000000000477 ) ) ;
#2865 = ADVANCED_FACE ( 'NONE', ( #24240 ), #28817, .F. ) ;
#2866 = PLANE ( 'NONE',  #1430 ) ;
#2867 = EDGE_LOOP ( 'NONE', ( #46115, #49842, #4255, #13345, #54855, #50718, #48598, #4064 ) ) ;
#2868 = CARTESIAN_POINT ( 'NONE',  ( -3.865535725358708596, -58.21137331173960661, 27.58472315868180402 ) ) ;
#2869 = CARTESIAN_POINT ( 'NONE',  ( -12.77647591501652791, 7.263973827022343954, 58.80487624720162643 ) ) ;
#2870 = CARTESIAN_POINT ( 'NONE',  ( -86.17927978631391284, 25.32700573188351001, -15.75888056856657471 ) ) ;
#2871 = CARTESIAN_POINT ( 'NONE',  ( 31.11269837220806522, -6.375108774214766072E-14, 0.000000000000000000 ) ) ;
#2872 = FACE_BOUND ( 'NONE', #12550, .T. ) ;
#2873 = AXIS2_PLACEMENT_3D ( 'NONE', #2658, #40623, #50495 ) ;
#2874 = B_SPLINE_CURVE_WITH_KNOTS ( 'NONE', 3,
 ( #17395, #12133, #33596, #6845, #44483, #65963, #17761, #7200, #50112, #63086, #9973, #8599, #30738, #68699, #46554, #40589, #14552, #25124, #36709, #67344, #14890, #36011, #19135, #57465, #35320, #62750, #57812, #19478, #36355, #47242, #68035, #62042, #13858, #31424, #9631, #52185, #41974, #62399, #9275, #63436, #40940, #20176, #14213, #35675 ),
 .UNSPECIFIED., .F., .F.,
 ( 4, 2, 2, 2, 2, 2, 2, 2, 2, 2, 2, 2, 2, 2, 2, 2, 2, 2, 2, 2, 2, 4 ),
 ( 0.02477387709520258163, 0.02633314402883776828, 0.02711277749565536854, 0.02789241096247296534, 0.02945167789610817627, 0.03023131136292576265, 0.03101094482974335251, 0.03257021176337856344, 0.03334984523019616370, 0.03412947869701375703, 0.03568874563064895755, 0.03646837909746653006, 0.03724801256428410257, 0.03802764603110168201, 0.03880727949791926146, 0.04036654643155440647, 0.04192581336518955148, 0.04348508029882469650, 0.04504434723245984151, 0.04660361416609498653, 0.04816288109973011766, 0.04972214803336524880 ),
 .UNSPECIFIED. ) ;
#2875 = EDGE_CURVE ( 'NONE', #42385, #61117, #18253, .T. ) ;
#2876 = ORIENTED_EDGE ( 'NONE', *, *, #29372, .T. ) ;
#2877 = ORIENTED_EDGE ( 'NONE', *, *, #26267, .F. ) ;
#2878 = DIRECTION ( 'NONE',  ( 0.000000000000000000, 0.000000000000000000, -1.000000000000000000 ) ) ;
#2879 = CARTESIAN_POINT ( 'NONE',  ( 432.4999999999999432, 207.5000000000000284, 0.000000000000000000 ) ) ;
#2880 = VECTOR ( 'NONE', #59830, 1000.000000000000000 ) ;
#2881 = CARTESIAN_POINT ( 'NONE',  ( -62.66631205405160188, -18.59153367093452758, 43.58025477438756212 ) ) ;
#2882 = LINE ( 'NONE', #63353, #38839 ) ;
#2883 = CARTESIAN_POINT ( 'NONE',  ( 8.290168341070513591, 6.376397093466350086, 91.57150589958799003 ) ) ;
#2884 = EDGE_CURVE ( 'NONE', #36808, #910, #34790, .T. ) ;
#2885 = CARTESIAN_POINT ( 'NONE',  ( 81.03898448521320574, 17.58847173596443625, -75.19045902363498612 ) ) ;
#2886 = AXIS2_PLACEMENT_3D ( 'NONE', #12370, #66210, #45064 ) ;
#2887 = VECTOR ( 'NONE', #14125, 1000.000000000000000 ) ;
#2888 = VERTEX_POINT ( 'NONE', #50960 ) ;
#2889 = AXIS2_PLACEMENT_3D ( 'NONE', #47748, #52683, #46726 ) ;
#2890 = LINE ( 'NONE', #34569, #25833 ) ;
#2891 = VECTOR ( 'NONE', #10003, 1000.000000000000000 ) ;
#2892 = CARTESIAN_POINT ( 'NONE',  ( 200.4590013143046292, 102.3556155835302945, -50.03054843160261811 ) ) ;
#2893 = VERTEX_POINT ( 'NONE', #68763 ) ;
#2894 = SHAPE_REPRESENTATION ( 'frame_Default<As Welded>', ( #66832 ), #12890 ) ;
#2895 = CARTESIAN_POINT ( 'NONE',  ( -7.825402957745087207, -170.0000000000000000, 18.27103044898354511 ) ) ;
#2896 = VERTEX_POINT ( 'NONE', #68432 ) ;
#2897 = AXIS2_PLACEMENT_3D ( 'NONE', #60259, #12078, #17706 ) ;
#2898 = CARTESIAN_POINT ( 'NONE',  ( -85.46258339457288855, 25.02772366257410752, -72.64209979375846160 ) ) ;
#2899 = DIRECTION ( 'NONE',  ( -0.000000000000000000, -0.000000000000000000, -1.000000000000000000 ) ) ;
#2900 = DIRECTION ( 'NONE',  ( -0.000000000000000000, -0.000000000000000000, -1.000000000000000000 ) ) ;
#2901 = ORIENTED_EDGE ( 'NONE', *, *, #42078, .F. ) ;
#2902 = ORIENTED_EDGE ( 'NONE', *, *, #54366, .F. ) ;
#2903 = CARTESIAN_POINT ( 'NONE',  ( 46.90208227351340042, 10.52324439420451263, 64.01647544768613329 ) ) ;
#2904 = CARTESIAN_POINT ( 'NONE',  ( -102.2801239173131052, 33.91021738430208643, -88.70367844590326456 ) ) ;
#2905 = CARTESIAN_POINT ( 'NONE',  ( 21.25987915030397701, 6.737472588634917159, 5.534856484934720378 ) ) ;
#2906 = VERTEX_POINT ( 'NONE', #2091 ) ;
#2907 = CARTESIAN_POINT ( 'NONE',  ( 178.1965488566140436, 77.14488558164481447, -77.50486268625550679 ) ) ;
#2908 = PLANE ( 'NONE',  #63965 ) ;
#2909 = LINE ( 'NONE', #51449, #54074 ) ;
#2910 = CARTESIAN_POINT ( 'NONE',  ( 80.15818551272214165, 18.36718314243333694, -39.49802388013461041 ) ) ;
#2912 = VERTEX_POINT ( 'NONE', #20576 ) ;
#2911 = CARTESIAN_POINT ( 'NONE',  ( 8.000000000000007105, 249.8719672152120381, -95.00000000000133582 ) ) ;
#2913 = ORIENTED_EDGE ( 'NONE', *, *, #469, .T. ) ;
#2914 = ORIENTED_EDGE ( 'NONE', *, *, #9847, .T. ) ;
#2915 = CARTESIAN_POINT ( 'NONE',  ( 46.13856685535759539, 9.381502944822527112, 13.90276314609397268 ) ) ;
#2916 = DIRECTION ( 'NONE',  ( -0.000000000000000000, 1.000000000000000000, -0.000000000000000000 ) ) ;
#2917 = CARTESIAN_POINT ( 'NONE',  ( -49.11825192196926082, 13.17012322555987325, -11.25932645589339565 ) ) ;
#2918 = EDGE_CURVE ( 'NONE', #60277, #49052, #10721, .T. ) ;
#2919 = CARTESIAN_POINT ( 'NONE',  ( 109.3047266816501377, 28.44977739115299542, -24.03376987702539225 ) ) ;
#2920 = CARTESIAN_POINT ( 'NONE',  ( 198.7029050523552485, 98.46895521196213963, 14.39901884897147788 ) ) ;
#2921 = CARTESIAN_POINT ( 'NONE',  ( -5.767955557622883589E-14, -26.11269837220806522, 0.000000000000000000 ) ) ;
#2922 = CARTESIAN_POINT ( 'NONE',  ( 207.5555325562649500, 112.1057321206939292, 83.44071583484532084 ) ) ;
#2923 = LINE ( 'NONE', #41930, #52350 ) ;
#2924 = DIRECTION ( 'NONE',  ( 1.000000000000000000, 0.000000000000000000, 0.000000000000000000 ) ) ;
#2925 = CARTESIAN_POINT ( 'NONE',  ( -450.6627218934913230, 217.8591479523843475, 78.55029585798814651 ) ) ;
#2927 = ORIENTED_EDGE ( 'NONE', *, *, #30408, .T. ) ;
#2926 = EDGE_CURVE ( 'NONE', #61056, #43813, #64883, .T. ) ;
#2928 = AXIS2_PLACEMENT_3D ( 'NONE', #57417, #46861, #14505 ) ;
#2929 = CARTESIAN_POINT ( 'NONE',  ( 15.78827728214693416, 7.507518794609588042, -23.67439350822212774 ) ) ;
#2930 = ORIENTED_EDGE ( 'NONE', *, *, #52098, .F. ) ;
#2931 = ORIENTED_EDGE ( 'NONE', *, *, #21135, .T. ) ;
#2932 = CARTESIAN_POINT ( 'NONE',  ( -17.50000000000000000, 207.5000000000000284, 20.00000000000000000 ) ) ;
#2933 = CIRCLE ( 'NONE', #64677, 242.4895526022646379 ) ;
#2934 = CARTESIAN_POINT ( 'NONE',  ( 188.2962140587030149, 87.71627202537840162, -72.64852955523822686 ) ) ;
#2935 = CARTESIAN_POINT ( 'NONE',  ( -165.6404838346739439, 80.60836113891892296, 38.93951364949523253 ) ) ;
#2936 = CARTESIAN_POINT ( 'NONE',  ( -94.77925136849377452, 29.13093715379786630, -42.28272860464903005 ) ) ;
#2937 = AXIS2_PLACEMENT_3D ( 'NONE', #60307, #49735, #55372 ) ;
#2938 = VECTOR ( 'NONE', #32124, 1000.000000000000000 ) ;
#2939 = CARTESIAN_POINT ( 'NONE',  ( -24.32776401346967887, 9.546905915310563984, 13.30497887696894210 ) ) ;
#2940 = CARTESIAN_POINT ( 'NONE',  ( 9.737557066527559257, 192.0000000000000000, 2.275957463600584596 ) ) ;
#2941 = CARTESIAN_POINT ( 'NONE',  ( 9.275903038161098735, 7.385619229189525292, -39.26677353779081159 ) ) ;
#2942 = AXIS2_PLACEMENT_3D ( 'NONE', #62210, #51241, #12213 ) ;
#2943 = CARTESIAN_POINT ( 'NONE',  ( 130.3019683985926349, 39.31883119822049366, -50.14450225213496992 ) ) ;
#2944 = ORIENTED_EDGE ( 'NONE', *, *, #30928, .T. ) ;
#2945 = EDGE_CURVE ( 'NONE', #18983, #62629, #43058, .T. ) ;
#2946 = ORIENTED_EDGE ( 'NONE', *, *, #38816, .F. ) ;
#2947 = AXIS2_PLACEMENT_3D ( 'NONE', #10243, #42268, #36303 ) ;
#2948 = EDGE_CURVE ( 'NONE', #44967, #17356, #65568, .T. ) ;
#2949 = CARTESIAN_POINT ( 'NONE',  ( 188.1640390495057602, 87.56943377085097779, 88.01576467520247604 ) ) ;
#2950 = CARTESIAN_POINT ( 'NONE',  ( -13.47680110791657349, 7.324966777230637049, 5.815555111528495580 ) ) ;
#2951 = CARTESIAN_POINT ( 'NONE',  ( 64.97411640938653932, -37.36411256620218069, 41.38025477438755928 ) ) ;
#2952 = CARTESIAN_POINT ( 'NONE',  ( -29.49620345460276027, 9.280093073089044964, -62.40110739915159144 ) ) ;
#2953 = EDGE_CURVE ( 'NONE', #6937, #46890, #35233, .T. ) ;
#2954 = UNCERTAINTY_MEASURE_WITH_UNIT (LENGTH_MEASURE( 1.000000000000000082E-05 ), #13188, 'distance_accuracy_value', 'NONE');
#2955 = EDGE_CURVE ( 'NONE', #36796, #51074, #58217, .T. ) ;
#2956 = CARTESIAN_POINT ( 'NONE',  ( -439.4229916354183274, 400.0000000000064801, 96.05029585798874336 ) ) ;
#2957 = VERTEX_POINT ( 'NONE', #32182 ) ;
#2958 = CARTESIAN_POINT ( 'NONE',  ( 437.3372781065085633, 390.0000000000001137, -146.4497041420117966 ) ) ;
#2959 = CARTESIAN_POINT ( 'NONE',  ( -61.10880364359507411, 17.43879918625640357, -73.99209842384989599 ) ) ;
#2960 = CARTESIAN_POINT ( 'NONE',  ( 200.4574930424075490, 102.3536505870638393, -64.46692893376646794 ) ) ;
#2961 = CARTESIAN_POINT ( 'NONE',  ( -175.9852529046322616, 90.37283472601130541, -35.26747372587856688 ) ) ;
#2962 = CARTESIAN_POINT ( 'NONE',  ( 105.4193882736796155, 26.71329717705294726, 4.502293189513017602 ) ) ;
#2963 = LINE ( 'NONE', #57118, #66829 ) ;
#2964 = DIRECTION ( 'NONE',  ( -0.000000000000000000, -0.000000000000000000, -1.000000000000000000 ) ) ;
#2965 = CARTESIAN_POINT ( 'NONE',  ( -52.68007207639879397, 14.05813534436550327, 57.54295262752664541 ) ) ;
#2966 = ADVANCED_FACE ( 'NONE', ( #16340 ), #20929, .F. ) ;
#2967 = CARTESIAN_POINT ( 'NONE',  ( -0.3734056954813063101, 6.520221844775928588, 65.43821756026045477 ) ) ;
#2968 = ORIENTED_EDGE ( 'NONE', *, *, #54046, .T. ) ;
#2969 = CARTESIAN_POINT ( 'NONE',  ( 279.3426986656771760, 21.43197803755064967, 4.967354168418942173 ) ) ;
#2970 = CARTESIAN_POINT ( 'NONE',  ( 156.3797504404255960, 58.07856685387021400, 56.33044317893267561 ) ) ;
#2971 = CARTESIAN_POINT ( 'NONE',  ( 5.799999999999999822, 8.000000000000000000, 0.000000000000000000 ) ) ;
#2972 = CARTESIAN_POINT ( 'NONE',  ( -50.13771638889890880, 13.41835215703894413, -37.03013167601228162 ) ) ;
#2973 = ADVANCED_FACE ( 'NONE', ( #69104 ), #47989, .F. ) ;
#2974 = DIRECTION ( 'NONE',  ( -1.000000000000000000, 0.000000000000000000, 0.000000000000000000 ) ) ;
#2975 = EDGE_CURVE ( 'NONE', #60490, #50015, #69523, .T. ) ;
#2976 = DIRECTION ( 'NONE',  ( 0.000000000000000000, -0.000000000000000000, -1.000000000000000000 ) ) ;
#2977 = EDGE_CURVE ( 'NONE', #2404, #30106, #39541, .T. ) ;
#2978 = ORIENTED_EDGE ( 'NONE', *, *, #21048, .T. ) ;
#2979 = DIRECTION ( 'NONE',  ( -1.387778780781445922E-16, 1.000000000000000000, 1.232595164407830946E-32 ) ) ;
#2980 = DIRECTION ( 'NONE',  ( 9.729495617646301779E-15, -5.551115123125782702E-17, 1.000000000000000000 ) ) ;
#2981 = EDGE_LOOP ( 'NONE', ( #13147, #27199, #10225, #40250 ) ) ;
#2982 = VECTOR ( 'NONE', #47038, 1000.000000000000000 ) ;
#2983 = ORIENTED_EDGE ( 'NONE', *, *, #34114, .F. ) ;
#2984 = CARTESIAN_POINT ( 'NONE',  ( -7.825402957745087207, -170.0000000000000000, 10.77103044898353090 ) ) ;
#2985 = DIRECTION ( 'NONE',  ( -1.000000000000000000, 0.000000000000000000, 0.000000000000000000 ) ) ;
#2986 = LINE ( 'NONE', #66329, #33613 ) ;
#2987 = ORIENTED_EDGE ( 'NONE', *, *, #39684, .T. ) ;
#2988 = CARTESIAN_POINT ( 'NONE',  ( 7.484861546145933353, -64.56761454192826477, 40.00000000000003553 ) ) ;
#2989 = CONICAL_SURFACE ( 'NONE', #27665, 74.95140232871122521, 0.8777644062502172329 ) ;
#2990 = CARTESIAN_POINT ( 'NONE',  ( -180.0179082103088319, 95.14811732286301549, 14.43829403818141444 ) ) ;
#2991 = CARTESIAN_POINT ( 'NONE',  ( -4.070918861171930914, 6.675509947362630925, 17.26827648209658506 ) ) ;
#2992 = CARTESIAN_POINT ( 'NONE',  ( 59.73312635112155533, 12.96464920523511388, -49.98156322790594430 ) ) ;
#2993 = LINE ( 'NONE', #45893, #29240 ) ;
#2994 = CARTESIAN_POINT ( 'NONE',  ( -1.313474075707242950, -8.479269695850868871, -0.3167204509598467999 ) ) ;
#2995 = CARTESIAN_POINT ( 'NONE',  ( 141.3707934840545022, 46.15056991286792965, 10.13612274068955443 ) ) ;
#2996 = CARTESIAN_POINT ( 'NONE',  ( 205.5105258529713694, 107.4632495673648549, 44.17461234944981641 ) ) ;
#2997 = ORIENTED_EDGE ( 'NONE', *, *, #22900, .T. ) ;
#2998 = CARTESIAN_POINT ( 'NONE',  ( 46.66904755831207297, -15.55634918610412853, 85.00100000000000477 ) ) ;
#2999 = AXIS2_PLACEMENT_3D ( 'NONE', #53087, #48837, #21109 ) ;
#3000 = DIRECTION ( 'NONE',  ( -1.261617073437677999E-16, 0.000000000000000000, -1.000000000000000000 ) ) ;
#3001 = LINE ( 'NONE', #61038, #52882 ) ;
#3002 = CARTESIAN_POINT ( 'NONE',  ( -71.46567093091299228, 20.77283810584936319, 93.80455591633044321 ) ) ;
#3004 = ORIENTED_EDGE ( 'NONE', *, *, #29144, .F. ) ;
#3003 = DIRECTION ( 'NONE',  ( 0.000000000000000000, -1.000000000000000000, 0.000000000000000000 ) ) ;
#3005 = CARTESIAN_POINT ( 'NONE',  ( 0.000000000000000000, 0.000000000000000000, 170.0000000000000000 ) ) ;
#3006 = ORIENTED_EDGE ( 'NONE', *, *, #12801, .T. ) ;
#3007 = CARTESIAN_POINT ( 'NONE',  ( -142.0081215801270389, 58.07066293384868061, 64.76555490188158615 ) ) ;
#3008 = LINE ( 'NONE', #45911, #69307 ) ;
#3009 = CARTESIAN_POINT ( 'NONE',  ( 44.99999999999995737, 25.00000000000000000, 1.999999999999984457 ) ) ;
#3010 = CARTESIAN_POINT ( 'NONE',  ( 188.5837490358996149, 86.53279111916964439, -17.19126881223536785 ) ) ;
#3011 = DIRECTION ( 'NONE',  ( -1.000000000000000000, 0.000000000000000000, 0.000000000000000000 ) ) ;
#3012 = CARTESIAN_POINT ( 'NONE',  ( -80.54915509118116290, 24.12810583352864313, -23.03467912020122554 ) ) ;
#3013 = CARTESIAN_POINT ( 'NONE',  ( -180.6215424137752166, 97.48070480470863686, -15.06146349129376638 ) ) ;
#3014 = EDGE_CURVE ( 'NONE', #26941, #30210, #39202, .T. ) ;
#3015 = CARTESIAN_POINT ( 'NONE',  ( -47.55316895016325418, 13.83165595246916979, 38.31999599868878192 ) ) ;
#3016 = VERTEX_POINT ( 'NONE', #7885 ) ;
#3017 = ORIENTED_EDGE ( 'NONE', *, *, #44711, .T. ) ;
#3018 = DIRECTION ( 'NONE',  ( -0.000000000000000000, -0.000000000000000000, -1.000000000000000000 ) ) ;
#3019 = DIRECTION ( 'NONE',  ( 1.000000000000000000, 0.000000000000000000, -0.000000000000000000 ) ) ;
#3020 = CARTESIAN_POINT ( 'NONE',  ( 163.7464701930790909, 62.69993100427430477, 59.61700847725186492 ) ) ;
#3021 = CARTESIAN_POINT ( 'NONE',  ( -173.1211646369891355, -170.0000000000000000, 65.16624519710472896 ) ) ;
#3022 = CARTESIAN_POINT ( 'NONE',  ( 184.3941060377211727, 82.01604625189463604, -50.46965181017390023 ) ) ;
#3023 = DIRECTION ( 'NONE',  ( 0.000000000000000000, 0.000000000000000000, 1.000000000000000000 ) ) ;
#3024 = CARTESIAN_POINT ( 'NONE',  ( 158.3604774538084712, 58.34594647925806754, -63.00838262857361372 ) ) ;
#3025 = VERTEX_POINT ( 'NONE', #49725 ) ;
#3026 = EDGE_CURVE ( 'NONE', #34992, #7668, #60298, .T. ) ;
#3027 = PRODUCT_DEFINITION_SHAPE ( 'NONE', 'NONE',  #69576 ) ;
#3028 = ORIENTED_EDGE ( 'NONE', *, *, #67045, .F. ) ;
#3029 = EDGE_CURVE ( 'NONE', #41495, #19589, #60995, .T. ) ;
#3030 = ORIENTED_EDGE ( 'NONE', *, *, #19041, .F. ) ;
#3031 = EDGE_CURVE ( 'NONE', #1172, #21805, #34299, .T. ) ;
#3032 = VECTOR ( 'NONE', #4571, 1000.000000000000000 ) ;
#3033 = CARTESIAN_POINT ( 'NONE',  ( -7.825402957745085430, 7.899365992529246761, 71.96013162991091860 ) ) ;
#3034 = CARTESIAN_POINT ( 'NONE',  ( 175.1402005715378891, 72.80033409921840359, -92.83546321808604773 ) ) ;
#3035 = CARTESIAN_POINT ( 'NONE',  ( 63.49940197359695304, 12.78497925206076502, -50.72069083216975827 ) ) ;
#3036 = CARTESIAN_POINT ( 'NONE',  ( 108.7032261419851977, -21.46110313769845135, -4.839973237437577680 ) ) ;
#3037 = ADVANCED_FACE ( 'NONE', ( #44100 ), #56068, .T. ) ;
#3038 = AXIS2_PLACEMENT_3D ( 'NONE', #5533, #54754, #23111 ) ;
#3039 = CARTESIAN_POINT ( 'NONE',  ( -62.15063206372445137, 17.75106610013994057, 35.34437635207743966 ) ) ;
#3040 = CARTESIAN_POINT ( 'NONE',  ( -97.49665543375859045, 31.53324358035374075, -9.872370814404565209 ) ) ;
#3041 = ADVANCED_FACE ( 'NONE', ( #27935 ), #22661, .F. ) ;
#3042 = CARTESIAN_POINT ( 'NONE',  ( 38.90894112122322213, 8.345444037631242651, 71.75838489642697482 ) ) ;
#3043 = DIRECTION ( 'NONE',  ( -0.000000000000000000, -0.000000000000000000, -1.000000000000000000 ) ) ;
#3044 = EDGE_LOOP ( 'NONE', ( #2914, #25695, #29990, #1660 ) ) ;
#3045 = AXIS2_PLACEMENT_3D ( 'NONE', #12113, #49371, #37184 ) ;
#3046 = CARTESIAN_POINT ( 'NONE',  ( 73.95984195137799588, -12.15131637179793955, 41.38025477438755928 ) ) ;
#3047 = FACE_OUTER_BOUND ( 'NONE', #41666, .T. ) ;
#3048 = CARTESIAN_POINT ( 'NONE',  ( -189.2352924136013144, 107.0839554967701019, -42.55778393734637177 ) ) ;
#3049 = DIRECTION ( 'NONE',  ( -0.8584487936018655452, -0.5128992774059070170, 0.000000000000000000 ) ) ;
#3050 = LINE ( 'NONE', #24157, #28594 ) ;
#3051 = CARTESIAN_POINT ( 'NONE',  ( 18.19858669090299941, 7.596860100017451600, -9.067989001026109719 ) ) ;
#3052 = CARTESIAN_POINT ( 'NONE',  ( 197.5334904971816457, 97.00846725096931777, 65.79350108939836161 ) ) ;
#3053 = AXIS2_PLACEMENT_3D ( 'NONE', #38989, #1697, #38628 ) ;
#3054 = VERTEX_POINT ( 'NONE', #12118 ) ;
#3055 = PRODUCT_CONTEXT ( 'NONE', #2208, 'mechanical' ) ;
#3056 = CARTESIAN_POINT ( 'NONE',  ( 6.400000000000000355, 9.237604307034018802, 0.000000000000000000 ) ) ;
#3057 = PLANE ( 'NONE',  #30957 ) ;
#3058 = EDGE_CURVE ( 'NONE', #60812, #57773, #58704, .T. ) ;
#3059 = CARTESIAN_POINT ( 'NONE',  ( 0.1306530452038120182, -7.903938623646872941, -2.309976723937608334 ) ) ;
#3060 = CARTESIAN_POINT ( 'NONE',  ( -175.7433116402202700, 90.09372610121394587, 84.96528934235752217 ) ) ;
#3061 = ORIENTED_EDGE ( 'NONE', *, *, #6840, .F. ) ;
#3062 = CARTESIAN_POINT ( 'NONE',  ( 127.2358066117906503, 38.72257733469227503, 6.605040416640627576 ) ) ;
#3063 = EDGE_LOOP ( 'NONE', ( #65576, #48668, #15693, #29611 ) ) ;
#3064 = EDGE_CURVE ( 'NONE', #32859, #9244, #55362, .T. ) ;
#3065 = CARTESIAN_POINT ( 'NONE',  ( -143.3925773749111556, 59.16144459815140522, -11.11823926598882650 ) ) ;
#3066 = CARTESIAN_POINT ( 'NONE',  ( 203.9228889538744909, 106.9879579748728418, 2.392848837412264285 ) ) ;
#3067 = VERTEX_POINT ( 'NONE', #28640 ) ;
#3068 = CARTESIAN_POINT ( 'NONE',  ( 155.1915247301153045, 57.16500775723477545, 83.44643162593852992 ) ) ;
#3069 = EDGE_LOOP ( 'NONE', ( #53736, #43448 ) ) ;
#3070 = CARTESIAN_POINT ( 'NONE',  ( -62.49137879463567202, 17.85440472148629354, 11.96262358591842734 ) ) ;
#3071 = DIRECTION ( 'NONE',  ( 1.000000000000000000, 0.000000000000000000, 0.000000000000000000 ) ) ;
#3072 = CARTESIAN_POINT ( 'NONE',  ( -3.306248862503413655, 500.0000000000000000, -91.64566090791306863 ) ) ;
#3073 = LINE ( 'NONE', #24536, #42722 ) ;
#3074 = LINE ( 'NONE', #56888, #2442 ) ;
#3076 = ORIENTED_EDGE ( 'NONE', *, *, #18911, .F. ) ;
#3075 = CARTESIAN_POINT ( 'NONE',  ( 0.000000000000000000, 6.928203230275505220, -4.000000000000007994 ) ) ;
#3077 = VECTOR ( 'NONE', #52022, 1000.000000000000000 ) ;
#3078 = CARTESIAN_POINT ( 'NONE',  ( 55.51597771111714508, 11.05737652677076177, 37.81267142505173240 ) ) ;
#3079 = ORIENTED_EDGE ( 'NONE', *, *, #67167, .T. ) ;
#3080 = ORIENTED_EDGE ( 'NONE', *, *, #68526, .T. ) ;
#3081 = AXIS2_PLACEMENT_3D ( 'NONE', #1029, #66114, #17904 ) ;
#3082 = CARTESIAN_POINT ( 'NONE',  ( -169.8972248494843029, 85.08697738648012887, 18.26369148981731882 ) ) ;
#3083 = CARTESIAN_POINT ( 'NONE',  ( 16.27765348919936983, 6.516472002017811960, -77.36349468914950478 ) ) ;
#3084 = CIRCLE ( 'NONE', #66010, 5.000000000000000000 ) ;
#3086 = ORIENTED_EDGE ( 'NONE', *, *, #62668, .F. ) ;
#3085 = FACE_OUTER_BOUND ( 'NONE', #4736, .T. ) ;
#3087 = CARTESIAN_POINT ( 'NONE',  ( -98.33967698037261584, 31.94276620606871475, 85.31931532774478910 ) ) ;
#3088 = CARTESIAN_POINT ( 'NONE',  ( -77.71490760329793090, 23.03637365463981013, -50.07002586140477263 ) ) ;
#3089 = CIRCLE ( 'NONE', #50229, 8.000000000000000000 ) ;
#3090 = ORIENTED_EDGE ( 'NONE', *, *, #38328, .F. ) ;
#3091 = AXIS2_PLACEMENT_3D ( 'NONE', #61680, #34958, #66297 ) ;
#3092 = CARTESIAN_POINT ( 'NONE',  ( 212.0075063341773784, 118.7912820769029594, -72.37935731155032215 ) ) ;
#3093 = ADVANCED_FACE ( 'NONE', ( #8228 ), #9260, .F. ) ;
#3094 = AXIS2_PLACEMENT_3D ( 'NONE', #16311, #33194, #481 ) ;
#3095 = CARTESIAN_POINT ( 'NONE',  ( 138.5684226926155418, 45.53585076428272771, 42.86542189636780620 ) ) ;
#3096 = EDGE_CURVE ( 'NONE', #32147, #11742, #65456, .T. ) ;
#3097 = DIRECTION ( 'NONE',  ( 1.000000000000000000, 0.000000000000000000, 0.000000000000000000 ) ) ;
#3098 = CARTESIAN_POINT ( 'NONE',  ( -128.7724923851857000, 49.63576597317771189, 18.20476702891221521 ) ) ;
#3099 = CARTESIAN_POINT ( 'NONE',  ( 181.0840389613909736, 80.03940679743418229, -63.06960825634327961 ) ) ;
#3100 = ORIENTED_EDGE ( 'NONE', *, *, #817, .T. ) ;
#3101 = EDGE_LOOP ( 'NONE', ( #24985, #13574, #25623 ) ) ;
#3102 = CARTESIAN_POINT ( 'NONE',  ( -144.9417090887490644, 61.69631066549398213, -21.42304724940910532 ) ) ;
#3103 = DIRECTION ( 'NONE',  ( 0.000000000000000000, 1.000000000000000000, 0.000000000000000000 ) ) ;
#3104 = FACE_OUTER_BOUND ( 'NONE', #8174, .T. ) ;
#3105 = CARTESIAN_POINT ( 'NONE',  ( -51.19577760053109472, 14.71865550854504257, -89.96963771126178244 ) ) ;
#3106 = CARTESIAN_POINT ( 'NONE',  ( -37.04655464516766727, -53.85410457537912521, 6.377659838150125914E-18 ) ) ;
#3107 = CARTESIAN_POINT ( 'NONE',  ( -146.5341851369306312, 61.69744206542953435, 31.32122742849548303 ) ) ;
#3108 = CARTESIAN_POINT ( 'NONE',  ( -123.0348077379026961, 45.83489305753316501, 45.05744747576095222 ) ) ;
#3109 = CARTESIAN_POINT ( 'NONE',  ( -167.9889421625799741, 81.59140042431229745, -74.54592677586461491 ) ) ;
#3110 = EDGE_CURVE ( 'NONE', #61225, #18664, #27538, .T. ) ;
#3111 = VERTEX_POINT ( 'NONE', #13507 ) ;
#3112 = CARTESIAN_POINT ( 'NONE',  ( -105.8879245385188455, 35.79035667534149923, 44.61188123920754833 ) ) ;
#3113 = VERTEX_POINT ( 'NONE', #34963 ) ;
#3114 = CARTESIAN_POINT ( 'NONE',  ( -38.87848244732136749, 10.93141945332450327, 9.888487578027829628 ) ) ;
#3115 = CARTESIAN_POINT ( 'NONE',  ( 81.76212856587194722, 18.87332718082995342, 58.34523743138716867 ) ) ;
#3116 = ADVANCED_FACE ( 'NONE', ( #51138 ), #14198, .T. ) ;
#3117 = ORIENTED_EDGE ( 'NONE', *, *, #29794, .F. ) ;
#3118 = CARTESIAN_POINT ( 'NONE',  ( 2.999999999999992450, 0.000000000000000000, 0.000000000000000000 ) ) ;
#3119 = CARTESIAN_POINT ( 'NONE',  ( 21.57182537987934978, 17.67134260003773960, -35.17198294190094288 ) ) ;
#3120 = CARTESIAN_POINT ( 'NONE',  ( -452.6627218934918346, 365.0000000000064233, -146.4497041420121377 ) ) ;
#3121 = EDGE_CURVE ( 'NONE', #10742, #65175, #4948, .T. ) ;
#3122 =( NAMED_UNIT ( * ) PLANE_ANGLE_UNIT ( ) SI_UNIT ( $, .RADIAN. ) );
#3123 = CARTESIAN_POINT ( 'NONE',  ( 34.84173759613683075, 7.859847277726518477, 16.54372376058861605 ) ) ;
#3124 = CARTESIAN_POINT ( 'NONE',  ( -13.92109095214680181, 8.375243258322926820, -47.29446107485116357 ) ) ;
#3125 = CARTESIAN_POINT ( 'NONE',  ( 44.99999999999999289, -20.00000000000000355, 0.000000000000000000 ) ) ;
#3126 = EDGE_LOOP ( 'NONE', ( #63304, #38150 ) ) ;
#3127 = VECTOR ( 'NONE', #17134, 1000.000000000000000 ) ;
#3128 = CARTESIAN_POINT ( 'NONE',  ( -16.68907004672388084, 73.11959341363670717, 0.000000000000000000 ) ) ;
#3129 = VERTEX_POINT ( 'NONE', #8923 ) ;
#3130 = LINE ( 'NONE', #4162, #38433 ) ;
#3131 = DIRECTION ( 'NONE',  ( 0.6234898018587318180, 0.7818314824680311359, 0.000000000000000000 ) ) ;
#3132 = LINE ( 'NONE', #61171, #3890 ) ;
#3133 = ORIENTED_EDGE ( 'NONE', *, *, #33675, .T. ) ;
#3134 = B_SPLINE_CURVE_WITH_KNOTS ( 'NONE', 3,
 ( #16768, #10451, #59668, #21356, #53703, #11481 ),
 .UNSPECIFIED., .F., .F.,
 ( 4, 2, 4 ),
 ( 0.03218947840871073246, 0.06469842185262329737, 0.09720736529653584146 ),
 .UNSPECIFIED. ) ;
#3135 = LINE ( 'NONE', #24596, #1938 ) ;
#3136 = CARTESIAN_POINT ( 'NONE',  ( -56.53161132927532861, 15.08292330397246594, -89.04960089425232184 ) ) ;
#3137 = DIRECTION ( 'NONE',  ( 1.000000000000000000, 0.000000000000000000, 0.000000000000000000 ) ) ;
#3138 = AXIS2_PLACEMENT_3D ( 'NONE', #31491, #3714, #68434 ) ;
#3139 = DIRECTION ( 'NONE',  ( -1.000000000000000000, 0.000000000000000000, 0.000000000000000000 ) ) ;
#3140 = APPLICATION_CONTEXT ( 'automotive_design' ) ;
#3141 = AXIS2_PLACEMENT_3D ( 'NONE', #68861, #20685, #1657 ) ;
#3142 = ORIENTED_EDGE ( 'NONE', *, *, #54067, .T. ) ;
#3143 =( LENGTH_UNIT ( ) NAMED_UNIT ( * ) SI_UNIT ( .MILLI., .METRE. ) );
#3144 = CARTESIAN_POINT ( 'NONE',  ( -149.5074843970971017, 65.50121172469319220, 57.56537183036274286 ) ) ;
#3145 = CARTESIAN_POINT ( 'NONE',  ( -118.6849742182704972, 41.92701402439728042, 40.20636930516527485 ) ) ;
#3146 = AXIS2_PLACEMENT_3D ( 'NONE', #50401, #40193, #18044 ) ;
#3147 = CARTESIAN_POINT ( 'NONE',  ( -61.39252081892700375, 16.47343302442958546, -46.73105210731662851 ) ) ;
#3148 = ORIENTED_EDGE ( 'NONE', *, *, #20639, .T. ) ;
#3149 = CARTESIAN_POINT ( 'NONE',  ( -179.2210908201801374, 95.76260491022615895, -64.66443386884608913 ) ) ;
#3150 = CARTESIAN_POINT ( 'NONE',  ( 132.6781767539480654, 41.88870008768979147, 83.26602666350336790 ) ) ;
#3151 = ADVANCED_FACE ( 'NONE', ( #51491 ), #25107, .T. ) ;
#3152 = CARTESIAN_POINT ( 'NONE',  ( 117.6916924104495479, 32.48309187151382105, 38.12703603328098012 ) ) ;
#3153 = CONICAL_SURFACE ( 'NONE', #46918, 74.95140232871122521, 0.8777644062502172329 ) ;
#3154 = DIRECTION ( 'NONE',  ( -0.000000000000000000, -0.000000000000000000, -1.000000000000000000 ) ) ;
#3155 = ORIENTED_EDGE ( 'NONE', *, *, #17216, .F. ) ;
#3156 = DIRECTION ( 'NONE',  ( -0.000000000000000000, 1.000000000000000000, -0.000000000000000000 ) ) ;
#3157 = DIRECTION ( 'NONE',  ( 0.000000000000000000, 1.000000000000000000, 0.000000000000000000 ) ) ;
#3158 = CARTESIAN_POINT ( 'NONE',  ( 66.30567821786758032, 13.45988234822862317, 70.90175730764632078 ) ) ;
#3159 = CARTESIAN_POINT ( 'NONE',  ( 182.8363374612695793, 80.39432370332461630, -90.11314248946574423 ) ) ;
#3160 = CARTESIAN_POINT ( 'NONE',  ( 0.000000000000000000, 0.000000000000000000, 40.00000000000003553 ) ) ;
#3161 = VERTEX_POINT ( 'NONE', #9956 ) ;
#3162 = CARTESIAN_POINT ( 'NONE',  ( -31.43908319763710679, -170.0000000000000000, 57.06100499665286208 ) ) ;
#3163 = ORIENTED_EDGE ( 'NONE', *, *, #53873, .F. ) ;
#3164 = CARTESIAN_POINT ( 'NONE',  ( 181.0840389613909736, -170.0000000000000000, 36.80859410551140343 ) ) ;
#3165 = CARTESIAN_POINT ( 'NONE',  ( 138.0718262224615103, 44.02755351423877528, 84.46378310921993204 ) ) ;
#3167 = ORIENTED_EDGE ( 'NONE', *, *, #33592, .T. ) ;
#3166 = CARTESIAN_POINT ( 'NONE',  ( 0.000000000000000000, 0.000000000000000000, 0.000000000000000000 ) ) ;
#3168 = CARTESIAN_POINT ( 'NONE',  ( -144.2029146819478456, 59.80706661873672658, -63.83344705439064626 ) ) ;
#3169 = CARTESIAN_POINT ( 'NONE',  ( 213.7147529443549843, 172.0000000000000284, 277.7621479143228385 ) ) ;
#3170 = CARTESIAN_POINT ( 'NONE',  ( 164.8942204024298803, 63.66138186734713855, -42.52176649176428214 ) ) ;
#3171 = EDGE_LOOP ( 'NONE', ( #50531, #3061, #20090 ) ) ;
#3172 = CARTESIAN_POINT ( 'NONE',  ( -101.8140949286062380, 33.67224128592400945, 18.67452391595143979 ) ) ;
#3173 = EDGE_CURVE ( 'NONE', #53918, #30808, #10975, .T. ) ;
#3174 = CARTESIAN_POINT ( 'NONE',  ( 55.63918192129861495, 12.10794348580856905, 92.51693346615715541 ) ) ;
#3175 = VECTOR ( 'NONE', #11581, 1000.000000000000000 ) ;
#3176 = CARTESIAN_POINT ( 'NONE',  ( 151.0575564466925869, 54.07682166848538685, -93.41829839593862062 ) ) ;
#3177 = DIRECTION ( 'NONE',  ( -0.000000000000000000, -0.000000000000000000, -1.000000000000000000 ) ) ;
#3178 = ADVANCED_FACE ( 'NONE', ( #37029 ), #47913, .F. ) ;
#3179 = DIRECTION ( 'NONE',  ( -1.000000000000000000, 0.000000000000000000, 0.000000000000000000 ) ) ;
#3180 = CARTESIAN_POINT ( 'NONE',  ( -32.41627406084101892, 9.753381371531530064, -62.20983653673231117 ) ) ;
#3181 = CARTESIAN_POINT ( 'NONE',  ( 94.02861641584117081, 23.15570573563316259, 35.96120553985514334 ) ) ;
#3182 = ORIENTED_EDGE ( 'NONE', *, *, #20387, .F. ) ;
#3183 = CARTESIAN_POINT ( 'NONE',  ( 34.76618902119824384, -54.93755186520707667, 170.0000000000000000 ) ) ;
#3184 = AXIS2_PLACEMENT_3D ( 'NONE', #43604, #65785, #22507 ) ;
#3185 = DIRECTION ( 'NONE',  ( -2.168404344971009361E-16, 0.000000000000000000, 1.000000000000000000 ) ) ;
#3186 = EDGE_LOOP ( 'NONE', ( #35248, #68104 ) ) ;
#3187 = EDGE_CURVE ( 'NONE', #40883, #22781, #424, .T. ) ;
#3188 = CARTESIAN_POINT ( 'NONE',  ( 154.6530827109543225, 56.75509330623209792, -9.825228603827484974 ) ) ;
#3189 = VECTOR ( 'NONE', #65915, 1000.000000000000000 ) ;
#3190 = CARTESIAN_POINT ( 'NONE',  ( 0.1230226671127766652, 25.12215469714594107, 0.000000000000000000 ) ) ;
#3191 = CARTESIAN_POINT ( 'NONE',  ( -36.00304714721387711, 11.40794940913596278, 43.68818208324128705 ) ) ;
#3192 = CARTESIAN_POINT ( 'NONE',  ( -155.1302201283145905, 69.09929365814132041, -64.18797151881071272 ) ) ;
#3193 = CARTESIAN_POINT ( 'NONE',  ( 58.68582878687972482, 11.70927268415886502, 84.84224536443331033 ) ) ;
#3194 = CARTESIAN_POINT ( 'NONE',  ( -50.52927270563907314, 13.51486287463704450, -75.56336441046521202 ) ) ;
#3195 = CARTESIAN_POINT ( 'NONE',  ( -0.3255842968951678240, 7.525381170773407291, -15.58124028427686447 ) ) ;
#3196 = DIRECTION ( 'NONE',  ( 0.000000000000000000, 0.000000000000000000, 1.000000000000000000 ) ) ;
#3197 = CARTESIAN_POINT ( 'NONE',  ( 0.000000000000000000, 0.000000000000000000, 170.0010000000000048 ) ) ;
#3198 = ORIENTED_EDGE ( 'NONE', *, *, #22337, .F. ) ;
#3199 = CIRCLE ( 'NONE', #40248, 299.9999999999999432 ) ;
#3200 = CARTESIAN_POINT ( 'NONE',  ( -96.45303203827904781, 31.03218867996498176, -37.76676309982019575 ) ) ;
#3201 = ORIENTED_EDGE ( 'NONE', *, *, #20529, .F. ) ;
#3202 = DIRECTION ( 'NONE',  ( -1.000000000000000000, -0.000000000000000000, -0.000000000000000000 ) ) ;
#3203 = EDGE_CURVE ( 'NONE', #40013, #14673, #39651, .T. ) ;
#3204 = CARTESIAN_POINT ( 'NONE',  ( 42.03719354205839664, 9.783015072457470040, -9.249201505377850907 ) ) ;
#3205 = EDGE_CURVE ( 'NONE', #15244, #53408, #69376, .T. ) ;
#3206 = CARTESIAN_POINT ( 'NONE',  ( 262.2516123306975260, 190.0000000000000000, -21.28179539054375624 ) ) ;
#3207 = CARTESIAN_POINT ( 'NONE',  ( 442.3372781065085633, 400.0000000000000568, -116.4497041420118393 ) ) ;
#3208 = CARTESIAN_POINT ( 'NONE',  ( 18.19858669090298520, 7.596860100017449824, 44.62111217990123890 ) ) ;
#3209 = CARTESIAN_POINT ( 'NONE',  ( -108.9145525555662459, 37.42858360505776716, -19.17698904105195368 ) ) ;
#3210 = ORIENTED_EDGE ( 'NONE', *, *, #30839, .T. ) ;
#3211 = DIRECTION ( 'NONE',  ( -0.000000000000000000, -0.000000000000000000, -1.000000000000000000 ) ) ;
#3212 = CARTESIAN_POINT ( 'NONE',  ( -167.6413528428655013, 81.22881971256910560, 60.01989802298776766 ) ) ;
#3213 = ORIENTED_EDGE ( 'NONE', *, *, #23131, .T. ) ;
#3214 = ORIENTED_EDGE ( 'NONE', *, *, #44601, .T. ) ;
#3215 = CYLINDRICAL_SURFACE ( 'NONE', #1728, 7.500000000000020428 ) ;
#3216 = CARTESIAN_POINT ( 'NONE',  ( -15.55634918610400597, 15.55634918610405748, 85.00100000000000477 ) ) ;
#3217 = CARTESIAN_POINT ( 'NONE',  ( 180.2572128312847894, 77.77323980479701504, -24.34663789818131363 ) ) ;
#3218 = CARTESIAN_POINT ( 'NONE',  ( 104.3759779378692372, 27.35691041569131343, 68.65435695942450423 ) ) ;
#3219 = DIRECTION ( 'NONE',  ( -1.000000000000000000, 0.000000000000000000, 0.000000000000000000 ) ) ;
#3220 = CARTESIAN_POINT ( 'NONE',  ( 57.09527843067914432, 12.40436368789086785, -20.98701010641955733 ) ) ;
#3221 = EDGE_LOOP ( 'NONE', ( #1037, #38280, #21637, #19798 ) ) ;
#3222 = FACE_OUTER_BOUND ( 'NONE', #5487, .T. ) ;
#3223 = ORIENTED_EDGE ( 'NONE', *, *, #30107, .T. ) ;
#3224 = CARTESIAN_POINT ( 'NONE',  ( 437.3372781065085633, 399.9999999999998863, 103.5502958579881891 ) ) ;
#3225 = CARTESIAN_POINT ( 'NONE',  ( 10.13563904803030447, 7.391572367417535538, 69.31278184914521034 ) ) ;
#3226 = FACE_BOUND ( 'NONE', #24376, .T. ) ;
#3227 = B_SPLINE_CURVE_WITH_KNOTS ( 'NONE', 3,
 ( #41962, #5696, #42308, #59503, #64104, #5363, #16601, #21200, #63423, #26820, #48247, #58469, #21530, #15228, #10281, #42975, #64446, #10977, #27154, #7099, #1837, #33500, #65499, #33143, #38405, #39125, #60563, #55629, #12379, #28199, #65149, #38770, #6404, #12031, #7460, #54577, #50368, #39457, #55990, #22934, #34196, #61263, #33839, #16943, #34549 ),
 .UNSPECIFIED., .F., .F.,
 ( 4, 2, 2, 2, 2, 2, 2, 2, 2, 2, 2, 1, 2, 2, 2, 2, 2, 2, 2, 2, 2, 2, 4 ),
 ( 0.000000000000000000, 0.001510509505236004449, 0.002265764257853984665, 0.003021019010471965097, 0.004531528515707889532, 0.005286783268325863892, 0.006042038020943839120, 0.007552547526179752280, 0.009063057031415664572, 0.01057356653665157860, 0.01132882128926953128, 0.01208407604188748395, 0.01283933079450543663, 0.01359458554712339277, 0.01510509505235930854, 0.01586034980497727509, 0.01661560455759524338, 0.01812611406283117996, 0.01963662356806712347, 0.02039187832068507789, 0.02114713307330302883, 0.02265764257853897234, 0.02416815208377491586 ),
 .UNSPECIFIED. ) ;
#3228 = VERTEX_POINT ( 'NONE', #59158 ) ;
#3229 = CIRCLE ( 'NONE', #31340, 30.00000000000000000 ) ;
#3230 = VERTEX_POINT ( 'NONE', #37355 ) ;
#3231 = CARTESIAN_POINT ( 'NONE',  ( 14.99999999999997158, 0.000000000000000000, -50.00000000000000000 ) ) ;
#3232 = CARTESIAN_POINT ( 'NONE',  ( -129.7676077573642317, 50.31906829115933988, 85.38013851079792005 ) ) ;
#3233 = DIRECTION ( 'NONE',  ( -0.000000000000000000, 0.000000000000000000, 1.000000000000000000 ) ) ;
#3234 = DIRECTION ( 'NONE',  ( 0.000000000000000000, 0.000000000000000000, 1.000000000000000000 ) ) ;
#3235 = CARTESIAN_POINT ( 'NONE',  ( 22.60048481713442925, 6.814323260940660099, 88.04925594562278945 ) ) ;
#3236 = CARTESIAN_POINT ( 'NONE',  ( 23.26327404354069017, 7.863253330465858504, 91.89846529273600595 ) ) ;
#3237 = AXIS2_PLACEMENT_3D ( 'NONE', #6631, #26704, #65382 ) ;
#3238 = ORIENTED_EDGE ( 'NONE', *, *, #449, .T. ) ;
#3239 = B_SPLINE_CURVE_WITH_KNOTS ( 'NONE', 3,
 ( #58474, #37364, #5369, #786, #10287, #59165 ),
 .UNSPECIFIED., .F., .F.,
 ( 4, 2, 4 ),
 ( 1.095770181108577017E-06, 0.03239442681617711595, 0.06478775786217312593 ),
 .UNSPECIFIED. ) ;
#3240 = CARTESIAN_POINT ( 'NONE',  ( 417.3372781065086770, 0.000000000000000000, 108.5502958579881891 ) ) ;
#3241 = CARTESIAN_POINT ( 'NONE',  ( 197.5344630110112689, 98.61758706718750034, -46.07028429264449443 ) ) ;
#3242 = EDGE_LOOP ( 'NONE', ( #5036, #23690, #1221, #58718 ) ) ;
#3243 = CARTESIAN_POINT ( 'NONE',  ( 109.4689210239672832, 29.63125812599453823, -89.61153874658103291 ) ) ;
#3244 = ORIENTED_EDGE ( 'NONE', *, *, #60272, .T. ) ;
#3245 = CARTESIAN_POINT ( 'NONE',  ( -86.06489347855097094, 25.27905598459106429, -70.71628207122289211 ) ) ;
#3246 = CARTESIAN_POINT ( 'NONE',  ( -55.05276343752910151, -170.0000000000000000, -35.21632399845986328 ) ) ;
#3247 = ORIENTED_EDGE ( 'NONE', *, *, #55021, .F. ) ;
#3248 = B_SPLINE_CURVE_WITH_KNOTS ( 'NONE', 3,
 ( #59426, #53792, #31670, #11238, #47836, #49214, #32705, #5959, #43597, #65066, #63688, #15503, #60825, #49559, #23899, #11944, #44662, #65416, #40075, #7726, #23211, #61532, #34468, #13350, #33417, #55197, #65778, #17925, #54845, #12298, #28831, #66137, #7020, #22500, #1392, #6669, #66477, #28473, #29177, #28118, #2440, #50622, #55547, #61182, #45346 ),
 .UNSPECIFIED., .F., .F.,
 ( 4, 2, 2, 2, 2, 2, 2, 2, 2, 2, 2, 2, 2, 1, 2, 2, 2, 2, 2, 2, 2, 2, 4 ),
 ( 0.02356759485890610670, 0.02503765354686410607, 0.02577268289084311964, 0.02650771223482212974, 0.02797777092278016728, 0.02944782961073820482, 0.03018285895471723226, 0.03091788829869625971, 0.03238794698665432847, 0.03312297633063336633, 0.03385800567461240418, 0.03532806436257047294, 0.03606309370654950386, 0.03679812305052854171, 0.03753315239450757956, 0.03826818173848661048, 0.03973824042644467924, 0.04120829911440275495, 0.04267835780236083065, 0.04341338714633986851, 0.04414841649031891330, 0.04561847517827700288, 0.04708853386623509246 ),
 .UNSPECIFIED. ) ;
#3249 = EDGE_LOOP ( 'NONE', ( #58804, #53989, #66441, #9980 ) ) ;
#3250 = CARTESIAN_POINT ( 'NONE',  ( 9.288975942802419894, 6.379608420846962780, -39.26802939540083770 ) ) ;
#3251 = CARTESIAN_POINT ( 'NONE',  ( -417.6627218934913230, 219.4906275429376308, -146.4497041420118819 ) ) ;
#3252 = DIRECTION ( 'NONE',  ( 0.000000000000000000, -1.000000000000000000, 0.000000000000000000 ) ) ;
#3253 = EDGE_LOOP ( 'NONE', ( #43790, #62406 ) ) ;
#3254 = ADVANCED_FACE ( 'NONE', ( #52841, #58140 ), #58814, .F. ) ;
#3255 = CARTESIAN_POINT ( 'NONE',  ( -31.11269837220812207, -31.11269837220801193, 85.00100000000000477 ) ) ;
#3256 = CARTESIAN_POINT ( 'NONE',  ( -52.67596829228261868, 15.09584868440939331, 3.842776829869207766 ) ) ;
#3257 = EDGE_CURVE ( 'NONE', #19058, #41538, #58468, .T. ) ;
#3258 = DIRECTION ( 'NONE',  ( 0.000000000000000000, 0.000000000000000000, 1.000000000000000000 ) ) ;
#3259 = CARTESIAN_POINT ( 'NONE',  ( 117.6916924104495479, 32.48309187151382105, -15.56206514764637205 ) ) ;
#3260 = CARTESIAN_POINT ( 'NONE',  ( 86.15454111412294935, 20.32174891186167898, -50.82156419891173726 ) ) ;
#3261 = CARTESIAN_POINT ( 'NONE',  ( -171.5972879015330079, 86.93873520575962743, -88.51518996746024470 ) ) ;
#3262 = ORIENTED_EDGE ( 'NONE', *, *, #53398, .F. ) ;
#3263 = EDGE_CURVE ( 'NONE', #46362, #11641, #10625, .T. ) ;
#3264 = EDGE_LOOP ( 'NONE', ( #28641, #52255, #19541, #43229, #54328, #3932, #7134, #33574, #55209, #62511, #15106, #27197 ) ) ;
#3265 = CARTESIAN_POINT ( 'NONE',  ( 9.319975126229035567, -170.0000000000000000, 94.99999999999866418 ) ) ;
#3266 = CARTESIAN_POINT ( 'NONE',  ( -179.1803008299640396, 95.71362642995448766, 87.57955674619184094 ) ) ;
#3267 = PLANE ( 'NONE',  #34590 ) ;
#3268 = FACE_OUTER_BOUND ( 'NONE', #19540, .T. ) ;
#3269 = LINE ( 'NONE', #67986, #50541 ) ;
#3270 = CARTESIAN_POINT ( 'NONE',  ( -31.22562209718039128, 9.556395044504670366, -89.00629854612922998 ) ) ;
#3271 = CARTESIAN_POINT ( 'NONE',  ( 201.2735851903138666, 103.4250806913139940, 83.71735717358380668 ) ) ;
#3272 = CARTESIAN_POINT ( 'NONE',  ( 206.3053863259450225, 110.3084416756849748, 44.07829468878483681 ) ) ;
#3273 = CYLINDRICAL_SURFACE ( 'NONE', #52235, 7.500000000000013323 ) ;
#3274 = LINE ( 'NONE', #47533, #24176 ) ;
#3275 = EDGE_LOOP ( 'NONE', ( #20431, #61803, #15637, #3793 ) ) ;
#3276 = CARTESIAN_POINT ( 'NONE',  ( 13.37708032728286511, 7.441924986912760609, -23.28047698542330579 ) ) ;
#3277 = EDGE_LOOP ( 'NONE', ( #37757, #39085, #17297, #3492 ) ) ;
#3278 = CARTESIAN_POINT ( 'NONE',  ( -17.50000000000002842, 207.5000000000000284, 380.0000000000000000 ) ) ;
#3279 = ORIENTED_EDGE ( 'NONE', *, *, #10790, .F. ) ;
#3280 = EDGE_CURVE ( 'NONE', #66579, #13178, #38056, .T. ) ;
#3281 = AXIS2_PLACEMENT_3D ( 'NONE', #23321, #66243, #2207 ) ;
#3282 = CARTESIAN_POINT ( 'NONE',  ( -142.5042386072303771, 59.74110826975217492, 8.639212595881256007 ) ) ;
#3283 = CARTESIAN_POINT ( 'NONE',  ( 182.7745872728868335, 81.77554423487160307, -63.21223272561038442 ) ) ;
#3284 = CARTESIAN_POINT ( 'NONE',  ( -147.7895256390024770, 64.04409735547015714, 72.42034331570219763 ) ) ;
#3285 = CARTESIAN_POINT ( 'NONE',  ( -98.67723517640904163, 30.98797878696539243, -35.93232513735526368 ) ) ;
#3286 = AXIS2_PLACEMENT_3D ( 'NONE', #22504, #42574, #16179 ) ;
#3287 = CARTESIAN_POINT ( 'NONE',  ( 32.14349651933088126, 7.576119504381656711, -45.07096977590022391 ) ) ;
#3288 = CARTESIAN_POINT ( 'NONE',  ( -108.1144194775597640, 35.84457139767598477, 6.435316743732402145 ) ) ;
#3289 = LINE ( 'NONE', #24747, #33740 ) ;
#3290 = CARTESIAN_POINT ( 'NONE',  ( 126.4754729582248132, 37.14269484129875565, -42.16813892752784909 ) ) ;
#3291 = ORIENTED_EDGE ( 'NONE', *, *, #18989, .F. ) ;
#3292 = VERTEX_POINT ( 'NONE', #53533 ) ;
#3293 = CARTESIAN_POINT ( 'NONE',  ( 187.0823097343935331, 86.37667841017882608, 94.99999999999866418 ) ) ;
#3294 = DIRECTION ( 'NONE',  ( 0.000000000000000000, 0.000000000000000000, -1.000000000000000000 ) ) ;
#3295 = CARTESIAN_POINT ( 'NONE',  ( -23.93880457192868860, 8.479983864459175180, -69.42207390290181479 ) ) ;
#3296 = CARTESIAN_POINT ( 'NONE',  ( 10.13405324523498763, 6.385324379632245417, 5.717892688488246833 ) ) ;
#3297 = CARTESIAN_POINT ( 'NONE',  ( 43.96421756700839722, 10.06386361114659778, -75.93710349221596800 ) ) ;
#3298 = CARTESIAN_POINT ( 'NONE',  ( 437.3372781065085633, 395.0000000000001137, -146.4497041420117966 ) ) ;
#3299 = CARTESIAN_POINT ( 'NONE',  ( 175.8855729601531550, 73.50624012737689839, -75.99701591278079604 ) ) ;
#3300 = CARTESIAN_POINT ( 'NONE',  ( 277.7808008216760527, -21.53681828009572996, -4.492424461587424034 ) ) ;
#3301 = CARTESIAN_POINT ( 'NONE',  ( 104.7034219878852213, 26.40210929103715998, 5.186479124812725772 ) ) ;
#3302 = CARTESIAN_POINT ( 'NONE',  ( -25.79929641484368830, 9.749255553662434792, 59.59226522692620165 ) ) ;
#3303 = CYLINDRICAL_SURFACE ( 'NONE', #9373, 65.00000000000000000 ) ;
#3304 = CARTESIAN_POINT ( 'NONE',  ( 412.3372781065085633, 219.4906275429376308, 113.5502958579881749 ) ) ;
#3305 = CARTESIAN_POINT ( 'NONE',  ( -7.336760511143397778, 6.859209474528205952, 56.96013162991089018 ) ) ;
#3306 = ORIENTED_EDGE ( 'NONE', *, *, #52121, .F. ) ;
#3307 = DIRECTION ( 'NONE',  ( -1.000000000000000000, 0.000000000000000000, 0.000000000000000000 ) ) ;
#3308 = CARTESIAN_POINT ( 'NONE',  ( 152.8672128926847904, 55.41186463791521533, 57.82799647549036592 ) ) ;
#3309 = DIRECTION ( 'NONE',  ( 0.000000000000000000, 0.000000000000000000, 1.000000000000000000 ) ) ;
#3310 = CARTESIAN_POINT ( 'NONE',  ( 86.62931800182293784, -170.0000000000000000, 37.21208757247931942 ) ) ;
#3311 = AXIS2_PLACEMENT_3D ( 'NONE', #56545, #46328, #29819 ) ;
#3312 = DIRECTION ( 'NONE',  ( 0.000000000000000000, 0.000000000000000000, -1.000000000000000000 ) ) ;
#3313 = LINE ( 'NONE', #24774, #4136 ) ;
#3314 = EDGE_CURVE ( 'NONE', #69327, #44889, #32443, .T. ) ;
#3315 = ORIENTED_EDGE ( 'NONE', *, *, #43959, .F. ) ;
#3316 = FACE_OUTER_BOUND ( 'NONE', #58462, .T. ) ;
#3317 = EDGE_LOOP ( 'NONE', ( #10425, #3809, #37410, #62214 ) ) ;
#3318 = EDGE_CURVE ( 'NONE', #27441, #34992, #35911, .T. ) ;
#3319 = ORIENTED_EDGE ( 'NONE', *, *, #44714, .T. ) ;
#3320 = DIRECTION ( 'NONE',  ( -0.9009688679024155933, -0.4338837391175656699, 0.000000000000000000 ) ) ;
#3321 = CARTESIAN_POINT ( 'NONE',  ( -178.7483298110140595, 93.61800926271538970, -74.02109263234427772 ) ) ;
#3322 = DIRECTION ( 'NONE',  ( 0.000000000000000000, 1.000000000000000000, -0.000000000000000000 ) ) ;
#3323 = ORIENTED_EDGE ( 'NONE', *, *, #68445, .F. ) ;
#3324 = DIRECTION ( 'NONE',  ( -0.000000000000000000, -0.000000000000000000, -1.000000000000000000 ) ) ;
#3325 = AXIS2_PLACEMENT_3D ( 'NONE', #33184, #21917, #38095 ) ;
#3326 = DIRECTION ( 'NONE',  ( -0.6234898018587318180, -0.7818314824680311359, 0.000000000000000000 ) ) ;
#3327 = CARTESIAN_POINT ( 'NONE',  ( -0.3258398948454875321, 6.518608385615802803, 10.26970237692722598 ) ) ;
#3328 = CARTESIAN_POINT ( 'NONE',  ( 46.68215785206009372, 190.0000000000000000, -77.29788463846088575 ) ) ;
#3329 = CARTESIAN_POINT ( 'NONE',  ( -81.01931326044683601, 24.31309346877659294, 45.04357807855111417 ) ) ;
#3330 = VECTOR ( 'NONE', #15934, 1000.000000000000000 ) ;
#3331 = CARTESIAN_POINT ( 'NONE',  ( -28.13527276074847450, 10.08983026464524890, -22.71023329608813057 ) ) ;
#3332 = CARTESIAN_POINT ( 'NONE',  ( 133.8566784816069344, 41.42467568809808398, 2.665790248531674678 ) ) ;
#3333 = EDGE_CURVE ( 'NONE', #9171, #11778, #44252, .T. ) ;
#3334 = EDGE_LOOP ( 'NONE', ( #10103, #31150, #43388, #49165 ) ) ;
#3335 = EDGE_CURVE ( 'NONE', #49023, #5910, #12029, .T. ) ;
#3336 = CARTESIAN_POINT ( 'NONE',  ( 112.1164716692773453, 29.75790342121400656, -36.14479581440889433 ) ) ;
#3337 = CARTESIAN_POINT ( 'NONE',  ( 12.03194517566455701, 6.409266703743584870, 70.86927069785514277 ) ) ;
#3338 = DIRECTION ( 'NONE',  ( 0.000000000000000000, 6.123233995736761105E-17, -1.000000000000000000 ) ) ;
#3339 = CARTESIAN_POINT ( 'NONE',  ( -77.17954427531354611, 22.83512059001850503, 84.24976070025458341 ) ) ;
#3341 = ORIENTED_EDGE ( 'NONE', *, *, #16818, .T. ) ;
#3340 = CARTESIAN_POINT ( 'NONE',  ( -118.8429087385162148, 42.02330229425614050, 94.38756965892528683 ) ) ;
#3342 = CARTESIAN_POINT ( 'NONE',  ( 69.72564955710446100, 15.37006465677308498, 40.67263069985552448 ) ) ;
#3343 = ORIENTED_EDGE ( 'NONE', *, *, #29208, .T. ) ;
#3344 = EDGE_CURVE ( 'NONE', #327, #48751, #18345, .T. ) ;
#3345 = VECTOR ( 'NONE', #10581, 1000.000000000000000 ) ;
#3346 = VERTEX_POINT ( 'NONE', #65497 ) ;
#3347 = CARTESIAN_POINT ( 'NONE',  ( -144.9287131874382055, 60.39056348581544142, 71.02503524604800589 ) ) ;
#3348 = CARTESIAN_POINT ( 'NONE',  ( 7.705763971469675511, -66.19838173227481093, 34.48241795236665297 ) ) ;
#3349 = CARTESIAN_POINT ( 'NONE',  ( 197.3059626281005592, 96.72682679064187994, -69.35964093074025527 ) ) ;
#3350 = DIRECTION ( 'NONE',  ( 0.4738686624730094610, -0.8805955318567321166, 0.000000000000000000 ) ) ;
#3351 = CARTESIAN_POINT ( 'NONE',  ( -124.3250225421925563, 45.46958056770280621, 72.30208039458051417 ) ) ;
#3352 = CARTESIAN_POINT ( 'NONE',  ( -80.32755469740936860, 24.04130076192507204, -8.453244365720355091 ) ) ;
#3353 = CARTESIAN_POINT ( 'NONE',  ( -179.2210908201801089, 95.76260491022613053, -10.97533268791872274 ) ) ;
#3354 = B_SPLINE_CURVE_WITH_KNOTS ( 'NONE', 3,
 ( #66889, #66539, #13404, #13745, #2505, #41175, #3204, #61246, #14444, #51036, #13067, #18327, #2850, #46094, #56305, #24317, #34867, #39785, #35201, #67238, #62634, #19364, #62275, #55971, #30278, #51726, #7783, #56656, #55613, #7442, #28894, #50347, #23955, #50681, #45405, #47127, #15478, #31996, #26718, #35897, #68590, #36932, #41863, #36591 ),
 .UNSPECIFIED., .F., .F.,
 ( 4, 2, 2, 2, 2, 2, 2, 2, 2, 2, 2, 2, 2, 2, 2, 2, 2, 2, 2, 2, 2, 4 ),
 ( 0.000000000000000000, 0.001472974678681649233, 0.002209462018022473849, 0.002945949357363298465, 0.004418924036044928616, 0.005891898714726559634, 0.007364873393408188050, 0.008101360732749003993, 0.008837848072089820803, 0.01031082275077145095, 0.01178379742945308284, 0.01252028476879389271, 0.01325677210813470605, 0.01472974678681633447, 0.01546623412615715301, 0.01620272146549796982, 0.01767569614417959997, 0.01914867082286123359, 0.01988515816220204346, 0.02062164550154285333, 0.02209462018022448002, 0.02356759485890610670 ),
 .UNSPECIFIED. ) ;
#3355 = LINE ( 'NONE', #13564, #8173 ) ;
#3356 = ORIENTED_EDGE ( 'NONE', *, *, #64407, .F. ) ;
#3357 = ORIENTED_EDGE ( 'NONE', *, *, #27947, .T. ) ;
#3358 = EDGE_CURVE ( 'NONE', #60780, #10495, #49294, .T. ) ;
#3359 = FACE_OUTER_BOUND ( 'NONE', #47238, .T. ) ;
#3360 = CARTESIAN_POINT ( 'NONE',  ( 102.7435092758398127, 25.56449004647817702, 64.22656014339364106 ) ) ;
#3361 = CARTESIAN_POINT ( 'NONE',  ( -10.00000000000000178, -31.50328976398030534, -5.000000000000000000 ) ) ;
#3362 = AXIS2_PLACEMENT_3D ( 'NONE', #53763, #27037, #48468 ) ;
#3364 = EDGE_CURVE ( 'NONE', #29619, #68173, #28557, .T. ) ;
#3363 = FACE_OUTER_BOUND ( 'NONE', #61772, .T. ) ;
#3365 = EDGE_CURVE ( 'NONE', #383, #54841, #53079, .T. ) ;
#3366 = EDGE_CURVE ( 'NONE', #60705, #17566, #50001, .T. ) ;
#3367 = CARTESIAN_POINT ( 'NONE',  ( -2.645453300864630819E-14, -15.55634918610403616, 0.000000000000000000 ) ) ;
#3368 = CARTESIAN_POINT ( 'NONE',  ( -3.806566064960824935E-15, 7.321656987762869662, -3.318518101603011417 ) ) ;
#3369 = CARTESIAN_POINT ( 'NONE',  ( 164.6499013411308852, 63.45576988183555756, -68.28286819017297660 ) ) ;
#3370 = ORIENTED_EDGE ( 'NONE', *, *, #2236, .F. ) ;
#3371 = VERTEX_POINT ( 'NONE', #54575 ) ;
#3372 = VERTEX_POINT ( 'NONE', #38403 ) ;
#3373 = CARTESIAN_POINT ( 'NONE',  ( -152.4930836497867404, 68.09400557494208783, -22.35209726688142950 ) ) ;
#3374 = CARTESIAN_POINT ( 'NONE',  ( -85.10774223992955001, 24.88053943842881566, 60.91269031592988625 ) ) ;
#3375 = LINE ( 'NONE', #67747, #44396 ) ;
#3376 = CARTESIAN_POINT ( 'NONE',  ( 109.6727132707902683, -21.42428528562852463, 5.000000000000001776 ) ) ;
#3377 = CARTESIAN_POINT ( 'NONE',  ( -62.41727141396692247, 17.83188754031766976, 39.30035831538882007 ) ) ;
#3378 = CARTESIAN_POINT ( 'NONE',  ( 60.74750367560205433, 24.13405452624939329, 3.125053320693559764E-16 ) ) ;
#3379 = VECTOR ( 'NONE', #14810, 1000.000000000000000 ) ;
#3380 = CARTESIAN_POINT ( 'NONE',  ( 55.91133443650748802, 12.16263767238152838, 34.85883350782107470 ) ) ;
#3381 = DIRECTION ( 'NONE',  ( -0.000000000000000000, -0.000000000000000000, 1.000000000000000000 ) ) ;
#3382 = ORIENTED_EDGE ( 'NONE', *, *, #57602, .T. ) ;
#3383 = DIRECTION ( 'NONE',  ( -1.000000000000000000, 0.000000000000000000, 0.000000000000000000 ) ) ;
#3384 = CARTESIAN_POINT ( 'NONE',  ( -102.2801239173131194, 33.91021738430207222, -23.17002667451225406 ) ) ;
#3385 = CARTESIAN_POINT ( 'NONE',  ( 4.680456609903976606, 6.535341423375585101, -0.01688885742776517068 ) ) ;
#3386 = CARTESIAN_POINT ( 'NONE',  ( 69.74037587279238437, 14.33355757956373999, -66.70732824439824071 ) ) ;
#3387 = CARTESIAN_POINT ( 'NONE',  ( 133.6288034103010034, 41.28708886999548611, -24.17876034193200852 ) ) ;
#3388 = CARTESIAN_POINT ( 'NONE',  ( 20.74561700410411191, 7.717362891868937425, -10.52513384833799748 ) ) ;
#3389 = CARTESIAN_POINT ( 'NONE',  ( -105.4589068214114462, 34.42476264325678414, -76.16844833364910983 ) ) ;
#3390 = EDGE_LOOP ( 'NONE', ( #67378, #26917 ) ) ;
#3391 = PRODUCT_CONTEXT ( 'NONE', #5772, 'mechanical' ) ;
#3392 = CIRCLE ( 'NONE', #57276, 242.4895526022646379 ) ;
#3393 = CARTESIAN_POINT ( 'NONE',  ( -447.6627218934919483, 370.0000000000056275, -141.4497041420121661 ) ) ;
#3394 = CARTESIAN_POINT ( 'NONE',  ( 14.83727810650406731, 400.0000000000001137, -353.9497041420119672 ) ) ;
#3395 = DIRECTION ( 'NONE',  ( 1.000000000000000000, 0.000000000000000000, 0.000000000000000000 ) ) ;
#3396 = ITEM_DEFINED_TRANSFORMATION ( 'NONE', 'NONE', #37660,  #66832 ) ;
#3397 = CARTESIAN_POINT ( 'NONE',  ( 186.7642514597452532, 86.02880938169744240, -38.82112059087446454 ) ) ;
#3398 = EDGE_LOOP ( 'NONE', ( #5312, #26253 ) ) ;
#3399 = EDGE_CURVE ( 'NONE', #16538, #26941, #22579, .T. ) ;
#3400 = ORIENTED_EDGE ( 'NONE', *, *, #22879, .F. ) ;
#3401 = CARTESIAN_POINT ( 'NONE',  ( 0.000000000000000000, 0.000000000000000000, -22.00000000000000355 ) ) ;
#3402 = CARTESIAN_POINT ( 'NONE',  ( 198.2588776805010582, 99.52972231602373654, 6.006846211185677298 ) ) ;
#3403 = ORIENTED_EDGE ( 'NONE', *, *, #15348, .F. ) ;
#3404 = ADVANCED_FACE ( 'NONE', ( #59848 ), #16941, .F. ) ;
#3405 = CARTESIAN_POINT ( 'NONE',  ( 150.3314594630236343, 53.54839609209004436, 92.90526760572284104 ) ) ;
#3406 = ORIENTED_EDGE ( 'NONE', *, *, #15857, .F. ) ;
#3407 = CARTESIAN_POINT ( 'NONE',  ( 126.3732561463888686, 38.23795180971327312, -70.93242266372757854 ) ) ;
#3408 = CARTESIAN_POINT ( 'NONE',  ( 126.6576865394845584, 37.24426596493989905, 39.13016143230759525 ) ) ;
#3409 = CARTESIAN_POINT ( 'NONE',  ( -46.95151391448268896, 47.29862502947880643, 34.48241824012614387 ) ) ;
#3410 = VECTOR ( 'NONE', #2671, 1000.000000000000000 ) ;
#3411 = DIRECTION ( 'NONE',  ( -0.000000000000000000, 1.000000000000000000, -0.000000000000000000 ) ) ;
#3412 = DIRECTION ( 'NONE',  ( 0.000000000000000000, 0.000000000000000000, 1.000000000000000000 ) ) ;
#3414 = ORIENTED_EDGE ( 'NONE', *, *, #12766, .T. ) ;
#3413 = CARTESIAN_POINT ( 'NONE',  ( -78.66644367742111399, 22.32174330031319798, 18.57365054920947500 ) ) ;
#3415 = EDGE_CURVE ( 'NONE', #35337, #45327, #38767, .T. ) ;
#3416 = CARTESIAN_POINT ( 'NONE',  ( 61.33627421985470818, 12.28939706835343237, 44.62650739186889837 ) ) ;
#3417 = VERTEX_POINT ( 'NONE', #18005 ) ;
#3419 = ORIENTED_EDGE ( 'NONE', *, *, #42188, .T. ) ;
#3418 = EDGE_CURVE ( 'NONE', #41404, #63707, #39455, .T. ) ;
#3420 = CARTESIAN_POINT ( 'NONE',  ( 173.6700117628886346, 72.79957362875113347, 37.97907060391748502 ) ) ;
#3421 = CARTESIAN_POINT ( 'NONE',  ( 17.48889770758266593, 6.561062909825351674, -77.17229571346548767 ) ) ;
#3422 = EDGE_CURVE ( 'NONE', #60851, #22871, #1589, .T. ) ;
#3424 = EDGE_LOOP ( 'NONE', ( #40584, #35783, #60824, #8916 ) ) ;
#3423 = CARTESIAN_POINT ( 'NONE',  ( -132.4776673493542773, 52.21763813822160216, 61.36330782950730622 ) ) ;
#3425 = DIRECTION ( 'NONE',  ( -0.8532989592251508659, 0.000000000000000000, 0.5214219847544543374 ) ) ;
#3426 = FACE_BOUND ( 'NONE', #67273, .T. ) ;
#3427 = ORIENTED_EDGE ( 'NONE', *, *, #48793, .T. ) ;
#3428 = CARTESIAN_POINT ( 'NONE',  ( 210.9608386442062908, 117.1762372255315654, -66.53635089985841944 ) ) ;
#3429 = CARTESIAN_POINT ( 'NONE',  ( 140.2058232509808704, 46.59155168125933244, 41.03386337616525736 ) ) ;
#3430 = CARTESIAN_POINT ( 'NONE',  ( 115.7612476187723729, 32.64200929566222698, 42.21417507095826949 ) ) ;
#3431 = CARTESIAN_POINT ( 'NONE',  ( -41.31727360890708667, -62.59299402909810084, 43.58025477438756212 ) ) ;
#3432 = CARTESIAN_POINT ( 'NONE',  ( 70.11969827741708627, 15.47408882293423993, -67.61050290499292714 ) ) ;
#3433 = ORIENTED_EDGE ( 'NONE', *, *, #31602, .T. ) ;
#3434 = EDGE_LOOP ( 'NONE', ( #30327, #19426, #55519, #42432 ) ) ;
#3435 = AXIS2_PLACEMENT_3D ( 'NONE', #57257, #35805, #24215 ) ;
#3436 = CARTESIAN_POINT ( 'NONE',  ( -142.0227972901369071, 59.36121938936274489, -16.02476559944369328 ) ) ;
#3437 = CARTESIAN_POINT ( 'NONE',  ( -125.6703656163501677, 47.55170550253210138, -49.91370389823395470 ) ) ;
#3439 = ADVANCED_FACE ( 'NONE', ( #7097 ), #12728, .T. ) ;
#3438 = PLANE ( 'NONE',  #44136 ) ;
#3440 = EDGE_CURVE ( 'NONE', #63135, #33282, #23294, .T. ) ;
#3441 = DIRECTION ( 'NONE',  ( 0.000000000000000000, 0.000000000000000000, -1.000000000000000000 ) ) ;
#3442 = DIRECTION ( 'NONE',  ( 1.000000000000000000, -0.000000000000000000, 0.000000000000000000 ) ) ;
#3443 = DIRECTION ( 'NONE',  ( 0.000000000000000000, 0.000000000000000000, 1.000000000000000000 ) ) ;
#3444 = EDGE_CURVE ( 'NONE', #31875, #38167, #35289, .T. ) ;
#3445 = CARTESIAN_POINT ( 'NONE',  ( -146.7345109736526183, 61.86270848728295135, 45.19291357465738201 ) ) ;
#3446 = CARTESIAN_POINT ( 'NONE',  ( 157.4703587214989113, 57.65129005721576760, 2.564916881789689018 ) ) ;
#3447 = CARTESIAN_POINT ( 'NONE',  ( -171.0814041607219451, 84.88598211196838861, -76.28622867029723409 ) ) ;
#3448 = ORIENTED_EDGE ( 'NONE', *, *, #37030, .T. ) ;
#3449 = CARTESIAN_POINT ( 'NONE',  ( -109.7790042512817905, 37.90666514836944145, 37.72788903940714533 ) ) ;
#3450 = ORIENTED_EDGE ( 'NONE', *, *, #23507, .T. ) ;
#3451 = CARTESIAN_POINT ( 'NONE',  ( -37.38262509017739177, 10.64263598035110192, 15.47271197860792036 ) ) ;
#3452 = CARTESIAN_POINT ( 'NONE',  ( 79.63513233364429311, 18.20496177163924401, 61.33758711607030989 ) ) ;
#3453 = ORIENTED_EDGE ( 'NONE', *, *, #28604, .F. ) ;
#3454 = CARTESIAN_POINT ( 'NONE',  ( -79.09141991249970260, 22.48360285952615811, -88.80455181264525777 ) ) ;
#3455 = DIRECTION ( 'NONE',  ( 0.000000000000000000, 0.000000000000000000, -1.000000000000000000 ) ) ;
#3456 = DIRECTION ( 'NONE',  ( -0.000000000000000000, 1.000000000000000000, -0.000000000000000000 ) ) ;
#3457 = LINE ( 'NONE', #19631, #60271 ) ;
#3458 = CARTESIAN_POINT ( 'NONE',  ( -452.6627218934913799, 364.9999999999998295, -146.4497041420117966 ) ) ;
#3459 = CARTESIAN_POINT ( 'NONE',  ( -14.33576511807126153, 8.413127487936190363, -39.16238487774285204 ) ) ;
#3460 = AXIS2_PLACEMENT_3D ( 'NONE', #7707, #40739, #29155 ) ;
#3461 = CARTESIAN_POINT ( 'NONE',  ( -37.07436112751821611, 11.60822760208522553, -10.99943049330883582 ) ) ;
#3462 = VERTEX_POINT ( 'NONE', #27498 ) ;
#3463 = CARTESIAN_POINT ( 'NONE',  ( 422.4999999999999432, 207.5000000000000284, -2.000000000000000000 ) ) ;
#3464 = ORIENTED_EDGE ( 'NONE', *, *, #39061, .F. ) ;
#3465 = DIRECTION ( 'NONE',  ( -0.000000000000000000, -1.000000000000000000, -0.000000000000000000 ) ) ;
#3466 = CARTESIAN_POINT ( 'NONE',  ( -58.75378739419585372, 16.75118858561005553, 58.12022478182042562 ) ) ;
#3467 = CARTESIAN_POINT ( 'NONE',  ( -189.9554299271398179, 108.0836897899587825, 14.80701051291223891 ) ) ;
#3468 = EDGE_LOOP ( 'NONE', ( #65720, #3807, #12439, #3464 ) ) ;
#3469 = CARTESIAN_POINT ( 'NONE',  ( 24.46491470961361614, -5.710143558202974923, 0.000000000000000000 ) ) ;
#3470 = CARTESIAN_POINT ( 'NONE',  ( -8.314575874103553588, 6.922894809783094239, -77.26262132240753999 ) ) ;
#3471 = CARTESIAN_POINT ( 'NONE',  ( -32.41982179707237322, 9.753975577087190985, 30.26490829174940345 ) ) ;
#3472 = SURFACE_SIDE_STYLE ('',( #51665 ) ) ;
#3473 = ORIENTED_EDGE ( 'NONE', *, *, #19374, .F. ) ;
#3474 = DIRECTION ( 'NONE',  ( 0.9108602745606089179, 0.4127148655274875955, -6.735622585533857586E-15 ) ) ;
#3475 = CARTESIAN_POINT ( 'NONE',  ( -156.9919426121902575, 72.16759471857098163, 65.62823907942903645 ) ) ;
#3476 = CARTESIAN_POINT ( 'NONE',  ( -118.9649285217356294, 42.09781191014327817, 35.23770179663537760 ) ) ;
#3477 = CARTESIAN_POINT ( 'NONE',  ( 0.7145311798163274108, 9.237604307034018802, -2.124379920709345337E-16 ) ) ;
#3478 = VERTEX_POINT ( 'NONE', #65860 ) ;
#3479 = DIRECTION ( 'NONE',  ( -0.000000000000000000, -0.000000000000000000, -1.000000000000000000 ) ) ;
#3480 = CARTESIAN_POINT ( 'NONE',  ( 90.91465859190770971, 20.92790537681858609, 57.89667315351857724 ) ) ;
#3481 = CARTESIAN_POINT ( 'NONE',  ( 447.3372781065086201, 0.000000000000000000, 83.55029585798817493 ) ) ;
#3482 = EDGE_CURVE ( 'NONE', #32392, #65236, #45072, .T. ) ;
#3483 = CARTESIAN_POINT ( 'NONE',  ( -121.5677746760273834, 43.71038933438990171, -63.11338067390871487 ) ) ;
#3484 = EDGE_LOOP ( 'NONE', ( #44919, #29130, #61279, #39171, #29061, #39628 ) ) ;
#3485 = CARTESIAN_POINT ( 'NONE',  ( 203.9276061909315274, 105.2889220654478919, 29.20772073876941377 ) ) ;
#3486 = CARTESIAN_POINT ( 'NONE',  ( 209.9518228411288874, 18.00000000000002842, 31.43423095485942298 ) ) ;
#3487 = DIRECTION ( 'NONE',  ( 1.387778780781445429E-16, -1.000000000000000000, -3.081487911019577365E-33 ) ) ;
#3488 = CARTESIAN_POINT ( 'NONE',  ( 140.8855094313932739, 47.03549517811091363, 12.79525956615474236 ) ) ;
#3489 = CARTESIAN_POINT ( 'NONE',  ( 0.000000000000000000, 0.000000000000000000, 170.0000000000000000 ) ) ;
#3490 = VECTOR ( 'NONE', #9251, 1000.000000000000114 ) ;
#3491 = VECTOR ( 'NONE', #39909, 1000.000000000000000 ) ;
#3492 = ORIENTED_EDGE ( 'NONE', *, *, #60667, .T. ) ;
#3493 = EDGE_CURVE ( 'NONE', #67476, #41408, #39123, .T. ) ;
#3494 = CARTESIAN_POINT ( 'NONE',  ( 162.0862735437575850, 62.63196145447161456, -22.71030774999397650 ) ) ;
#3495 = ORIENTED_EDGE ( 'NONE', *, *, #8743, .F. ) ;
#3496 = CARTESIAN_POINT ( 'NONE',  ( 70.26639875985988226, 15.51307715494295358, 66.13948629930069956 ) ) ;
#3497 = CARTESIAN_POINT ( 'NONE',  ( 126.9909055734727019, 37.43041694803015673, 93.80275659116571774 ) ) ;
#3498 = EDGE_CURVE ( 'NONE', #14375, #1535, #61261, .T. ) ;
#3499 = EDGE_CURVE ( 'NONE', #37504, #7511, #66212, .T. ) ;
#3501 = ORIENTED_EDGE ( 'NONE', *, *, #36557, .F. ) ;
#3500 = CARTESIAN_POINT ( 'NONE',  ( 149.4165763529819344, -26.99999999999998224, 108.9999999999999858 ) ) ;
#3502 = CARTESIAN_POINT ( 'NONE',  ( 163.1313205310724470, 63.49733392291054201, -38.69832981363442315 ) ) ;
#3503 = CIRCLE ( 'NONE', #56271, 24.69999999999999929 ) ;
#3504 = DIRECTION ( 'NONE',  ( 1.000000000000000000, 0.000000000000000000, 0.000000000000000000 ) ) ;
#3505 = CARTESIAN_POINT ( 'NONE',  ( 160.4963793545268800, 60.04225845346905999, -50.50113425675434797 ) ) ;
#3506 = EDGE_LOOP ( 'NONE', ( #56785, #7196, #50859, #10391 ) ) ;
#3507 = CARTESIAN_POINT ( 'NONE',  ( -96.02159028238558847, 30.82695531378848841, 15.31486708033657784 ) ) ;
#3508 = CARTESIAN_POINT ( 'NONE',  ( 55.59973583101010774, 12.10012336970133262, 89.83280078296678539 ) ) ;
#3509 = CARTESIAN_POINT ( 'NONE',  ( 150.6472384575835122, 53.77757500042995531, -94.17017552904665934 ) ) ;
#3510 = CARTESIAN_POINT ( 'NONE',  ( 82.34401416830215226, 19.05992892018826623, -22.63702806220790364 ) ) ;
#3511 = CARTESIAN_POINT ( 'NONE',  ( -178.9182503768213621, 95.39606678475963975, -91.13644876916208659 ) ) ;
#3512 = CARTESIAN_POINT ( 'NONE',  ( 150.0889146124742695, 52.13243511955542431, 62.39775547893556507 ) ) ;
#3513 = CARTESIAN_POINT ( 'NONE',  ( -142.0747101610765242, 59.40211529287933701, -95.00000000000133582 ) ) ;
#3514 = ORIENTED_EDGE ( 'NONE', *, *, #60185, .T. ) ;
#3515 = CARTESIAN_POINT ( 'NONE',  ( -101.8187363387487494, 33.67461140603123937, 57.36362509687881328 ) ) ;
#3516 = CARTESIAN_POINT ( 'NONE',  ( 181.0840389613909736, -170.0000000000000000, -97.41415884680698412 ) ) ;
#3517 = ORIENTED_EDGE ( 'NONE', *, *, #33458, .T. ) ;
#3518 = FACE_OUTER_BOUND ( 'NONE', #5864, .T. ) ;
#3519 = CARTESIAN_POINT ( 'NONE',  ( -56.33023788822384859, 15.02754539266624789, 84.10929812850636722 ) ) ;
#3520 = CARTESIAN_POINT ( 'NONE',  ( 26.99999999999999645, 0.000000000000000000, -0.000000000000000000 ) ) ;
#3521 = CARTESIAN_POINT ( 'NONE',  ( -12.50000000000002842, -18.06806526123148160, 380.0000000000000000 ) ) ;
#3522 = CARTESIAN_POINT ( 'NONE',  ( 59.54768723222450433, 11.89486923077556035, 84.34372402572785177 ) ) ;
#3523 = ADVANCED_FACE ( 'NONE', ( #56675 ), #2866, .F. ) ;
#3524 = CARTESIAN_POINT ( 'NONE',  ( 185.1710994180822638, 84.30654632312743502, 16.26852148075597171 ) ) ;
#3525 = CARTESIAN_POINT ( 'NONE',  ( 210.6475357757681763, 114.8748261044495962, -48.39950946580693625 ) ) ;
#3526 = CARTESIAN_POINT ( 'NONE',  ( 173.5837434292113528, 71.34409607026157119, 9.675991114982885222 ) ) ;
#3527 = CARTESIAN_POINT ( 'NONE',  ( -61.86845765289634613, 16.61548683002699534, 7.833006060118358427 ) ) ;
#3528 = ORIENTED_EDGE ( 'NONE', *, *, #31290, .F. ) ;
#3529 = DIRECTION ( 'NONE',  ( -0.7071067811865474617, -4.906538933386759377E-15, 0.7071067811865474617 ) ) ;
#3530 = ORIENTED_EDGE ( 'NONE', *, *, #45276, .F. ) ;
#3531 = DIRECTION ( 'NONE',  ( 0.000000000000000000, 0.000000000000000000, 1.000000000000000000 ) ) ;
#3532 = APPLICATION_CONTEXT ( 'automotive_design' ) ;
#3533 = DIRECTION ( 'NONE',  ( -0.000000000000000000, -0.000000000000000000, -1.000000000000000000 ) ) ;
#3534 = SURFACE_SIDE_STYLE ('',( #42208 ) ) ;
#3535 = PLANE ( 'NONE',  #7568 ) ;
#3536 = CARTESIAN_POINT ( 'NONE',  ( -10.99038543402095058, 7.117699646488151011, 84.49731268521362892 ) ) ;
#3537 = CYLINDRICAL_SURFACE ( 'NONE', #63646, 65.00000000000000000 ) ;
#3538 = VERTEX_POINT ( 'NONE', #8494 ) ;
#3539 = CARTESIAN_POINT ( 'NONE',  ( -71.67841390531690138, 19.78168466957075822, 62.02784106711190049 ) ) ;
#3540 = CARTESIAN_POINT ( 'NONE',  ( -169.1041038606267648, 82.76530082651282783, 58.81708485632820071 ) ) ;
#3541 = ORIENTED_EDGE ( 'NONE', *, *, #3648, .T. ) ;
#3542 = VERTEX_POINT ( 'NONE', #55148 ) ;
#3543 = CARTESIAN_POINT ( 'NONE',  ( -156.6692143066620702, 70.50016761530885390, 35.97663252705407899 ) ) ;
#3544 = DIRECTION ( 'NONE',  ( 1.000000000000000000, -0.000000000000000000, -0.000000000000000000 ) ) ;
#3546 = CARTESIAN_POINT ( 'NONE',  ( 174.6176230994777541, 72.30829341023246570, -13.04120643648126965 ) ) ;
#3545 = VECTOR ( 'NONE', #38363, 1000.000000000000000 ) ;
#3547 = VECTOR ( 'NONE', #40734, 1000.000000000000000 ) ;
#3548 = CARTESIAN_POINT ( 'NONE',  ( -170.2856292770789821, 85.50720222068220266, 58.20975371259029174 ) ) ;
#3549 = DIRECTION ( 'NONE',  ( 0.7071067811865476838, 1.110223024625156294E-16, 0.7071067811865474617 ) ) ;
#3550 = CARTESIAN_POINT ( 'NONE',  ( 55.52751777340359496, 12.08567914268656729, -15.88646113736828447 ) ) ;
#3551 = ORIENTED_EDGE ( 'NONE', *, *, #14250, .T. ) ;
#3552 = CARTESIAN_POINT ( 'NONE',  ( -4.238248308523542285, -66.51046379052904456, 34.48241795236666718 ) ) ;
#3553 = ORIENTED_EDGE ( 'NONE', *, *, #22471, .F. ) ;
#3554 = CARTESIAN_POINT ( 'NONE',  ( 212.1700216741375300, 117.1889356120871497, 9.135482143913240094 ) ) ;
#3555 = CARTESIAN_POINT ( 'NONE',  ( 14.80291736570134731, 7.477373894757625372, 71.81068398635675010 ) ) ;
#3556 = DIRECTION ( 'NONE',  ( 1.000000000000000000, 0.000000000000000000, 0.000000000000000000 ) ) ;
#3557 = CARTESIAN_POINT ( 'NONE',  ( 15.36604569585143309, 6.487299053250196401, -89.20804527961311692 ) ) ;
#3558 = EDGE_CURVE ( 'NONE', #38399, #17506, #28422, .T. ) ;
#3559 = ADVANCED_FACE ( 'NONE', ( #18572 ), #60439, .F. ) ;
#3560 = ADVANCED_FACE ( 'NONE', ( #39678 ), #67728, .T. ) ;
#3561 = B_SPLINE_CURVE_WITH_KNOTS ( 'NONE', 3,
 ( #18057, #50751, #28966, #29297, #13471, #51106, #18394, #34241, #56727, #39510, #40887, #39851, #61309, #46158, #60957, #23679, #61652, #7514, #35269, #24028, #67633, #56371, #34929, #34599, #29641, #2571, #7851, #8193, #62348, #50060, #2915, #29993, #13134, #45823, #51454, #12779, #14161, #35622, #55682, #15877, #4975, #19782, #25069, #52477, #63032 ),
 .UNSPECIFIED., .F., .F.,
 ( 4, 2, 2, 2, 2, 2, 2, 2, 2, 2, 2, 2, 2, 1, 2, 2, 2, 2, 2, 2, 2, 2, 4 ),
 ( 0.02352719711393054525, 0.02499986300757018470, 0.02573619595438999402, 0.02647252890120980334, 0.02794519479484942198, 0.02941786068848904062, 0.03015419363530885341, 0.03089052658212866620, 0.03236319247576828484, 0.03309952542258809416, 0.03383585836940790348, 0.03530852426304752212, 0.03604485720986733144, 0.03678119015668713382, 0.03751752310350694314, 0.03825385605032674552, 0.03972652194396637804, 0.04119918783760599668, 0.04267185373124562919, 0.04340818667806543157, 0.04414451962488523395, 0.04561718551852482484, 0.04708985141216440878 ),
 .UNSPECIFIED. ) ;
#3562 = VERTEX_POINT ( 'NONE', #44952 ) ;
#3563 = ORIENTED_EDGE ( 'NONE', *, *, #52893, .T. ) ;
#3564 = CARTESIAN_POINT ( 'NONE',  ( 0.000000000000000000, 0.000000000000000000, 0.000000000000000000 ) ) ;
#3565 = DIRECTION ( 'NONE',  ( -1.000000000000000000, -0.000000000000000000, -0.000000000000000000 ) ) ;
#3566 = CARTESIAN_POINT ( 'NONE',  ( 39.40195752203892710, 9.424259417798133143, -77.46436805589148378 ) ) ;
#3567 = CARTESIAN_POINT ( 'NONE',  ( 181.0840389613909736, -170.0000000000000000, -97.41415884680698412 ) ) ;
#3568 = CARTESIAN_POINT ( 'NONE',  ( 16.44502386301708086, 6.521830180776601260, 83.70387535602117168 ) ) ;
#3569 = CARTESIAN_POINT ( 'NONE',  ( 23.17379743143359505, 7.857626726498480707, 92.54999467873835783 ) ) ;
#3570 = VERTEX_POINT ( 'NONE', #13307 ) ;
#3571 = FACE_OUTER_BOUND ( 'NONE', #7865, .T. ) ;
#3572 = CARTESIAN_POINT ( 'NONE',  ( 197.3064269725218765, 98.33232022113057269, -42.51203141086486426 ) ) ;
#3573 = ORIENTED_EDGE ( 'NONE', *, *, #17782, .T. ) ;
#3574 = DIRECTION ( 'NONE',  ( 1.000000000000000000, 0.000000000000000000, -0.000000000000000000 ) ) ;
#3575 = EDGE_LOOP ( 'NONE', ( #20280, #65714, #25182, #9840, #14109 ) ) ;
#3576 = CARTESIAN_POINT ( 'NONE',  ( -85.45399718454959270, 25.02415453493130570, -66.25966646325893805 ) ) ;
#3577 = CARTESIAN_POINT ( 'NONE',  ( -55.05276343752908730, 15.72344139423347720, -8.371773407996169425 ) ) ;
#3578 = EDGE_CURVE ( 'NONE', #9829, #58885, #61487, .T. ) ;
#3579 = ORIENTED_EDGE ( 'NONE', *, *, #59019, .T. ) ;
#3580 = EDGE_CURVE ( 'NONE', #63871, #16484, #61932, .T. ) ;
#3581 = VECTOR ( 'NONE', #57124, 1000.000000000000000 ) ;
#3582 = ORIENTED_EDGE ( 'NONE', *, *, #15343, .F. ) ;
#3583 = CARTESIAN_POINT ( 'NONE',  ( 44.34362023773823580, 10.12115849931653067, 58.59490733264918561 ) ) ;
#3584 = CYLINDRICAL_SURFACE ( 'NONE', #18065, 30.00000000000000000 ) ;
#3585 = CARTESIAN_POINT ( 'NONE',  ( 22.52576749827964164, 6.809805260274345073, 7.338887533324804480 ) ) ;
#3586 = AXIS2_PLACEMENT_3D ( 'NONE', #12327, #33447, #27444 ) ;
#3587 = ORIENTED_EDGE ( 'NONE', *, *, #68829, .T. ) ;
#3588 = PRODUCT_DEFINITION_SHAPE ( 'NONE', 'NONE',  #45241 ) ;
#3589 = VECTOR ( 'NONE', #31637, 1000.000000000000000 ) ;
#3590 = VECTOR ( 'NONE', #42220, 1000.000000000000000 ) ;
#3591 = CARTESIAN_POINT ( 'NONE',  ( -28.04483122278597662, 9.058704822772433829, 84.70984886725781848 ) ) ;
#3592 = CARTESIAN_POINT ( 'NONE',  ( 173.6007744016332595, 72.73482010729017588, -69.98774395762167444 ) ) ;
#3593 = CARTESIAN_POINT ( 'NONE',  ( 73.57152302639893549, 14.62167909564604429, 170.0000000000000000 ) ) ;
#3594 = CARTESIAN_POINT ( 'NONE',  ( 108.3906473026529653, 28.03385344351496400, -36.13980848578636085 ) ) ;
#3595 = B_SPLINE_CURVE_WITH_KNOTS ( 'NONE', 3,
 ( #22887, #61570, #39763, #40113, #55948, #7763, #61898, #66863, #18662, #40453, #13385, #61220 ),
 .UNSPECIFIED., .F., .F.,
 ( 4, 2, 2, 2, 2, 4 ),
 ( 0.000000000000000000, 0.002486957010932606960, 0.004973914021865213919, 0.007460871032797820011, 0.008704349538264120889, 0.009947828043730422634 ),
 .UNSPECIFIED. ) ;
#3596 = AXIS2_PLACEMENT_3D ( 'NONE', #19332, #9134, #56272 ) ;
#3597 = CARTESIAN_POINT ( 'NONE',  ( 79.12879321038293767, 18.04902206524925745, -43.08565838544853221 ) ) ;
#3598 = CARTESIAN_POINT ( 'NONE',  ( -165.7614670400926684, 80.73254387118949182, -94.42993858856560507 ) ) ;
#3599 = ORIENTED_EDGE ( 'NONE', *, *, #2055, .F. ) ;
#3600 = ORIENTED_EDGE ( 'NONE', *, *, #15027, .F. ) ;
#3601 = CARTESIAN_POINT ( 'NONE',  ( -79.14638003838382474, 23.58242782405880078, -61.96000122218159589 ) ) ;
#3602 = CARTESIAN_POINT ( 'NONE',  ( 427.4999999999999432, -18.06806526123148160, -2.000000000000000000 ) ) ;
#3603 = FACE_OUTER_BOUND ( 'NONE', #44316, .T. ) ;
#3604 = DIRECTION ( 'NONE',  ( 2.220446049250313081E-16, 0.000000000000000000, 1.000000000000000000 ) ) ;
#3605 = DIRECTION ( 'NONE',  ( -0.000000000000000000, -0.000000000000000000, 1.000000000000000000 ) ) ;
#3606 = DIRECTION ( 'NONE',  ( -0.000000000000000000, 1.000000000000000000, 0.000000000000000000 ) ) ;
#3607 = CARTESIAN_POINT ( 'NONE',  ( -119.5563837756079693, 43.64229894412652300, -65.21578466046432254 ) ) ;
#3608 = CARTESIAN_POINT ( 'NONE',  ( 211.7357196141372242, 118.3691710715567211, 39.31684144783690726 ) ) ;
#3609 = CARTESIAN_POINT ( 'NONE',  ( -84.53753601793931693, 25.73343139558517478, 60.06906254790580135 ) ) ;
#3610 = CYLINDRICAL_SURFACE ( 'NONE', #28683, 246.3582898394606957 ) ;
#3611 = ORIENTED_EDGE ( 'NONE', *, *, #13648, .T. ) ;
#3612 = CARTESIAN_POINT ( 'NONE',  ( 11.20486344102687504, 7.403248964808831545, -10.21748692402197634 ) ) ;
#3613 = VERTEX_POINT ( 'NONE', #28786 ) ;
#3614 = CARTESIAN_POINT ( 'NONE',  ( 198.7084915431530305, 98.47675983942194478, -21.50361554362704553 ) ) ;
#3615 = ORIENTED_EDGE ( 'NONE', *, *, #30109, .T. ) ;
#3616 = DIRECTION ( 'NONE',  ( -0.000000000000000000, 1.000000000000000000, -0.000000000000000000 ) ) ;
#3617 = CARTESIAN_POINT ( 'NONE',  ( 183.1873354889582686, 82.20882912211249050, -77.78155292010042388 ) ) ;
#3618 = CARTESIAN_POINT ( 'NONE',  ( -190.6985136298601731, 109.1272424661242582, -95.00000000000133582 ) ) ;
#3619 = CARTESIAN_POINT ( 'NONE',  ( 444.9999999999999432, 225.0000000000000000, 0.000000000000000000 ) ) ;
#3620 = CARTESIAN_POINT ( 'NONE',  ( 34.45817031441434608, 7.817703378455679086, -48.78147938101668757 ) ) ;
#3621 = LINE ( 'NONE', #51125, #64131 ) ;
#3622 = CARTESIAN_POINT ( 'NONE',  ( 9.045716588192243890, 7.384596431530736638, -39.69777131749945198 ) ) ;
#3623 = CARTESIAN_POINT ( 'NONE',  ( 128.9253503890652439, 38.52561778336671239, -49.17949685352920852 ) ) ;
#3624 = ORIENTED_EDGE ( 'NONE', *, *, #9148, .T. ) ;
#3625 = VERTEX_POINT ( 'NONE', #50237 ) ;
#3626 = FACE_OUTER_BOUND ( 'NONE', #64552, .T. ) ;
#3627 = DIRECTION ( 'NONE',  ( -0.000000000000000000, -0.000000000000000000, -1.000000000000000000 ) ) ;
#3628 = PLANE ( 'NONE',  #3844 ) ;
#3629 = UNCERTAINTY_MEASURE_WITH_UNIT (LENGTH_MEASURE( 1.000000000000000082E-05 ), #16852, 'distance_accuracy_value', 'NONE');
#3630 = AXIS2_PLACEMENT_3D ( 'NONE', #28129, #66490, #44673 ) ;
#3631 = DIRECTION ( 'NONE',  ( 0.7071067811865474617, -5.551115123125781716E-16, 0.7071067811865475727 ) ) ;
#3632 = ADVANCED_FACE ( 'NONE', ( #23511 ), #48674, .T. ) ;
#3633 = DIRECTION ( 'NONE',  ( 1.792759282944491616E-18, -4.776790026843708002E-18, -1.000000000000000000 ) ) ;
#3634 = CARTESIAN_POINT ( 'NONE',  ( 186.0827296088607170, 85.28826835108064586, -11.28428718647697693 ) ) ;
#3635 = CARTESIAN_POINT ( 'NONE',  ( 209.6698611676810629, 115.2210955123518090, 15.49623849697043632 ) ) ;
#3636 = AXIS2_PLACEMENT_3D ( 'NONE', #21413, #38283, #65379 ) ;
#3637 = CARTESIAN_POINT ( 'NONE',  ( -180.6011569556094969, 95.85968111394265634, -42.84200977746586858 ) ) ;
#3638 = CARTESIAN_POINT ( 'NONE',  ( 91.51282003084293137, 21.14522045960332264, -10.76386589503217728 ) ) ;
#3639 = CARTESIAN_POINT ( 'NONE',  ( -23.93895920923072751, 9.495000752338448535, 64.31892236427358966 ) ) ;
#3640 = FACE_OUTER_BOUND ( 'NONE', #7061, .T. ) ;
#3641 = CARTESIAN_POINT ( 'NONE',  ( -55.05276343752910151, 14.68156374112636797, 72.16187836339486239 ) ) ;
#3642 = EDGE_CURVE ( 'NONE', #3054, #66077, #28394, .T. ) ;
#3643 = AXIS2_PLACEMENT_3D ( 'NONE', #58333, #69236, #32312 ) ;
#3644 = EDGE_CURVE ( 'NONE', #21636, #60543, #50981, .T. ) ;
#3645 = CARTESIAN_POINT ( 'NONE',  ( -3.244108878396729345, 6.635632329121485817, 70.41866219491829781 ) ) ;
#3646 = ORIENTED_EDGE ( 'NONE', *, *, #5690, .T. ) ;
#3647 = FACE_OUTER_BOUND ( 'NONE', #22136, .T. ) ;
#3648 = EDGE_CURVE ( 'NONE', #15461, #1035, #69111, .T. ) ;
#3649 = AXIS2_PLACEMENT_3D ( 'NONE', #4128, #13639, #40372 ) ;
#3650 = CARTESIAN_POINT ( 'NONE',  ( 157.2533363798599169, 58.75760182111574892, 56.25401806271707272 ) ) ;
#3651 = LINE ( 'NONE', #53889, #16378 ) ;
#3652 = CARTESIAN_POINT ( 'NONE',  ( -49.45858366215606594, 13.25262207532078484, -47.71791105718050119 ) ) ;
#3653 = FACE_BOUND ( 'NONE', #46999, .T. ) ;
#3654 = DIRECTION ( 'NONE',  ( -1.000000000000000000, 0.000000000000000000, 0.000000000000000000 ) ) ;
#3655 = EDGE_LOOP ( 'NONE', ( #54292, #41870 ) ) ;
#3656 = CARTESIAN_POINT ( 'NONE',  ( -189.5593729888621510, 107.5326066953720527, -93.58956526689634359 ) ) ;
#3657 = DIRECTION ( 'NONE',  ( -0.000000000000000000, -0.000000000000000000, -1.000000000000000000 ) ) ;
#3658 = ORIENTED_EDGE ( 'NONE', *, *, #56244, .F. ) ;
#3659 = ORIENTED_EDGE ( 'NONE', *, *, #14979, .F. ) ;
#3660 = CYLINDRICAL_SURFACE ( 'NONE', #51048, 7.500000000000013323 ) ;
#3661 = CARTESIAN_POINT ( 'NONE',  ( -178.0658882571760842, 92.80593104957419825, -74.70044367160248555 ) ) ;
#3662 = CARTESIAN_POINT ( 'NONE',  ( -64.83840629396348731, 4.580509716059292913, 170.0000000000000000 ) ) ;
#3663 = EDGE_CURVE ( 'NONE', #23198, #50057, #6129, .T. ) ;
#3664 = ORIENTED_EDGE ( 'NONE', *, *, #5871, .F. ) ;
#3665 = FACE_OUTER_BOUND ( 'NONE', #32196, .T. ) ;
#3666 = CARTESIAN_POINT ( 'NONE',  ( 0.000000000000000000, 0.000000000000000000, -27.00000000000000000 ) ) ;
#3667 = CARTESIAN_POINT ( 'NONE',  ( -27.00000000000000355, 26.99999999999999645, 0.000000000000000000 ) ) ;
#3668 = CARTESIAN_POINT ( 'NONE',  ( 58.47885130911550533, 12.69429933094348328, -49.21325034717124680 ) ) ;
#3669 = DIRECTION ( 'NONE',  ( -1.000000000000000000, 0.000000000000000000, 0.000000000000000000 ) ) ;
#3670 = CARTESIAN_POINT ( 'NONE',  ( -23.98747857548121942, 9.501432345103355104, -14.98739851332648954 ) ) ;
#3671 = CARTESIAN_POINT ( 'NONE',  ( 135.6651581599210488, 42.52720121194705882, 2.883460403371903347 ) ) ;
#3672 = ORIENTED_EDGE ( 'NONE', *, *, #12701, .F. ) ;
#3673 =( LENGTH_UNIT ( ) NAMED_UNIT ( * ) SI_UNIT ( .MILLI., .METRE. ) );
#3674 = CARTESIAN_POINT ( 'NONE',  ( 15.29293866748104236, 6.484959508098437020, 71.85925826316895382 ) ) ;
#3675 = CARTESIAN_POINT ( 'NONE',  ( 6.400000000000000355, 4.618802153517001408, -8.000000000000000000 ) ) ;
#3676 = LINE ( 'NONE', #56449, #63447 ) ;
#3678 = EDGE_LOOP ( 'NONE', ( #22909, #31406, #7315, #35548, #23744, #13705, #14515, #10673, #19243 ) ) ;
#3677 = DIRECTION ( 'NONE',  ( 0.000000000000000000, 0.000000000000000000, 1.000000000000000000 ) ) ;
#3679 = CARTESIAN_POINT ( 'NONE',  ( 63.98689050258324329, 13.93365232918667651, 44.76545543697432095 ) ) ;
#3680 = ORIENTED_EDGE ( 'NONE', *, *, #8167, .T. ) ;
#3681 = CONICAL_SURFACE ( 'NONE', #16025, 65.00000000000000000, 0.7853981633974497223 ) ;
#3682 = VERTEX_POINT ( 'NONE', #15998 ) ;
#3683 = VECTOR ( 'NONE', #69513, 1000.000000000000000 ) ;
#3684 = CARTESIAN_POINT ( 'NONE',  ( -143.2464978228198902, 59.04559547356110727, 69.20284246303761222 ) ) ;
#3685 = DIRECTION ( 'NONE',  ( 1.000000000000000000, 0.000000000000000000, -0.000000000000000000 ) ) ;
#3686 = DIRECTION ( 'NONE',  ( 0.000000000000000000, 0.000000000000000000, -1.000000000000000000 ) ) ;
#3687 = CARTESIAN_POINT ( 'NONE',  ( 184.3994103300443328, 82.02159554764421046, -10.13810525658259465 ) ) ;
#3688 = AXIS2_PLACEMENT_3D ( 'NONE', #57880, #42390, #47306 ) ;
#3689 = CARTESIAN_POINT ( 'NONE',  ( -118.9468627709228912, 42.08677365399179848, 67.80319248315890945 ) ) ;
#3690 = CARTESIAN_POINT ( 'NONE',  ( -84.55783695959767954, 25.74181993349144904, -11.10319101795209029 ) ) ;
#3691 = FACE_OUTER_BOUND ( 'NONE', #25914, .T. ) ;
#3692 = AXIS2_PLACEMENT_3D ( 'NONE', #33582, #55008, #6830 ) ;
#3693 = CARTESIAN_POINT ( 'NONE',  ( -51.77431913897919458, 14.86466849149170955, 44.58036524786519550 ) ) ;
#3694 = ORIENTED_EDGE ( 'NONE', *, *, #20467, .T. ) ;
#3695 = ORIENTED_EDGE ( 'NONE', *, *, #26987, .F. ) ;
#3696 = FACE_OUTER_BOUND ( 'NONE', #32892, .T. ) ;
#3697 = LINE ( 'NONE', #61741, #36098 ) ;
#3698 = VECTOR ( 'NONE', #49701, 1000.000000000000000 ) ;
#3699 = CARTESIAN_POINT ( 'NONE',  ( 105.2351883444108722, 26.63316404209145460, 85.20707925349449852 ) ) ;
#3700 = CARTESIAN_POINT ( 'NONE',  ( -55.05276343752910151, -170.0000000000000000, 10.97277718246748890 ) ) ;
#3701 = EDGE_CURVE ( 'NONE', #25401, #56789, #25051, .T. ) ;
#3702 = CARTESIAN_POINT ( 'NONE',  ( 447.3372781065085633, 400.0000000000000568, -146.4497041420118251 ) ) ;
#3703 = CARTESIAN_POINT ( 'NONE',  ( 412.3372781065082791, 400.0000000000040927, 78.55029585798418168 ) ) ;
#3704 = CARTESIAN_POINT ( 'NONE',  ( -145.1827711476570641, 61.89240998680990913, 85.77519060852361577 ) ) ;
#3705 = EDGE_LOOP ( 'NONE', ( #55339, #15386, #56019, #65378, #27658 ) ) ;
#3706 = ORIENTED_EDGE ( 'NONE', *, *, #48102, .T. ) ;
#3707 = ORIENTED_EDGE ( 'NONE', *, *, #60071, .F. ) ;
#3708 = CARTESIAN_POINT ( 'NONE',  ( 175.5364600822697412, 73.17492830764774681, -92.34967047772518356 ) ) ;
#3709 = DIRECTION ( 'NONE',  ( 1.000000000000000000, 0.000000000000000000, 0.000000000000000000 ) ) ;
#3710 = CARTESIAN_POINT ( 'NONE',  ( -24.87827947785784133, 3.494138152041632583, 0.000000000000000000 ) ) ;
#3711 = B_SPLINE_CURVE_WITH_KNOTS ( 'NONE', 3,
 ( #43384, #22634, #7155, #22285, #5749, #44073, #64854, #28616, #65556, #27554, #11031, #48998, #39176, #64506, #11371, #43723, #11724, #28251, #22989, #33556, #16654, #65200, #21583, #54982, #16995, #17349, #27205, #6800, #38464, #59902, #38110, #50065, #16313, #33197, #54635, #6462, #65921, #49696, #38823, #60619, #1526, #44433, #37769, #34246 ),
 .UNSPECIFIED., .F., .F.,
 ( 4, 2, 2, 2, 2, 2, 2, 2, 2, 2, 2, 2, 1, 2, 2, 2, 2, 2, 2, 1, 2, 2, 4 ),
 ( 0.02381751147647563974, 0.02531129726520767523, 0.02605819015957369644, 0.02680508305393972113, 0.02829886884267175662, 0.02979265463140379211, 0.03053954752576980639, 0.03128644042013582066, 0.03278022620886785615, 0.03427401199759988470, 0.03576779778633192713, 0.03651469068069795182, 0.03726158357506398344, 0.03800847646943000813, 0.03875536936379603975, 0.04024915515252809606, 0.04174294094126015930, 0.04323672672999220867, 0.04398361962435823336, 0.04473051251872425804, 0.04547740541309028273, 0.04622429830745630741, 0.04771808409618833596 ),
 .UNSPECIFIED. ) ;
#3712 = CARTESIAN_POINT ( 'NONE',  ( -59.95412189755933952, 17.09836075175410386, 32.11962012825880919 ) ) ;
#3713 = CARTESIAN_POINT ( 'NONE',  ( -38.54712373114178803, 11.89174538567465689, -72.10478228046926574 ) ) ;
#3714 = DIRECTION ( 'NONE',  ( -0.000000000000000000, 0.000000000000000000, 1.000000000000000000 ) ) ;
#3715 = CARTESIAN_POINT ( 'NONE',  ( 9.288975942802414565, 6.379608420846960115, -12.42347880493715806 ) ) ;
#3716 = ORIENTED_EDGE ( 'NONE', *, *, #64221, .T. ) ;
#3717 = CARTESIAN_POINT ( 'NONE',  ( -0.3258398948454875876, 6.518608385615804579, -43.41939880400013863 ) ) ;
#3718 = CARTESIAN_POINT ( 'NONE',  ( 182.7720841008444381, 80.32850885226594073, 56.34244215664639199 ) ) ;
#3719 = CARTESIAN_POINT ( 'NONE',  ( -118.3960663196800880, 41.75130200162919891, 10.70744975955315148 ) ) ;
#3720 = CARTESIAN_POINT ( 'NONE',  ( -56.44201257846587083, -32.26641783793643725, 41.38025477438755928 ) ) ;
#3721 = CARTESIAN_POINT ( 'NONE',  ( 17.48889770758268014, 6.561062909825351674, 57.05045723885289988 ) ) ;
#3722 = CARTESIAN_POINT ( 'NONE',  ( 23.24047374271773236, 7.861801299833793166, -15.19526073016659140 ) ) ;
#3723 = CARTESIAN_POINT ( 'NONE',  ( 9.045716588192243890, 7.384596431530730420, 13.99132986342793572 ) ) ;
#3724 = EDGE_CURVE ( 'NONE', #45155, #23284, #31659, .T. ) ;
#3725 =( GEOMETRIC_REPRESENTATION_CONTEXT ( 3 ) GLOBAL_UNCERTAINTY_ASSIGNED_CONTEXT ( ( #66987 ) ) GLOBAL_UNIT_ASSIGNED_CONTEXT ( ( #56756, #15223, #36690 ) ) REPRESENTATION_CONTEXT ( 'NONE', 'WORKASPACE' ) );
#3726 = B_SPLINE_CURVE_WITH_KNOTS ( 'NONE', 3,
 ( #4730, #26196, #9327, #68744, #41681, #47630, #30437, #51886, #5075, #58202, #36063, #58531, #47975, #25522, #52233, #69084, #69441, #3699, #20561, #63829, #14942, #42024, #21257, #20917, #42368, #57175, #15641, #31143, #8990, #52578, #46606, #68087, #19887, #41345, #62797, #14601, #57518, #30788, #57860, #36407, #68421, #20223, #4397, #63484, #59564, #5428, #32167, #21944, #53936, #43734, #10692, #37781, #54991, #59916, #27566, #11735 ),
 .UNSPECIFIED., .F., .F.,
 ( 4, 2, 2, 2, 2, 2, 2, 2, 2, 2, 2, 2, 2, 2, 2, 2, 2, 2, 2, 2, 2, 2, 2, 2, 2, 2, 2, 4 ),
 ( 0.000000000000000000, 0.002104237472784967113, 0.003156356209177476474, 0.004208474945569985401, 0.005260593681962493461, 0.006312712418355004122, 0.007364831154747513049, 0.008416949891140022844, 0.01052118736392504070, 0.01157330610031757911, 0.01262542483671011927, 0.01367754357310265942, 0.01472966230949519784, 0.01683389978228026426, 0.01788601851867279574, 0.01893813725506532722, 0.01999025599145785870, 0.02104237472785039018, 0.02314661220063543579, 0.02419873093702797420, 0.02525084967342050915, 0.02630296840981304410, 0.02735508714620558252, 0.02840720588259811746, 0.02945932461899065241, 0.03051144335538318736, 0.03156356209177572231, 0.03366779956456074363 ),
 .UNSPECIFIED. ) ;
#3727 = ORIENTED_EDGE ( 'NONE', *, *, #39222, .F. ) ;
#3728 = AXIS2_PLACEMENT_3D ( 'NONE', #49624, #7078, #1816 ) ;
#3729 = SHAPE_DEFINITION_REPRESENTATION ( #23215, #36585 ) ;
#3730 = EDGE_CURVE ( 'NONE', #40116, #20254, #63256, .T. ) ;
#3731 = CARTESIAN_POINT ( 'NONE',  ( 48.11816970607237209, 43.69944786994017250, 40.00000000000003553 ) ) ;
#3732 = DIRECTION ( 'NONE',  ( 1.000000000000000000, 0.000000000000000000, 0.000000000000000000 ) ) ;
#3733 = CARTESIAN_POINT ( 'NONE',  ( -103.2164890789475606, 34.39030697009940951, -35.05845294305762394 ) ) ;
#3734 = CONTEXT_DEPENDENT_SHAPE_REPRESENTATION ( #48089, #21980 ) ;
#3735 = CARTESIAN_POINT ( 'NONE',  ( 188.4920037102894241, 87.93425473911916868, -42.51552582893779686 ) ) ;
#3736 = VERTEX_POINT ( 'NONE', #33589 ) ;
#3737 = CIRCLE ( 'NONE', #64433, 10.00000000000000000 ) ;
#3738 = ORIENTED_EDGE ( 'NONE', *, *, #14434, .T. ) ;
#3739 = AXIS2_PLACEMENT_3D ( 'NONE', #60067, #28413, #22097 ) ;
#3740 = CARTESIAN_POINT ( 'NONE',  ( -27.70562707895080479, 9.007984652865417274, -22.49608191275522628 ) ) ;
#3741 = B_SPLINE_CURVE_WITH_KNOTS ( 'NONE', 3,
 ( #26161, #58495, #46573, #63103 ),
 .UNSPECIFIED., .F., .F.,
 ( 4, 4 ),
 ( 0.1259919275528360028, 0.1829744153748751323 ),
 .UNSPECIFIED. ) ;
#3742 = AXIS2_PLACEMENT_3D ( 'NONE', #59163, #32448, #64805 ) ;
#3743 = CARTESIAN_POINT ( 'NONE',  ( 149.4165763529819344, 225.8585178651493663, 108.9999999999999858 ) ) ;
#3744 = EDGE_LOOP ( 'NONE', ( #59233, #13673, #7017, #48460 ) ) ;
#3745 = AXIS2_PLACEMENT_3D ( 'NONE', #53453, #68615, #21797 ) ;
#3746 = CARTESIAN_POINT ( 'NONE',  ( 163.9480004224415666, 64.17952544697072881, 94.44126775434629906 ) ) ;
#3747 = ADVANCED_FACE ( 'NONE', ( #45514 ), #66998, .F. ) ;
#3748 = ORIENTED_EDGE ( 'NONE', *, *, #63637, .F. ) ;
#3749 = CARTESIAN_POINT ( 'NONE',  ( 0.000000000000000000, 190.0000000000000000, 0.000000000000000000 ) ) ;
#3750 = DIRECTION ( 'NONE',  ( -1.000000000000000000, 0.000000000000000000, 0.000000000000000000 ) ) ;
#3751 = CARTESIAN_POINT ( 'NONE',  ( -152.9143627383495527, 68.46626892668658115, 44.91786962733564792 ) ) ;
#3752 = CIRCLE ( 'NONE', #29602, 243.4957430088094839 ) ;
#3753 = ADVANCED_FACE ( 'NONE', ( #59941 ), #6837, .T. ) ;
#3754 = EDGE_CURVE ( 'NONE', #4587, #18030, #61352, .T. ) ;
#3755 = DIRECTION ( 'NONE',  ( -1.000000000000000000, 0.000000000000000000, 0.000000000000000000 ) ) ;
#3756 = DIRECTION ( 'NONE',  ( -1.000000000000000000, -0.000000000000000000, -0.000000000000000000 ) ) ;
#3758 = ORIENTED_EDGE ( 'NONE', *, *, #8617, .T. ) ;
#3757 = CARTESIAN_POINT ( 'NONE',  ( 0.000000000000000000, 0.000000000000000000, 40.00000000000003553 ) ) ;
#3759 = DIRECTION ( 'NONE',  ( 6.405132834375901070E-16, -1.000000000000000000, -6.405132834375902056E-16 ) ) ;
#3760 = ORIENTED_EDGE ( 'NONE', *, *, #30873, .F. ) ;
#3761 = EDGE_LOOP ( 'NONE', ( #20378, #17915 ) ) ;
#3762 = DIRECTION ( 'NONE',  ( -1.000000000000000000, 0.000000000000000000, 0.000000000000000000 ) ) ;
#3763 = CARTESIAN_POINT ( 'NONE',  ( -32.29264255508331871, 10.75330965162339147, -89.05198297107156691 ) ) ;
#3765 = ORIENTED_EDGE ( 'NONE', *, *, #65097, .T. ) ;
#3764 = CARTESIAN_POINT ( 'NONE',  ( -132.5976199670998881, 52.30296609017646148, 61.59159971231706265 ) ) ;
#3766 = CARTESIAN_POINT ( 'NONE',  ( -104.6733177284973522, 35.14812073506915624, 84.57539980412138902 ) ) ;
#3767 = FACE_OUTER_BOUND ( 'NONE', #30666, .T. ) ;
#3768 = ORIENTED_EDGE ( 'NONE', *, *, #68082, .T. ) ;
#3769 = CYLINDRICAL_SURFACE ( 'NONE', #69250, 65.00000000000000000 ) ;
#3770 = CARTESIAN_POINT ( 'NONE',  ( -131.2955621888335429, 51.38237199780173370, -74.48357675656784238 ) ) ;
#3772 = CARTESIAN_POINT ( 'NONE',  ( 112.1100957124161397, 30.86846953551571104, 29.83213851092833835 ) ) ;
#3771 = VECTOR ( 'NONE', #23467, 1000.000000000000000 ) ;
#3773 = CARTESIAN_POINT ( 'NONE',  ( -71.90777365577140756, 21.14201501538314076, 41.38025477438755928 ) ) ;
#3774 = CARTESIAN_POINT ( 'NONE',  ( 64.69738688745238164, 14.10375742873388383, -62.75224125784992424 ) ) ;
#3775 = VERTEX_POINT ( 'NONE', #7191 ) ;
#3776 = VERTEX_POINT ( 'NONE', #34281 ) ;
#3777 = CIRCLE ( 'NONE', #61078, 4.171999999999999709 ) ;
#3778 = CARTESIAN_POINT ( 'NONE',  ( 0.000000000000000000, 0.000000000000000000, 0.000000000000000000 ) ) ;
#3779 = CARTESIAN_POINT ( 'NONE',  ( -166.7049310409072405, 80.25944422923581101, -38.31930149277814479 ) ) ;
#3780 = CARTESIAN_POINT ( 'NONE',  ( -31.90315521289150524, 56.64813493366005304, 43.58025477438756923 ) ) ;
#3781 = AXIS2_PLACEMENT_3D ( 'NONE', #3700, #24820, #24487 ) ;
#3782 = CARTESIAN_POINT ( 'NONE',  ( -48.84172885504641215, 13.10362374101116956, -92.17860550746377157 ) ) ;
#3783 = CARTESIAN_POINT ( 'NONE',  ( -50.65633458199173589, 14.58352428224076114, -90.32529372262172274 ) ) ;
#3784 = ADVANCED_FACE ( 'NONE', ( #7893 ), #49385, .T. ) ;
#3785 = CARTESIAN_POINT ( 'NONE',  ( -72.62976060914719767, -18.74780984163136566, 170.0000000000000000 ) ) ;
#3786 = CARTESIAN_POINT ( 'NONE',  ( 69.72789637502502558, 15.37065610545704253, -46.57588281048915491 ) ) ;
#3787 = VECTOR ( 'NONE', #54739, 1000.000000000000000 ) ;
#3788 = FACE_OUTER_BOUND ( 'NONE', #19947, .T. ) ;
#3789 = CARTESIAN_POINT ( 'NONE',  ( 210.6475357757681763, 114.8748261044495678, 58.97869289604779652 ) ) ;
#3790 = EDGE_LOOP ( 'NONE', ( #19909, #52215, #66218, #50084 ) ) ;
#3792 = CARTESIAN_POINT ( 'NONE',  ( 0.000000000000000000, 0.000000000000000000, 0.000000000000000000 ) ) ;
#3791 = AXIS2_PLACEMENT_3D ( 'NONE', #56338, #3233, #51757 ) ;
#3793 = ORIENTED_EDGE ( 'NONE', *, *, #13114, .T. ) ;
#3794 = EDGE_CURVE ( 'NONE', #9029, #24506, #17753, .T. ) ;
#3795 = CARTESIAN_POINT ( 'NONE',  ( 79.40386128751609363, 18.13359811229536689, -95.00000000000133582 ) ) ;
#3796 = VECTOR ( 'NONE', #59516, 1000.000000000000000 ) ;
#3797 = CARTESIAN_POINT ( 'NONE',  ( 79.12879321038292346, 18.04902206524926811, 64.29254397640617924 ) ) ;
#3798 = EDGE_LOOP ( 'NONE', ( #4231, #15355, #58430, #58254 ) ) ;
#3799 = CARTESIAN_POINT ( 'NONE',  ( -83.74395355181556511, 24.32073993326131855, -90.76757344677447747 ) ) ;
#3800 = DIRECTION ( 'NONE',  ( -0.9639628606958512425, -0.2660368455666826670, 0.000000000000000000 ) ) ;
#3801 = DIRECTION ( 'NONE',  ( -1.000000000000000000, -1.156482317317871725E-15, 0.000000000000000000 ) ) ;
#3802 = CARTESIAN_POINT ( 'NONE',  ( -17.50000000000000000, -17.50000000000000000, 20.00000000000000000 ) ) ;
#3803 = CARTESIAN_POINT ( 'NONE',  ( 34.83825437341838693, 7.859462995505725580, 4.597600571500676025 ) ) ;
#3804 = CARTESIAN_POINT ( 'NONE',  ( -452.6627218934914367, 399.9999999999998863, -146.4497041420118251 ) ) ;
#3805 = AXIS2_PLACEMENT_3D ( 'NONE', #7710, #9695, #9340 ) ;
#3806 = DIRECTION ( 'NONE',  ( -0.000000000000000000, -0.000000000000000000, -1.000000000000000000 ) ) ;
#3807 = ORIENTED_EDGE ( 'NONE', *, *, #56294, .T. ) ;
#3808 = CARTESIAN_POINT ( 'NONE',  ( -118.9946151492785162, 43.29610461813053490, -93.12245335861705087 ) ) ;
#3809 = ORIENTED_EDGE ( 'NONE', *, *, #30277, .F. ) ;
#3810 = CARTESIAN_POINT ( 'NONE',  ( 63.01563776193091826, -170.0000000000000000, 44.81296093922130552 ) ) ;
#3811 = CARTESIAN_POINT ( 'NONE',  ( 11.21312910819262498, 7.403355431336988701, -75.82688043949028156 ) ) ;
#3812 = CARTESIAN_POINT ( 'NONE',  ( -189.2346268516247392, 107.0830361517164988, 11.78999996383570092 ) ) ;
#3813 = EDGE_CURVE ( 'NONE', #2957, #57714, #49733, .T. ) ;
#3814 = CARTESIAN_POINT ( 'NONE',  ( 15.78827728214693060, 6.500811158483329244, 71.85925826316895382 ) ) ;
#3815 = CARTESIAN_POINT ( 'NONE',  ( -15.32550079334879456, 7.496023944924843363, -70.00453783701779287 ) ) ;
#3816 = CARTESIAN_POINT ( 'NONE',  ( 0.000000000000000000, 0.000000000000000000, -5.000000000000000000 ) ) ;
#3817 = EDGE_CURVE ( 'NONE', #2651, #47695, #50454, .T. ) ;
#3818 = ADVANCED_FACE ( 'NONE', ( #1217 ), #1932, .T. ) ;
#3819 = ORIENTED_EDGE ( 'NONE', *, *, #66204, .F. ) ;
#3820 = CARTESIAN_POINT ( 'NONE',  ( 684.5501828525930250, 847.8234287996408511, 698.5068267248682332 ) ) ;
#3821 = ADVANCED_FACE ( 'NONE', ( #39549 ), #2611, .T. ) ;
#3822 = CARTESIAN_POINT ( 'NONE',  ( -156.4797890011541313, 71.69341087347112307, 62.28821244478771746 ) ) ;
#3823 = CARTESIAN_POINT ( 'NONE',  ( 173.8623159076319382, 72.97967239795016781, -18.92509683218599292 ) ) ;
#3824 = CARTESIAN_POINT ( 'NONE',  ( -119.6995109608661352, 42.54844499216734022, 33.88379391638913773 ) ) ;
#3825 = CARTESIAN_POINT ( 'NONE',  ( 0.000000000000000000, 6.928203230275506108, 4.000000000000006217 ) ) ;
#3826 = ORIENTED_EDGE ( 'NONE', *, *, #64880, .T. ) ;
#3827 = CARTESIAN_POINT ( 'NONE',  ( -174.7817412490651918, 90.52199442492062076, -76.38243644640435548 ) ) ;
#3828 = CARTESIAN_POINT ( 'NONE',  ( 127.5112704970419486, 38.87838270771662508, 94.71298516231503584 ) ) ;
#3829 = CARTESIAN_POINT ( 'NONE',  ( 116.5096233816161941, 31.89062767870468917, 32.98306140069937697 ) ) ;
#3830 = CARTESIAN_POINT ( 'NONE',  ( 73.95984195137785377, 12.15131637179898583, 41.38025477438755928 ) ) ;
#3831 = VECTOR ( 'NONE', #5641, 1000.000000000000114 ) ;
#3832 = B_SPLINE_CURVE_WITH_KNOTS ( 'NONE', 3,
 ( #4490, #35113, #59611, #11427, #53647, #6154, #65621, #64917, #53983, #894, #43096, #22347, #38170, #186, #33615, #43784, #37832, #59273, #32552, #21997, #60329, #27616, #37477, #59967, #16023, #28314, #65258, #42751, #17051, #38521, #10746, #26927, #11784, #11090, #32897, #55041, #6864, #16712, #48701, #32216, #54335, #33260, #5472, #48353, #5809, #21642, #49059, #17408 ),
 .UNSPECIFIED., .F., .F.,
 ( 4, 2, 2, 2, 2, 2, 2, 2, 2, 2, 2, 2, 2, 2, 2, 2, 2, 2, 2, 2, 2, 2, 2, 4 ),
 ( 0.000000000000000000, 0.001591515129442197789, 0.003183030258884395579, 0.003978787823605494690, 0.004774545388326592935, 0.006366060517768843199, 0.007957575647211093464, 0.009549090776653343729, 0.01034484834137447233, 0.01114060590609559920, 0.01193636347081672780, 0.01273212103553785467, 0.01432363616498015003, 0.01591515129442242979, 0.01671090885914355492, 0.01750666642386468699, 0.01830242398858581906, 0.01909818155330694767, 0.02068969668274926385, 0.02148545424747042368, 0.02228121181219158004, 0.02387272694163383377, 0.02466848450635492074, 0.02546424207107600771 ),
 .UNSPECIFIED. ) ;
#3833 = CARTESIAN_POINT ( 'NONE',  ( -123.4416615615273116, 44.90042688650401459, -62.16667402822235289 ) ) ;
#3834 = EDGE_CURVE ( 'NONE', #64271, #1254, #23024, .T. ) ;
#3835 = ORIENTED_EDGE ( 'NONE', *, *, #21190, .F. ) ;
#3836 = CARTESIAN_POINT ( 'NONE',  ( 198.7029050523553053, 98.46895521196215384, 41.24356943943517706 ) ) ;
#3837 = CARTESIAN_POINT ( 'NONE',  ( 117.6916924104495479, 32.48309187151382105, -69.25116632857373133 ) ) ;
#3838 = AXIS2_PLACEMENT_3D ( 'NONE', #23707, #33916, #6824 ) ;
#3839 = FACE_OUTER_BOUND ( 'NONE', #25670, .T. ) ;
#3840 = CARTESIAN_POINT ( 'NONE',  ( 140.4641697461913168, 46.75994457266055093, 13.75233122400834240 ) ) ;
#3841 = FACE_OUTER_BOUND ( 'NONE', #20050, .T. ) ;
#3842 = EDGE_CURVE ( 'NONE', #19257, #9227, #44476, .T. ) ;
#3843 = EDGE_CURVE ( 'NONE', #35195, #22151, #28650, .T. ) ;
#3844 = AXIS2_PLACEMENT_3D ( 'NONE', #9257, #52168, #68354 ) ;
#3845 = ORIENTED_EDGE ( 'NONE', *, *, #1380, .F. ) ;
#3846 = AXIS2_PLACEMENT_3D ( 'NONE', #29576, #2511, #51044 ) ;
#3847 = FACE_OUTER_BOUND ( 'NONE', #29740, .T. ) ;
#3848 = AXIS2_PLACEMENT_3D ( 'NONE', #39912, #7213, #45186 ) ;
#3849 = ORIENTED_EDGE ( 'NONE', *, *, #26324, .F. ) ;
#3850 = CARTESIAN_POINT ( 'NONE',  ( 99.71998884745383407, 0.000000000000000000, 7.478223336038896996 ) ) ;
#3851 = CARTESIAN_POINT ( 'NONE',  ( 141.3359578064694233, 46.12776601070872573, 91.36406821307745929 ) ) ;
#3852 = AXIS2_PLACEMENT_3D ( 'NONE', #4188, #25656, #42829 ) ;
#3854 = EDGE_LOOP ( 'NONE', ( #26584, #28103, #17107, #64079, #38779, #9643, #4054 ) ) ;
#3853 = DIRECTION ( 'NONE',  ( -1.000000000000000000, 0.000000000000000000, 0.000000000000000000 ) ) ;
#3855 = CARTESIAN_POINT ( 'NONE',  ( -180.4643341113398094, 95.69224917234934935, 39.87708186227253293 ) ) ;
#3856 = CARTESIAN_POINT ( 'NONE',  ( -31.11269837220809364, -15.55634918610397754, 2.000000000000001776 ) ) ;
#3857 = CARTESIAN_POINT ( 'NONE',  ( 117.6924004117966263, 33.61107268965020722, -44.43629281926136088 ) ) ;
#3858 = VERTEX_POINT ( 'NONE', #65592 ) ;
#3859 = CARTESIAN_POINT ( 'NONE',  ( 28.73969596345624211, -50.76944258518214070, 27.58472369392173107 ) ) ;
#3860 = ADVANCED_BREP_SHAPE_REPRESENTATION ( '', ( #63623, #66832 ), #10752 ) ;
#3861 = CARTESIAN_POINT ( 'NONE',  ( 55.52491259852590133, 12.08515669078798460, 90.50025533462843441 ) ) ;
#3862 = CYLINDRICAL_SURFACE ( 'NONE', #39982, 5.000000000000000888 ) ;
#3863 = CARTESIAN_POINT ( 'NONE',  ( 53.32245423372562243, 37.19594572654711584, 3.061616997868437868E-16 ) ) ;
#3864 = DIRECTION ( 'NONE',  ( -0.000000000000000000, -0.000000000000000000, -1.000000000000000000 ) ) ;
#3865 = CARTESIAN_POINT ( 'NONE',  ( 151.1607415860635228, 52.90668588398091288, 59.66759169391354334 ) ) ;
#3866 = DIRECTION ( 'NONE',  ( -1.000000000000000000, -0.000000000000000000, -0.000000000000000000 ) ) ;
#3867 = EDGE_LOOP ( 'NONE', ( #36108, #28405, #537, #61706 ) ) ;
#3868 = CARTESIAN_POINT ( 'NONE',  ( -97.49665543375864729, 31.53324358035376918, 70.66128095698653055 ) ) ;
#3869 = LINE ( 'NONE', #20730, #10810 ) ;
#3870 = ORIENTED_EDGE ( 'NONE', *, *, #47160, .T. ) ;
#3871 = CARTESIAN_POINT ( 'NONE',  ( -40.24154210098803475, 63.23235722614447951, 41.38025477438755928 ) ) ;
#3872 = CARTESIAN_POINT ( 'NONE',  ( -61.09101882797757099, 16.38378112650486784, 87.01151449968797635 ) ) ;
#3873 = CARTESIAN_POINT ( 'NONE',  ( 107.0447263249841257, 28.53200276018954895, 43.89932290840497586 ) ) ;
#3874 = PLANE ( 'NONE',  #706 ) ;
#3875 = DIRECTION ( 'NONE',  ( -0.000000000000000000, 0.000000000000000000, -1.000000000000000000 ) ) ;
#3876 = CARTESIAN_POINT ( 'NONE',  ( 188.5651904823862139, 88.01586411309102687, 10.57501070353481509 ) ) ;
#3877 = CARTESIAN_POINT ( 'NONE',  ( 0.000000000000000000, 70.00000000000000000, 0.000000000000000000 ) ) ;
#3878 = CARTESIAN_POINT ( 'NONE',  ( 173.6718135456487175, 71.42581476597409562, 11.14533547892623488 ) ) ;
#3879 = ORIENTED_EDGE ( 'NONE', *, *, #36691, .F. ) ;
#3880 = EDGE_CURVE ( 'NONE', #19652, #60812, #44141, .T. ) ;
#3881 = AXIS2_PLACEMENT_3D ( 'NONE', #38901, #22708, #12166 ) ;
#3882 = CARTESIAN_POINT ( 'NONE',  ( 0.000000000000000000, 0.000000000000000000, 0.000000000000000000 ) ) ;
#3883 = ORIENTED_EDGE ( 'NONE', *, *, #65380, .F. ) ;
#3884 = CARTESIAN_POINT ( 'NONE',  ( 280.0000000000000000, -21.42428528562853529, -4.999999999999990230 ) ) ;
#3885 = DIRECTION ( 'NONE',  ( -0.04486483035050447404, -0.9989930665413151445, 0.000000000000000000 ) ) ;
#3886 = CARTESIAN_POINT ( 'NONE',  ( 0.000000000000000000, 0.000000000000000000, 0.000000000000000000 ) ) ;
#3887 = DIRECTION ( 'NONE',  ( 0.000000000000000000, -0.000000000000000000, -1.000000000000000000 ) ) ;
#3888 = CARTESIAN_POINT ( 'NONE',  ( 15.78827728214693416, 7.507518794609575608, 45.01470767270524931 ) ) ;
#3889 = CARTESIAN_POINT ( 'NONE',  ( -109.7643866341847172, 37.89854104106755273, -16.22134575533492651 ) ) ;
#3890 = VECTOR ( 'NONE', #56233, 1000.000000000000000 ) ;
#3891 = ORIENTED_EDGE ( 'NONE', *, *, #46841, .F. ) ;
#3892 = DIRECTION ( 'NONE',  ( 0.000000000000000000, -6.123233995736762338E-17, 1.000000000000000000 ) ) ;
#3893 = CARTESIAN_POINT ( 'NONE',  ( 199.6034222400379861, 99.61037244215080477, -91.99663670549787753 ) ) ;
#3894 = EDGE_LOOP ( 'NONE', ( #61364, #1472, #45906, #56335 ) ) ;
#3895 = AXIS2_PLACEMENT_3D ( 'NONE', #1732, #33745, #7004 ) ;
#3896 = ORIENTED_EDGE ( 'NONE', *, *, #60752, .F. ) ;
#3897 = ADVANCED_FACE ( 'NONE', ( #56414 ), #3303, .T. ) ;
#3898 = B_SPLINE_CURVE_WITH_KNOTS ( 'NONE', 3,
 ( #34732, #13272, #3066, #45964, #56169, #19575, #7986, #35411, #56877, #2712, #30145, #24174, #51595, #45623, #3402, #41032, #53973, #52612, #5116, #43087, #20957, #26579, #11080, #64203, #16015, #59266, #32209, #10387, #41726, #58573, #9721, #37824, #36447, #48693, #4437, #21635, #69127, #57899, #63184, #15339, #64556, #5463, #31184, #37467, #31859, #25899, #47328, #42410, #52949, #42744 ),
 .UNSPECIFIED., .F., .F.,
 ( 4, 2, 2, 2, 2, 2, 2, 2, 2, 2, 2, 2, 2, 2, 2, 2, 2, 2, 2, 2, 2, 2, 2, 2, 4 ),
 ( 0.03296461860586794024, 0.03492857779726578349, 0.03689253698866362674, 0.03885649618006146999, 0.04082045537145931324, 0.04278441456285715649, 0.04376639415855611281, 0.04474837375425506913, 0.04573035334995402545, 0.04671233294565298177, 0.04720332274350245300, 0.04769431254135192422, 0.04867629213705086666, 0.04965827173274981604, 0.05064025132844876542, 0.05162223092414770786, 0.05260421051984665031, 0.05358619011554559969, 0.05456816971124454907, 0.05555014930694349151, 0.05653212890264243395, 0.05849608809404029108, 0.06046004728543815515, 0.06242400647683601922, 0.06438796566823387635 ),
 .UNSPECIFIED. ) ;
#3899 = CARTESIAN_POINT ( 'NONE',  ( -155.7495771807047333, 69.65980221699319941, 34.03292314250037975 ) ) ;
#3900 = DIRECTION ( 'NONE',  ( -0.000000000000000000, 1.000000000000000000, -0.000000000000000000 ) ) ;
#3901 = CARTESIAN_POINT ( 'NONE',  ( 173.7227242028391174, 71.47307702680407715, -18.34505588493575345 ) ) ;
#3902 = SURFACE_SIDE_STYLE ('',( #14792 ) ) ;
#3903 = CIRCLE ( 'NONE', #523, 65.36598343705435354 ) ;
#3904 = LINE ( 'NONE', #29250, #45362 ) ;
#3905 = EDGE_CURVE ( 'NONE', #17632, #45870, #3997, .T. ) ;
#3906 = VERTEX_POINT ( 'NONE', #13515 ) ;
#3907 = DIRECTION ( 'NONE',  ( -0.000000000000000000, 1.000000000000000000, -0.000000000000000000 ) ) ;
#3908 = ORIENTED_EDGE ( 'NONE', *, *, #60509, .T. ) ;
#3909 = CARTESIAN_POINT ( 'NONE',  ( 212.1962110266999559, 117.2292732107321314, 9.486508075812803753 ) ) ;
#3910 = CARTESIAN_POINT ( 'NONE',  ( 8.287863202055538281, 7.382585476140732794, 64.84750261709777419 ) ) ;
#3911 = CARTESIAN_POINT ( 'NONE',  ( 204.6977192012829789, 106.3443248447423599, 29.20772073876942088 ) ) ;
#3912 = FACE_BOUND ( 'NONE', #27307, .T. ) ;
#3913 = VERTEX_POINT ( 'NONE', #61691 ) ;
#3914 = VERTEX_POINT ( 'NONE', #8237 ) ;
#3915 = CARTESIAN_POINT ( 'NONE',  ( 110.3272854519634052, -21.42428528562852463, 5.000000000000005329 ) ) ;
#3916 = CARTESIAN_POINT ( 'NONE',  ( -119.6460721175663480, 43.69798148487400624, 87.64758983319130436 ) ) ;
#3917 = CARTESIAN_POINT ( 'NONE',  ( -166.3175803736862406, 79.86140754556168986, -12.19923997767886981 ) ) ;
#3918 = CARTESIAN_POINT ( 'NONE',  ( -31.43908319763710679, 9.591432048623758533, 45.21645440618919309 ) ) ;
#3919 = CARTESIAN_POINT ( 'NONE',  ( 11.47034038687561441, 6.400817013728348215, 85.06273559740630219 ) ) ;
#3920 = EDGE_CURVE ( 'NONE', #35022, #39565, #636, .T. ) ;
#3921 = B_SPLINE_CURVE_WITH_KNOTS ( 'NONE', 3,
 ( #27555, #33895, #6801, #18755, #66959, #33557 ),
 .UNSPECIFIED., .F., .F.,
 ( 4, 2, 4 ),
 ( 0.03218945466321621734, 0.06469840457090983432, 0.09720735447860343048 ),
 .UNSPECIFIED. ) ;
#3922 = CARTESIAN_POINT ( 'NONE',  ( 22.25657943806483274, 7.801867731668604478, 94.99999999999866418 ) ) ;
#3923 = ORIENTED_EDGE ( 'NONE', *, *, #39148, .F. ) ;
#3924 = EDGE_CURVE ( 'NONE', #671, #69067, #51148, .T. ) ;
#3925 = CARTESIAN_POINT ( 'NONE',  ( 13.24564585880136036, -63.65041531508826012, 170.0000000000000000 ) ) ;
#3926 = CARTESIAN_POINT ( 'NONE',  ( -95.05546640093037070, 29.25972325950976582, 62.78387324367114530 ) ) ;
#3927 = ORIENTED_EDGE ( 'NONE', *, *, #12373, .F. ) ;
#3928 = DIRECTION ( 'NONE',  ( 0.000000000000000000, 0.000000000000000000, 1.000000000000000000 ) ) ;
#3929 = ORIENTED_EDGE ( 'NONE', *, *, #39789, .T. ) ;
#3930 = AXIS2_PLACEMENT_3D ( 'NONE', #64672, #21748, #44244 ) ;
#3931 = CARTESIAN_POINT ( 'NONE',  ( -60.98168946575806615, 17.40090852531920618, -11.25214144170228714 ) ) ;
#3932 = ORIENTED_EDGE ( 'NONE', *, *, #3096, .T. ) ;
#3933 = VECTOR ( 'NONE', #53497, 1000.000000000000000 ) ;
#3934 = ORIENTED_EDGE ( 'NONE', *, *, #8106, .F. ) ;
#3935 = CARTESIAN_POINT ( 'NONE',  ( 8.848532525911927848, 6.377649276597439965, -40.14341413102923894 ) ) ;
#3936 = CARTESIAN_POINT ( 'NONE',  ( 55.65793654284613012, 50.28674377798307660, 43.58025477438756923 ) ) ;
#3937 = CARTESIAN_POINT ( 'NONE',  ( 18.19980344696536534, 6.589834367837005935, 3.564186700565433519 ) ) ;
#3938 = CIRCLE ( 'NONE', #23016, 65.00000000000000000 ) ;
#3939 = VECTOR ( 'NONE', #54041, 1000.000000000000000 ) ;
#3940 = VERTEX_POINT ( 'NONE', #13851 ) ;
#3941 = CONICAL_SURFACE ( 'NONE', #67971, 74.95140232871122521, 0.8777644062502172329 ) ;
#3942 = CARTESIAN_POINT ( 'NONE',  ( -35.68454966275956508, 10.32676244612189187, 85.21450729991012452 ) ) ;
#3943 = DIRECTION ( 'NONE',  ( -0.8410447872859948548, 0.000000000000000000, 0.5409654940743040541 ) ) ;
#3944 = AXIS2_PLACEMENT_3D ( 'NONE', #67199, #40779, #62236 ) ;
#3945 = LINE ( 'NONE', #57754, #60605 ) ;
#3946 = CARTESIAN_POINT ( 'NONE',  ( 106.0171289417044136, 26.97542621030655141, -37.22168915489021401 ) ) ;
#3947 = CARTESIAN_POINT ( 'NONE',  ( 444.9999999999999432, -35.00000000000000000, -2.000000000000000000 ) ) ;
#3948 = CARTESIAN_POINT ( 'NONE',  ( -173.1211646369891355, 88.63826465341151106, -88.40105834567734178 ) ) ;
#3949 = EDGE_LOOP ( 'NONE', ( #17413, #41981, #67353, #11189 ) ) ;
#3950 = PRODUCT_DEFINITION ( 'UNKNOWN', '', #68169, #43669 ) ;
#3951 = CARTESIAN_POINT ( 'NONE',  ( -20.55634918610411077, -46.66904755831208718, 0.000000000000000000 ) ) ;
#3952 = CARTESIAN_POINT ( 'NONE',  ( -80.56139928459657540, 24.13290941644247667, -62.19941343312095228 ) ) ;
#3953 = DIRECTION ( 'NONE',  ( 0.000000000000000000, 0.000000000000000000, -1.000000000000000000 ) ) ;
#3954 = DIRECTION ( 'NONE',  ( 1.000000000000000000, 0.000000000000000000, 0.000000000000000000 ) ) ;
#3955 = DIRECTION ( 'NONE',  ( -0.000000000000000000, -1.000000000000000000, -0.000000000000000000 ) ) ;
#3956 = LINE ( 'NONE', #25073, #49414 ) ;
#3957 = CARTESIAN_POINT ( 'NONE',  ( -152.5046761101291679, 66.76407727525179325, 18.25504938878692940 ) ) ;
#3958 = CARTESIAN_POINT ( 'NONE',  ( -118.4470345550925998, 42.96051736048243441, -70.30058100330663251 ) ) ;
#3959 = EDGE_CURVE ( 'NONE', #38702, #53656, #25115, .T. ) ;
#3960 = CARTESIAN_POINT ( 'NONE',  ( -10.96274578891745755, -22.46815979931523799, 0.000000000000000000 ) ) ;
#3961 = DIRECTION ( 'NONE',  ( -0.000000000000000000, 1.000000000000000000, -0.000000000000000000 ) ) ;
#3962 = CARTESIAN_POINT ( 'NONE',  ( -104.5827168854524416, 33.96561401163047123, 30.86578353306401112 ) ) ;
#3963 = ORIENTED_EDGE ( 'NONE', *, *, #8078, .F. ) ;
#3964 = EDGE_CURVE ( 'NONE', #11003, #3736, #67338, .T. ) ;
#3965 = CARTESIAN_POINT ( 'NONE',  ( -62.55024818870805348, 17.87229771727388794, 91.88754048207763958 ) ) ;
#3966 = EDGE_LOOP ( 'NONE', ( #4112, #51745 ) ) ;
#3967 = CARTESIAN_POINT ( 'NONE',  ( 198.8687991397276562, 98.67887821384415759, -21.70767789263648950 ) ) ;
#3968 = VERTEX_POINT ( 'NONE', #47233 ) ;
#3969 = CARTESIAN_POINT ( 'NONE',  ( -145.3246383987844865, 62.00818849034185121, 5.146554988373365447 ) ) ;
#3970 = LINE ( 'NONE', #25087, #24901 ) ;
#3971 = DIRECTION ( 'NONE',  ( -1.000000000000000000, 0.000000000000000000, 0.000000000000000000 ) ) ;
#3972 = LINE ( 'NONE', #57436, #13122 ) ;
#3973 = CARTESIAN_POINT ( 'NONE',  ( 139.7883986595927865, 46.32091287009615144, -48.11977978458424587 ) ) ;
#3974 = CARTESIAN_POINT ( 'NONE',  ( -15.67984581961064450, 63.08044415722863363, 170.0000000000000000 ) ) ;
#3975 = CARTESIAN_POINT ( 'NONE',  ( 198.0640335990182450, 97.66860687174101940, 93.90131546401161700 ) ) ;
#3976 = CARTESIAN_POINT ( 'NONE',  ( 8.478575283864733692, 7.382882227715644063, -41.32250106610652551 ) ) ;
#3977 = DIRECTION ( 'NONE',  ( -0.000000000000000000, -0.000000000000000000, 1.000000000000000000 ) ) ;
#3978 = CARTESIAN_POINT ( 'NONE',  ( 129.6961120139404215, 38.96846414226720157, -49.76800638012151268 ) ) ;
#3979 = EDGE_LOOP ( 'NONE', ( #60158, #1057, #656, #3707 ) ) ;
#3980 = ORIENTED_EDGE ( 'NONE', *, *, #34314, .F. ) ;
#3981 = EDGE_CURVE ( 'NONE', #51672, #48751, #63078, .T. ) ;
#3982 = CARTESIAN_POINT ( 'NONE',  ( 178.4097654444205432, 77.35573068857576118, 83.48439424739329695 ) ) ;
#3983 = DIRECTION ( 'NONE',  ( 0.8584487936018728726, -0.5128992774058949156, 0.000000000000000000 ) ) ;
#3984 = CARTESIAN_POINT ( 'NONE',  ( -29.51060362117876679, 9.282716514427262311, -76.91369189782112414 ) ) ;
#3985 = EDGE_CURVE ( 'NONE', #26979, #34764, #36288, .T. ) ;
#3986 = EDGE_CURVE ( 'NONE', #49220, #59826, #14882, .T. ) ;
#3987 = AXIS2_PLACEMENT_3D ( 'NONE', #45053, #29926, #14093 ) ;
#3988 = CARTESIAN_POINT ( 'NONE',  ( 13.84937401517046851, 6.446378549072246500, 17.91938108381891936 ) ) ;
#3989 = CYLINDRICAL_SURFACE ( 'NONE', #60363, 246.3582898394606957 ) ;
#3990 = VECTOR ( 'NONE', #9870, 1000.000000000000000 ) ;
#3991 = AXIS2_PLACEMENT_3D ( 'NONE', #255, #64636, #38596 ) ;
#3992 = CARTESIAN_POINT ( 'NONE',  ( 0.000000000000000000, 0.000000000000000000, -50.00000000000000000 ) ) ;
#3993 = CARTESIAN_POINT ( 'NONE',  ( 174.6127059037622189, 72.30368563770913681, -74.39996846163762712 ) ) ;
#3994 = CARTESIAN_POINT ( 'NONE',  ( 0.000000000000000000, 0.000000000000000000, 40.00000000000003553 ) ) ;
#3995 = CARTESIAN_POINT ( 'NONE',  ( 88.52345267551656605, 20.07594890262054577, -23.73786243512815020 ) ) ;
#3996 = CARTESIAN_POINT ( 'NONE',  ( -25.07901552294941894, 9.649193085547803861, 68.54352610857644379 ) ) ;
#3997 = LINE ( 'NONE', #8590, #30718 ) ;
#3998 =( GEOMETRIC_REPRESENTATION_CONTEXT ( 3 ) GLOBAL_UNCERTAINTY_ASSIGNED_CONTEXT ( ( #41612 ) ) GLOBAL_UNIT_ASSIGNED_CONTEXT ( ( #41278, #57115, #8928 ) ) REPRESENTATION_CONTEXT ( 'NONE', 'WORKASPACE' ) );
#3999 = DIRECTION ( 'NONE',  ( -1.000000000000000000, -0.000000000000000000, -0.000000000000000000 ) ) ;
#4000 = AXIS2_PLACEMENT_3D ( 'NONE', #32142, #21921, #69063 ) ;
#4001 = ORIENTED_EDGE ( 'NONE', *, *, #55018, .T. ) ;
#4002 = LINE ( 'NONE', #9970, #39539 ) ;
#4003 = DIRECTION ( 'NONE',  ( -0.000000000000000000, 1.000000000000000000, -0.000000000000000000 ) ) ;
#4004 = CARTESIAN_POINT ( 'NONE',  ( -1.368053087914143706, -58.32353603131943487, 27.58472369367942889 ) ) ;
#4005 = CARTESIAN_POINT ( 'NONE',  ( -55.05276343752909440, 14.68156374112638041, -35.21632399845986328 ) ) ;
#4006 = DIRECTION ( 'NONE',  ( -0.000000000000000000, -0.000000000000000000, 1.000000000000000000 ) ) ;
#4007 = CYLINDRICAL_SURFACE ( 'NONE', #6388, 23.50000000000000000 ) ;
#4008 = ORIENTED_EDGE ( 'NONE', *, *, #30408, .F. ) ;
#4009 = ADVANCED_FACE ( 'NONE', ( #3640 ), #46547, .F. ) ;
#4010 = CARTESIAN_POINT ( 'NONE',  ( -78.66644367742111399, 22.32174330031316956, 45.41820113967312977 ) ) ;
#4011 = CARTESIAN_POINT ( 'NONE',  ( -58.33245019990696534, 15.58496056636070470, 71.42426283422710753 ) ) ;
#4012 = ORIENTED_EDGE ( 'NONE', *, *, #21210, .F. ) ;
#4013 = ORIENTED_EDGE ( 'NONE', *, *, #1334, .F. ) ;
#4014 = CARTESIAN_POINT ( 'NONE',  ( -149.5074843970971301, 64.17983161892345834, 30.72082123989904900 ) ) ;
#4015 = CARTESIAN_POINT ( 'NONE',  ( 444.9999999999999432, 225.0000000000000000, 380.0000000000000000 ) ) ;
#4016 = CARTESIAN_POINT ( 'NONE',  ( 133.8566784816069060, 42.60093787723656789, -89.71241211332301191 ) ) ;
#4017 = VERTEX_POINT ( 'NONE', #31083 ) ;
#4018 = FACE_BOUND ( 'NONE', #5277, .T. ) ;
#4019 = PLANE ( 'NONE',  #57823 ) ;
#4020 = CARTESIAN_POINT ( 'NONE',  ( 56.29445224195347919, 12.24017809212662655, -46.58514210915670617 ) ) ;
#4021 = CARTESIAN_POINT ( 'NONE',  ( -85.90077524418997257, 26.30132018890136081, 39.91278707234438627 ) ) ;
#4022 = CARTESIAN_POINT ( 'NONE',  ( -24.95029760921699591, 9.631514785009935409, -19.74184417840635675 ) ) ;
#4023 = PLANE ( 'NONE',  #21900 ) ;
#4024 = PRODUCT ( 'SIEVE', 'SIEVE', '', ( #61095 ) ) ;
#4025 = ORIENTED_EDGE ( 'NONE', *, *, #11025, .T. ) ;
#4026 = SURFACE_SIDE_STYLE ('',( #64140 ) ) ;
#4027 = CARTESIAN_POINT ( 'NONE',  ( 10.13846145460683168, 6.385368868491635652, 69.31597689299731258 ) ) ;
#4028 = DIRECTION ( 'NONE',  ( -0.000000000000000000, 1.000000000000000000, -0.000000000000000000 ) ) ;
#4029 = CARTESIAN_POINT ( 'NONE',  ( 200.0000000000000000, 3.000000000000030198, -3.000000000000030198 ) ) ;
#4030 = CARTESIAN_POINT ( 'NONE',  ( 0.000000000000000000, 0.000000000000000000, 0.000000000000000000 ) ) ;
#4031 = AXIS2_PLACEMENT_3D ( 'NONE', #27744, #49185, #1025 ) ;
#4033 = ORIENTED_EDGE ( 'NONE', *, *, #59864, .T. ) ;
#4032 = DIRECTION ( 'NONE',  ( -0.000000000000000000, 1.000000000000000000, 0.000000000000000000 ) ) ;
#4034 = CARTESIAN_POINT ( 'NONE',  ( 70.41705859591010608, 15.55317472777718280, 36.07559689591754903 ) ) ;
#4035 = VERTEX_POINT ( 'NONE', #68691 ) ;
#4036 = EDGE_CURVE ( 'NONE', #50267, #15307, #38531, .T. ) ;
#4037 = ORIENTED_EDGE ( 'NONE', *, *, #63361, .T. ) ;
#4038 = B_SPLINE_CURVE_WITH_KNOTS ( 'NONE', 3,
 ( #60997, #18435, #34966, #13845, #45157, #66304, #56409, #29006, #44470, #30032, #2606, #51143, #34634, #40240, #2959, #62029, #13166, #17749, #35307, #24065, #13510, #8231, #40575, #12462, #50448, #12822, #66993, #24418, #2268, #39890, #34276, #56765, #23715, #56071, #8585, #33926, #18781, #7888, #45509, #29334, #1556, #50785, #23018, #1926 ),
 .UNSPECIFIED., .F., .F.,
 ( 4, 2, 2, 2, 2, 2, 2, 2, 2, 2, 2, 2, 1, 2, 2, 2, 2, 2, 2, 1, 2, 2, 4 ),
 ( 0.02381751147647563280, 0.02531129726520771686, 0.02605819015957376236, 0.02680508305393981133, 0.02829886884267190580, 0.02979265463140400028, 0.03053954752577002496, 0.03128644042013604964, 0.03278022620886809901, 0.03427401199760014838, 0.03576779778633219775, 0.03651469068069820856, 0.03726158357506421243, 0.03800847646943021629, 0.03875536936379622016, 0.04024915515252823484, 0.04174294094126024257, 0.04323672672999225031, 0.04398361962435824724, 0.04473051251872425804, 0.04547740541309026191, 0.04622429830745626578, 0.04771808409618829433 ),
 .UNSPECIFIED. ) ;
#4039 = SURFACE_STYLE_FILL_AREA ( #30775 ) ;
#4040 = DIRECTION ( 'NONE',  ( -0.000000000000000000, -0.000000000000000000, -1.000000000000000000 ) ) ;
#4041 = LINE ( 'NONE', #62439, #56806 ) ;
#4042 = PRODUCT_DEFINITION_FORMATION_WITH_SPECIFIED_SOURCE ( 'ANY', '', #51893, .NOT_KNOWN. ) ;
#4044 = CARTESIAN_POINT ( 'NONE',  ( -102.2801239173131194, -170.0000000000000000, 38.01907450641511588 ) ) ;
#4043 = VECTOR ( 'NONE', #45035, 1000.000000000000000 ) ;
#4045 = EDGE_CURVE ( 'NONE', #19247, #46266, #9872, .T. ) ;
#4046 = CARTESIAN_POINT ( 'NONE',  ( -118.3960663196801306, 41.75130200162922023, 64.39655094048056583 ) ) ;
#4047 = LINE ( 'NONE', #20909, #68127 ) ;
#4048 = CARTESIAN_POINT ( 'NONE',  ( 15.55634918610396511, -46.66904755831214402, 85.00100000000000477 ) ) ;
#4049 = VECTOR ( 'NONE', #11638, 1000.000000000000000 ) ;
#4050 = ADVANCED_FACE ( 'NONE', ( #31754 ), #69386, .T. ) ;
#4051 = DIRECTION ( 'NONE',  ( 0.000000000000000000, 0.000000000000000000, 1.000000000000000000 ) ) ;
#4052 = EDGE_LOOP ( 'NONE', ( #25158, #36833, #15279, #17366 ) ) ;
#4053 =( REPRESENTATION_RELATIONSHIP ('NONE','NONE', #40274, #50551 ) REPRESENTATION_RELATIONSHIP_WITH_TRANSFORMATION ( #31588 )SHAPE_REPRESENTATION_RELATIONSHIP( ) );
#4054 = ORIENTED_EDGE ( 'NONE', *, *, #64477, .F. ) ;
#4055 = DIRECTION ( 'NONE',  ( -1.000000000000000000, 1.540743955509788682E-33, 1.110223024625156540E-16 ) ) ;
#4056 = ADVANCED_FACE ( 'NONE', ( #5018 ), #84, .F. ) ;
#4057 = CARTESIAN_POINT ( 'NONE',  ( -86.06525741550314024, 26.37048289224654951, -41.36178332953014092 ) ) ;
#4058 = CARTESIAN_POINT ( 'NONE',  ( 157.9160637431159273, 57.99786926216935967, 71.25401806271709404 ) ) ;
#4059 = CARTESIAN_POINT ( 'NONE',  ( -149.5074843970971017, 65.50121172469319220, 3.876270649435370252 ) ) ;
#4060 = CARTESIAN_POINT ( 'NONE',  ( 181.0840389613909736, 78.60582251573003987, -36.22505766587961062 ) ) ;
#4061 = CARTESIAN_POINT ( 'NONE',  ( -166.2425995121691642, 79.78465616981384301, 94.99999999999866418 ) ) ;
#4062 = CARTESIAN_POINT ( 'NONE',  ( 161.7209903610255139, 61.03262545641849357, -64.27214371681093041 ) ) ;
#4063 = ORIENTED_EDGE ( 'NONE', *, *, #23203, .F. ) ;
#4064 = ORIENTED_EDGE ( 'NONE', *, *, #62499, .T. ) ;
#4065 = EDGE_LOOP ( 'NONE', ( #60343, #16016, #47481, #9262 ) ) ;
#4066 = DIRECTION ( 'NONE',  ( -0.000000000000000000, -0.000000000000000000, -1.000000000000000000 ) ) ;
#4067 = DIRECTION ( 'NONE',  ( -0.000000000000000000, -0.000000000000000000, 1.000000000000000000 ) ) ;
#4068 = ADVANCED_FACE ( 'NONE', ( #32106 ), #32794, .F. ) ;
#4069 = CARTESIAN_POINT ( 'NONE',  ( 70.11766033381771024, 14.43277633974326513, -45.68147077570210257 ) ) ;
#4070 = CYLINDRICAL_SURFACE ( 'NONE', #24334, 5.000000000000004441 ) ;
#4071 = ADVANCED_FACE ( 'NONE', ( #20505 ), #5928, .T. ) ;
#4072 = B_SPLINE_CURVE_WITH_KNOTS ( 'NONE', 3,
 ( #48225, #37009, #48565, #51 ),
 .UNSPECIFIED., .F., .F.,
 ( 4, 4 ),
 ( 9.900409499089635938E-07, 0.05658314289920116785 ),
 .UNSPECIFIED. ) ;
#4073 = CARTESIAN_POINT ( 'NONE',  ( -38.17232309348610642, 11.81874355808868771, -66.32131283007623779 ) ) ;
#4074 = CARTESIAN_POINT ( 'NONE',  ( -24.75616454008739709, -3.483147608717210630, 0.000000000000000000 ) ) ;
#4075 = CARTESIAN_POINT ( 'NONE',  ( 31.90217595456442012, 7.552213897210512172, 64.75245333076260579 ) ) ;
#4076 = CARTESIAN_POINT ( 'NONE',  ( 11.21387192505586761, 6.397095920409659797, -22.13791506854233049 ) ) ;
#4077 = VERTEX_POINT ( 'NONE', #69027 ) ;
#4078 = PLANE ( 'NONE',  #3688 ) ;
#4079 = CARTESIAN_POINT ( 'NONE',  ( 188.4904153916304210, 86.42965364612516055, 62.43372719721995168 ) ) ;
#4080 = CARTESIAN_POINT ( 'NONE',  ( -119.2682179969168601, 42.28333404791699479, 14.82846940081925347 ) ) ;
#4081 = CARTESIAN_POINT ( 'NONE',  ( 70.02892116572941461, 14.40944430928135489, -67.39582635729337312 ) ) ;
#4082 = CARTESIAN_POINT ( 'NONE',  ( 126.3737790127712515, 37.08609730334947585, -16.10780632754811847 ) ) ;
#4083 = CARTESIAN_POINT ( 'NONE',  ( -5.066666666666671759, 0.000000000000000000, -11.86666666666666536 ) ) ;
#4084 = CARTESIAN_POINT ( 'NONE',  ( 8.537735592981558597, 7.383000420390738228, 12.60408504631577742 ) ) ;
#4085 = ORIENTED_EDGE ( 'NONE', *, *, #15028, .T. ) ;
#4086 = VECTOR ( 'NONE', #31580, 1000.000000000000000 ) ;
#4087 = CARTESIAN_POINT ( 'NONE',  ( 187.5325688887158151, 85.37769363979911930, 13.83221296240295572 ) ) ;
#4088 = SHAPE_DEFINITION_REPRESENTATION ( #20886, #7414 ) ;
#4089 = CARTESIAN_POINT ( 'NONE',  ( 23.63370729589335184, -52.11334794818031924, 133.5802547743875550 ) ) ;
#4090 = CARTESIAN_POINT ( 'NONE',  ( -12.77952633087662093, -21.62918162951127243, 3.061616997868437868E-16 ) ) ;
#4091 = LINE ( 'NONE', #42405, #16612 ) ;
#4092 = CONTEXT_DEPENDENT_SHAPE_REPRESENTATION ( #32796, #23152 ) ;
#4093 = CARTESIAN_POINT ( 'NONE',  ( 185.5457097283155008, 84.70846743303874860, -37.67841935146066135 ) ) ;
#4094 = ORIENTED_EDGE ( 'NONE', *, *, #39694, .T. ) ;
#4095 = CIRCLE ( 'NONE', #6335, 65.36598343705435354 ) ;
#4096 = VECTOR ( 'NONE', #43353, 1000.000000000000000 ) ;
#4097 = PRODUCT_DEFINITION_FORMATION_WITH_SPECIFIED_SOURCE ( 'ANY', '', #62996, .NOT_KNOWN. ) ;
#4098 = ORIENTED_EDGE ( 'NONE', *, *, #66400, .T. ) ;
#4099 = CARTESIAN_POINT ( 'NONE',  ( -147.3614567344829140, 62.37986555269943523, -8.268114818102619168 ) ) ;
#4100 = DIRECTION ( 'NONE',  ( 0.000000000000000000, 1.000000000000000000, 0.000000000000000000 ) ) ;
#4101 = EDGE_LOOP ( 'NONE', ( #34045, #40743 ) ) ;
#4102 = CARTESIAN_POINT ( 'NONE',  ( 112.5721302457195634, 29.97407549554798933, 71.10054341115458953 ) ) ;
#4103 = EDGE_LOOP ( 'NONE', ( #11564, #8330, #38539, #59538 ) ) ;
#4104 = CARTESIAN_POINT ( 'NONE',  ( 131.3924949472283004, 41.12442122814100287, -77.45525042326674736 ) ) ;
#4105 = DIRECTION ( 'NONE',  ( -1.000000000000000000, 0.000000000000000000, 0.000000000000000000 ) ) ;
#4106 = DIRECTION ( 'NONE',  ( 1.000000000000000000, -0.000000000000000000, -0.000000000000000000 ) ) ;
#4107 = DIRECTION ( 'NONE',  ( -0.000000000000000000, -0.000000000000000000, -1.000000000000000000 ) ) ;
#4108 = DIRECTION ( 'NONE',  ( -0.000000000000000000, -0.000000000000000000, 1.000000000000000000 ) ) ;
#4110 = ORIENTED_EDGE ( 'NONE', *, *, #50020, .T. ) ;
#4109 = DIRECTION ( 'NONE',  ( -1.000000000000000000, 0.000000000000000000, 0.000000000000000000 ) ) ;
#4111 = DIRECTION ( 'NONE',  ( -0.000000000000000000, -0.000000000000000000, -1.000000000000000000 ) ) ;
#4112 = ORIENTED_EDGE ( 'NONE', *, *, #10677, .F. ) ;
#4113 = ORIENTED_EDGE ( 'NONE', *, *, #40667, .T. ) ;
#4114 = CARTESIAN_POINT ( 'NONE',  ( -122.8118341587044711, 44.49743491855734590, -22.42191975060944031 ) ) ;
#4115 = CARTESIAN_POINT ( 'NONE',  ( -2.645453300864630819E-14, -10.55634918610403439, 0.000000000000000000 ) ) ;
#4116 = CARTESIAN_POINT ( 'NONE',  ( -179.2177980985565000, 94.18084789436638005, -19.74344003203561471 ) ) ;
#4118 = EDGE_LOOP ( 'NONE', ( #27509, #50059, #51468, #64476, #63468, #11482, #54903 ) ) ;
#4117 = CARTESIAN_POINT ( 'NONE',  ( -132.4896623150433754, 52.22616402022728010, 68.54373966055456435 ) ) ;
#4119 = LINE ( 'NONE', #41409, #61177 ) ;
#4120 = CARTESIAN_POINT ( 'NONE',  ( 86.62931800182293784, -170.0000000000000000, 64.05663816294301682 ) ) ;
#4121 = EDGE_LOOP ( 'NONE', ( #15370, #59184, #63446, #6452 ) ) ;
#4122 = CARTESIAN_POINT ( 'NONE',  ( -57.43251939610647128, 15.33203492375494648, -23.00071778682259094 ) ) ;
#4123 = EDGE_CURVE ( 'NONE', #25726, #42920, #11325, .T. ) ;
#4124 = VECTOR ( 'NONE', #23446, 1000.000000000000000 ) ;
#4125 = CARTESIAN_POINT ( 'NONE',  ( -130.5904357464317798, 50.88938808445630713, -63.39065355895628784 ) ) ;
#4126 = CARTESIAN_POINT ( 'NONE',  ( 58.79612034558317646, 11.73326361111144145, -90.69579281747449784 ) ) ;
#4127 = CARTESIAN_POINT ( 'NONE',  ( -23.85457283326439182, 7.880174245944055578, 0.000000000000000000 ) ) ;
#4128 = CARTESIAN_POINT ( 'NONE',  ( -422.6627218934914367, 0.000000000000000000, -146.4497041420118251 ) ) ;
#4129 = ORIENTED_EDGE ( 'NONE', *, *, #4673, .T. ) ;
#4130 = ORIENTED_EDGE ( 'NONE', *, *, #28912, .F. ) ;
#4131 = VECTOR ( 'NONE', #2015, 1000.000000000000000 ) ;
#4132 = ADVANCED_FACE ( 'NONE', ( #15922 ), #15236, .T. ) ;
#4133 = CARTESIAN_POINT ( 'NONE',  ( 181.0840389613909736, -170.0000000000000000, 63.65314469597510794 ) ) ;
#4134 = CARTESIAN_POINT ( 'NONE',  ( -165.7138623879809529, 79.24467249981145756, -40.99702868041568138 ) ) ;
#4135 = DIRECTION ( 'NONE',  ( 0.000000000000000000, 1.000000000000000000, -0.000000000000000000 ) ) ;
#4136 = VECTOR ( 'NONE', #3654, 1000.000000000000000 ) ;
#4137 = CARTESIAN_POINT ( 'NONE',  ( 61.28323125814129213, -21.66484633135379667, 40.00000000000003553 ) ) ;
#4138 = CARTESIAN_POINT ( 'NONE',  ( -72.35078170365750339, 21.08176362823952488, 33.86556106749917205 ) ) ;
#4139 = FACE_OUTER_BOUND ( 'NONE', #54207, .T. ) ;
#4140 = PRODUCT_DEFINITION_FORMATION_WITH_SPECIFIED_SOURCE ( 'ANY', '', #11948, .NOT_KNOWN. ) ;
#4141 = CARTESIAN_POINT ( 'NONE',  ( 63.98689050258322908, 13.93365232918667473, -35.76819633441670732 ) ) ;
#4142 = CARTESIAN_POINT ( 'NONE',  ( -173.1211646369891355, 88.63826465341152527, -34.71195716474998960 ) ) ;
#4143 = CARTESIAN_POINT ( 'NONE',  ( 211.7419975634644516, 116.5322580952101248, 60.89782388646611366 ) ) ;
#4144 = ORIENTED_EDGE ( 'NONE', *, *, #53038, .F. ) ;
#4145 = CARTESIAN_POINT ( 'NONE',  ( -108.0980548770427845, 35.83569586822709141, -10.91122087686984976 ) ) ;
#4147 = ORIENTED_EDGE ( 'NONE', *, *, #28779, .T. ) ;
#4146 = B_SPLINE_CURVE_WITH_KNOTS ( 'NONE', 3,
 ( #52912, #4735, #22303, #45144, #60979, #54290, #33573, #6817, #66623, #28267, #59921, #17364, #18419, #59569, #34261, #17735, #11739, #28988, #23703, #60289, #33218, #22650, #44089, #43740, #65218, #32855, #55706, #38480, #54652, #23367, #7535, #6477, #50434, #12805, #2255, #60634, #12450, #65573, #11385, #28629, #6112, #38842, #33909, #23003, #17009, #49013, #7174, #39529 ),
 .UNSPECIFIED., .F., .F.,
 ( 4, 2, 2, 2, 2, 2, 2, 2, 2, 2, 2, 2, 2, 2, 2, 2, 2, 2, 2, 2, 2, 2, 2, 4 ),
 ( 7.757919228897728493E-18, 0.001591515129442220991, 0.003183030258884434176, 0.003978787823605536324, 0.004774545388326638037, 0.006366060517768890037, 0.007957575647211142036, 0.009549090776653395771, 0.01034484834137452437, 0.01114060590609565297, 0.01193636347081678331, 0.01273212103553791712, 0.01432363616498018473, 0.01591515129442245061, 0.01671090885914358615, 0.01750666642386471822, 0.01830242398858585723, 0.01909818155330698930, 0.02068969668274931242, 0.02148545424747046878, 0.02228121181219162514, 0.02387272694163386499, 0.02466848450635494502, 0.02546424207107601811 ),
 .UNSPECIFIED. ) ;
#4149 = CIRCLE ( 'NONE', #55822, 1.500000000000001332 ) ;
#4148 = CARTESIAN_POINT ( 'NONE',  ( -179.2175250771078936, 94.18012766206246056, -91.50370824807137637 ) ) ;
#4150 = CARTESIAN_POINT ( 'NONE',  ( 82.73618382051374454, 19.18661415186669572, 70.47170656936988564 ) ) ;
#4151 = CARTESIAN_POINT ( 'NONE',  ( 10.55634918610400419, -15.55634918610406103, 0.000000000000000000 ) ) ;
#4152 = ADVANCED_FACE ( 'NONE', ( #15588, #58822 ), #37037, .T. ) ;
#4153 = CARTESIAN_POINT ( 'NONE',  ( 70.60157554497493493, -25.16207943727098950, 41.38025477438755928 ) ) ;
#4154 = CARTESIAN_POINT ( 'NONE',  ( 33.46033188299906413, 8.722678254080099336, 5.985838565680452916 ) ) ;
#4155 = CARTESIAN_POINT ( 'NONE',  ( 0.000000000000000000, 65.13282190615278466, -5.000000000000000000 ) ) ;
#4156 = CARTESIAN_POINT ( 'NONE',  ( -449.7337897053568554, 364.9999999999998295, -143.5207719538772722 ) ) ;
#4157 = FACE_OUTER_BOUND ( 'NONE', #4605, .T. ) ;
#4158 = DIRECTION ( 'NONE',  ( -1.000000000000000000, 0.000000000000000000, 0.000000000000000000 ) ) ;
#4159 = ORIENTED_EDGE ( 'NONE', *, *, #52250, .F. ) ;
#4160 = CARTESIAN_POINT ( 'NONE',  ( -23.14886993799567705, -9.760512885997105315, 0.000000000000000000 ) ) ;
#4161 = ORIENTED_EDGE ( 'NONE', *, *, #14337, .F. ) ;
#4162 = CARTESIAN_POINT ( 'NONE',  ( 74.39890044415633952, 7.951074708187157114, 170.0000000000000000 ) ) ;
#4163 = CARTESIAN_POINT ( 'NONE',  ( -190.6985136298601731, 109.1272424661242582, -95.00000000000133582 ) ) ;
#4164 = DIRECTION ( 'NONE',  ( 0.000000000000000000, -0.000000000000000000, -1.000000000000000000 ) ) ;
#4165 = CARTESIAN_POINT ( 'NONE',  ( -58.91195363087619086, 15.75019387706849727, -89.97097185737439418 ) ) ;
#4166 = FACE_BOUND ( 'NONE', #26669, .T. ) ;
#4167 = CARTESIAN_POINT ( 'NONE',  ( 152.6804161981489472, 55.27286404993342472, -49.40040420956763256 ) ) ;
#4168 = ORIENTED_EDGE ( 'NONE', *, *, #18126, .T. ) ;
#4169 = CARTESIAN_POINT ( 'NONE',  ( 684.5501828525945029, 847.8234287996372132, 616.5068267248686880 ) ) ;
#4170 = CARTESIAN_POINT ( 'NONE',  ( -157.0069571479806996, 72.18154199622281908, 64.76481382543292398 ) ) ;
#4171 = CARTESIAN_POINT ( 'NONE',  ( -13.24252603915519444, -63.63674649211960599, 170.0000000000000000 ) ) ;
#4172 = CARTESIAN_POINT ( 'NONE',  ( 5.799999999999999822, -6.928203230275509661, -3.999999999999998224 ) ) ;
#4173 = CARTESIAN_POINT ( 'NONE',  ( -7.825402957745081878, 7.899365992529270741, 30.11558103944718923 ) ) ;
#4174 = ORIENTED_EDGE ( 'NONE', *, *, #26295, .F. ) ;
#4175 = CARTESIAN_POINT ( 'NONE',  ( -175.1968289912784940, 90.99944698359489337, -61.83708215555294885 ) ) ;
#4176 = CARTESIAN_POINT ( 'NONE',  ( 93.85846834761625246, 22.01563781856520663, 62.04340769976120384 ) ) ;
#4177 = VECTOR ( 'NONE', #31591, 1000.000000000000000 ) ;
#4178 = PRODUCT_DEFINITION_SHAPE ( 'NONE', 'NONE',  #69619 ) ;
#4179 = CARTESIAN_POINT ( 'NONE',  ( 202.7540649946182896, 105.3989460363904698, -24.23651903053695378 ) ) ;
#4180 = CARTESIAN_POINT ( 'NONE',  ( 0.000000000000000000, 0.000000000000000000, 43.58025477438756212 ) ) ;
#4181 = DIRECTION ( 'NONE',  ( -1.000000000000000000, 0.000000000000000000, -0.000000000000000000 ) ) ;
#4182 = ORIENTED_EDGE ( 'NONE', *, *, #46122, .F. ) ;
#4183 = CARTESIAN_POINT ( 'NONE',  ( 201.5903370237273862, 102.1785392640257584, 29.86822796726585594 ) ) ;
#4184 = FACE_OUTER_BOUND ( 'NONE', #48901, .T. ) ;
#4185 = CIRCLE ( 'NONE', #761, 89.99999999999997158 ) ;
#4186 = CARTESIAN_POINT ( 'NONE',  ( 182.7745872728868051, 81.77554423487158886, 44.16596963624431993 ) ) ;
#4187 = CARTESIAN_POINT ( 'NONE',  ( 141.3036441389950824, 47.31002705502925920, 9.125830029735173099 ) ) ;
#4188 = CARTESIAN_POINT ( 'NONE',  ( 0.000000000000000000, 0.000000000000000000, 0.000000000000000000 ) ) ;
#4189 = CIRCLE ( 'NONE', #54729, 9.999999999999994671 ) ;
#4190 = EDGE_LOOP ( 'NONE', ( #41859, #2257, #52891, #50930 ) ) ;
#4191 = EDGE_CURVE ( 'NONE', #55532, #38915, #26137, .T. ) ;
#4192 = AXIS2_PLACEMENT_3D ( 'NONE', #59060, #5260, #59405 ) ;
#4193 = CARTESIAN_POINT ( 'NONE',  ( 133.8566784816069344, -170.0000000000000000, 10.16579024853168889 ) ) ;
#4194 = ORIENTED_EDGE ( 'NONE', *, *, #40811, .F. ) ;
#4195 = EDGE_CURVE ( 'NONE', #14640, #7559, #37718, .T. ) ;
#4196 = VECTOR ( 'NONE', #55684, 1000.000000000000000 ) ;
#4197 = CARTESIAN_POINT ( 'NONE',  ( -109.7078892845591582, 36.71702188566216307, -41.44327227783652745 ) ) ;
#4198 = CARTESIAN_POINT ( 'NONE',  ( 126.5497923654802008, 37.18409895203431148, 92.42836552067784339 ) ) ;
#4199 = CARTESIAN_POINT ( 'NONE',  ( -56.96214175905167565, 15.20165595797839586, 45.07424718572830358 ) ) ;
#4201 = ORIENTED_EDGE ( 'NONE', *, *, #38594, .T. ) ;
#4200 = DIRECTION ( 'NONE',  ( 0.000000000000000000, 0.000000000000000000, 1.000000000000000000 ) ) ;
#4202 = CARTESIAN_POINT ( 'NONE',  ( -179.2177980985565284, 94.18084789436638005, 33.94566114889175878 ) ) ;
#4203 = CARTESIAN_POINT ( 'NONE',  ( 437.3372781065085633, 394.9999999999999432, 91.05029585798857283 ) ) ;
#4204 = CARTESIAN_POINT ( 'NONE',  ( 110.7167338301704120, 30.21148223254619225, -35.92243756565369495 ) ) ;
#4205 = ORIENTED_EDGE ( 'NONE', *, *, #66591, .T. ) ;
#4206 = FACE_OUTER_BOUND ( 'NONE', #56753, .T. ) ;
#4207 = ADVANCED_FACE ( 'NONE', ( #5370, #26826, #10984, #27860, #50009, #49651, #18013, #44746, #16949, #38776, #49303, #66225, #28564, #18352, #1844, #59858, #55996, #44382, #6755, #65506, #1136, #54934, #1479, #65871, #22940, #39814, #65155, #22587, #29261, #60220, #17666, #33507, #34201, #55635, #23641, #23301, #39130, #38413, #39462, #7468, #12038, #787, #2189, #55285, #34556, #60569, #11678, #44027, #22240, #28921, #33149, #12385, #33844, #66563, #17304, #28205, #7105, #61268, #60913, #45080, #12736, #50373, #13091, #7810, #43679, #54585, #6411, #24685, #61948, #3912, #14467, #19737, #23981, #2872, #46119, #41199, #24341, #35924, #25381, #34892, #67590, #8500, #51062, #14800, #13767, #8852, #45784, #50710, #51751, #30644, #62304, #40161, #9534, #3226, #51417, #67259, #40847, #52092, #19389, #35225, #14116, #35578, #9187 ), #57375, .T. ) ;
#4208 = EDGE_CURVE ( 'NONE', #27210, #48270, #46816, .T. ) ;
#4209 = FACE_OUTER_BOUND ( 'NONE', #6614, .T. ) ;
#4210 = ORIENTED_EDGE ( 'NONE', *, *, #53344, .T. ) ;
#4211 = CARTESIAN_POINT ( 'NONE',  ( 140.0614732283738704, 45.29930344725075742, 59.63437826547444587 ) ) ;
#4212 = CARTESIAN_POINT ( 'NONE',  ( -169.8842709557924877, 83.59602878049474839, 31.54149301594271648 ) ) ;
#4213 = DIRECTION ( 'NONE',  ( 1.000000000000000000, -0.000000000000000000, 0.000000000000000000 ) ) ;
#4214 = CARTESIAN_POINT ( 'NONE',  ( 412.3372781065085633, 219.4906275429376308, -144.4497041420117682 ) ) ;
#4215 = VERTEX_POINT ( 'NONE', #29594 ) ;
#4216 = CARTESIAN_POINT ( 'NONE',  ( 157.4703587214989398, -170.0000000000000000, 17.56491688178971700 ) ) ;
#4217 = VERTEX_POINT ( 'NONE', #19045 ) ;
#4218 = EDGE_CURVE ( 'NONE', #2906, #61020, #61068, .T. ) ;
#4219 = CARTESIAN_POINT ( 'NONE',  ( 150.2193536046551685, 53.46717047532148825, -18.71536020992064309 ) ) ;
#4220 = CARTESIAN_POINT ( 'NONE',  ( 208.0306608271317259, 112.7988899307264887, -23.70348385667363189 ) ) ;
#4221 = CARTESIAN_POINT ( 'NONE',  ( 107.0555969502564722, 28.53646637607231895, 30.30581710560821662 ) ) ;
#4222 = FACE_OUTER_BOUND ( 'NONE', #2289, .T. ) ;
#4223 = CIRCLE ( 'NONE', #47977, 4.999999999999997335 ) ;
#4224 = CARTESIAN_POINT ( 'NONE',  ( 5.799999999999999822, 4.618802153517001408, -8.000000000000000000 ) ) ;
#4225 = CARTESIAN_POINT ( 'NONE',  ( 183.9887307715836471, 83.05100282186906213, 16.88219682803630306 ) ) ;
#4226 = CARTESIAN_POINT ( 'NONE',  ( 37.34307124463426675, -44.82188588777072624, 27.58472369417913583 ) ) ;
#4227 = CARTESIAN_POINT ( 'NONE',  ( 230.9999999999999432, -2.000000000000000000, 0.000000000000000000 ) ) ;
#4228 = ORIENTED_EDGE ( 'NONE', *, *, #11749, .T. ) ;
#4229 = VECTOR ( 'NONE', #1293, 1000.000000000000000 ) ;
#4230 = CARTESIAN_POINT ( 'NONE',  ( 110.2429982417149574, -170.0000000000000000, -70.26698815611737814 ) ) ;
#4231 = ORIENTED_EDGE ( 'NONE', *, *, #26052, .T. ) ;
#4232 = CARTESIAN_POINT ( 'NONE',  ( -75.65611349188969825, 22.26947559308020530, 57.88921423585124160 ) ) ;
#4233 = EDGE_CURVE ( 'NONE', #6944, #45198, #13429, .T. ) ;
#4234 = CARTESIAN_POINT ( 'NONE',  ( 62.04326772936977363, 12.44884401098615534, -77.51769772343732257 ) ) ;
#4235 = CIRCLE ( 'NONE', #8711, 35.00000000000000000 ) ;
#4236 = CARTESIAN_POINT ( 'NONE',  ( 0.000000000000000000, 0.000000000000000000, 40.00000000000003553 ) ) ;
#4237 = DIRECTION ( 'NONE',  ( 0.000000000000000000, -0.000000000000000000, -1.000000000000000000 ) ) ;
#4238 = CARTESIAN_POINT ( 'NONE',  ( -9.133021071383323530, 6.979519547623484144, 83.91237909771824377 ) ) ;
#4239 = EDGE_CURVE ( 'NONE', #2530, #28747, #69404, .T. ) ;
#4240 = EDGE_CURVE ( 'NONE', #40678, #25506, #42573, .T. ) ;
#4241 = EDGE_CURVE ( 'NONE', #32499, #62713, #15839, .T. ) ;
#4242 = CIRCLE ( 'NONE', #3146, 25.00000000000145306 ) ;
#4243 = DIRECTION ( 'NONE',  ( -1.000000000000000000, 0.000000000000000000, 0.000000000000000000 ) ) ;
#4244 = VERTEX_POINT ( 'NONE', #15155 ) ;
#4245 = CARTESIAN_POINT ( 'NONE',  ( 16.83496191631032346, 55.85777011067597897, 27.58472369377037481 ) ) ;
#4246 = CARTESIAN_POINT ( 'NONE',  ( 204.0464538518397148, 105.4549945320416953, -90.03620575426465678 ) ) ;
#4247 = ORIENTED_EDGE ( 'NONE', *, *, #45253, .T. ) ;
#4248 = B_SPLINE_CURVE_WITH_KNOTS ( 'NONE', 3,
 ( #45934, #62104, #9336, #13579, #68096, #51219, #67399, #4407, #41007, #62461, #3708, #3034, #68758, #30114, #25186, #56483, #20234, #35385 ),
 .UNSPECIFIED., .F., .F.,
 ( 4, 2, 2, 2, 2, 2, 2, 2, 4 ),
 ( 0.01201226291592704873, 0.01492726547989151054, 0.01638476676187372236, 0.01784226804385593418, 0.01929976932583814253, 0.02075727060782035782, 0.02148602124881145159, 0.02221477188980254883, 0.02367227317178470167 ),
 .UNSPECIFIED. ) ;
#4249 = ORIENTED_EDGE ( 'NONE', *, *, #48713, .T. ) ;
#4250 = CARTESIAN_POINT ( 'NONE',  ( -150.3791492925491298, 64.92185203933372861, 30.75880558023102296 ) ) ;
#4251 = CARTESIAN_POINT ( 'NONE',  ( 60.40277045393652600, 12.08176563382370183, -36.18631425159986037 ) ) ;
#4252 = CYLINDRICAL_SURFACE ( 'NONE', #48497, 7.500000000000013323 ) ;
#4253 = VECTOR ( 'NONE', #53682, 1000.000000000000000 ) ;
#4254 = DIRECTION ( 'NONE',  ( 1.387778780781445922E-16, -1.000000000000000000, -1.232595164407830946E-32 ) ) ;
#4255 = ORIENTED_EDGE ( 'NONE', *, *, #21903, .T. ) ;
#4256 = CARTESIAN_POINT ( 'NONE',  ( -132.2161740628506550, 52.03204870034952734, 34.07724243096232186 ) ) ;
#4257 = VERTEX_POINT ( 'NONE', #31338 ) ;
#4258 = CARTESIAN_POINT ( 'NONE',  ( 22.62427395637551086, 7.823784829753562597, -46.11402725324526131 ) ) ;
#4259 = CARTESIAN_POINT ( 'NONE',  ( -145.9181947914995874, 62.49417193455359154, 44.81018965788452846 ) ) ;
#4260 = B_SPLINE_CURVE_WITH_KNOTS ( 'NONE', 3,
 ( #27856, #37359, #43675, #5014, #16945, #33145, #53185, #11674, #54581, #79, #47916, #59162, #6406, #32101, #49299, #1132, #58818, #44023, #22583, #58471, #69380, #10283, #54930, #23977, #2870, #44378, #33502, #2186, #7101, #17300, #44743, #13088, #1475, #45429, #66909, #2524, #8146, #39811, #28918, #18704, #7465, #34890, #29258, #50006, #49647, #56330, #60910 ),
 .UNSPECIFIED., .F., .F.,
 ( 4, 2, 2, 2, 2, 2, 2, 2, 2, 2, 2, 2, 1, 2, 2, 2, 2, 2, 2, 2, 2, 2, 2, 4 ),
 ( 0.000000000000000000, 0.001520400357568930287, 0.002280600536353414188, 0.003040800715137898305, 0.004561201072706868274, 0.005321401251491338080, 0.006081601430275807886, 0.007602001787844721477, 0.008362201966629193017, 0.009122402145413663690, 0.01064280250298261024, 0.01140300268176708612, 0.01216320286055155853, 0.01292340303933604308, 0.01368360321812052589, 0.01520400357568950193, 0.01596420375447399342, 0.01672440393325848665, 0.01824480429082747657, 0.01976520464839646649, 0.02052540482718095971, 0.02128560500596544947, 0.02280600536353444285, 0.02432640572110343624 ),
 .UNSPECIFIED. ) ;
#4261 = DIRECTION ( 'NONE',  ( -0.9639628606958550172, 0.2660368455666687892, 0.000000000000000000 ) ) ;
#4262 = ORIENTED_EDGE ( 'NONE', *, *, #58288, .T. ) ;
#4263 = ORIENTED_EDGE ( 'NONE', *, *, #2659, .T. ) ;
#4264 = LINE ( 'NONE', #35927, #67110 ) ;
#4265 = CARTESIAN_POINT ( 'NONE',  ( -127.3773789194800372, 48.68981405637768489, 84.45179168653085355 ) ) ;
#4266 = CARTESIAN_POINT ( 'NONE',  ( -167.6413528428656150, 81.22881971256914824, -20.51375374840328547 ) ) ;
#4267 = CARTESIAN_POINT ( 'NONE',  ( 29.31537786019797664, 16.05900809008567975, 6.893343212288939093 ) ) ;
#4268 = CARTESIAN_POINT ( 'NONE',  ( 14.47678578469710864, 6.462159579077012772, 83.81204869879134378 ) ) ;
#4269 = CARTESIAN_POINT ( 'NONE',  ( 80.16939877002758408, 17.31693935407226448, -66.32369062857475228 ) ) ;
#4270 = AXIS2_PLACEMENT_3D ( 'NONE', #11426, #20963, #48021 ) ;
#4271 = EDGE_LOOP ( 'NONE', ( #40131, #56927, #23005, #48343 ) ) ;
#4272 = DIRECTION ( 'NONE',  ( 0.000000000000000000, 0.000000000000000000, -1.000000000000000000 ) ) ;
#4273 = CARTESIAN_POINT ( 'NONE',  ( 0.000000000000000000, 0.000000000000000000, -9.500000000000000000 ) ) ;
#4274 = EDGE_LOOP ( 'NONE', ( #32274, #55909, #20060, #69556 ) ) ;
#4275 = B_SPLINE_CURVE_WITH_KNOTS ( 'NONE', 3,
 ( #2929, #35972, #39863, #35636, #67310, #3276, #56739, #62359, #56045, #13482, #67994, #50761, #61320, #19096, #46519, #40550, #13146, #24041, #57087, #13818, #35283, #34943, #30351, #41257, #45134, #2582, #34609, #30008, #18760, #61663, #24736, #46171, #7863, #51804, #56383, #3612, #29310, #7526, #25082, #2242, #19440, #28976, #66963, #50423, #23691 ),
 .UNSPECIFIED., .F., .F.,
 ( 4, 2, 2, 1, 2, 2, 2, 2, 2, 2, 2, 2, 2, 2, 2, 2, 2, 2, 2, 2, 2, 2, 4 ),
 ( 0.02346057189573569693, 0.02492590417315493703, 0.02565857031186456055, 0.02639123645057418407, 0.02712390258928380760, 0.02785656872799342765, 0.02932190100541267816, 0.03005456714412230862, 0.03078723328283193561, 0.03225256556025118959, 0.03298523169896081658, 0.03371789783767044357, 0.03518323011508970449, 0.03664856239250896541, 0.03738122853121858546, 0.03811389466992821246, 0.03957922694734747338, 0.04104455922476672736, 0.04250989150218598134, 0.04324255764089560833, 0.04397522377960523532, 0.04544055605702450318, 0.04690588833444375716 ),
 .UNSPECIFIED. ) ;
#4277 = CARTESIAN_POINT ( 'NONE',  ( -85.35127931077727226, 24.98147633332999717, 7.663918504084784367 ) ) ;
#4276 = CIRCLE ( 'NONE', #68301, 25.00000000000296296 ) ;
#4278 = ORIENTED_EDGE ( 'NONE', *, *, #64901, .F. ) ;
#4279 = ADVANCED_FACE ( 'NONE', ( #36613 ), #64030, .F. ) ;
#4280 = CARTESIAN_POINT ( 'NONE',  ( -60.66101049381765620, 17.30588917955502382, -10.86812352032706741 ) ) ;
#4281 = ORIENTED_EDGE ( 'NONE', *, *, #27062, .T. ) ;
#4282 = VECTOR ( 'NONE', #5457, 1000.000000000000114 ) ;
#4283 = VERTEX_POINT ( 'NONE', #4938 ) ;
#4284 = CARTESIAN_POINT ( 'NONE',  ( -120.1650841064593891, 44.02024060322521848, 16.12247377298220030 ) ) ;
#4285 = CARTESIAN_POINT ( 'NONE',  ( -180.6009936245623635, 95.85948119829087943, 65.79761809826371177 ) ) ;
#4286 = PRESENTATION_LAYER_ASSIGNMENT (  '', '', ( #63832 ) ) ;
#4287 = CARTESIAN_POINT ( 'NONE',  ( 133.3990214534116774, 41.14886683286415092, 56.36538236340677344 ) ) ;
#4288 = ORIENTED_EDGE ( 'NONE', *, *, #58975, .F. ) ;
#4289 = EDGE_CURVE ( 'NONE', #66440, #49450, #4845, .T. ) ;
#4290 = EDGE_CURVE ( 'NONE', #36739, #40678, #341, .T. ) ;
#4291 = ADVANCED_FACE ( 'NONE', ( #53795 ), #52766, .F. ) ;
#4292 = CARTESIAN_POINT ( 'NONE',  ( -38.73622948742834637, 10.90353827065863968, 89.64304421912086696 ) ) ;
#4293 = VECTOR ( 'NONE', #68342, 1000.000000000000000 ) ;
#4294 = CARTESIAN_POINT ( 'NONE',  ( 173.8623159076320235, 72.97967239795021044, -72.61419801311336641 ) ) ;
#4295 = CARTESIAN_POINT ( 'NONE',  ( 74.99999999999998579, 9.184850993605147156E-15, 85.00000000000000000 ) ) ;
#4296 = DIRECTION ( 'NONE',  ( 0.000000000000000000, 0.000000000000000000, 1.000000000000000000 ) ) ;
#4297 = EDGE_CURVE ( 'NONE', #24824, #66237, #10464, .T. ) ;
#4298 = CARTESIAN_POINT ( 'NONE',  ( -28.81317668042940028, 9.175023678939295380, 30.68696444450949201 ) ) ;
#4299 = DIRECTION ( 'NONE',  ( -0.000000000000000000, -0.000000000000000000, -1.000000000000000000 ) ) ;
#4300 = ORIENTED_EDGE ( 'NONE', *, *, #23587, .F. ) ;
#4301 = DIRECTION ( 'NONE',  ( -0.000000000000000000, -0.000000000000000000, -1.000000000000000000 ) ) ;
#4302 = CARTESIAN_POINT ( 'NONE',  ( -85.95621526752228192, 26.32462117888283260, -71.24159791805112718 ) ) ;
#4303 = CARTESIAN_POINT ( 'NONE',  ( -1.901316136557078540, 6.577199328112531163, -91.92888192959523508 ) ) ;
#4304 = DIRECTION ( 'NONE',  ( -1.000000000000000000, 0.000000000000000000, 0.000000000000000000 ) ) ;
#4305 = CARTESIAN_POINT ( 'NONE',  ( -190.6985136298601731, 109.1272424661242582, -19.71767969763411799 ) ) ;
#4306 = CARTESIAN_POINT ( 'NONE',  ( 129.4987365823222092, 38.85470922756778833, 4.057026465556845984 ) ) ;
#4307 = CARTESIAN_POINT ( 'NONE',  ( 32.60744088438708133, 7.622802803743367051, -93.62651044593049221 ) ) ;
#4308 = CARTESIAN_POINT ( 'NONE',  ( -123.0348077379026535, 45.83489305753316501, -62.32075488609377345 ) ) ;
#4309 = CARTESIAN_POINT ( 'NONE',  ( -23.70047331481904251, -76.98764151615553430, 133.5802547743875550 ) ) ;
#4310 = CARTESIAN_POINT ( 'NONE',  ( 162.6190874793280727, 61.76782592053314147, 4.606215609171663949 ) ) ;
#4311 = CARTESIAN_POINT ( 'NONE',  ( -108.9136445001389859, 36.28030794288191174, 41.52760062685047870 ) ) ;
#4312 = ORIENTED_EDGE ( 'NONE', *, *, #17546, .T. ) ;
#4313 = CARTESIAN_POINT ( 'NONE',  ( -62.43646393413946782, 17.83771684480761976, 92.86132313336962341 ) ) ;
#4314 = EDGE_LOOP ( 'NONE', ( #18950, #35368, #65861, #24670 ) ) ;
#4315 = CARTESIAN_POINT ( 'NONE',  ( 16.78635691501517613, 0.000000000000000000, -4.435653166495499455 ) ) ;
#4316 = ORIENTED_EDGE ( 'NONE', *, *, #40336, .F. ) ;
#4317 = CARTESIAN_POINT ( 'NONE',  ( 22.62427395637552507, 7.823784829753567927, -72.95857784370898003 ) ) ;
#4318 = DIRECTION ( 'NONE',  ( -0.8160245890732938934, -0.5780171883497599028, 0.000000000000000000 ) ) ;
#4319 = CARTESIAN_POINT ( 'NONE',  ( 445.3372781065086201, 177.8591479523844612, 78.55029585798806124 ) ) ;
#4320 = FACE_OUTER_BOUND ( 'NONE', #58122, .T. ) ;
#4321 = ADVANCED_FACE ( 'NONE', ( #52442, #69302, #10552 ), #59082, .F. ) ;
#4322 = ADVANCED_FACE ( 'NONE', ( #27075 ), #64387, .T. ) ;
#4323 = DIRECTION ( 'NONE',  ( 1.000000000000000000, 0.000000000000000000, -0.000000000000000000 ) ) ;
#4324 = CARTESIAN_POINT ( 'NONE',  ( 31.90217595456442012, 7.552213897210508620, -42.62574903109214830 ) ) ;
#4325 = DIRECTION ( 'NONE',  ( 1.000000000000000000, 0.000000000000000000, 0.000000000000000000 ) ) ;
#4326 = LINE ( 'NONE', #10273, #68947 ) ;
#4327 = EDGE_CURVE ( 'NONE', #69014, #18870, #37986, .T. ) ;
#4328 = DIRECTION ( 'NONE',  ( -1.000000000000000000, 0.000000000000000000, 0.000000000000000000 ) ) ;
#4329 = ORIENTED_EDGE ( 'NONE', *, *, #68056, .F. ) ;
#4330 = ORIENTED_EDGE ( 'NONE', *, *, #55674, .F. ) ;
#4331 = VECTOR ( 'NONE', #69217, 1000.000000000000000 ) ;
#4332 = CARTESIAN_POINT ( 'NONE',  ( 173.9006248317893437, 73.01561032181524524, 92.66295374434788812 ) ) ;
#4333 = DIRECTION ( 'NONE',  ( 0.000000000000000000, -0.000000000000000000, 1.000000000000000000 ) ) ;
#4334 = PLANE ( 'NONE',  #50993 ) ;
#4335 = CIRCLE ( 'NONE', #22295, 243.4957430088094839 ) ;
#4336 = B_SPLINE_CURVE_WITH_KNOTS ( 'NONE', 3,
 ( #53270, #159, #31494, #52594, #14960, #64183, #68437, #42727, #53620, #20581, #30809, #68766, #63852, #63166, #52256, #20243, #37109, #58899, #48325, #10714, #25543, #21617, #52926, #4415, #36425, #15995, #43063, #25879, #58222, #64534, #41703, #32188, #4752, #37444, #26215, #26899, #36086, #47654, #42043, #47996, #46978, #57542, #9345 ),
 .UNSPECIFIED., .F., .F.,
 ( 4, 2, 2, 2, 2, 2, 2, 2, 1, 2, 2, 2, 2, 2, 2, 2, 2, 2, 2, 2, 2, 4 ),
 ( 3.469446951953614189E-18, 0.001466285743483479757, 0.002199428615225219093, 0.002932571486966958647, 0.004398857230450446860, 0.005865142973933935508, 0.007331428717417423288, 0.008064571589159165443, 0.008797714460900907599, 0.009530857332642649754, 0.01026400020438439191, 0.01173028594786787449, 0.01319657169135135533, 0.01466285743483483790, 0.01539600030657657832, 0.01612914317831831701, 0.01759542892180180479, 0.01906171466528529257, 0.01979485753702703299, 0.02052800040876876994, 0.02199428615225223690, 0.02346057189573570387 ),
 .UNSPECIFIED. ) ;
#4337 = UNCERTAINTY_MEASURE_WITH_UNIT (LENGTH_MEASURE( 1.000000000000000082E-05 ), #21203, 'distance_accuracy_value', 'NONE');
#4338 = CARTESIAN_POINT ( 'NONE',  ( 67.88711180968651604, 14.89360689134522353, -91.19259204464900392 ) ) ;
#4339 =( GEOMETRIC_REPRESENTATION_CONTEXT ( 3 ) GLOBAL_UNCERTAINTY_ASSIGNED_CONTEXT ( ( #9258 ) ) GLOBAL_UNIT_ASSIGNED_CONTEXT ( ( #38027, #66523, #46082 ) ) REPRESENTATION_CONTEXT ( 'NONE', 'WORKASPACE' ) );
#4340 = DIRECTION ( 'NONE',  ( -4.946224812893509176E-48, 1.000000000000000000, 3.697785493223491743E-32 ) ) ;
#4341 = DIRECTION ( 'NONE',  ( 0.5508969814520944253, 0.8345732537213078617, -0.000000000000000000 ) ) ;
#4342 = CARTESIAN_POINT ( 'NONE',  ( 210.9608386442062340, 117.1762372255315938, 13.99730087153263369 ) ) ;
#4343 = CARTESIAN_POINT ( 'NONE',  ( -78.66644367742109978, 23.39876645725288284, -76.96000122218160300 ) ) ;
#4344 = CARTESIAN_POINT ( 'NONE',  ( 93.08533330311587406, 21.72562315962718671, -20.32652723706974029 ) ) ;
#4345 = CARTESIAN_POINT ( 'NONE',  ( -31.43908319763709969, 10.61114334766715928, 72.06100499665289760 ) ) ;
#4346 = DIRECTION ( 'NONE',  ( -1.000000000000000000, 0.000000000000000000, 0.000000000000000000 ) ) ;
#4347 = DIRECTION ( 'NONE',  ( -1.000000000000000000, 0.000000000000000000, 0.000000000000000000 ) ) ;
#4348 = EDGE_LOOP ( 'NONE', ( #4033, #62830, #17819, #64317 ) ) ;
#4349 = CARTESIAN_POINT ( 'NONE',  ( -6.774725108395606377, -24.06456107444444825, 0.000000000000000000 ) ) ;
#4350 = DIRECTION ( 'NONE',  ( -0.3930250316539278255, 0.9195277725514487965, 0.000000000000000000 ) ) ;
#4351 = CARTESIAN_POINT ( 'NONE',  ( -53.38065169970958834, 15.27943072477081365, 71.97705297215981091 ) ) ;
#4352 = FACE_OUTER_BOUND ( 'NONE', #11897, .T. ) ;
#4353 = CARTESIAN_POINT ( 'NONE',  ( -51.99406906667275052, 13.88268392809766283, -35.86411590326191856 ) ) ;
#4354 = CARTESIAN_POINT ( 'NONE',  ( -4.164416015344989397, -64.86646004871190030, 170.0000000000000000 ) ) ;
#4355 = ORIENTED_EDGE ( 'NONE', *, *, #12645, .F. ) ;
#4356 = DIRECTION ( 'NONE',  ( -0.000000000000000000, 1.000000000000000000, -0.000000000000000000 ) ) ;
#4357 = CARTESIAN_POINT ( 'NONE',  ( 0.7145311798163274108, 9.237604307034018802, -2.124379920709345337E-16 ) ) ;
#4358 = ORIENTED_EDGE ( 'NONE', *, *, #49839, .F. ) ;
#4359 = ORIENTED_EDGE ( 'NONE', *, *, #48104, .F. ) ;
#4360 = EDGE_CURVE ( 'NONE', #40284, #69371, #53442, .T. ) ;
#4361 = CARTESIAN_POINT ( 'NONE',  ( 46.75120595639165089, 10.49875654307468231, 89.57072679854206854 ) ) ;
#4362 = CARTESIAN_POINT ( 'NONE',  ( -178.5835577246388084, 93.42126246260832545, -74.20141784023681453 ) ) ;
#4363 = CARTESIAN_POINT ( 'NONE',  ( 135.7265100247341536, 43.74748294124387371, -89.93937249815461143 ) ) ;
#4364 = VERTEX_POINT ( 'NONE', #44294 ) ;
#4365 = CARTESIAN_POINT ( 'NONE',  ( -173.1211646369891071, 87.12891641440859303, -7.867406574286297527 ) ) ;
#4366 = CARTESIAN_POINT ( 'NONE',  ( 24.39800339187844003, 60.26242556095705538, 41.38025477438755928 ) ) ;
#4367 = CARTESIAN_POINT ( 'NONE',  ( -6.840165690716681013, 7.836465889224657921, 3.319927015524997138 ) ) ;
#4368 = DIRECTION ( 'NONE',  ( -0.000000000000000000, -0.000000000000000000, 1.000000000000000000 ) ) ;
#4369 = CARTESIAN_POINT ( 'NONE',  ( 0.000000000000000000, 0.000000000000000000, 41.38025477438755928 ) ) ;
#4370 = CARTESIAN_POINT ( 'NONE',  ( 93.71772995179811971, 21.96265635001559247, 39.67534872124095813 ) ) ;
#4371 = B_SPLINE_CURVE_WITH_KNOTS ( 'NONE', 3,
 ( #58627, #10443, #43831, #65311, #64262, #5855, #6209, #27662, #54385, #32943, #31917, #53345, #32264, #26296, #53696, #60016, #17098, #43490, #16759, #64966, #31565, #16070, #38220, #4825, #26971, #69528, #47726, #59661, #69188, #48401, #43142, #21016, #27311, #5176, #26638, #11475, #64611, #54029, #233, #42461, #63918, #21347, #21691, #16422, #42794 ),
 .UNSPECIFIED., .F., .F.,
 ( 4, 2, 2, 2, 2, 2, 2, 2, 2, 2, 2, 1, 2, 2, 2, 2, 2, 2, 2, 2, 2, 2, 4 ),
 ( 0.000000000000000000, 0.001510509505235922700, 0.002265764257853866703, 0.003021019010471810273, 0.004531528515707697845, 0.005286783268325657460, 0.006042038020943617076, 0.007552547526179537174, 0.009063057031415456405, 0.01057356653665137737, 0.01132882128926933699, 0.01208407604188729660, 0.01283933079450525622, 0.01359458554712321930, 0.01510509505235920619, 0.01586034980497719182, 0.01661560455759517399, 0.01812611406283112792, 0.01963662356806708184, 0.02039187832068503972, 0.02114713307330299760, 0.02265764257853894806, 0.02416815208377490198 ),
 .UNSPECIFIED. ) ;
#4372 = EDGE_CURVE ( 'NONE', #11778, #9171, #17235, .T. ) ;
#4373 = VERTEX_POINT ( 'NONE', #7022 ) ;
#4374 = CARTESIAN_POINT ( 'NONE',  ( 9.416656162223551618, 6.380306691996769253, 68.32325512165303394 ) ) ;
#4375 = EDGE_CURVE ( 'NONE', #56665, #43797, #55551, .T. ) ;
#4376 = CYLINDRICAL_SURFACE ( 'NONE', #64379, 185.0000000000000000 ) ;
#4377 = CARTESIAN_POINT ( 'NONE',  ( 197.3700262219430783, 98.41176242030789467, 38.33750891837946284 ) ) ;
#4378 = VECTOR ( 'NONE', #2631, 1000.000000000000000 ) ;
#4379 = EDGE_CURVE ( 'NONE', #12998, #41403, #48441, .T. ) ;
#4380 = CARTESIAN_POINT ( 'NONE',  ( -76.28906486289076838, 22.50303357844624230, 84.48732397307654196 ) ) ;
#4382 = ORIENTED_EDGE ( 'NONE', *, *, #4520, .T. ) ;
#4381 = CARTESIAN_POINT ( 'NONE',  ( 230.9999999999999432, 225.0000000000000000, -2.000000000000000000 ) ) ;
#4383 = VERTEX_POINT ( 'NONE', #34811 ) ;
#4384 = AXIS2_PLACEMENT_3D ( 'NONE', #3481, #29873, #67509 ) ;
#4385 = ORIENTED_EDGE ( 'NONE', *, *, #37619, .F. ) ;
#4386 = CARTESIAN_POINT ( 'NONE',  ( -5.066666666666664653, 8.000000000000000000, 43.13333333333333286 ) ) ;
#4387 = CARTESIAN_POINT ( 'NONE',  ( 201.9777685760379882, 102.6876480786892927, -77.67199324841566010 ) ) ;
#4388 = CARTESIAN_POINT ( 'NONE',  ( 204.6977192012829789, -170.0000000000000000, -51.32593103262161094 ) ) ;
#4389 = CYLINDRICAL_SURFACE ( 'NONE', #65772, 7.500000000000013323 ) ;
#4390 = CARTESIAN_POINT ( 'NONE',  ( -85.12122836439577611, 25.97531040437156591, -11.91969542759261280 ) ) ;
#4391 = LINE ( 'NONE', #57852, #25285 ) ;
#4392 = CARTESIAN_POINT ( 'NONE',  ( -151.6716822472524484, 66.03661194063731443, -49.50755342994084884 ) ) ;
#4393 = ORIENTED_EDGE ( 'NONE', *, *, #4520, .F. ) ;
#4394 = ORIENTED_EDGE ( 'NONE', *, *, #65093, .T. ) ;
#4395 = CARTESIAN_POINT ( 'NONE',  ( -417.6627218934913230, 219.4906275429376308, 111.5502958579881749 ) ) ;
#4396 = CARTESIAN_POINT ( 'NONE',  ( 0.000000000000000000, 35.26862320190615208, -5.000000000000000000 ) ) ;
#4397 = CARTESIAN_POINT ( 'NONE',  ( 117.0725462099858447, 32.17176564273682260, 87.68110821929519716 ) ) ;
#4398 = CARTESIAN_POINT ( 'NONE',  ( 117.0069443446175512, 33.26475960880694771, -13.32765567664555029 ) ) ;
#4399 = CARTESIAN_POINT ( 'NONE',  ( 544.6745185807129701, 190.0000000000000000, 34.73878747406611467 ) ) ;
#4400 = DIRECTION ( 'NONE',  ( -3.946780934433987212E-15, -1.000000000000000000, 5.551115123125782702E-17 ) ) ;
#4401 = ADVANCED_FACE ( 'NONE', ( #14035 ), #66831, .F. ) ;
#4402 = CARTESIAN_POINT ( 'NONE',  ( 1.667562369267758360, -64.99262834925670518, 43.58025477438756923 ) ) ;
#4403 = ORIENTED_EDGE ( 'NONE', *, *, #17309, .T. ) ;
#4404 = VERTEX_POINT ( 'NONE', #67182 ) ;
#4405 = ORIENTED_EDGE ( 'NONE', *, *, #49887, .F. ) ;
#4406 = DIRECTION ( 'NONE',  ( -1.000000000000000000, 0.000000000000000000, 0.000000000000000000 ) ) ;
#4407 = CARTESIAN_POINT ( 'NONE',  ( 176.7302122685738652, 74.31432059049257077, -91.29563362033026408 ) ) ;
#4408 = LINE ( 'NONE', #25872, #23224 ) ;
#4409 = CARTESIAN_POINT ( 'NONE',  ( -38.92718193365330848, 11.96647478777220286, -69.17238878754035625 ) ) ;
#4410 = AXIS2_PLACEMENT_3D ( 'NONE', #23079, #24730, #27991 ) ;
#4411 = CARTESIAN_POINT ( 'NONE',  ( -153.1121305730337383, 67.29834700374526335, -8.887376870342574620 ) ) ;
#4412 = CYLINDRICAL_SURFACE ( 'NONE', #21049, 65.00000000000000000 ) ;
#4413 = CARTESIAN_POINT ( 'NONE',  ( 13.14401442664831343, 6.430459733718342008, -9.151694974088321999 ) ) ;
#4414 = SHAPE_REPRESENTATION_RELATIONSHIP ( 'NONE' , 'NONE' ,  #63080, #69249 ) ;
#4415 = CARTESIAN_POINT ( 'NONE',  ( 23.23965501943000689, 7.861749956303025755, 9.686424920567322516 ) ) ;
#4416 = CARTESIAN_POINT ( 'NONE',  ( 16.92909711280922735, 28.82167224275331208, 6.893343212288921329 ) ) ;
#4417 = CARTESIAN_POINT ( 'NONE',  ( -118.4622862908118606, 41.79153065058246597, 12.32190642974081030 ) ) ;
#4418 = DIRECTION ( 'NONE',  ( -1.000000000000000000, 0.000000000000000000, 0.000000000000000000 ) ) ;
#4419 = CARTESIAN_POINT ( 'NONE',  ( -13.24252603915608617, 63.63674649211943546, 133.5802547743875550 ) ) ;
#4420 = DIRECTION ( 'NONE',  ( 1.000000000000000000, -0.000000000000000000, -0.000000000000000000 ) ) ;
#4421 = CARTESIAN_POINT ( 'NONE',  ( 9.050324533885207856, 7.384616180193985358, 7.339830793012372290 ) ) ;
#4422 = CIRCLE ( 'NONE', #29131, 35.00000000000000000 ) ;
#4423 = EDGE_LOOP ( 'NONE', ( #51163, #12212, #67956, #68008 ) ) ;
#4424 = CARTESIAN_POINT ( 'NONE',  ( -31.11269837220812207, -31.11269837220801193, 0.000000000000000000 ) ) ;
#4425 = APPLICATION_PROTOCOL_DEFINITION ( 'draft international standard', 'automotive_design', 1998, #51611 ) ;
#4426 = CARTESIAN_POINT ( 'NONE',  ( 175.5493994043410737, 73.18740965572601453, 41.87606852396054080 ) ) ;
#4427 = CARTESIAN_POINT ( 'NONE',  ( -17.35806700812657155, -28.56537427343508995, 6.893342935626296963 ) ) ;
#4428 = CARTESIAN_POINT ( 'NONE',  ( -102.2801239173131052, 33.91021738430207222, -50.01457726497594081 ) ) ;
#4429 = PRESENTATION_LAYER_ASSIGNMENT (  '', '', ( #68453 ) ) ;
#4430 = CARTESIAN_POINT ( 'NONE',  ( 184.3966782763552317, 83.48172388049826509, -50.46844882507220831 ) ) ;
#4431 = EDGE_LOOP ( 'NONE', ( #49238, #30176, #26418, #57787, #61721, #36911, #47133, #38510 ) ) ;
#4432 = EDGE_CURVE ( 'NONE', #53754, #46832, #13689, .T. ) ;
#4433 = ORIENTED_EDGE ( 'NONE', *, *, #30921, .F. ) ;
#4434 = EDGE_CURVE ( 'NONE', #10004, #46743, #54311, .T. ) ;
#4435 = CARTESIAN_POINT ( 'NONE',  ( 209.3223706822284100, 18.00000000000002842, 31.44247402469554942 ) ) ;
#4436 = EDGE_CURVE ( 'NONE', #67011, #61969, #24948, .T. ) ;
#4437 = CARTESIAN_POINT ( 'NONE',  ( 198.4059165548112276, 99.71594270191990006, 13.95396656640263089 ) ) ;
#4438 = ORIENTED_EDGE ( 'NONE', *, *, #56470, .T. ) ;
#4439 = EDGE_CURVE ( 'NONE', #61512, #35195, #55470, .T. ) ;
#4440 = DIRECTION ( 'NONE',  ( -1.000000000000000000, 0.000000000000000000, 0.000000000000000000 ) ) ;
#4441 = ORIENTED_EDGE ( 'NONE', *, *, #62368, .F. ) ;
#4442 = CARTESIAN_POINT ( 'NONE',  ( 144.4165763529819344, -26.99999999999998224, 129.0000000000000000 ) ) ;
#4443 = CARTESIAN_POINT ( 'NONE',  ( 133.6288034103010602, 41.28708886999552163, 29.51034083899532590 ) ) ;
#4444 = CARTESIAN_POINT ( 'NONE',  ( -25.87147652227456263, 70.00000000000000000, 129.5802547743875550 ) ) ;
#4445 = AXIS2_PLACEMENT_3D ( 'NONE', #32054, #54172, #26777 ) ;
#4446 = DIRECTION ( 'NONE',  ( 0.000000000000000000, 0.000000000000000000, -1.000000000000000000 ) ) ;
#4447 = PLANE ( 'NONE',  #28287 ) ;
#4449 = ORIENTED_EDGE ( 'NONE', *, *, #37207, .T. ) ;
#4448 = DIRECTION ( 'NONE',  ( -0.000000000000000000, -0.000000000000000000, -1.000000000000000000 ) ) ;
#4450 = DIRECTION ( 'NONE',  ( -0.7071067811865543451, -7.105427357601001070E-15, -0.7071067811865408004 ) ) ;
#4451 = ORIENTED_EDGE ( 'NONE', *, *, #11819, .F. ) ;
#4452 = ORIENTED_EDGE ( 'NONE', *, *, #34660, .T. ) ;
#4453 = CARTESIAN_POINT ( 'NONE',  ( -118.7011677090247019, 41.93687969120205850, -17.71047622372893215 ) ) ;
#4454 = CARTESIAN_POINT ( 'NONE',  ( 5.799999999999999822, 9.237604307034018802, 0.000000000000000000 ) ) ;
#4456 = EDGE_CURVE ( 'NONE', #7966, #64522, #50106, .T. ) ;
#4455 =( REPRESENTATION_RELATIONSHIP ('NONE','NONE', #40274, #60409 ) REPRESENTATION_RELATIONSHIP_WITH_TRANSFORMATION ( #37203 )SHAPE_REPRESENTATION_RELATIONSHIP( ) );
#4457 = CARTESIAN_POINT ( 'NONE',  ( 26.11269837220806167, 0.000000000000000000, 2.000000000000000000 ) ) ;
#4458 = ADVANCED_FACE ( 'NONE', ( #43861 ), #27341, .T. ) ;
#4459 = B_SPLINE_CURVE_WITH_KNOTS ( 'NONE', 3,
 ( #49447, #67058, #44887, #17816, #18504, #2672, #44171, #39271, #49802, #29068, #60715, #60374, #1993, #1627, #24135, #12531, #66021, #45576, #65659, #50513, #66368, #17448, #33993, #54734, #23092, #18854, #33652, #61063, #40303, #28003, #38925, #12188, #39957, #50855, #55431, #1280, #7262, #12891, #55080, #22737, #6900, #50164, #61413 ),
 .UNSPECIFIED., .F., .F.,
 ( 4, 2, 2, 2, 2, 2, 2, 2, 2, 2, 2, 2, 1, 2, 2, 2, 2, 2, 2, 2, 2, 4 ),
 ( 0.02362927190606132002, 0.02510248541563188038, 0.02583909217041715708, 0.02657569892520243032, 0.02804891243477299068, 0.02952212594434355103, 0.03025873269912882774, 0.03099533945391410791, 0.03246855296348467868, 0.03394176647305525985, 0.03541497998262583408, 0.03615158673741113160, 0.03688819349219642912, 0.03762480024698172665, 0.03836140700176702417, 0.03983462051133762616, 0.04130783402090822121, 0.04278104753047881625, 0.04351765428526410684, 0.04425426104004940436, 0.04572747454961999247, 0.04720068805919058752 ),
 .UNSPECIFIED. ) ;
#4461 = ORIENTED_EDGE ( 'NONE', *, *, #65946, .F. ) ;
#4460 = CARTESIAN_POINT ( 'NONE',  ( -147.7845268487069461, 62.73119438705056439, -35.00051754678168692 ) ) ;
#4462 = DIRECTION ( 'NONE',  ( 1.156482317317871478E-16, 0.000000000000000000, 1.000000000000000000 ) ) ;
#4463 = AXIS2_PLACEMENT_3D ( 'NONE', #8026, #23865, #29827 ) ;
#4464 = PLANE ( 'NONE',  #60927 ) ;
#4465 = VERTEX_POINT ( 'NONE', #38962 ) ;
#4466 = CARTESIAN_POINT ( 'NONE',  ( -62.48965350618346548, 16.80247907725182799, -14.86921336900190482 ) ) ;
#4467 = CARTESIAN_POINT ( 'NONE',  ( -127.4644500646575125, 48.74852676951795161, -76.59546237094302512 ) ) ;
#4468 = CARTESIAN_POINT ( 'NONE',  ( 39.40195752203892710, 9.424259417798138472, -89.30891864635511013 ) ) ;
#4469 = CARTESIAN_POINT ( 'NONE',  ( -101.3602137809054540, 32.31558061113913283, 3.716661569264940734 ) ) ;
#4470 = CARTESIAN_POINT ( 'NONE',  ( -94.88380767928869375, 29.17964217339916999, -68.08975550236192475 ) ) ;
#4471 = ORIENTED_EDGE ( 'NONE', *, *, #14219, .T. ) ;
#4472 = ORIENTED_EDGE ( 'NONE', *, *, #53094, .F. ) ;
#4473 = AXIS2_PLACEMENT_3D ( 'NONE', #6447, #59199, #11358 ) ;
#4474 = CARTESIAN_POINT ( 'NONE',  ( 187.9007786055418592, 85.78077355327280884, -67.43016102822709001 ) ) ;
#4475 = CARTESIAN_POINT ( 'NONE',  ( -167.9853834315979384, 81.58767916550894483, -36.72585540580842434 ) ) ;
#4476 = PLANE ( 'NONE',  #54164 ) ;
#4477 = CIRCLE ( 'NONE', #13469, 25.12245591505646303 ) ;
#4478 = CARTESIAN_POINT ( 'NONE',  ( 103.0004140566503139, 26.76634862952791494, -68.25275454392931351 ) ) ;
#4479 = CARTESIAN_POINT ( 'NONE',  ( -75.65611349188965562, 22.26947559308018043, 31.04466364538752288 ) ) ;
#4480 = CARTESIAN_POINT ( 'NONE',  ( 86.62931800182293784, 19.42108912189597092, 29.71208757247930521 ) ) ;
#4481 = CARTESIAN_POINT ( 'NONE',  ( 0.1306530452038078272, 5.952467836904149934, -5.690023276062396107 ) ) ;
#4482 = DIRECTION ( 'NONE',  ( 0.000000000000000000, -1.000000000000000000, 0.000000000000000000 ) ) ;
#4483 = CARTESIAN_POINT ( 'NONE',  ( -165.7138623879809529, 79.24467249981142913, -67.84157927087939299 ) ) ;
#4484 = EDGE_LOOP ( 'NONE', ( #2107, #34781, #40469, #13611 ) ) ;
#4485 = PLANE ( 'NONE',  #61384 ) ;
#4486 = VERTEX_POINT ( 'NONE', #16788 ) ;
#4487 = CARTESIAN_POINT ( 'NONE',  ( 85.83322572930757133, 20.21160859307071789, -89.51066537983908233 ) ) ;
#4488 = PLANE ( 'NONE',  #10493 ) ;
#4489 = LINE ( 'NONE', #19627, #58799 ) ;
#4490 = CARTESIAN_POINT ( 'NONE',  ( 133.8566784816069060, 42.60093787723655367, 71.35489142945907304 ) ) ;
#4491 = CARTESIAN_POINT ( 'NONE',  ( -67.03031041878467988, 33.66749151869449008, 170.0000000000000000 ) ) ;
#4492 = CARTESIAN_POINT ( 'NONE',  ( 437.3372781065086201, 0.000000000000000000, -141.4497041420118251 ) ) ;
#4493 = CARTESIAN_POINT ( 'NONE',  ( 33.44527180510250020, 7.709232309484699286, -74.54778285784610148 ) ) ;
#4494 = CARTESIAN_POINT ( 'NONE',  ( 0.000000000000000000, 0.000000000000000000, 25.00000000000007816 ) ) ;
#4495 = VECTOR ( 'NONE', #58359, 1000.000000000000227 ) ;
#4496 = CARTESIAN_POINT ( 'NONE',  ( -33.36965723649377935, 10.93726715887721568, -23.22402601025658697 ) ) ;
#4497 = EDGE_LOOP ( 'NONE', ( #21687, #30146, #44935, #48645 ) ) ;
#4498 = CARTESIAN_POINT ( 'NONE',  ( -123.6557841886868658, 46.23505328920332147, -88.94146719048309535 ) ) ;
#4499 = EDGE_LOOP ( 'NONE', ( #31374, #26256 ) ) ;
#4500 = CARTESIAN_POINT ( 'NONE',  ( 64.98797965777978902, -1.250000000000021094, 170.0000000000000000 ) ) ;
#4501 = CARTESIAN_POINT ( 'NONE',  ( -27.92096271590487788, -31.01184599629533167, 13.79046412439886460 ) ) ;
#4502 = CARTESIAN_POINT ( 'NONE',  ( -24.07146903340143496, 8.497560047608732958, 12.33779482100903735 ) ) ;
#4503 = DIRECTION ( 'NONE',  ( -0.8118923937861950435, -0.5838071093367415143, 0.000000000000000000 ) ) ;
#4504 = CARTESIAN_POINT ( 'NONE',  ( -15.31363169557738502, 7.494880774891999664, -70.25007158120349970 ) ) ;
#4505 = CARTESIAN_POINT ( 'NONE',  ( -100.4262673593280368, 31.84860241619272969, -8.387597469391586458 ) ) ;
#4506 = CARTESIAN_POINT ( 'NONE',  ( 151.7783534118502189, 54.60545177578660514, -38.73408018630978233 ) ) ;
#4507 = ORIENTED_EDGE ( 'NONE', *, *, #67988, .F. ) ;
#4508 = CARTESIAN_POINT ( 'NONE',  ( 403.0071894358271152, 1011.991584617514945, 569.0068267248735765 ) ) ;
#4509 = AXIS2_PLACEMENT_3D ( 'NONE', #52504, #4325, #66976 ) ;
#4510 = LINE ( 'NONE', #10469, #38529 ) ;
#4511 = CARTESIAN_POINT ( 'NONE',  ( 174.4912080999798718, 73.57140295268874297, -13.29444283027056883 ) ) ;
#4512 = CARTESIAN_POINT ( 'NONE',  ( -109.3386876948163717, 37.66246927061208538, 62.27823371598848468 ) ) ;
#4513 = DIRECTION ( 'NONE',  ( 0.000000000000000000, 0.000000000000000000, -1.000000000000000000 ) ) ;
#4514 = EDGE_LOOP ( 'NONE', ( #56246, #66798, #21095, #54977 ) ) ;
#4515 = DIRECTION ( 'NONE',  ( 0.7071067811865475727, 0.000000000000000000, 0.7071067811865474617 ) ) ;
#4516 = CARTESIAN_POINT ( 'NONE',  ( -0.8011128725815461760, 6.535315321814184841, -13.43344384470691111 ) ) ;
#4517 = CARTESIAN_POINT ( 'NONE',  ( 112.5554747942045850, 29.96654954475021171, 29.97270286920888438 ) ) ;
#4518 = EDGE_CURVE ( 'NONE', #28008, #68407, #60749, .T. ) ;
#4519 = CARTESIAN_POINT ( 'NONE',  ( -157.0046402715469753, 70.80872207626528336, 91.63790604792896488 ) ) ;
#4520 = EDGE_CURVE ( 'NONE', #9355, #65052, #29182, .T. ) ;
#4521 = CARTESIAN_POINT ( 'NONE',  ( 135.6842057900327347, 42.53841116629840968, 44.29889548343480499 ) ) ;
#4522 = VERTEX_POINT ( 'NONE', #37906 ) ;
#4523 = CARTESIAN_POINT ( 'NONE',  ( 199.3743599161302882, 99.31857334527873604, 42.01559847254342372 ) ) ;
#4524 = CARTESIAN_POINT ( 'NONE',  ( 41.66904755831210849, -9.150666335777657423E-14, 85.00100000000000477 ) ) ;
#4525 = CARTESIAN_POINT ( 'NONE',  ( 187.5165082312810512, 86.85340440641662951, 32.94302383692840408 ) ) ;
#4526 = CARTESIAN_POINT ( 'NONE',  ( 155.7265855639938934, 57.57443315515126159, 29.60160751965668524 ) ) ;
#4527 = EDGE_CURVE ( 'NONE', #58159, #37433, #21720, .T. ) ;
#4528 = CARTESIAN_POINT ( 'NONE',  ( -21.27554331372911278, -61.43430442924894663, 41.38025477438755928 ) ) ;
#4529 = VECTOR ( 'NONE', #51177, 1000.000000000000000 ) ;
#4530 = VERTEX_POINT ( 'NONE', #44576 ) ;
#4531 = CARTESIAN_POINT ( 'NONE',  ( 173.9457771591584390, 73.05793967547532475, 61.33444114611717879 ) ) ;
#4532 = ORIENTED_EDGE ( 'NONE', *, *, #64291, .T. ) ;
#4533 = CARTESIAN_POINT ( 'NONE',  ( -109.5142642360664098, 36.61018064014776741, -44.56230308795456097 ) ) ;
#4534 = CARTESIAN_POINT ( 'NONE',  ( 2.699999999999990408, 2.467663300281916154E-15, 19.99999999999998934 ) ) ;
#4535 = ADVANCED_FACE ( 'NONE', ( #49836 ), #6595, .F. ) ;
#4536 = CYLINDRICAL_SURFACE ( 'NONE', #13736, 7.500000000000020428 ) ;
#4538 = VERTEX_POINT ( 'NONE', #28390 ) ;
#4537 = DIRECTION ( 'NONE',  ( 0.000000000000000000, 1.000000000000000000, -0.000000000000000000 ) ) ;
#4539 = CARTESIAN_POINT ( 'NONE',  ( -177.5259994307673423, 92.16784265327251546, 32.23362038954493158 ) ) ;
#4540 = AXIS2_PLACEMENT_3D ( 'NONE', #13314, #56207, #63225 ) ;
#4541 = CARTESIAN_POINT ( 'NONE',  ( 15.78827728214693416, 6.500811158483284835, -23.67439350822212774 ) ) ;
#4542 = DIRECTION ( 'NONE',  ( -1.000000000000000000, 0.000000000000000000, 0.000000000000000000 ) ) ;
#4543 = VERTEX_POINT ( 'NONE', #5882 ) ;
#4544 = CYLINDRICAL_SURFACE ( 'NONE', #15389, 5.000000000000000888 ) ;
#4545 = DIRECTION ( 'NONE',  ( -0.04486483035051862939, 0.9989930665413143673, 0.000000000000000000 ) ) ;
#4546 = CARTESIAN_POINT ( 'NONE',  ( 140.1999945597798956, 45.38880890490929687, 59.84517000566086153 ) ) ;
#4547 = DIRECTION ( 'NONE',  ( -0.000000000000000000, -1.000000000000000000, -0.000000000000000000 ) ) ;
#4548 = FACE_OUTER_BOUND ( 'NONE', #35942, .T. ) ;
#4549 = CARTESIAN_POINT ( 'NONE',  ( 422.4999999999999432, 207.5000000000000284, 378.0000000000000000 ) ) ;
#4550 = ORIENTED_EDGE ( 'NONE', *, *, #22704, .T. ) ;
#4551 = CARTESIAN_POINT ( 'NONE',  ( 46.89016064832840414, 10.52130577388959409, 10.08109367583877969 ) ) ;
#4552 = ORIENTED_EDGE ( 'NONE', *, *, #15580, .F. ) ;
#4553 = VECTOR ( 'NONE', #17826, 1000.000000000000000 ) ;
#4554 = CARTESIAN_POINT ( 'NONE',  ( 150.9013375937531123, 53.96275732797608526, -13.15108574339470060 ) ) ;
#4555 = LINE ( 'NONE', #14764, #53364 ) ;
#4556 = CARTESIAN_POINT ( 'NONE',  ( 102.7938674513918755, 26.67851209377774424, 38.12245759428292757 ) ) ;
#4557 = B_SPLINE_CURVE_WITH_KNOTS ( 'NONE', 3,
 ( #1103, #38384, #53848, #64772, #69356, #59480, #54191, #37334, #27128, #17267, #32422, #42950, #16579, #64420, #48561, #16920, #65476, #6013, #38741, #32763, #27473, #12004, #48916, #11640, #38036, #22209, #54550, #43998, #43296, #21175, #60186, #754, #15889, #46, #11291, #5340, #47890, #53153, #37684, #49269, #16231, #43647, #5666, #42620, #65124 ),
 .UNSPECIFIED., .F., .F.,
 ( 4, 2, 2, 2, 2, 2, 2, 2, 2, 2, 2, 1, 2, 2, 2, 2, 2, 2, 2, 2, 2, 2, 4 ),
 ( 1.440969542111313559E-17, 0.001510509505235931157, 0.002265764257853871907, 0.003021019010471812441, 0.004531528515707694375, 0.005286783268325651389, 0.006042038020943608402, 0.007552547526179553654, 0.009063057031415498038, 0.01057356653665144156, 0.01132882128926941678, 0.01208407604188739722, 0.01283933079450537591, 0.01359458554712335808, 0.01510509505235932415, 0.01586034980497731325, 0.01661560455759529889, 0.01812611406283125629, 0.01963662356806721021, 0.02039187832068517156, 0.02114713307330312944, 0.02265764257853901745, 0.02416815208377490892 ),
 .UNSPECIFIED. ) ;
#4558 = CARTESIAN_POINT ( 'NONE',  ( -150.3791492925491298, 64.92185203933370019, -76.61939678162372047 ) ) ;
#4559 = CARTESIAN_POINT ( 'NONE',  ( 188.9999999999999432, 192.0000000000000000, 380.0000000000000000 ) ) ;
#4560 = CARTESIAN_POINT ( 'NONE',  ( 184.3966782763551464, 83.48172388049827930, 3.220652355855141202 ) ) ;
#4561 = CARTESIAN_POINT ( 'NONE',  ( 209.4789161463551181, 113.1367444519303689, -49.60865656310190985 ) ) ;
#4562 = CARTESIAN_POINT ( 'NONE',  ( -15.45727656667689409, 73.34020256436167529, 41.38025477438755928 ) ) ;
#4563 = VERTEX_POINT ( 'NONE', #16454 ) ;
#4564 = DIRECTION ( 'NONE',  ( 1.000000000000000000, 3.697785493223491743E-32, 0.000000000000000000 ) ) ;
#4565 = ORIENTED_EDGE ( 'NONE', *, *, #1100, .F. ) ;
#4566 = CARTESIAN_POINT ( 'NONE',  ( -74.39861643904070831, 21.81123504700009264, 70.93476632660724590 ) ) ;
#4567 = CARTESIAN_POINT ( 'NONE',  ( -94.79166046756729713, 29.13671350128076654, -42.02362451379906361 ) ) ;
#4568 = CARTESIAN_POINT ( 'NONE',  ( 58.47673920847982743, 11.66523265296354772, -76.05570035470118739 ) ) ;
#4569 = LINE ( 'NONE', #30280, #63057 ) ;
#4570 = DIRECTION ( 'NONE',  ( 0.000000000000000000, -1.000000000000000000, 0.000000000000000000 ) ) ;
#4571 = DIRECTION ( 'NONE',  ( -0.8090169943749422332, -0.5877852522924802425, 0.000000000000000000 ) ) ;
#4572 = CARTESIAN_POINT ( 'NONE',  ( 164.8444104055694481, 64.93678790243656351, -71.86516271918338816 ) ) ;
#4573 = ORIENTED_EDGE ( 'NONE', *, *, #57997, .F. ) ;
#4574 = EDGE_CURVE ( 'NONE', #38828, #13453, #27371, .T. ) ;
#4575 = CARTESIAN_POINT ( 'NONE',  ( 0.000000000000000000, 0.000000000000000000, 0.000000000000000000 ) ) ;
#4576 = CARTESIAN_POINT ( 'NONE',  ( 198.4942811600313064, 98.20737091473505131, -93.29402655745694517 ) ) ;
#4577 = VERTEX_POINT ( 'NONE', #23126 ) ;
#4578 = ORIENTED_EDGE ( 'NONE', *, *, #67425, .F. ) ;
#4579 = CARTESIAN_POINT ( 'NONE',  ( -31.43908319763709969, 10.61114334766717171, -62.16174795566551836 ) ) ;
#4580 = CARTESIAN_POINT ( 'NONE',  ( -15.55634918610411077, -41.66904755831209428, 85.00100000000000477 ) ) ;
#4581 = DIRECTION ( 'NONE',  ( 0.000000000000000000, -1.000000000000000000, 0.000000000000000000 ) ) ;
#4582 = CARTESIAN_POINT ( 'NONE',  ( -26.28838124991334979, 20.64471194235530049, 6.893343212288937316 ) ) ;
#4583 = CARTESIAN_POINT ( 'NONE',  ( -142.2626321327577159, 58.26997216742665842, 9.417068183414567528 ) ) ;
#4584 = AXIS2_PLACEMENT_3D ( 'NONE', #60998, #55723, #33927 ) ;
#4585 = ORIENTED_EDGE ( 'NONE', *, *, #35200, .F. ) ;
#4586 = CARTESIAN_POINT ( 'NONE',  ( -132.9126122820979106, 52.52752252041127434, 35.46337234881715972 ) ) ;
#4587 = VERTEX_POINT ( 'NONE', #12222 ) ;
#4588 = CARTESIAN_POINT ( 'NONE',  ( 209.9944361927104808, 113.8994774711241291, 4.548133007360330993 ) ) ;
#4589 = CARTESIAN_POINT ( 'NONE',  ( -143.8756912989386763, 60.83492035645721074, 43.18009283058132297 ) ) ;
#4590 = AXIS2_PLACEMENT_3D ( 'NONE', #44668, #50982, #20015 ) ;
#4591 = CARTESIAN_POINT ( 'NONE',  ( 212.0180052085437694, 116.9552462415714871, 38.37144164438262095 ) ) ;
#4592 = DIRECTION ( 'NONE',  ( -0.000000000000000000, -0.000000000000000000, -1.000000000000000000 ) ) ;
#4593 = PRODUCT_DEFINITION_SHAPE ( 'NONE', 'NONE',  #56848 ) ;
#4594 = ADVANCED_FACE ( 'NONE', ( #49482 ), #33688, .F. ) ;
#4595 = VECTOR ( 'NONE', #8965, 1000.000000000000000 ) ;
#4596 = VERTEX_POINT ( 'NONE', #55118 ) ;
#4597 = VERTEX_POINT ( 'NONE', #11501 ) ;
#4598 = CARTESIAN_POINT ( 'NONE',  ( 111.2988829979105105, -21.46124357533057747, -4.839350883597181685 ) ) ;
#4599 = CARTESIAN_POINT ( 'NONE',  ( -165.9986675144416211, 79.53506019208356292, -13.00008028462095133 ) ) ;
#4600 = DIRECTION ( 'NONE',  ( 0.000000000000000000, 0.000000000000000000, 1.000000000000000000 ) ) ;
#4601 = ADVANCED_FACE ( 'NONE', ( #54409 ), #1315, .F. ) ;
#4602 = CARTESIAN_POINT ( 'NONE',  ( 66.94779593213115731, 13.61918177102165650, 43.70422013568025221 ) ) ;
#4603 = AXIS2_PLACEMENT_3D ( 'NONE', #54725, #6552, #6195 ) ;
#4604 = CARTESIAN_POINT ( 'NONE',  ( -190.0468231512975876, 108.2116162189844886, -72.35473219539915135 ) ) ;
#4605 = EDGE_LOOP ( 'NONE', ( #59725, #21567, #9865, #35561 ) ) ;
#4606 = CARTESIAN_POINT ( 'NONE',  ( 11.30618213853490239, -74.15344055032291237, 170.0000000000000000 ) ) ;
#4607 = CARTESIAN_POINT ( 'NONE',  ( -94.79534239005249674, 29.13842790650043924, 64.32042552946333558 ) ) ;
#4608 = ORIENTED_EDGE ( 'NONE', *, *, #19669, .T. ) ;
#4609 = CARTESIAN_POINT ( 'NONE',  ( -80.55742067659895156, 23.05042616197510696, 3.800353480099713632 ) ) ;
#4610 = EDGE_LOOP ( 'NONE', ( #55131, #56451, #22653, #24646 ) ) ;
#4612 = ORIENTED_EDGE ( 'NONE', *, *, #31145, .F. ) ;
#4611 = EDGE_CURVE ( 'NONE', #58000, #22638, #49131, .T. ) ;
#4613 = ORIENTED_EDGE ( 'NONE', *, *, #50509, .T. ) ;
#4614 = CARTESIAN_POINT ( 'NONE',  ( -118.9668643994983341, 43.27909474462860828, 14.16267398761431195 ) ) ;
#4615 = ADVANCED_FACE ( 'NONE', ( #20512 ), #30386, .F. ) ;
#4617 = EDGE_CURVE ( 'NONE', #55210, #15602, #36710, .T. ) ;
#4616 = CARTESIAN_POINT ( 'NONE',  ( -176.3896317155479210, 90.84057090619016606, 58.40173573172133814 ) ) ;
#4618 = CARTESIAN_POINT ( 'NONE',  ( 19.54475376904847650, 6.649964688461120765, 17.16624909598245097 ) ) ;
#4619 = ORIENTED_EDGE ( 'NONE', *, *, #21593, .T. ) ;
#4620 = DIRECTION ( 'NONE',  ( 0.9839295885986295565, 0.1785568947986370392, 0.000000000000000000 ) ) ;
#4621 = LINE ( 'NONE', #59459, #61269 ) ;
#4622 = LINE ( 'NONE', #38017, #64786 ) ;
#4623 = CARTESIAN_POINT ( 'NONE',  ( 107.0471828278920583, 27.43080724084234490, -36.62059212188487578 ) ) ;
#4624 = CARTESIAN_POINT ( 'NONE',  ( -25.81763596640060854, 8.735969132042862739, 32.74552005507152330 ) ) ;
#4625 = CARTESIAN_POINT ( 'NONE',  ( -13.24252603915608617, 63.63674649211943546, 40.00000000000003553 ) ) ;
#4626 = ORIENTED_EDGE ( 'NONE', *, *, #17150, .F. ) ;
#4627 = AXIS2_PLACEMENT_3D ( 'NONE', #8850, #67257, #25026 ) ;
#4628 = CARTESIAN_POINT ( 'NONE',  ( 47.91750368872954624, -19.31887499200363223, 26.66469104408689006 ) ) ;
#4629 = CARTESIAN_POINT ( 'NONE',  ( -81.24432217070636852, 24.40203426192926628, -62.41292138135722922 ) ) ;
#4631 = CARTESIAN_POINT ( 'NONE',  ( 173.8576514579035575, 72.97529922124009261, 11.99223922032557255 ) ) ;
#4630 = AXIS2_PLACEMENT_3D ( 'NONE', #37735, #47583, #63792 ) ;
#4632 = LINE ( 'NONE', #15196, #49150 ) ;
#4633 = CARTESIAN_POINT ( 'NONE',  ( -843.0889760620008246, -561.4220607509099636, 0.000000000000000000 ) ) ;
#4634 = CARTESIAN_POINT ( 'NONE',  ( 138.4794054115212703, 44.28634680695354575, -91.29333943486163605 ) ) ;
#4635 = CARTESIAN_POINT ( 'NONE',  ( -156.4841188516942623, 70.33041971808550841, 8.609805402347420866 ) ) ;
#4636 = CARTESIAN_POINT ( 'NONE',  ( 198.7765072002625288, 100.1872738704526427, 94.99999999999866418 ) ) ;
#4638 = CARTESIAN_POINT ( 'NONE',  ( 64.93495251696904802, 13.12601614965099373, 3.214085396426615837 ) ) ;
#4637 = AXIS2_PLACEMENT_3D ( 'NONE', #21081, #17074, #49079 ) ;
#4639 = VECTOR ( 'NONE', #59498, 1000.000000000000114 ) ;
#4640 = CARTESIAN_POINT ( 'NONE',  ( -85.96384504792885650, 26.32782846176031200, 66.51262591793364720 ) ) ;
#4641 = CARTESIAN_POINT ( 'NONE',  ( -109.6660553119435377, 36.69391917620600196, 39.34755413696105109 ) ) ;
#4642 = ORIENTED_EDGE ( 'NONE', *, *, #18650, .T. ) ;
#4643 = CONTEXT_DEPENDENT_SHAPE_REPRESENTATION ( #69153, #35033 ) ;
#4644 = CARTESIAN_POINT ( 'NONE',  ( -54.76617051175221462, 15.64622803826644670, 84.00532038758548481 ) ) ;
#4645 = ORIENTED_EDGE ( 'NONE', *, *, #62722, .F. ) ;
#4646 = DIRECTION ( 'NONE',  ( 0.000000000000000000, 0.000000000000000000, 1.000000000000000000 ) ) ;
#4647 = ORIENTED_EDGE ( 'NONE', *, *, #18931, .F. ) ;
#4648 = CARTESIAN_POINT ( 'NONE',  ( 22.89270809252619898, 7.840160460323052583, -67.44744513715251344 ) ) ;
#4649 = SURFACE_STYLE_USAGE ( .BOTH. , #58450 ) ;
#4650 = PLANE ( 'NONE',  #24544 ) ;
#4651 = CARTESIAN_POINT ( 'NONE',  ( 64.93495251696904802, 13.12601614965099373, -23.63046519403706469 ) ) ;
#4652 = CARTESIAN_POINT ( 'NONE',  ( 136.9822423813093337, 44.53121110416872597, -50.34504590549451564 ) ) ;
#4653 = CARTESIAN_POINT ( 'NONE',  ( 31.95008798096002423, 7.556925044648911793, -42.13730592359904392 ) ) ;
#4654 = EDGE_CURVE ( 'NONE', #23082, #15354, #60817, .T. ) ;
#4655 = LINE ( 'NONE', #26116, #55110 ) ;
#4656 = LINE ( 'NONE', #52833, #38629 ) ;
#4657 = PLANE ( 'NONE',  #54285 ) ;
#4658 = ORIENTED_EDGE ( 'NONE', *, *, #37299, .T. ) ;
#4659 = ORIENTED_EDGE ( 'NONE', *, *, #47648, .T. ) ;
#4660 = EDGE_CURVE ( 'NONE', #9825, #16384, #502, .T. ) ;
#4661 = CARTESIAN_POINT ( 'NONE',  ( 176.5251334471615223, 75.51433118793448784, 84.53325931958181627 ) ) ;
#4662 = CARTESIAN_POINT ( 'NONE',  ( -167.4860113959264538, 82.52233889531183308, -10.41155452729346820 ) ) ;
#4663 = CARTESIAN_POINT ( 'NONE',  ( 185.0000000000000000, 0.000000000000000000, 2.499999999999999556 ) ) ;
#4664 = CARTESIAN_POINT ( 'NONE',  ( 283.7669346082183779, 21.75174821959686255, 3.303877464828343768 ) ) ;
#4665 = DIRECTION ( 'NONE',  ( -0.000000000000000000, -1.000000000000000000, -0.000000000000000000 ) ) ;
#4666 = CARTESIAN_POINT ( 'NONE',  ( 175.8963338753314360, 73.51705463274394958, -65.14750092172043594 ) ) ;
#4667 = CARTESIAN_POINT ( 'NONE',  ( -179.0654441437004891, 93.99779465816536117, -46.79209166540439924 ) ) ;
#4668 = CARTESIAN_POINT ( 'NONE',  ( 90.31682503704263354, 20.71196693118261223, -9.927970538514026444 ) ) ;
#4669 = DIRECTION ( 'NONE',  ( -0.000000000000000000, 1.000000000000000000, -0.000000000000000000 ) ) ;
#4670 = DIRECTION ( 'NONE',  ( 0.000000000000000000, 0.000000000000000000, -1.000000000000000000 ) ) ;
#4671 = ADVANCED_FACE ( 'NONE', ( #46909 ), #52095, .T. ) ;
#4672 = CARTESIAN_POINT ( 'NONE',  ( 160.4986104110022893, 61.33701824525266488, 70.61926442309403740 ) ) ;
#4673 = EDGE_CURVE ( 'NONE', #3292, #41626, #41975, .T. ) ;
#4674 = EDGE_CURVE ( 'NONE', #347, #60092, #5713, .T. ) ;
#4675 = VERTEX_POINT ( 'NONE', #37729 ) ;
#4676 = CARTESIAN_POINT ( 'NONE',  ( 132.0563630623057065, 41.51825634609595284, 2.881408396022717255 ) ) ;
#4677 = DIRECTION ( 'NONE',  ( 0.000000000000000000, 0.000000000000000000, 1.000000000000000000 ) ) ;
#4678 = VECTOR ( 'NONE', #35673, 1000.000000000000114 ) ;
#4679 = DIRECTION ( 'NONE',  ( -0.000000000000000000, -0.000000000000000000, -1.000000000000000000 ) ) ;
#4680 = CARTESIAN_POINT ( 'NONE',  ( -2.699999999999990408, 0.000000000000000000, 0.000000000000000000 ) ) ;
#4681 = EDGE_CURVE ( 'NONE', #64121, #16854, #19506, .T. ) ;
#4682 = CARTESIAN_POINT ( 'NONE',  ( 149.9872551245000807, 52.05943539582079893, 10.63948890275607795 ) ) ;
#4683 = CARTESIAN_POINT ( 'NONE',  ( -8.481162655887866109, 7.942265590435539480, 83.80506270299520111 ) ) ;
#4684 = AXIS2_PLACEMENT_3D ( 'NONE', #58250, #22002, #20968 ) ;
#4685 = B_SPLINE_CURVE_WITH_KNOTS ( 'NONE', 3,
 ( #58289, #42796, #69189, #69529, #53697, #21692, #58628, #4826, #27313, #31566, #59662, #10444, #31918, #43491, #63578, #63919, #32265, #47727, #37882, #64263, #16760, #26972, #5517, #5177, #235, #16071, #58978, #43143, #64967, #27663, #26639, #592, #15733, #64612, #48756, #16423, #59325, #32603, #38221, #6210, #11476, #53002, #32944, #36850, #54030, #26297, #5856 ),
 .UNSPECIFIED., .F., .F.,
 ( 4, 2, 2, 2, 2, 2, 2, 2, 2, 2, 2, 1, 2, 2, 2, 2, 2, 2, 2, 2, 2, 2, 2, 4 ),
 ( 0.000000000000000000, 0.003297771944418886533, 0.004122214930523581712, 0.004946657916628276891, 0.006595543888837667248, 0.007419986874942389316, 0.008244429861047111383, 0.009068872847151831715, 0.009893315833256553782, 0.01154220180546602914, 0.01236664479157077029, 0.01319108777767551144, 0.01401553076378025085, 0.01483997374988498853, 0.01566441673598972795, 0.01648885972209446910, 0.01813774569430390976, 0.01896218868040865438, 0.01978663166651340247, 0.02061107465261814709, 0.02143551763872289170, 0.02308440361093238441, 0.02473328958314187712, 0.02638217555535137329 ),
 .UNSPECIFIED. ) ;
#4686 = ORIENTED_EDGE ( 'NONE', *, *, #66109, .F. ) ;
#4687 = CARTESIAN_POINT ( 'NONE',  ( 8.390996311772815019, 10.00000000000000000, -33.00000000000000000 ) ) ;
#4688 = CARTESIAN_POINT ( 'NONE',  ( -60.97011009284707939, 16.34812508431679134, 69.29634183800428104 ) ) ;
#4689 = ORIENTED_EDGE ( 'NONE', *, *, #15095, .T. ) ;
#4690 = AXIS2_PLACEMENT_3D ( 'NONE', #10679, #63473, #25852 ) ;
#4691 = COLOUR_RGB ( '',0.7921568627450980005, 0.8196078431372548767, 0.9333333333333333481 ) ;
#4692 = ORIENTED_EDGE ( 'NONE', *, *, #24012, .F. ) ;
#4693 = CARTESIAN_POINT ( 'NONE',  ( 40.07437664823315515, 9.512804923423081149, 83.62581982957500770 ) ) ;
#4694 = CARTESIAN_POINT ( 'NONE',  ( -50.92620509423012720, -55.07344309828840068, 170.0000000000000000 ) ) ;
#4695 = CARTESIAN_POINT ( 'NONE',  ( 9.737557066527559257, 188.0000000000000000, 2.275957463600585040 ) ) ;
#4696 = VERTEX_POINT ( 'NONE', #32805 ) ;
#4697 = DIRECTION ( 'NONE',  ( -0.000000000000000000, -0.000000000000000000, -1.000000000000000000 ) ) ;
#4698 = DIRECTION ( 'NONE',  ( -0.000000000000000000, -0.000000000000000000, -1.000000000000000000 ) ) ;
#4699 = CIRCLE ( 'NONE', #30626, 25.00000000000000000 ) ;
#4700 = CARTESIAN_POINT ( 'NONE',  ( -7.336630171688589996, 7.867399454768227329, 3.271030448983515804 ) ) ;
#4701 = EDGE_CURVE ( 'NONE', #37117, #10376, #11608, .T. ) ;
#4703 = EDGE_CURVE ( 'NONE', #59711, #8166, #66737, .T. ) ;
#4702 = CARTESIAN_POINT ( 'NONE',  ( 176.6156959113760365, 75.60152827082541194, -37.68265618882365686 ) ) ;
#4704 = EDGE_CURVE ( 'NONE', #10742, #21319, #42324, .T. ) ;
#4705 = CARTESIAN_POINT ( 'NONE',  ( 164.9484057732149438, 63.70705320020925200, 91.28889419560704255 ) ) ;
#4706 = DIRECTION ( 'NONE',  ( 0.000000000000000000, -1.000000000000000000, 1.479221584281239571E-31 ) ) ;
#4707 = ADVANCED_FACE ( 'NONE', ( #10643 ), #441, .F. ) ;
#4708 = ORIENTED_EDGE ( 'NONE', *, *, #14752, .F. ) ;
#4709 = CARTESIAN_POINT ( 'NONE',  ( 0.4973051450695264442, -3.866309095700703136, 8.000000000000000000 ) ) ;
#4710 = DIRECTION ( 'NONE',  ( -0.000000000000000000, -0.000000000000000000, -1.000000000000000000 ) ) ;
#4711 = CARTESIAN_POINT ( 'NONE',  ( 8.337549025192453556, 7.382630697225778249, 36.52698723587364071 ) ) ;
#4712 = CARTESIAN_POINT ( 'NONE',  ( 197.9868529032975744, 99.18611233336802968, 33.34703807473912462 ) ) ;
#4713 = CARTESIAN_POINT ( 'NONE',  ( -86.07103743106915772, 26.37291038375863650, 92.84346461836889830 ) ) ;
#4715 = ORIENTED_EDGE ( 'NONE', *, *, #59441, .F. ) ;
#4714 = CARTESIAN_POINT ( 'NONE',  ( 74.39890044415652426, -7.951074708186050444, 170.0000000000000000 ) ) ;
#4716 = ORIENTED_EDGE ( 'NONE', *, *, #57128, .F. ) ;
#4717 = ORIENTED_EDGE ( 'NONE', *, *, #37321, .T. ) ;
#4718 = CARTESIAN_POINT ( 'NONE',  ( -55.05276343752910151, -170.0000000000000000, -42.71632399845987749 ) ) ;
#4719 = CARTESIAN_POINT ( 'NONE',  ( 197.2200752504830916, 96.62072041958360558, -70.00624559352947074 ) ) ;
#4720 = CARTESIAN_POINT ( 'NONE',  ( -33.12994257348895388, 10.89587983539684046, 57.24998983726293034 ) ) ;
#4721 = CARTESIAN_POINT ( 'NONE',  ( 110.2429982417149574, -170.0000000000000000, 71.45576479620103783 ) ) ;
#4722 = CARTESIAN_POINT ( 'NONE',  ( 155.7262569076171701, 56.30477153194512852, -63.11863533963168749 ) ) ;
#4723 = FACE_OUTER_BOUND ( 'NONE', #69286, .T. ) ;
#4724 = CARTESIAN_POINT ( 'NONE',  ( -156.0171627975468027, 69.90368824761765154, -38.57899779329219569 ) ) ;
#4725 = ORIENTED_EDGE ( 'NONE', *, *, #60038, .T. ) ;
#4726 = ORIENTED_EDGE ( 'NONE', *, *, #60338, .T. ) ;
#4727 = B_SPLINE_CURVE_WITH_KNOTS ( 'NONE', 3,
 ( #56541, #40020, #34417, #7327, #18566, #39673, #51619, #30169, #18223, #55863, #29465, #3428, #13303, #67459, #24204, #34757, #46325, #13632, #61130, #56194, #8010, #24891, #23854, #29124, #45292, #56901, #3092, #12956, #67801, #39332, #8369, #7678, #50924, #29816, #51279, #8719, #40704, #60774, #18918, #12599, #34055, #67128, #50574, #2394 ),
 .UNSPECIFIED., .F., .F.,
 ( 4, 2, 2, 2, 2, 2, 2, 2, 2, 2, 2, 2, 2, 2, 2, 2, 2, 2, 2, 2, 2, 4 ),
 ( 1.387778780781445676E-17, 0.004120577325733522020, 0.006180865988600256142, 0.008241154651466991998, 0.01030144331433372612, 0.01133158764576704981, 0.01236173197720037524, 0.01339187630863369893, 0.01442202064006702263, 0.01545216497150034632, 0.01648230930293367175, 0.01699738146865035354, 0.01751245363436703534, 0.01854259796580040934, 0.01957274229723378334, 0.02060288662866715387, 0.02266317529153390881, 0.02472346395440066374, 0.02678375261726741868, 0.02781389694870082738, 0.02884404128013423607, 0.03296461860586797493 ),
 .UNSPECIFIED. ) ;
#4728 = CARTESIAN_POINT ( 'NONE',  ( 69.83260694998128315, 15.39825517924928988, -13.23929702939983954 ) ) ;
#4729 = PLANE ( 'NONE',  #13598 ) ;
#4730 = CARTESIAN_POINT ( 'NONE',  ( 104.0290905220488469, 26.11184870228230892, 94.99999999999866418 ) ) ;
#4731 = CARTESIAN_POINT ( 'NONE',  ( 117.4711568421290053, 33.49899443629671936, -14.51207208499641332 ) ) ;
#4732 = CIRCLE ( 'NONE', #44038, 4.999999999999997335 ) ;
#4733 = CARTESIAN_POINT ( 'NONE',  ( -68.06184294702747195, 31.38946074233368222, 41.38025477438755928 ) ) ;
#4734 = CARTESIAN_POINT ( 'NONE',  ( 21.25987915030395925, 6.737472588634914494, 32.37940707539839735 ) ) ;
#4735 = CARTESIAN_POINT ( 'NONE',  ( 134.3182571105339491, 42.88121222759021833, -9.178760341931971212 ) ) ;
#4736 = EDGE_LOOP ( 'NONE', ( #52229, #39664, #60234, #6306 ) ) ;
#4737 = EDGE_LOOP ( 'NONE', ( #2724, #13378, #43528, #13191 ) ) ;
#4738 = VERTEX_POINT ( 'NONE', #6056 ) ;
#4739 = AXIS2_PLACEMENT_3D ( 'NONE', #280, #64310, #58676 ) ;
#4740 = EDGE_CURVE ( 'NONE', #60572, #16162, #27167, .T. ) ;
#4741 = CARTESIAN_POINT ( 'NONE',  ( -63.73419499958998813, 12.83646726144838013, 41.38025477438755928 ) ) ;
#4742 = CARTESIAN_POINT ( 'NONE',  ( 36.99999522780156269, 9.122638774496635961, -50.22900309971504385 ) ) ;
#4743 = DIRECTION ( 'NONE',  ( 0.000000000000000000, -1.000000000000000000, 0.000000000000000000 ) ) ;
#4744 = AXIS2_PLACEMENT_3D ( 'NONE', #11177, #37921, #48791 ) ;
#4745 = DIRECTION ( 'NONE',  ( -0.000000000000000000, -0.000000000000000000, -1.000000000000000000 ) ) ;
#4746 = CARTESIAN_POINT ( 'NONE',  ( 197.2199163281728147, 98.22431253015354002, 62.88886963507403749 ) ) ;
#4747 = B_SPLINE_CURVE_WITH_KNOTS ( 'NONE', 3,
 ( #57970, #62906, #20678, #3136, #67496, #35482, #56943, #8763, #30212, #4165, #24931, #62565, #14377, #51663, #46365, #35832, #30547, #51998, #25631, #47065, #69543, #38586, #27676, #64979 ),
 .UNSPECIFIED., .F., .F.,
 ( 4, 2, 2, 2, 2, 2, 2, 2, 2, 2, 2, 4 ),
 ( 0.01050068220271658387, 0.01181995631628032263, 0.01247959337306220329, 0.01313923042984408221, 0.01445850454340786087, 0.01511814160018975020, 0.01577777865697164300, 0.01709705277053541819, 0.01775668982731730752, 0.01841632688409919338, 0.01973560099766296164, 0.02105487511122672642 ),
 .UNSPECIFIED. ) ;
#4748 = ORIENTED_EDGE ( 'NONE', *, *, #50280, .T. ) ;
#4749 = CARTESIAN_POINT ( 'NONE',  ( 36.99625334683020839, 8.108440754877200618, 57.13776175391618750 ) ) ;
#4750 = CARTESIAN_POINT ( 'NONE',  ( 14.08699529666005823, 6.452200550165255954, -8.865815044285954016 ) ) ;
#4751 =( NAMED_UNIT ( * ) PLANE_ANGLE_UNIT ( ) SI_UNIT ( $, .RADIAN. ) );
#4752 = CARTESIAN_POINT ( 'NONE',  ( 20.74185656603722450, 7.717159106492280429, 5.017094231853548081 ) ) ;
#4753 = CARTESIAN_POINT ( 'NONE',  ( 188.0081045302011091, 85.89855126821611009, 60.75689848136790516 ) ) ;
#4754 = PLANE ( 'NONE',  #29745 ) ;
#4755 = CARTESIAN_POINT ( 'NONE',  ( -79.61931371420119774, 22.68640080971621487, -35.16116692163456037 ) ) ;
#4756 = CARTESIAN_POINT ( 'NONE',  ( 63.72039997003725631, -12.83396383267754537, 40.00000000000003553 ) ) ;
#4757 = EDGE_CURVE ( 'NONE', #38637, #41110, #62186, .T. ) ;
#4758 = DIRECTION ( 'NONE',  ( 0.9510565162951500895, 0.3090169943749583314, 2.500042656554809847E-16 ) ) ;
#4759 = DIRECTION ( 'NONE',  ( -1.000000000000000000, 0.000000000000000000, 0.000000000000000000 ) ) ;
#4760 = EDGE_CURVE ( 'NONE', #56686, #52761, #69269, .T. ) ;
#4761 = EDGE_CURVE ( 'NONE', #28769, #14491, #60577, .T. ) ;
#4762 = ORIENTED_EDGE ( 'NONE', *, *, #33113, .F. ) ;
#4763 = CARTESIAN_POINT ( 'NONE',  ( 187.2465631085773339, 85.06582225041682932, 14.26867246100197661 ) ) ;
#4764 = APPLICATION_PROTOCOL_DEFINITION ( 'draft international standard', 'automotive_design', 1998, #66008 ) ;
#4765 = CARTESIAN_POINT ( 'NONE',  ( 31.11269837220809364, 20.55634918610396866, 0.000000000000000000 ) ) ;
#4766 = FACE_OUTER_BOUND ( 'NONE', #24856, .T. ) ;
#4767 = CARTESIAN_POINT ( 'NONE',  ( -107.7886332494339570, 36.81249801143973599, -37.40149486631479192 ) ) ;
#4768 = DIRECTION ( 'NONE',  ( 1.000000000000000000, 0.000000000000000000, 1.734723475976805517E-15 ) ) ;
#4769 = EDGE_LOOP ( 'NONE', ( #6850, #46312, #5479, #66133 ) ) ;
#4770 = EDGE_LOOP ( 'NONE', ( #62843, #29806, #13390, #1354 ) ) ;
#4771 = CARTESIAN_POINT ( 'NONE',  ( 0.000000000000000000, 0.000000000000000000, -10.00000000000000000 ) ) ;
#4772 = CARTESIAN_POINT ( 'NONE',  ( 173.9662866282169205, 71.69964987613715834, 88.12574805637403585 ) ) ;
#4773 = ORIENTED_EDGE ( 'NONE', *, *, #26684, .T. ) ;
#4774 = CARTESIAN_POINT ( 'NONE',  ( 117.6916924104495479, 32.48309187151379973, 64.97158662374468463 ) ) ;
#4775 = VERTEX_POINT ( 'NONE', #2536 ) ;
#4776 = DIRECTION ( 'NONE',  ( -2.616877698022195692E-18, -4.379915515250404077E-18, -1.000000000000000000 ) ) ;
#4777 = FACE_BOUND ( 'NONE', #67741, .T. ) ;
#4778 = CARTESIAN_POINT ( 'NONE',  ( 31.11269837220803325, -15.55634918610409656, 2.000000000000001776 ) ) ;
#4779 = VECTOR ( 'NONE', #45800, 1000.000000000000000 ) ;
#4780 = ADVANCED_FACE ( 'NONE', ( #33159 ), #1143, .T. ) ;
#4781 = CARTESIAN_POINT ( 'NONE',  ( -99.10260179032844974, 31.19580119595418211, 44.81688323301395371 ) ) ;
#4782 = CARTESIAN_POINT ( 'NONE',  ( 0.000000000000000000, 0.000000000000000000, 2.500000000000030198 ) ) ;
#4783 = CIRCLE ( 'NONE', #63194, 65.36598343705435354 ) ;
#4785 = EDGE_LOOP ( 'NONE', ( #23234, #53980 ) ) ;
#4784 = DIRECTION ( 'NONE',  ( 8.673617379884039170E-17, 1.033681467326434846E-16, 1.000000000000000000 ) ) ;
#4786 = EDGE_CURVE ( 'NONE', #50015, #60490, #1385, .T. ) ;
#4787 = DIRECTION ( 'NONE',  ( -0.000000000000000000, -0.000000000000000000, -1.000000000000000000 ) ) ;
#4788 = ORIENTED_EDGE ( 'NONE', *, *, #53257, .F. ) ;
#4789 = AXIS2_PLACEMENT_3D ( 'NONE', #65321, #38580, #60026 ) ;
#4790 = ORIENTED_EDGE ( 'NONE', *, *, #32185, .T. ) ;
#4791 = CARTESIAN_POINT ( 'NONE',  ( -118.8504142000305563, 42.02789424825281372, -12.97858553378794610 ) ) ;
#4792 = AXIS2_PLACEMENT_3D ( 'NONE', #12377, #6038, #23634 ) ;
#4793 = LINE ( 'NONE', #26258, #10044 ) ;
#4794 = DIRECTION ( 'NONE',  ( 0.000000000000000000, 0.000000000000000000, -1.000000000000000000 ) ) ;
#4795 = CARTESIAN_POINT ( 'NONE',  ( 42.02161712141799654, -16.09918303830818687, 30.00000000000000000 ) ) ;
#4797 = ORIENTED_EDGE ( 'NONE', *, *, #48258, .F. ) ;
#4796 = CARTESIAN_POINT ( 'NONE',  ( -7.825402957745087207, 6.891034867348158954, 45.11558103944722120 ) ) ;
#4798 = CARTESIAN_POINT ( 'NONE',  ( -103.8075682002152007, 34.69679037577547831, 84.35934033286845590 ) ) ;
#4799 = VECTOR ( 'NONE', #923, 1000.000000000000000 ) ;
#4800 = EDGE_LOOP ( 'NONE', ( #6610, #17998, #29657, #19956 ) ) ;
#4801 = CARTESIAN_POINT ( 'NONE',  ( -55.05276343752909440, 14.68156374112637330, -8.371773407996169425 ) ) ;
#4802 = CARTESIAN_POINT ( 'NONE',  ( -133.1566699306513328, 52.70203339370771545, -71.14848980824044133 ) ) ;
#4803 = CARTESIAN_POINT ( 'NONE',  ( 311.9975424824652350, 0.000000000000000000, 254.5114349394235091 ) ) ;
#4804 = CARTESIAN_POINT ( 'NONE',  ( -100.4466073551323007, 31.85873123265078277, 3.887263631221759663 ) ) ;
#4805 = LINE ( 'NONE', #59305, #49723 ) ;
#4806 = ORIENTED_EDGE ( 'NONE', *, *, #27448, .F. ) ;
#4807 = ORIENTED_EDGE ( 'NONE', *, *, #63113, .T. ) ;
#4808 = DIRECTION ( 'NONE',  ( -1.000000000000000000, 0.000000000000000000, 0.000000000000000000 ) ) ;
#4809 = CARTESIAN_POINT ( 'NONE',  ( -170.2747214445849693, 84.01465441107040988, -35.26017206050354247 ) ) ;
#4810 = DIRECTION ( 'NONE',  ( 0.000000000000000000, 0.000000000000000000, 1.000000000000000000 ) ) ;
#4811 = LINE ( 'NONE', #15720, #2982 ) ;
#4812 = CARTESIAN_POINT ( 'NONE',  ( -76.33235143960695268, 22.51916353135074900, 45.04974780934608702 ) ) ;
#4813 = CARTESIAN_POINT ( 'NONE',  ( 80.73012746365749592, 17.49169339352364716, 41.86980492191601400 ) ) ;
#4814 = CARTESIAN_POINT ( 'NONE',  ( 70.11969827741708627, 15.47408882293423993, -40.76595231452924395 ) ) ;
#4815 = CARTESIAN_POINT ( 'NONE',  ( 42.48820792780864508, 9.847387255477766388, -49.95978026808956685 ) ) ;
#4816 = CARTESIAN_POINT ( 'NONE',  ( 206.7099580236350107, 109.1417833474364443, 70.78891289186701385 ) ) ;
#4818 = ORIENTED_EDGE ( 'NONE', *, *, #27003, .F. ) ;
#4817 = EDGE_CURVE ( 'NONE', #23974, #44398, #13439, .T. ) ;
#4819 = CARTESIAN_POINT ( 'NONE',  ( -36.11269837220801548, 36.11269837220812207, 0.000000000000000000 ) ) ;
#4820 = EDGE_LOOP ( 'NONE', ( #62298, #10740, #2877, #36069, #7715, #7144, #60896, #28446, #21234 ) ) ;
#4821 = CARTESIAN_POINT ( 'NONE',  ( -15.22871623201694469, 7.486724405784662473, -44.14333518623142538 ) ) ;
#4822 = EDGE_CURVE ( 'NONE', #52905, #31875, #62567, .T. ) ;
#4823 = AXIS2_PLACEMENT_3D ( 'NONE', #600, #43844, #5866 ) ;
#4824 = CARTESIAN_POINT ( 'NONE',  ( 14.66690460840507804, -20.39656099473392814, 0.000000000000000000 ) ) ;
#4825 = CARTESIAN_POINT ( 'NONE',  ( 94.11733320392093560, 23.18939451097131155, 63.56296009108370981 ) ) ;
#4826 = CARTESIAN_POINT ( 'NONE',  ( 153.2384531768735769, 54.43344429203622781, -10.57026377980718657 ) ) ;
#4827 = CARTESIAN_POINT ( 'NONE',  ( 0.000000000000000000, 6.928203230275505220, -4.000000000000007994 ) ) ;
#4828 = DIRECTION ( 'NONE',  ( 4.974206872490772509E-18, 1.135330258912677140E-18, -1.000000000000000000 ) ) ;
#4829 = CARTESIAN_POINT ( 'NONE',  ( 36.76746179515744473, 8.081433644308901876, -62.93801830221686089 ) ) ;
#4830 = CARTESIAN_POINT ( 'NONE',  ( -99.10674985723794350, 32.31836975419496838, -76.17106620709191134 ) ) ;
#4831 = VECTOR ( 'NONE', #25004, 1000.000000000000000 ) ;
#4832 = CARTESIAN_POINT ( 'NONE',  ( -36.37229078872273647, 11.47648211215765812, -21.64289120047060067 ) ) ;
#4833 = ORIENTED_EDGE ( 'NONE', *, *, #30042, .F. ) ;
#4834 = VECTOR ( 'NONE', #51632, 1000.000000000000000 ) ;
#4835 = DIRECTION ( 'NONE',  ( 0.1342332658176667304, -0.9909497617679331460, 0.000000000000000000 ) ) ;
#4836 = EDGE_LOOP ( 'NONE', ( #31185, #40353, #53092, #63097 ) ) ;
#4837 = CARTESIAN_POINT ( 'NONE',  ( 0.2033771190674383833, 0.000000000000000000, 4.235016458833691821 ) ) ;
#4838 = FILL_AREA_STYLE_COLOUR ( '', #64366 ) ;
#4839 = CARTESIAN_POINT ( 'NONE',  ( -24.18258876560172155, 8.512344710720682883, 8.913579529955121927 ) ) ;
#4840 = DIRECTION ( 'NONE',  ( 1.000000000000000000, 0.000000000000000000, 0.000000000000000000 ) ) ;
#4841 = EDGE_CURVE ( 'NONE', #8386, #11991, #57577, .T. ) ;
#4842 = CARTESIAN_POINT ( 'NONE',  ( -5.416136198635861376, 6.745992685878681172, 30.50884761992566752 ) ) ;
#4843 = FACE_OUTER_BOUND ( 'NONE', #65401, .T. ) ;
#4844 = CARTESIAN_POINT ( 'NONE',  ( 156.3797504404255392, 58.07856685387020690, -51.04775918292205716 ) ) ;
#4845 = CIRCLE ( 'NONE', #31809, 74.95140232871122521 ) ;
#4846 = EDGE_CURVE ( 'NONE', #5410, #10221, #63300, .T. ) ;
#4847 = ADVANCED_FACE ( 'NONE', ( #5297 ), #68957, .T. ) ;
#4848 = VERTEX_POINT ( 'NONE', #21141 ) ;
#4850 = VECTOR ( 'NONE', #46965, 1000.000000000000000 ) ;
#4849 = DIRECTION ( 'NONE',  ( -0.4127148655274867073, 0.9108602745606092510, 7.570395943812493020E-15 ) ) ;
#4851 = CARTESIAN_POINT ( 'NONE',  ( -189.9638655956220532, 108.0957249433520815, -18.49776328886134280 ) ) ;
#4852 = CARTESIAN_POINT ( 'NONE',  ( 173.5836858989432017, 72.71885240881779566, -16.59373086107160944 ) ) ;
#4853 = CARTESIAN_POINT ( 'NONE',  ( -107.2385267828037030, 36.51474259889401708, 59.23132442209924164 ) ) ;
#4854 = CONTEXT_DEPENDENT_SHAPE_REPRESENTATION ( #66514, #41229 ) ;
#4855 = DIRECTION ( 'NONE',  ( 0.000000000000000000, 0.000000000000000000, 1.000000000000000000 ) ) ;
#4856 = VERTEX_POINT ( 'NONE', #37997 ) ;
#4857 = LINE ( 'NONE', #42492, #4331 ) ;
#4858 = CARTESIAN_POINT ( 'NONE',  ( 88.99522780200244654, 20.24180937454204354, 71.17773731472695431 ) ) ;
#4859 = CARTESIAN_POINT ( 'NONE',  ( 204.3091227790962421, 107.5190503136782354, -9.481380442157895772 ) ) ;
#4860 = CARTESIAN_POINT ( 'NONE',  ( -142.7660513839927034, 58.66578555228782221, 88.60591720006654270 ) ) ;
#4861 = CARTESIAN_POINT ( 'NONE',  ( 139.6203063421347110, 45.01495791936839908, 32.18546459676473148 ) ) ;
#4862 = ORIENTED_EDGE ( 'NONE', *, *, #45702, .F. ) ;
#4863 = LINE ( 'NONE', #16793, #36809 ) ;
#4864 = CARTESIAN_POINT ( 'NONE',  ( 82.95856197793166587, 19.25847567427442542, 3.809032710648850184 ) ) ;
#4865 = CARTESIAN_POINT ( 'NONE',  ( 161.1112535418156710, 61.83422628788727593, 16.62590986968896090 ) ) ;
#4866 = DIRECTION ( 'NONE',  ( -0.3090169943749447312, -0.9510565162951544194, 0.000000000000000000 ) ) ;
#4867 = VERTEX_POINT ( 'NONE', #37293 ) ;
#4868 = ADVANCED_FACE ( 'NONE', ( #22170 ), #20779, .T. ) ;
#4869 = CARTESIAN_POINT ( 'NONE',  ( 178.1965488566139868, 77.14488558164480025, 56.71789026606290918 ) ) ;
#4870 = VERTEX_POINT ( 'NONE', #26755 ) ;
#4871 = CARTESIAN_POINT ( 'NONE',  ( -108.9136445001389859, 36.28030794288191174, -39.00605114454056377 ) ) ;
#4872 = FACE_OUTER_BOUND ( 'NONE', #46601, .T. ) ;
#4873 = AXIS2_PLACEMENT_3D ( 'NONE', #1842, #50708, #55633 ) ;
#4874 = DIRECTION ( 'NONE',  ( 0.000000000000000000, -1.000000000000000000, 0.000000000000000000 ) ) ;
#4875 = AXIS2_PLACEMENT_3D ( 'NONE', #67150, #56217, #8033 ) ;
#4877 = ORIENTED_EDGE ( 'NONE', *, *, #51267, .T. ) ;
#4876 = CARTESIAN_POINT ( 'NONE',  ( 150.9013375937531407, 53.96275732797613500, 13.69346484706898437 ) ) ;
#4878 = FACE_OUTER_BOUND ( 'NONE', #57232, .T. ) ;
#4879 = FACE_OUTER_BOUND ( 'NONE', #7002, .T. ) ;
#4880 = CARTESIAN_POINT ( 'NONE',  ( -39.29440389294403246, -17.09499999999999886, 4.000000000000000000 ) ) ;
#4881 = VECTOR ( 'NONE', #9082, 1000.000000000000114 ) ;
#4882 = ORIENTED_EDGE ( 'NONE', *, *, #49397, .T. ) ;
#4883 = CARTESIAN_POINT ( 'NONE',  ( -102.2801239173131052, 33.91021738430207222, 3.674523915951417585 ) ) ;
#4884 = VECTOR ( 'NONE', #12771, 999.9999999999998863 ) ;
#4885 = CIRCLE ( 'NONE', #59958, 500.0000000000000000 ) ;
#4886 = CARTESIAN_POINT ( 'NONE',  ( 140.8984307802396359, 45.84194788389002895, 61.22238341269675743 ) ) ;
#4887 = CARTESIAN_POINT ( 'NONE',  ( -176.3763474213711504, 92.36993073950279154, 31.55091585264105447 ) ) ;
#4888 = VECTOR ( 'NONE', #64816, 1000.000000000000000 ) ;
#4889 = CARTESIAN_POINT ( 'NONE',  ( -35.17600017528511813, 10.23461991275926763, -76.16909263517460715 ) ) ;
#4890 = CARTESIAN_POINT ( 'NONE',  ( 88.53025347111697840, 21.14438024052372711, 29.94122557606181800 ) ) ;
#4891 = VERTEX_POINT ( 'NONE', #9893 ) ;
#4892 = CARTESIAN_POINT ( 'NONE',  ( 46.12611922993085045, 10.39838587005582049, 7.238115754011925418 ) ) ;
#4893 = VERTEX_POINT ( 'NONE', #58403 ) ;
#4894 = ORIENTED_EDGE ( 'NONE', *, *, #26906, .F. ) ;
#4895 = VECTOR ( 'NONE', #6302, 1000.000000000000000 ) ;
#4896 = CARTESIAN_POINT ( 'NONE',  ( 36.64089410029568228, 65.45232906116417837, 43.58025477438756212 ) ) ;
#4897 = EDGE_CURVE ( 'NONE', #66948, #13402, #48184, .T. ) ;
#4898 = CARTESIAN_POINT ( 'NONE',  ( 212.1669304543881651, 119.0398299474538959, -17.68208531959118091 ) ) ;
#4899 = DIRECTION ( 'NONE',  ( 0.01527021686369653929, 0.000000000000000000, 0.9998834034410890581 ) ) ;
#4900 = CARTESIAN_POINT ( 'NONE',  ( -152.9119739516381173, 67.12135129037710612, -75.85561049297035652 ) ) ;
#4901 = DIRECTION ( 'NONE',  ( 0.6427876096865403621, -0.7660444431189770143, 1.393823445737823288E-16 ) ) ;
#4902 = CARTESIAN_POINT ( 'NONE',  ( -51.82969867401513397, 54.20961478705410030, 43.58025477438756212 ) ) ;
#4903 = CARTESIAN_POINT ( 'NONE',  ( 204.6977192012829789, 106.3443248447423315, -36.32593103262158252 ) ) ;
#4904 = EDGE_CURVE ( 'NONE', #26503, #8633, #55459, .T. ) ;
#4905 = CARTESIAN_POINT ( 'NONE',  ( 63.00000000000000000, 7.715274834628325378E-15, 170.0000000000000000 ) ) ;
#4906 = ORIENTED_EDGE ( 'NONE', *, *, #35345, .F. ) ;
#4907 = CYLINDRICAL_SURFACE ( 'NONE', #36334, 7.500000000000020428 ) ;
#4909 = EDGE_LOOP ( 'NONE', ( #310, #34298, #9189, #55164 ) ) ;
#4908 = EDGE_CURVE ( 'NONE', #37858, #36451, #7392, .T. ) ;
#4910 = CARTESIAN_POINT ( 'NONE',  ( -71.57025115638938928, 20.80908992785612099, 62.28357928173872438 ) ) ;
#4911 = CARTESIAN_POINT ( 'NONE',  ( 207.4696221732442609, 110.2206209205161969, -77.65139825956335073 ) ) ;
#4912 = CARTESIAN_POINT ( 'NONE',  ( 56.30011474572736319, 11.21470186335419683, -73.41388707145787862 ) ) ;
#4913 = CARTESIAN_POINT ( 'NONE',  ( -121.2119672714299270, 44.67540322905997385, 70.84369768003189449 ) ) ;
#4914 = EDGE_CURVE ( 'NONE', #2403, #18591, #2646, .T. ) ;
#4915 = PLANE ( 'NONE',  #62582 ) ;
#4916 = DIRECTION ( 'NONE',  ( -1.000000000000000000, 0.000000000000000000, 0.000000000000000000 ) ) ;
#4917 = EDGE_LOOP ( 'NONE', ( #61243, #18481, #55829, #16565 ) ) ;
#4918 = CARTESIAN_POINT ( 'NONE',  ( -71.37402418445425667, 19.67651958824263758, 62.99220628321225490 ) ) ;
#4919 = CARTESIAN_POINT ( 'NONE',  ( -173.1211646369891355, 87.12891641440857882, 72.66624519710475738 ) ) ;
#4920 = ORIENTED_EDGE ( 'NONE', *, *, #2190, .T. ) ;
#4921 = ORIENTED_EDGE ( 'NONE', *, *, #14230, .T. ) ;
#4922 = CARTESIAN_POINT ( 'NONE',  ( 0.000000000000000000, 0.000000000000000000, 0.000000000000000000 ) ) ;
#4923 = CARTESIAN_POINT ( 'NONE',  ( 55.51547041749725508, 11.05727559334826893, -43.46285331346358305 ) ) ;
#4924 = FACE_OUTER_BOUND ( 'NONE', #68709, .T. ) ;
#4925 = DIRECTION ( 'NONE',  ( 1.000000000000000000, 0.000000000000000000, 0.000000000000000000 ) ) ;
#4926 = AXIS2_PLACEMENT_3D ( 'NONE', #54248, #48974, #54958 ) ;
#4927 = DIRECTION ( 'NONE',  ( -0.000000000000000000, -0.000000000000000000, -1.000000000000000000 ) ) ;
#4928 = EDGE_CURVE ( 'NONE', #9934, #23357, #60498, .T. ) ;
#4929 = ORIENTED_EDGE ( 'NONE', *, *, #43895, .F. ) ;
#4930 = CIRCLE ( 'NONE', #44230, 10.00000000000000000 ) ;
#4931 = EDGE_LOOP ( 'NONE', ( #41920, #43256, #8121, #49854, #5742, #37890, #29263, #26525, #1154 ) ) ;
#4932 = CARTESIAN_POINT ( 'NONE',  ( -128.1282195935087600, 49.19720162550165554, 30.95687802063085670 ) ) ;
#4933 = ORIENTED_EDGE ( 'NONE', *, *, #26432, .T. ) ;
#4934 = CARTESIAN_POINT ( 'NONE',  ( -44.99999999999998579, 25.00000000000000000, 1.999999999999984457 ) ) ;
#4935 = CARTESIAN_POINT ( 'NONE',  ( 0.01678220608715907600, 0.7854258608507247441, -8.000000000000001776 ) ) ;
#4936 = CONICAL_SURFACE ( 'NONE', #1573, 74.95140232871122521, 0.8777644062502172329 ) ;
#4937 = CARTESIAN_POINT ( 'NONE',  ( 5.204170427930454100E-14, 6.000000000000000000, -30.00000000000021316 ) ) ;
#4938 = CARTESIAN_POINT ( 'NONE',  ( -12.77952633087691403, 21.62918162951106993, 0.000000000000000000 ) ) ;
#4939 = CIRCLE ( 'NONE', #12784, 65.36598343705435354 ) ;
#4940 = DIRECTION ( 'NONE',  ( -0.9639628606958550172, 0.2660368455666687892, 0.000000000000000000 ) ) ;
#4941 = AXIS2_PLACEMENT_3D ( 'NONE', #7124, #6773, #39149 ) ;
#4942 = DIRECTION ( 'NONE',  ( -0.000000000000000000, -0.000000000000000000, -1.000000000000000000 ) ) ;
#4943 = AXIS2_PLACEMENT_3D ( 'NONE', #56175, #41396, #7991 ) ;
#4944 = VERTEX_POINT ( 'NONE', #59784 ) ;
#4945 = ORIENTED_EDGE ( 'NONE', *, *, #30263, .T. ) ;
#4946 = CARTESIAN_POINT ( 'NONE',  ( -2.309976723937615439, 7.903938623646864059, -0.1306530452038096035 ) ) ;
#4947 = CARTESIAN_POINT ( 'NONE',  ( -2.000000000000000000, 192.0000000000000000, 0.000000000000000000 ) ) ;
#4948 = CIRCLE ( 'NONE', #10407, 10.00000000000000178 ) ;
#4949 = CARTESIAN_POINT ( 'NONE',  ( -169.1041038606267648, 82.76530082651285625, -21.71656691506287018 ) ) ;
#4950 = CARTESIAN_POINT ( 'NONE',  ( 0.000000000000000000, 190.0000000000000000, 380.0000000000000000 ) ) ;
#4951 = CARTESIAN_POINT ( 'NONE',  ( 64.93495251696903381, 13.12601614965099017, 30.05863598689030880 ) ) ;
#4952 = CARTESIAN_POINT ( 'NONE',  ( 49.76301652092226391, -41.81676920493045202, 40.00000000000003553 ) ) ;
#4953 = EDGE_LOOP ( 'NONE', ( #54643, #42832, #50469, #17326 ) ) ;
#4954 = CARTESIAN_POINT ( 'NONE',  ( -20.55634918610408945, -31.11269837220804035, 0.000000000000000000 ) ) ;
#4955 = FACE_OUTER_BOUND ( 'NONE', #64021, .T. ) ;
#4956 = ORIENTED_EDGE ( 'NONE', *, *, #22874, .T. ) ;
#4957 = CARTESIAN_POINT ( 'NONE',  ( -81.90266786693713641, 23.58030232261292980, 17.85658396585434105 ) ) ;
#4958 = ORIENTED_EDGE ( 'NONE', *, *, #24011, .F. ) ;
#4959 = VERTEX_POINT ( 'NONE', #27791 ) ;
#4960 = CARTESIAN_POINT ( 'NONE',  ( 8.336882341125877005, 6.376438415325265119, -44.00243688774482820 ) ) ;
#4961 = CARTESIAN_POINT ( 'NONE',  ( -180.4654253355436424, 95.69358270527506249, 63.61568511560930261 ) ) ;
#4962 = CARTESIAN_POINT ( 'NONE',  ( 127.1040286383415037, 37.49395136275125395, 60.58097942537040126 ) ) ;
#4963 = ORIENTED_EDGE ( 'NONE', *, *, #67890, .F. ) ;
#4964 = EDGE_CURVE ( 'NONE', #5356, #3417, #49229, .T. ) ;
#4965 = CARTESIAN_POINT ( 'NONE',  ( -36.19806511523993464, 10.42097839459253983, 85.59994145001356003 ) ) ;
#4966 = CARTESIAN_POINT ( 'NONE',  ( 157.4703587214989113, 57.65129005721575339, 44.40946747225338953 ) ) ;
#4967 = AXIS2_PLACEMENT_3D ( 'NONE', #36555, #36209, #9132 ) ;
#4968 = LINE ( 'NONE', #27107, #33681 ) ;
#4969 = CARTESIAN_POINT ( 'NONE',  ( 429.8372781065087338, 388.0000000000065938, 91.05029585798857283 ) ) ;
#4970 = CARTESIAN_POINT ( 'NONE',  ( 140.4641697461913452, 46.75994457266057225, -66.78132054738273382 ) ) ;
#4971 = CARTESIAN_POINT ( 'NONE',  ( 445.3372781065085633, 177.8591479523844612, -111.4497041420119388 ) ) ;
#4972 = ORIENTED_EDGE ( 'NONE', *, *, #28424, .T. ) ;
#4973 = AXIS2_PLACEMENT_3D ( 'NONE', #13671, #50611, #3131 ) ;
#4974 = CARTESIAN_POINT ( 'NONE',  ( 432.4999999999999432, 207.5000000000000284, 20.00000000000000000 ) ) ;
#4975 = CARTESIAN_POINT ( 'NONE',  ( 41.81982603358027006, 8.735900550613179050, 17.68552455925381039 ) ) ;
#4976 = CARTESIAN_POINT ( 'NONE',  ( 176.6156959113759513, 75.60152827082541194, 16.00644499210370597 ) ) ;
#4977 = CARTESIAN_POINT ( 'NONE',  ( -118.4470345550925856, 42.96051736048244152, -43.45603041284294932 ) ) ;
#4978 = CARTESIAN_POINT ( 'NONE',  ( -5.000000000000058620, -31.11269837220806878, 2.000000000000000000 ) ) ;
#4979 = DIRECTION ( 'NONE',  ( -0.8584487936018655452, -0.5128992774059070170, 0.000000000000000000 ) ) ;
#4980 = CIRCLE ( 'NONE', #462, 25.00000000000145306 ) ;
#4981 = CARTESIAN_POINT ( 'NONE',  ( 34.63049175740484742, 7.836802300168049129, -91.01871974183544012 ) ) ;
#4982 = CARTESIAN_POINT ( 'NONE',  ( -120.6739978760426055, 44.33795494230366074, -63.86731139866689944 ) ) ;
#4983 = VECTOR ( 'NONE', #548, 1000.000000000000000 ) ;
#4984 = EDGE_CURVE ( 'NONE', #12323, #24023, #34483, .T. ) ;
#4985 = CARTESIAN_POINT ( 'NONE',  ( 66.30567821786753768, 13.45988234822861251, 17.21265612671894019 ) ) ;
#4986 = CARTESIAN_POINT ( 'NONE',  ( -85.36298448216594181, 26.07611629625833416, 68.17787176330473642 ) ) ;
#4987 = CARTESIAN_POINT ( 'NONE',  ( 41.04421810250191527, 9.644095118781809362, -89.47936863587655409 ) ) ;
#4988 = EDGE_LOOP ( 'NONE', ( #67374, #3849, #16908, #44677, #2325, #29922, #50568 ) ) ;
#4990 = AXIS2_PLACEMENT_3D ( 'NONE', #28858, #13370, #13032 ) ;
#4989 = CONTEXT_DEPENDENT_SHAPE_REPRESENTATION ( #53425, #19306 ) ;
#4991 = CARTESIAN_POINT ( 'NONE',  ( -7.306921717852591591, 37.63116478967256739, 13.32819397642332504 ) ) ;
#4992 = ORIENTED_EDGE ( 'NONE', *, *, #9172, .T. ) ;
#4993 = DIRECTION ( 'NONE',  ( 0.000000000000000000, -0.04541273895899431562, 0.9989683093773507050 ) ) ;
#4994 = VERTEX_POINT ( 'NONE', #18285 ) ;
#4995 = PLANE ( 'NONE',  #37706 ) ;
#4996 = DIRECTION ( 'NONE',  ( 0.000000000000000000, 0.000000000000000000, 1.000000000000000000 ) ) ;
#4997 = CARTESIAN_POINT ( 'NONE',  ( -148.6471085600700519, 64.76880961642444845, 57.60225718838557896 ) ) ;
#4998 = EDGE_CURVE ( 'NONE', #1313, #29309, #26242, .T. ) ;
#4999 = CARTESIAN_POINT ( 'NONE',  ( 70.11438327604406595, 14.43198353181102433, -13.94311793805158040 ) ) ;
#5000 = CARTESIAN_POINT ( 'NONE',  ( 135.6647932137618113, 43.70902528961477174, -36.23038487884888781 ) ) ;
#5001 = CARTESIAN_POINT ( 'NONE',  ( -48.58011387679029269, 14.07568064779664851, -73.35782377364151330 ) ) ;
#5002 = CARTESIAN_POINT ( 'NONE',  ( -31.43908319763710679, -170.0000000000000000, -77.16174795566554678 ) ) ;
#5003 = DIRECTION ( 'NONE',  ( 0.7693125429406515448, 0.000000000000000000, 0.6388726095820577155 ) ) ;
#5004 = ORIENTED_EDGE ( 'NONE', *, *, #35996, .T. ) ;
#5005 = ORIENTED_EDGE ( 'NONE', *, *, #30906, .T. ) ;
#5006 = CARTESIAN_POINT ( 'NONE',  ( 183.4883381146856891, 82.52303242823217033, 83.37056451303936910 ) ) ;
#5007 = SURFACE_STYLE_USAGE ( .BOTH. , #65054 ) ;
#5008 = CARTESIAN_POINT ( 'NONE',  ( -171.4943428135323416, 86.82484920477511992, -7.997380618965306276 ) ) ;
#5009 = EDGE_CURVE ( 'NONE', #33759, #34668, #37367, .T. ) ;
#5010 = PRODUCT_DEFINITION_CONTEXT ( 'detailed design', #48477, 'design' ) ;
#5011 = CARTESIAN_POINT ( 'NONE',  ( 0.000000000000000000, 0.000000000000000000, -10.00000000000000000 ) ) ;
#5012 = CARTESIAN_POINT ( 'NONE',  ( 281.6210066600216919, 21.48343462569976836, 4.741142292097720201 ) ) ;
#5013 = CARTESIAN_POINT ( 'NONE',  ( -9.763294602873866523, 7.024900256480053784, 71.70961793505638582 ) ) ;
#5014 = CARTESIAN_POINT ( 'NONE',  ( -80.31691774066408129, 22.95709084517030618, -8.450926537141361550 ) ) ;
#5015 = CARTESIAN_POINT ( 'NONE',  ( -86.05211524933166345, 26.36495896184001708, -95.00000000000133582 ) ) ;
#5016 = CARTESIAN_POINT ( 'NONE',  ( 41.80536115778106421, 8.734184316430665618, -23.38395991615332647 ) ) ;
#5017 = CARTESIAN_POINT ( 'NONE',  ( -78.66644367742111399, -170.0000000000000000, 11.07365054920946079 ) ) ;
#5018 = FACE_OUTER_BOUND ( 'NONE', #39727, .T. ) ;
#5019 = CARTESIAN_POINT ( 'NONE',  ( 162.6205203824432317, 63.07332653227192054, 69.21143974246140829 ) ) ;
#5020 = VECTOR ( 'NONE', #68078, 1000.000000000000000 ) ;
#5021 = EDGE_LOOP ( 'NONE', ( #61322, #21114 ) ) ;
#5022 = CARTESIAN_POINT ( 'NONE',  ( -125.4433371161043311, 46.19736518073186460, -34.91370389823390497 ) ) ;
#5023 = CARTESIAN_POINT ( 'NONE',  ( -439.4229916354183842, 388.0000000000064801, -128.9497041420121093 ) ) ;
#5024 = FACE_OUTER_BOUND ( 'NONE', #51493, .T. ) ;
#5025 = DIRECTION ( 'NONE',  ( 0.000000000000000000, 0.000000000000000000, 1.000000000000000000 ) ) ;
#5026 = CARTESIAN_POINT ( 'NONE',  ( 150.0973882686025149, 52.13852366454154463, 11.46627940338942153 ) ) ;
#5027 = CARTESIAN_POINT ( 'NONE',  ( -11.83735969105690167, 8.195029568776297069, 84.95963025573755090 ) ) ;
#5028 = VECTOR ( 'NONE', #63305, 1000.000000000000000 ) ;
#5029 = VECTOR ( 'NONE', #25803, 1000.000000000000000 ) ;
#5030 = VERTEX_POINT ( 'NONE', #43954 ) ;
#5031 = AXIS2_PLACEMENT_3D ( 'NONE', #48409, #43149, #64619 ) ;
#5032 = DIRECTION ( 'NONE',  ( -0.000000000000000000, 0.000000000000000000, -1.000000000000000000 ) ) ;
#5033 = AXIS2_PLACEMENT_3D ( 'NONE', #67529, #67881, #9476 ) ;
#5034 = CARTESIAN_POINT ( 'NONE',  ( -71.28077210551055032, 20.70883253687733117, -95.00000000000133582 ) ) ;
#5035 = ORIENTED_EDGE ( 'NONE', *, *, #9397, .T. ) ;
#5036 = ORIENTED_EDGE ( 'NONE', *, *, #34058, .F. ) ;
#5037 = VECTOR ( 'NONE', #55405, 1000.000000000000000 ) ;
#5038 = DIRECTION ( 'NONE',  ( -0.000000000000000000, 1.000000000000000000, -0.000000000000000000 ) ) ;
#5039 = CARTESIAN_POINT ( 'NONE',  ( 0.000000000000000000, 0.000000000000000000, 41.38025477438755928 ) ) ;
#5040 = CARTESIAN_POINT ( 'NONE',  ( 29.99999999999999645, -27.00000000000000355, 15.00000000000000000 ) ) ;
#5041 = ORIENTED_EDGE ( 'NONE', *, *, #67906, .F. ) ;
#5042 = CARTESIAN_POINT ( 'NONE',  ( -58.32860549785896609, 15.58423118879329294, -76.31204309374547279 ) ) ;
#5043 = FACE_OUTER_BOUND ( 'NONE', #147, .T. ) ;
#5044 = CARTESIAN_POINT ( 'NONE',  ( 33.03621582719333816, 7.666716336587136027, -20.24858811402686953 ) ) ;
#5045 = CARTESIAN_POINT ( 'NONE',  ( 173.9457771591584674, 73.05793967547533896, -46.04376121573756819 ) ) ;
#5046 = CARTESIAN_POINT ( 'NONE',  ( 163.4909271546005698, 62.48739187115877058, 86.07095713937944481 ) ) ;
#5047 = CARTESIAN_POINT ( 'NONE',  ( 32.68347998332510684, -12.52158680757303344, 0.000000000000000000 ) ) ;
#5048 = ADVANCED_FACE ( 'NONE', ( #2457 ), #65562, .T. ) ;
#5049 = EDGE_LOOP ( 'NONE', ( #1005, #792, #45442, #14583 ) ) ;
#5050 = EDGE_CURVE ( 'NONE', #55210, #28296, #17940, .T. ) ;
#5051 = FACE_OUTER_BOUND ( 'NONE', #45723, .T. ) ;
#5052 = CARTESIAN_POINT ( 'NONE',  ( -27.70185240367227664, 10.02491413133431486, 31.20927824995889921 ) ) ;
#5053 = CARTESIAN_POINT ( 'NONE',  ( 197.3756653044963514, 98.41886189307120958, 35.07559596873900176 ) ) ;
#5054 = CARTESIAN_POINT ( 'NONE',  ( -86.16954081945932842, 26.41440641755240293, 91.85847073401009766 ) ) ;
#5056 = EDGE_LOOP ( 'NONE', ( #42269, #24175, #40184, #42974 ) ) ;
#5055 = LINE ( 'NONE', #32486, #53418 ) ;
#5057 = ORIENTED_EDGE ( 'NONE', *, *, #30929, .F. ) ;
#5058 = ORIENTED_EDGE ( 'NONE', *, *, #48308, .F. ) ;
#5059 = DIRECTION ( 'NONE',  ( -0.000000000000000000, -0.000000000000000000, 1.000000000000000000 ) ) ;
#5060 = CARTESIAN_POINT ( 'NONE',  ( 72.99999999999998579, 8.939921633775675282E-15, 85.00000000000000000 ) ) ;
#5061 = EDGE_CURVE ( 'NONE', #67779, #9014, #65792, .T. ) ;
#5062 = FACE_OUTER_BOUND ( 'NONE', #58838, .T. ) ;
#5063 = EDGE_CURVE ( 'NONE', #29619, #53557, #1407, .T. ) ;
#5064 = DIRECTION ( 'NONE',  ( -1.000000000000000000, 0.000000000000000000, -1.110223024625156294E-16 ) ) ;
#5065 = DIRECTION ( 'NONE',  ( -0.4338837391175656699, 0.9009688679024155933, 5.102127870520019688E-18 ) ) ;
#5066 = CARTESIAN_POINT ( 'NONE',  ( 20.74093720376649941, 6.709541214524348263, -21.82772143202600290 ) ) ;
#5067 = AXIS2_PLACEMENT_3D ( 'NONE', #6785, #12072, #61300 ) ;
#5068 = CARTESIAN_POINT ( 'NONE',  ( 198.7765072002625288, -170.0000000000000000, 94.99999999999866418 ) ) ;
#5069 = ORIENTED_EDGE ( 'NONE', *, *, #52323, .T. ) ;
#5070 = ORIENTED_EDGE ( 'NONE', *, *, #6132, .T. ) ;
#5071 = EDGE_CURVE ( 'NONE', #29654, #21604, #65432, .T. ) ;
#5072 = CARTESIAN_POINT ( 'NONE',  ( 68.62997155117723480, 15.08415013720829201, -11.37927540543296701 ) ) ;
#5073 = AXIS2_PLACEMENT_3D ( 'NONE', #51772, #46483, #51435 ) ;
#5074 = CARTESIAN_POINT ( 'NONE',  ( -86.16710354151692286, 26.41338104675946852, -42.38095692992142460 ) ) ;
#5075 = CARTESIAN_POINT ( 'NONE',  ( 102.7472068462325012, 25.56604832181697162, 90.36773254186026350 ) ) ;
#5076 = EDGE_CURVE ( 'NONE', #50492, #67476, #66494, .T. ) ;
#5077 = CARTESIAN_POINT ( 'NONE',  ( 112.5537757279407458, 31.07998172410697535, -9.426844704073509718 ) ) ;
#5078 = AXIS2_PLACEMENT_3D ( 'NONE', #60418, #29110, #49145 ) ;
#5079 = AXIS2_PLACEMENT_3D ( 'NONE', #60400, #28035, #12215 ) ;
#5080 = CARTESIAN_POINT ( 'NONE',  ( 181.9406741394861058, 79.47484497224790800, -36.26201039870598919 ) ) ;
#5081 = CARTESIAN_POINT ( 'NONE',  ( 35.39413431650373099, 0.000000000000000000, -9.999999999999998224 ) ) ;
#5082 = CARTESIAN_POINT ( 'NONE',  ( -155.6080424972482774, 70.89247817759412840, 87.53634334609833445 ) ) ;
#5083 = ORIENTED_EDGE ( 'NONE', *, *, #5149, .F. ) ;
#5084 = ORIENTED_EDGE ( 'NONE', *, *, #25971, .T. ) ;
#5085 = ORIENTED_EDGE ( 'NONE', *, *, #28263, .T. ) ;
#5086 = AXIS2_PLACEMENT_3D ( 'NONE', #62696, #14496, #46851 ) ;
#5087 = CARTESIAN_POINT ( 'NONE',  ( -156.6644740249450649, 71.86407434531901117, -17.72729415336047865 ) ) ;
#5088 = CARTESIAN_POINT ( 'NONE',  ( 36.09469435220864852, 9.015003538710487874, -49.86883716977957448 ) ) ;
#5089 = CARTESIAN_POINT ( 'NONE',  ( 179.4207200232661137, 76.93724985992177778, 71.01710357248663286 ) ) ;
#5090 = ADVANCED_FACE ( 'NONE', ( #7034 ), #16879, .T. ) ;
#5091 = DIRECTION ( 'NONE',  ( 5.096990367256702165E-18, 2.289061013375335776E-19, -1.000000000000000000 ) ) ;
#5092 = EDGE_CURVE ( 'NONE', #3346, #26889, #39741, .T. ) ;
#5093 = CARTESIAN_POINT ( 'NONE',  ( 21.38432669263065833, -61.76910524360950916, 3.125053320693560257E-16 ) ) ;
#5094 = ADVANCED_FACE ( 'NONE', ( #38341 ), #61199, .T. ) ;
#5095 = ORIENTED_EDGE ( 'NONE', *, *, #20108, .T. ) ;
#5096 = EDGE_CURVE ( 'NONE', #66616, #22625, #52147, .T. ) ;
#5097 = CARTESIAN_POINT ( 'NONE',  ( 39.40195752203892710, 8.409560354027400209, 56.75838489642694640 ) ) ;
#5098 = CARTESIAN_POINT ( 'NONE',  ( -152.2964402771108610, 66.58174574061952455, 72.03110441543591946 ) ) ;
#5099 = CARTESIAN_POINT ( 'NONE',  ( 149.0250918491436778, 0.000000000000000000, -4.435653166495538535 ) ) ;
#5100 = CARTESIAN_POINT ( 'NONE',  ( 185.5572090022886016, 83.24697331286186852, 69.69128790936149187 ) ) ;
#5101 = DIRECTION ( 'NONE',  ( 1.000000000000000000, 1.001918829714556097E-14, -9.899279560275163638E-15 ) ) ;
#5102 = DIRECTION ( 'NONE',  ( -1.000000000000000000, 0.000000000000000000, 0.000000000000000000 ) ) ;
#5103 = CARTESIAN_POINT ( 'NONE',  ( -442.6627218934913799, 0.000000000000000000, -136.4497041420118251 ) ) ;
#5104 = DIRECTION ( 'NONE',  ( -0.000000000000000000, -0.000000000000000000, -1.000000000000000000 ) ) ;
#5105 = CARTESIAN_POINT ( 'NONE',  ( 14.81290967676422277, 7.477658233646008235, 3.217552154449582424 ) ) ;
#5106 = ORIENTED_EDGE ( 'NONE', *, *, #51386, .T. ) ;
#5107 = DIRECTION ( 'NONE',  ( 1.000000000000000000, 0.000000000000000000, 0.000000000000000000 ) ) ;
#5108 = SHAPE_DEFINITION_REPRESENTATION ( #35610, #63080 ) ;
#5109 = DIRECTION ( 'NONE',  ( 1.000000000000000000, 0.000000000000000000, -0.000000000000000000 ) ) ;
#5110 = CARTESIAN_POINT ( 'NONE',  ( -132.9109786433856755, 51.29129389542017492, -39.75304253929575538 ) ) ;
#5111 = CARTESIAN_POINT ( 'NONE',  ( -108.5248383251030901, 37.21456094989613206, -46.67577077482953030 ) ) ;
#5112 = FACE_OUTER_BOUND ( 'NONE', #62244, .T. ) ;
#5113 = VERTEX_POINT ( 'NONE', #68215 ) ;
#5114 = VERTEX_POINT ( 'NONE', #40430 ) ;
#5115 = CARTESIAN_POINT ( 'NONE',  ( -23.99924996210628336, 8.487987924059016365, -14.99299851994305577 ) ) ;
#5116 = CARTESIAN_POINT ( 'NONE',  ( 197.5344630110112973, 98.61758706718747192, 7.618816888282892386 ) ) ;
#5117 = ORIENTED_EDGE ( 'NONE', *, *, #39806, .F. ) ;
#5118 = VECTOR ( 'NONE', #13219, 1000.000000000000114 ) ;
#5119 = FACE_OUTER_BOUND ( 'NONE', #39832, .T. ) ;
#5120 = ORIENTED_EDGE ( 'NONE', *, *, #47618, .T. ) ;
#5121 = CARTESIAN_POINT ( 'NONE',  ( 129.4887940973039235, 40.01039828304091373, -64.25216638727819429 ) ) ;
#5122 = CARTESIAN_POINT ( 'NONE',  ( 132.7179291807801746, 40.74118679001691845, 29.59377605348581142 ) ) ;
#5123 = AXIS2_PLACEMENT_3D ( 'NONE', #5757, #63827, #58199 ) ;
#5124 = LINE ( 'NONE', #4778, #49873 ) ;
#5125 = CARTESIAN_POINT ( 'NONE',  ( 157.4703587214989113, 57.65129005721575339, -89.81328548006499091 ) ) ;
#5126 = VECTOR ( 'NONE', #63857, 1000.000000000000000 ) ;
#5128 = DIRECTION ( 'NONE',  ( -1.000000000000000000, 0.000000000000000000, 0.000000000000000000 ) ) ;
#5127 = CIRCLE ( 'NONE', #24237, 242.4895526022646379 ) ;
#5130 = EDGE_LOOP ( 'NONE', ( #32465, #36018, #4205, #43467 ) ) ;
#5129 = CARTESIAN_POINT ( 'NONE',  ( 8.000000000000007105, 249.8719672152120381, -95.00000000000133582 ) ) ;
#5131 =( GEOMETRIC_REPRESENTATION_CONTEXT ( 3 ) GLOBAL_UNCERTAINTY_ASSIGNED_CONTEXT ( ( #65583 ) ) GLOBAL_UNIT_ASSIGNED_CONTEXT ( ( #3143, #55544, #13007 ) ) REPRESENTATION_CONTEXT ( 'NONE', 'WORKASPACE' ) );
#5132 = AXIS2_PLACEMENT_3D ( 'NONE', #56450, #51868, #41661 ) ;
#5133 = VERTEX_POINT ( 'NONE', #56967 ) ;
#5134 = ORIENTED_EDGE ( 'NONE', *, *, #19397, .T. ) ;
#5135 =( BOUNDED_CURVE ( )  B_SPLINE_CURVE ( 3, ( #39750, #65803, #55574, #17599 ),
 .UNSPECIFIED., .F., .F. ) 
 B_SPLINE_CURVE_WITH_KNOTS ( ( 4, 4 ),
 ( 1.570796326794883679, 3.141592653589778461 ),
 .UNSPECIFIED. ) 
 CURVE ( )  GEOMETRIC_REPRESENTATION_ITEM ( )  RATIONAL_B_SPLINE_CURVE ( ( 1.000000000000000000, 0.8047378541243654926, 0.8047378541243654926, 1.000000000000000000 ) ) 
 REPRESENTATION_ITEM ( '' )  );
#5137 = ADVANCED_FACE ( 'NONE', ( #56258 ), #41479, .F. ) ;
#5136 = CARTESIAN_POINT ( 'NONE',  ( -167.0073208999199608, 82.02183861952778443, 7.124899887039663149 ) ) ;
#5138 = VECTOR ( 'NONE', #28617, 1000.000000000000000 ) ;
#5139 = FACE_BOUND ( 'NONE', #5452, .T. ) ;
#5140 = CARTESIAN_POINT ( 'NONE',  ( -178.7458319892713803, 93.61502008198021940, -10.39986922783644374 ) ) ;
#5141 = CARTESIAN_POINT ( 'NONE',  ( -166.3231866619663890, 81.31146386205588783, -65.87609374347549362 ) ) ;
#5143 = ORIENTED_EDGE ( 'NONE', *, *, #21925, .F. ) ;
#5142 = DIRECTION ( 'NONE',  ( 0.000000000000000000, 0.000000000000000000, -1.000000000000000000 ) ) ;
#5144 = CARTESIAN_POINT ( 'NONE',  ( -106.2831548001319959, 36.00138616880182241, 85.35841622373546045 ) ) ;
#5145 = ORIENTED_EDGE ( 'NONE', *, *, #67910, .F. ) ;
#5146 = CARTESIAN_POINT ( 'NONE',  ( 56.48986020701288169, 12.27998416584893704, 94.71400107496813803 ) ) ;
#5147 = CYLINDRICAL_SURFACE ( 'NONE', #1901, 7.500000000000020428 ) ;
#5148 = ADVANCED_FACE ( 'NONE', ( #51683 ), #13364, .F. ) ;
#5149 = EDGE_CURVE ( 'NONE', #9638, #32243, #67191, .T. ) ;
#5150 = EDGE_CURVE ( 'NONE', #417, #634, #12847, .T. ) ;
#5151 = CARTESIAN_POINT ( 'NONE',  ( 79.11678624235125312, 16.99307331934756604, -16.46842441967982751 ) ) ;
#5152 = CARTESIAN_POINT ( 'NONE',  ( -132.9227230387960788, 52.53474289881228287, -66.62845719056252847 ) ) ;
#5153 = DIRECTION ( 'NONE',  ( -1.000000000000000000, 0.000000000000000000, 0.000000000000000000 ) ) ;
#5154 = CARTESIAN_POINT ( 'NONE',  ( -97.47339919287389876, 30.40512551257286944, 16.95259712630159044 ) ) ;
#5155 = CARTESIAN_POINT ( 'NONE',  ( -154.4518102898914549, 68.48895432927903926, -90.34576860233968887 ) ) ;
#5156 = ORIENTED_EDGE ( 'NONE', *, *, #23205, .T. ) ;
#5157 = EDGE_LOOP ( 'NONE', ( #14135, #29533, #1574, #37825 ) ) ;
#5158 = EDGE_CURVE ( 'NONE', #15307, #27145, #61873, .T. ) ;
#5159 = CYLINDRICAL_SURFACE ( 'NONE', #24851, 65.00000000000000000 ) ;
#5160 = CARTESIAN_POINT ( 'NONE',  ( 11.82322073186613309, 6.406156243758797331, 31.14383489137281202 ) ) ;
#5161 = CARTESIAN_POINT ( 'NONE',  ( -2.282530889443167084E-17, 4.999999999999999112, 21.42428528562853529 ) ) ;
#5162 = DIRECTION ( 'NONE',  ( -0.3930250316539278255, 0.9195277725514487965, 0.000000000000000000 ) ) ;
#5163 = DIRECTION ( 'NONE',  ( -0.5508969814521065267, 0.8345732537212999791, 0.000000000000000000 ) ) ;
#5164 = DIRECTION ( 'NONE',  ( -0.000000000000000000, -1.000000000000000000, -0.000000000000000000 ) ) ;
#5165 = CARTESIAN_POINT ( 'NONE',  ( 84.28078136020371858, 18.63296074526051527, 44.33893942252232989 ) ) ;
#5166 = CARTESIAN_POINT ( 'NONE',  ( 23.37466875127750754, -46.07527483894288878, 26.66469104408689361 ) ) ;
#5167 = CARTESIAN_POINT ( 'NONE',  ( 41.34269507549202416, 9.685203600174698835, -50.38080312760155266 ) ) ;
#5168 = CARTESIAN_POINT ( 'NONE',  ( -15.55634918610400597, 20.55634918610405748, 2.000000000000001776 ) ) ;
#5169 = PRODUCT ( 'motor assembly', 'motor assembly', '', ( #10047 ) ) ;
#5170 = VERTEX_POINT ( 'NONE', #57308 ) ;
#5171 = DIRECTION ( 'NONE',  ( -0.000000000000000000, 1.000000000000000000, -0.000000000000000000 ) ) ;
#5172 = ORIENTED_EDGE ( 'NONE', *, *, #42706, .T. ) ;
#5173 = VECTOR ( 'NONE', #39093, 1000.000000000000000 ) ;
#5174 = CARTESIAN_POINT ( 'NONE',  ( -34.51918258780364823, 10.11719938103014904, 4.029186606375436241 ) ) ;
#5175 = CARTESIAN_POINT ( 'NONE',  ( 83.59652366361571296, 19.46709838196855813, 70.92029102677756214 ) ) ;
#5176 = CARTESIAN_POINT ( 'NONE',  ( 92.21252738308864139, 22.47457138983957137, 59.02458724508797872 ) ) ;
#5177 = CARTESIAN_POINT ( 'NONE',  ( 149.9838583332407893, 52.05699766415857255, -17.30813132279020294 ) ) ;
#5178 = DIRECTION ( 'NONE',  ( -0.000000000000000000, -0.000000000000000000, -1.000000000000000000 ) ) ;
#5179 = VECTOR ( 'NONE', #22746, 1000.000000000000000 ) ;
#5180 = CARTESIAN_POINT ( 'NONE',  ( 38.42384008295177011, 8.283891555743467805, -62.51250981452189137 ) ) ;
#5181 = DIRECTION ( 'NONE',  ( 0.000000000000000000, 0.000000000000000000, 1.000000000000000000 ) ) ;
#5182 = DIRECTION ( 'NONE',  ( -0.1342332658176522420, -0.9909497617679351444, 0.000000000000000000 ) ) ;
#5183 = EDGE_CURVE ( 'NONE', #902, #36668, #9118, .T. ) ;
#5184 = EDGE_CURVE ( 'NONE', #22856, #4077, #33009, .T. ) ;
#5185 = AXIS2_PLACEMENT_3D ( 'NONE', #67857, #26320, #19651 ) ;
#5186 = VECTOR ( 'NONE', #48521, 1000.000000000000000 ) ;
#5187 = ORIENTED_EDGE ( 'NONE', *, *, #12766, .F. ) ;
#5188 = DIRECTION ( 'NONE',  ( -1.000000000000000000, 0.000000000000000000, 0.000000000000000000 ) ) ;
#5189 = ORIENTED_EDGE ( 'NONE', *, *, #28493, .T. ) ;
#5190 = CARTESIAN_POINT ( 'NONE',  ( 0.000000000000000000, 0.000000000000000000, 0.000000000000000000 ) ) ;
#5191 = CARTESIAN_POINT ( 'NONE',  ( 9.689943677145722134, 7.388265075009365468, -74.23619429177909979 ) ) ;
#5193 = EDGE_CURVE ( 'NONE', #30932, #4994, #40774, .T. ) ;
#5192 = CARTESIAN_POINT ( 'NONE',  ( 22.91085947427763614, -30.73415342201930756, 13.32819397642333392 ) ) ;
#5194 = CARTESIAN_POINT ( 'NONE',  ( -15.55634918610400597, 20.55634918610405748, 85.00100000000000477 ) ) ;
#5195 = CARTESIAN_POINT ( 'NONE',  ( -0.8011128725815451768, 6.535315321814186618, 40.25565733622043041 ) ) ;
#5196 = DIRECTION ( 'NONE',  ( 0.000000000000000000, 1.000000000000000000, 0.000000000000000000 ) ) ;
#5197 = CARTESIAN_POINT ( 'NONE',  ( 80.46041939316872060, 18.46168943176929034, 86.62235641862685043 ) ) ;
#5198 = AXIS2_PLACEMENT_3D ( 'NONE', #13319, #8030, #50945 ) ;
#5199 = EDGE_LOOP ( 'NONE', ( #19131, #50473, #60429, #68962 ) ) ;
#5200 = CARTESIAN_POINT ( 'NONE',  ( 620.5106130828497726, 928.6907676558208777, 788.0951305877202913 ) ) ;
#5201 = DIRECTION ( 'NONE',  ( -0.000000000000000000, -0.000000000000000000, 1.000000000000000000 ) ) ;
#5202 = CARTESIAN_POINT ( 'NONE',  ( 179.4227152810057930, 78.36166152262363482, -24.20640214036799520 ) ) ;
#5203 = CARTESIAN_POINT ( 'NONE',  ( -109.7790042512817905, 37.90666514836944145, 64.57243962987085695 ) ) ;
#5204 = CONTEXT_DEPENDENT_SHAPE_REPRESENTATION ( #18842, #12533 ) ;
#5205 = CARTESIAN_POINT ( 'NONE',  ( -132.8150886319751578, 52.45790550853840273, -45.31429239349645144 ) ) ;
#5206 = VERTEX_POINT ( 'NONE', #51345 ) ;
#5207 = DIRECTION ( 'NONE',  ( -0.000000000000000000, 1.000000000000000000, -0.000000000000000000 ) ) ;
#5208 = CARTESIAN_POINT ( 'NONE',  ( 94.07616572255072640, 22.09777530676767654, 63.03225789469448159 ) ) ;
#5209 = CARTESIAN_POINT ( 'NONE',  ( -154.6244975120027902, 68.64332268850641583, 86.39598974807935861 ) ) ;
#5210 = PLANE ( 'NONE',  #52619 ) ;
#5211 = VERTEX_POINT ( 'NONE', #46391 ) ;
#5212 = LINE ( 'NONE', #48433, #21044 ) ;
#5213 = CARTESIAN_POINT ( 'NONE',  ( 82.34401416830218068, 19.05992892018826979, 4.207522528255770666 ) ) ;
#5214 = CARTESIAN_POINT ( 'NONE',  ( 159.2258951716709703, 60.31399909112331414, 2.759764520436461588 ) ) ;
#5215 = LINE ( 'NONE', #21057, #64490 ) ;
#5216 = ORIENTED_EDGE ( 'NONE', *, *, #11597, .F. ) ;
#5217 = CARTESIAN_POINT ( 'NONE',  ( 46.66904755831210139, 4.999999999999909406, 85.00100000000000477 ) ) ;
#5218 = ORIENTED_EDGE ( 'NONE', *, *, #23199, .F. ) ;
#5219 = VECTOR ( 'NONE', #53760, 1000.000000000000000 ) ;
#5221 = ADVANCED_FACE ( 'NONE', ( #3841 ), #18979, .T. ) ;
#5220 = CARTESIAN_POINT ( 'NONE',  ( -76.78936026062118003, 21.61552955137052479, -23.03615461302700851 ) ) ;
#5222 = DIRECTION ( 'NONE',  ( 0.000000000000000000, -0.000000000000000000, -1.000000000000000000 ) ) ;
#5223 = DIRECTION ( 'NONE',  ( 1.000000000000000000, 0.000000000000000000, -0.000000000000000000 ) ) ;
#5224 = AXIS2_PLACEMENT_3D ( 'NONE', #67576, #45774, #40485 ) ;
#5226 = ORIENTED_EDGE ( 'NONE', *, *, #40932, .F. ) ;
#5225 = DIRECTION ( 'NONE',  ( 1.387778780781445922E-16, -1.000000000000000000, 0.000000000000000000 ) ) ;
#5227 = CARTESIAN_POINT ( 'NONE',  ( -178.2381786520593892, 93.01028335822118720, 43.81022153523580442 ) ) ;
#5228 = FACE_OUTER_BOUND ( 'NONE', #4118, .T. ) ;
#5229 = DIRECTION ( 'NONE',  ( 0.000000000000000000, 0.000000000000000000, 1.000000000000000000 ) ) ;
#5230 = CIRCLE ( 'NONE', #44555, 22.00000000000000355 ) ;
#5231 = EDGE_LOOP ( 'NONE', ( #57842, #67743, #13618, #3448 ) ) ;
#5232 = CARTESIAN_POINT ( 'NONE',  ( -143.3980294393558950, 60.45217072626398647, 33.86310790016815275 ) ) ;
#5233 = DIRECTION ( 'NONE',  ( 0.000000000000000000, 0.000000000000000000, 1.000000000000000000 ) ) ;
#5234 = EDGE_CURVE ( 'NONE', #25372, #38916, #8075, .T. ) ;
#5235 = CARTESIAN_POINT ( 'NONE',  ( 139.3067271572849108, 44.81402783181196980, 69.01324371968860305 ) ) ;
#5236 = CARTESIAN_POINT ( 'NONE',  ( -167.9853834315979384, 81.58767916550894483, 43.80779636558261103 ) ) ;
#5237 = CARTESIAN_POINT ( 'NONE',  ( 128.0882145863933488, 39.20607399008169125, 59.03564582321932619 ) ) ;
#5238 = EDGE_CURVE ( 'NONE', #13950, #30161, #35854, .T. ) ;
#5239 = ORIENTED_EDGE ( 'NONE', *, *, #60440, .T. ) ;
#5241 = EDGE_CURVE ( 'NONE', #30922, #11740, #52371, .T. ) ;
#5240 = CARTESIAN_POINT ( 'NONE',  ( 45.76405797021010358, 10.34101216371941767, 14.54853712646751340 ) ) ;
#5242 = ORIENTED_EDGE ( 'NONE', *, *, #14158, .F. ) ;
#5243 = EDGE_LOOP ( 'NONE', ( #2473, #20569, #48322, #43568 ) ) ;
#5244 = DIRECTION ( 'NONE',  ( -0.000000000000000000, -0.000000000000000000, -1.000000000000000000 ) ) ;
#5245 = EDGE_CURVE ( 'NONE', #45779, #42920, #25311, .T. ) ;
#5246 = DIRECTION ( 'NONE',  ( 1.000000000000000000, 0.000000000000000000, 0.000000000000000000 ) ) ;
#5247 = SURFACE_STYLE_USAGE ( .BOTH. , #43554 ) ;
#5248 = CARTESIAN_POINT ( 'NONE',  ( -102.2801239173131194, -170.0000000000000000, -15.67002667451224163 ) ) ;
#5249 = FACE_OUTER_BOUND ( 'NONE', #17680, .T. ) ;
#5250 = CARTESIAN_POINT ( 'NONE',  ( 9.962235950564870990, 64.23203137738423152, 170.0000000000000000 ) ) ;
#5251 = CARTESIAN_POINT ( 'NONE',  ( -131.2803255164624545, 50.14412978403778709, 70.18912820271620490 ) ) ;
#5252 = CARTESIAN_POINT ( 'NONE',  ( 24.33197399592810228, 22.91807451166457810, 6.893342938366306072 ) ) ;
#5253 = ORIENTED_EDGE ( 'NONE', *, *, #58288, .F. ) ;
#5254 = CARTESIAN_POINT ( 'NONE',  ( 23.63370729589335895, -52.11334794818031213, 73.58025477438755502 ) ) ;
#5255 = ORIENTED_EDGE ( 'NONE', *, *, #32277, .F. ) ;
#5256 = CARTESIAN_POINT ( 'NONE',  ( -78.19438069111009781, 23.21811806230639164, 57.26275173013681297 ) ) ;
#5257 = CARTESIAN_POINT ( 'NONE',  ( 181.5072453427591199, 79.03352099595181812, 29.30859410551139277 ) ) ;
#5258 = CARTESIAN_POINT ( 'NONE',  ( 60.63507185982732040, 12.13307030573224310, -62.94891509126097873 ) ) ;
#5259 = CARTESIAN_POINT ( 'NONE',  ( -78.18913509716431065, 22.13995206110505265, 18.57365054920947145 ) ) ;
#5260 = DIRECTION ( 'NONE',  ( 1.000000000000000000, 0.000000000000000000, 0.000000000000000000 ) ) ;
#5261 = CARTESIAN_POINT ( 'NONE',  ( 21.75198946226450403, 7.772524967554921282, 32.94053441732803833 ) ) ;
#5262 = CARTESIAN_POINT ( 'NONE',  ( 202.3068201863369495, 103.1211636617681791, 83.26500311953536482 ) ) ;
#5263 = CARTESIAN_POINT ( 'NONE',  ( 164.8908506817023749, 64.97619709085124384, -69.34418866066772580 ) ) ;
#5264 = EDGE_LOOP ( 'NONE', ( #19487, #7410, #68230, #42287 ) ) ;
#5265 = CARTESIAN_POINT ( 'NONE',  ( -32.68347998332510684, -12.52158680757305298, 30.00000000000000000 ) ) ;
#5266 = FACE_OUTER_BOUND ( 'NONE', #39432, .T. ) ;
#5267 = ORIENTED_EDGE ( 'NONE', *, *, #18972, .F. ) ;
#5268 = EDGE_CURVE ( 'NONE', #22494, #32164, #467, .T. ) ;
#5269 = ORIENTED_EDGE ( 'NONE', *, *, #7319, .T. ) ;
#5270 = CARTESIAN_POINT ( 'NONE',  ( -28.13527276074848160, 10.08983026464525068, -76.39933447701551472 ) ) ;
#5271 = CARTESIAN_POINT ( 'NONE',  ( 55.90536342106781831, 11.13510150712953184, -45.65778433454865848 ) ) ;
#5272 = CARTESIAN_POINT ( 'NONE',  ( -185.0000000000000000, 2.265596578422603396E-14, 2.499999999999999556 ) ) ;
#5273 = VECTOR ( 'NONE', #19989, 1000.000000000000000 ) ;
#5274 = CYLINDRICAL_SURFACE ( 'NONE', #41754, 65.00000000000000000 ) ;
#5275 = DIRECTION ( 'NONE',  ( 0.000000000000000000, 1.000000000000000000, -0.000000000000000000 ) ) ;
#5276 = CIRCLE ( 'NONE', #45711, 4.250000000000000000 ) ;
#5277 = EDGE_LOOP ( 'NONE', ( #54537, #58069 ) ) ;
#5278 = ORIENTED_EDGE ( 'NONE', *, *, #1996, .F. ) ;
#5279 = DIRECTION ( 'NONE',  ( -0.000000000000000000, 0.000000000000000000, 1.000000000000000000 ) ) ;
#5280 = VECTOR ( 'NONE', #47775, 1000.000000000000000 ) ;
#5281 = ORIENTED_EDGE ( 'NONE', *, *, #24163, .T. ) ;
#5282 = DIRECTION ( 'NONE',  ( -1.000000000000000000, 0.000000000000000000, 0.000000000000000000 ) ) ;
#5283 = CARTESIAN_POINT ( 'NONE',  ( 186.6289143948428944, 85.88097584402285634, -92.34696716306295627 ) ) ;
#5284 = CARTESIAN_POINT ( 'NONE',  ( 61.33627421985470818, 12.28939706835342882, 71.47105798233256735 ) ) ;
#5285 = CARTESIAN_POINT ( 'NONE',  ( 41.66904755831212981, 15.55634918610394379, 2.000000000000001776 ) ) ;
#5286 = AXIS2_PLACEMENT_3D ( 'NONE', #46791, #20396, #24661 ) ;
#5287 = FACE_OUTER_BOUND ( 'NONE', #18779, .T. ) ;
#5288 =( LENGTH_UNIT ( ) NAMED_UNIT ( * ) SI_UNIT ( .MILLI., .METRE. ) );
#5289 = AXIS2_PLACEMENT_3D ( 'NONE', #24118, #66692, #13218 ) ;
#5290 = CARTESIAN_POINT ( 'NONE',  ( 0.000000000000000000, 0.000000000000000000, 133.5802547743875550 ) ) ;
#5291 = VERTEX_POINT ( 'NONE', #61545 ) ;
#5292 = ORIENTED_EDGE ( 'NONE', *, *, #45012, .T. ) ;
#5293 = CARTESIAN_POINT ( 'NONE',  ( 5.799999999999999822, -9.237604307034018802, 3.355146209984123968E-17 ) ) ;
#5294 = CARTESIAN_POINT ( 'NONE',  ( 6.400000000000000355, -4.618802153517016507, -8.000000000000000000 ) ) ;
#5295 = LINE ( 'NONE', #63702, #33005 ) ;
#5296 = LINE ( 'NONE', #9892, #65809 ) ;
#5297 = FACE_OUTER_BOUND ( 'NONE', #5578, .T. ) ;
#5298 = CARTESIAN_POINT ( 'NONE',  ( 11.47475555585564422, 7.407171684781389764, 85.05957700157702561 ) ) ;
#5299 = ORIENTED_EDGE ( 'NONE', *, *, #15797, .T. ) ;
#5300 = EDGE_CURVE ( 'NONE', #24137, #58000, #24268, .T. ) ;
#5301 = CARTESIAN_POINT ( 'NONE',  ( -102.2801239173131052, 32.78103895658057354, 57.36362509687880618 ) ) ;
#5302 = ADVANCED_FACE ( 'NONE', ( #29524 ), #29883, .T. ) ;
#5303 = EDGE_LOOP ( 'NONE', ( #9494, #46522, #52950, #1731 ) ) ;
#5304 = CARTESIAN_POINT ( 'NONE',  ( -71.56718866013693514, 19.74312628447962936, 40.38945691434815899 ) ) ;
#5305 = ORIENTED_EDGE ( 'NONE', *, *, #22711, .F. ) ;
#5306 = ADVANCED_FACE ( 'NONE', ( #30234 ), #63957, .F. ) ;
#5307 = EDGE_CURVE ( 'NONE', #1035, #54490, #5215, .T. ) ;
#5308 = ORIENTED_EDGE ( 'NONE', *, *, #60924, .T. ) ;
#5309 = CARTESIAN_POINT ( 'NONE',  ( -122.3994536713185255, 45.42826354555018042, 17.91575039578479078 ) ) ;
#5310 = CARTESIAN_POINT ( 'NONE',  ( -180.2252811616041868, 95.40045830523432357, 67.58802342263081187 ) ) ;
#5311 = CARTESIAN_POINT ( 'NONE',  ( 129.1381264900935264, 38.64720302602608371, 69.70481210122846960 ) ) ;
#5312 = ORIENTED_EDGE ( 'NONE', *, *, #36471, .F. ) ;
#5313 = VECTOR ( 'NONE', #51755, 1000.000000000000000 ) ;
#5314 = SURFACE_SIDE_STYLE ('',( #53485 ) ) ;
#5315 = CIRCLE ( 'NONE', #30041, 8.000000000000000000 ) ;
#5316 = LINE ( 'NONE', #10238, #50013 ) ;
#5317 = DIRECTION ( 'NONE',  ( -0.7227948638273978821, 0.6910626489868580968, 5.102127870520021999E-18 ) ) ;
#5318 = DIRECTION ( 'NONE',  ( 0.000000000000000000, 0.000000000000000000, -1.000000000000000000 ) ) ;
#5319 = CARTESIAN_POINT ( 'NONE',  ( 55.04622673932353649, 19.32405938320713545, 27.58472315868179692 ) ) ;
#5320 = EDGE_CURVE ( 'NONE', #30745, #45870, #39804, .T. ) ;
#5321 = LINE ( 'NONE', #59115, #3545 ) ;
#5322 = CARTESIAN_POINT ( 'NONE',  ( -30.46060138092288838, 9.432375387772214737, 45.16858539813694051 ) ) ;
#5323 = VECTOR ( 'NONE', #24064, 1000.000000000000000 ) ;
#5325 = EDGE_CURVE ( 'NONE', #62792, #66752, #31273, .T. ) ;
#5324 = CARTESIAN_POINT ( 'NONE',  ( -144.2155061717026001, 61.10843690942975570, -63.83700193691978342 ) ) ;
#5326 = ORIENTED_EDGE ( 'NONE', *, *, #12858, .F. ) ;
#5327 = DIRECTION ( 'NONE',  ( 0.000000000000000000, 0.000000000000000000, 1.000000000000000000 ) ) ;
#5328 = COLOUR_RGB ( '',0.7921568627450980005, 0.8196078431372548767, 0.9333333333333333481 ) ;
#5329 = CYLINDRICAL_SURFACE ( 'NONE', #1723, 65.36598343705435354 ) ;
#5330 = CARTESIAN_POINT ( 'NONE',  ( -173.5372686962700470, 89.10569330281724376, 57.66624519710474317 ) ) ;
#5331 = CARTESIAN_POINT ( 'NONE',  ( 0.01678220609566008145, 0.7854258609844494421, 8.000000000000000000 ) ) ;
#5332 = CARTESIAN_POINT ( 'NONE',  ( -118.6302575928420424, 43.07263081214308897, -40.52659648218294564 ) ) ;
#5333 = CARTESIAN_POINT ( 'NONE',  ( -85.90077524418997257, 26.30132018890136791, 13.06823648188070131 ) ) ;
#5334 = VECTOR ( 'NONE', #56402, 1000.000000000000000 ) ;
#5335 = DIRECTION ( 'NONE',  ( -0.7660444431189771253, 0.6427876096865404731, 0.000000000000000000 ) ) ;
#5336 = CARTESIAN_POINT ( 'NONE',  ( 112.2224082406587229, 21.53716320950900709, 4.490767689115658712 ) ) ;
#5337 = FACE_OUTER_BOUND ( 'NONE', #17010, .T. ) ;
#5338 = CARTESIAN_POINT ( 'NONE',  ( 123.4242852856285566, 10.00000000000000000, -30.00000000000000000 ) ) ;
#5339 = CARTESIAN_POINT ( 'NONE',  ( 159.2319614735955611, 59.03334608081209467, 2.761277528605094567 ) ) ;
#5340 = CARTESIAN_POINT ( 'NONE',  ( 91.12448333640236342, 22.07449368110502519, -22.50004146135145433 ) ) ;
#5341 = ORIENTED_EDGE ( 'NONE', *, *, #59299, .F. ) ;
#5342 = AXIS2_PLACEMENT_3D ( 'NONE', #63389, #9578, #4304 ) ;
#5343 = CARTESIAN_POINT ( 'NONE',  ( -34.74023699876256899, 11.17830703027882677, 4.119991731420149073 ) ) ;
#5344 = ORIENTED_EDGE ( 'NONE', *, *, #35996, .F. ) ;
#5345 = LINE ( 'NONE', #25777, #10448 ) ;
#5346 = VERTEX_POINT ( 'NONE', #26674 ) ;
#5347 = CARTESIAN_POINT ( 'NONE',  ( 41.49663191311347532, 50.03028622612080767, 40.00000000000003553 ) ) ;
#5348 = CARTESIAN_POINT ( 'NONE',  ( 116.9226937574463392, 33.22232883683771121, 87.37277608428736642 ) ) ;
#5349 = CARTESIAN_POINT ( 'NONE',  ( -31.90315521289063128, -56.64813493366051489, 170.0000000000000000 ) ) ;
#5350 = CARTESIAN_POINT ( 'NONE',  ( -13.90880002535191373, -35.72171433227753568, 13.32819299319724848 ) ) ;
#5351 = CARTESIAN_POINT ( 'NONE',  ( 137.4031600461561027, 44.79620770172218869, -50.13600223372191778 ) ) ;
#5352 = CARTESIAN_POINT ( 'NONE',  ( -55.05276343752909440, 15.72344139423348786, -77.06087458892358200 ) ) ;
#5353 = DIRECTION ( 'NONE',  ( -0.000000000000000000, -0.000000000000000000, -1.000000000000000000 ) ) ;
#5354 = DIRECTION ( 'NONE',  ( 1.000000000000000000, 0.000000000000000000, 0.000000000000000000 ) ) ;
#5355 = EDGE_LOOP ( 'NONE', ( #29578, #35095, #48562, #52524 ) ) ;
#5356 = VERTEX_POINT ( 'NONE', #10485 ) ;
#5357 = CARTESIAN_POINT ( 'NONE',  ( 36.09469435220862010, 9.015003538710470110, 57.50936519207515829 ) ) ;
#5358 = CARTESIAN_POINT ( 'NONE',  ( 173.7956935488108741, 72.91723771116217279, 92.27808959496401542 ) ) ;
#5359 = B_SPLINE_CURVE_WITH_KNOTS ( 'NONE', 3,
 ( #54404, #32625, #32970, #33334, #27683, #54052, #60037, #17119, #44204, #22415, #11855, #55112, #16782, #65689, #10818, #26656, #69552, #6229, #54758, #42816, #38957, #16449, #21370, #38241, #22762, #27335, #49126, #6589, #16093, #64285, #37901, #1310, #58999, #17477, #43161, #32285, #53717, #5539, #59348, #11159, #39986, #45954, #67420, #39641, #50883, #51243 ),
 .UNSPECIFIED., .F., .F.,
 ( 4, 2, 2, 2, 2, 2, 2, 2, 2, 2, 2, 2, 2, 2, 2, 2, 2, 2, 2, 2, 2, 2, 4 ),
 ( 6.938893903907228378E-18, 0.001615199098318937949, 0.003230398196637868959, 0.004037997745797339451, 0.004845597294956811678, 0.006460796393275753530, 0.007268395942435259584, 0.008075995491594763903, 0.009691194589913741317, 0.01049879413907324130, 0.01130639368823274302, 0.01211399323739224473, 0.01292159278655174819, 0.01453679188487075509, 0.01615199098318976373, 0.01695959053234924810, 0.01776719008150873594, 0.01938238917982776019, 0.02099758827814678791, 0.02180518782730633473, 0.02261278737646588155, 0.02422798647478491621, 0.02584318557310394740 ),
 .UNSPECIFIED. ) ;
#5360 = FACE_OUTER_BOUND ( 'NONE', #36717, .T. ) ;
#5361 = CARTESIAN_POINT ( 'NONE',  ( 68.75860316153080021, 15.11750091268465113, -92.06867044945352063 ) ) ;
#5362 = ORIENTED_EDGE ( 'NONE', *, *, #32620, .F. ) ;
#5363 = CARTESIAN_POINT ( 'NONE',  ( 88.98064924903390249, 21.30386569031177402, 17.49345524372335703 ) ) ;
#5364 = CARTESIAN_POINT ( 'NONE',  ( 184.9757174666826813, 84.09845285279330085, -23.29565043318131146 ) ) ;
#5365 = CARTESIAN_POINT ( 'NONE',  ( 209.6642862813004911, 115.2127693334914085, 4.225474144247091779 ) ) ;
#5366 = AXIS2_PLACEMENT_3D ( 'NONE', #65979, #17774, #7580 ) ;
#5367 = CARTESIAN_POINT ( 'NONE',  ( -177.1540936177023298, 91.73126115633630207, -48.55048610981354784 ) ) ;
#5368 = DIRECTION ( 'NONE',  ( 0.000000000000000000, 0.9997420440737085912, 0.02271222823333339524 ) ) ;
#5369 = CARTESIAN_POINT ( 'NONE',  ( 26.53820682833769951, -51.95411367369387534, 27.58472315868180402 ) ) ;
#5370 = FACE_BOUND ( 'NONE', #67995, .T. ) ;
#5371 = B_SPLINE_CURVE_WITH_KNOTS ( 'NONE', 3,
 ( #67885, #45727, #46066, #18647, #19333, #3505, #2817, #23925, #56980, #40786, #41141, #18994, #40445, #28863, #51358, #61210, #29204, #67536, #61891, #8445, #13712, #35165, #62243, #55938, #56625, #3170, #55578, #14059, #7408, #50312, #35520, #8797, #30246, #51697, #24974, #46405, #19679, #62607, #14414, #2131, #23583, #66855, #45023, #66506 ),
 .UNSPECIFIED., .F., .F.,
 ( 4, 2, 2, 2, 2, 2, 2, 2, 2, 2, 2, 2, 2, 2, 2, 2, 2, 2, 2, 2, 2, 4 ),
 ( 0.02638217555535139064, 0.02805347641364859881, 0.02972477727194580352, 0.03139607813024301169, 0.03306737898854021640, 0.03390302941768884304, 0.03473867984683746968, 0.03640998070513472989, 0.03724563113428334959, 0.03808128156343197623, 0.03891693199258059593, 0.03975258242172921563, 0.04058823285087784227, 0.04142388328002646197, 0.04225953370917508167, 0.04309518413832370831, 0.04476648499662094771, 0.04643778585491818711, 0.04810908671321541957, 0.04978038757151265897, 0.05145168842980989143, 0.05312298928810713083 ),
 .UNSPECIFIED. ) ;
#5372 = DIRECTION ( 'NONE',  ( 1.000000000000000000, 0.000000000000000000, 0.000000000000000000 ) ) ;
#5373 = VECTOR ( 'NONE', #9109, 1000.000000000000000 ) ;
#5374 =( REPRESENTATION_RELATIONSHIP ('NONE','NONE', #40274, #60409 ) REPRESENTATION_RELATIONSHIP_WITH_TRANSFORMATION ( #26106 )SHAPE_REPRESENTATION_RELATIONSHIP( ) );
#5375 = VERTEX_POINT ( 'NONE', #11173 ) ;
#5376 = VECTOR ( 'NONE', #24854, 1000.000000000000227 ) ;
#5377 = CARTESIAN_POINT ( 'NONE',  ( 55.76286625948333864, -170.0000000000000000, -95.00000000000133582 ) ) ;
#5378 = CARTESIAN_POINT ( 'NONE',  ( 36.61292551086603453, 65.40035471292272007, 41.38025477438755928 ) ) ;
#5379 = CARTESIAN_POINT ( 'NONE',  ( 0.000000000000000000, 9.237604307034020579, 0.000000000000000000 ) ) ;
#5380 = CYLINDRICAL_SURFACE ( 'NONE', #54519, 7.500000000000013323 ) ;
#5381 = CARTESIAN_POINT ( 'NONE',  ( 152.8558173410470147, 54.14978343559395313, 15.99724100256723780 ) ) ;
#5382 = CARTESIAN_POINT ( 'NONE',  ( -15.32772194461970194, 8.507097118773966571, 91.57259910632232902 ) ) ;
#5383 = ORIENTED_EDGE ( 'NONE', *, *, #25327, .T. ) ;
#5384 = CARTESIAN_POINT ( 'NONE',  ( -417.6627218934913230, 179.4906275429376308, 111.5502958579881749 ) ) ;
#5385 = CARTESIAN_POINT ( 'NONE',  ( -5.000000000000026645, -10.55634918610403439, 85.00100000000000477 ) ) ;
#5386 = ADVANCED_FACE ( 'NONE', ( #37216 ), #43179, .T. ) ;
#5387 = VERTEX_POINT ( 'NONE', #64656 ) ;
#5388 = VECTOR ( 'NONE', #1458, 1000.000000000000000 ) ;
#5389 = EDGE_LOOP ( 'NONE', ( #16285, #24039, #36941, #57316 ) ) ;
#5390 = CARTESIAN_POINT ( 'NONE',  ( 33.62702447824805319, 8.740302253715633185, 86.30590074997479633 ) ) ;
#5391 = LINE ( 'NONE', #69408, #29896 ) ;
#5392 = EDGE_CURVE ( 'NONE', #66440, #11134, #64302, .T. ) ;
#5393 = CARTESIAN_POINT ( 'NONE',  ( 102.8111940033034273, 25.59308899183601937, 38.15290668819717013 ) ) ;
#5394 = ORIENTED_EDGE ( 'NONE', *, *, #8361, .T. ) ;
#5395 = DIRECTION ( 'NONE',  ( 0.000000000000000000, 0.000000000000000000, -1.000000000000000000 ) ) ;
#5396 = EDGE_CURVE ( 'NONE', #8866, #12095, #27008, .T. ) ;
#5397 = CARTESIAN_POINT ( 'NONE',  ( 32.67604596315971577, 7.629767358313817915, -19.60289529770304995 ) ) ;
#5398 = CARTESIAN_POINT ( 'NONE',  ( 173.9405361758638264, 73.05302209498819366, -41.42269835059776284 ) ) ;
#5399 = DIRECTION ( 'NONE',  ( 0.000000000000000000, -1.000000000000000000, 0.000000000000000000 ) ) ;
#5400 = CARTESIAN_POINT ( 'NONE',  ( 93.08533330311594511, 21.72562315962721513, 33.36257394385762609 ) ) ;
#5401 = ORIENTED_EDGE ( 'NONE', *, *, #14159, .F. ) ;
#5402 = CARTESIAN_POINT ( 'NONE',  ( -48.71337292867760738, 14.10768470390589435, -38.70095378530758978 ) ) ;
#5403 = DIRECTION ( 'NONE',  ( 1.000000000000000000, 0.000000000000000000, 0.000000000000000000 ) ) ;
#5405 = EDGE_CURVE ( 'NONE', #34747, #44455, #54167, .T. ) ;
#5404 = CARTESIAN_POINT ( 'NONE',  ( 24.91130694661013578, 3.250319586706704733, 0.000000000000000000 ) ) ;
#5406 = CARTESIAN_POINT ( 'NONE',  ( 149.4165763529819344, 225.8585178651493663, 138.9999999999999716 ) ) ;
#5407 = CARTESIAN_POINT ( 'NONE',  ( -31.43908319763710679, -170.0000000000000000, -69.66174795566553257 ) ) ;
#5409 = ORIENTED_EDGE ( 'NONE', *, *, #63357, .T. ) ;
#5408 = CARTESIAN_POINT ( 'NONE',  ( -29.87147652227455552, 68.79592317125366208, 133.5802547743875550 ) ) ;
#5410 = VERTEX_POINT ( 'NONE', #41821 ) ;
#5411 = ORIENTED_EDGE ( 'NONE', *, *, #10375, .T. ) ;
#5412 = DIRECTION ( 'NONE',  ( 1.000000000000000000, 1.850550996349095901E-16, 1.228197773518735191E-20 ) ) ;
#5413 = CARTESIAN_POINT ( 'NONE',  ( -165.9072201026428957, 80.88235209323546826, 89.92767665983485870 ) ) ;
#5414 = CARTESIAN_POINT ( 'NONE',  ( -31.43908319763710679, -170.0000000000000000, -15.97264677473816974 ) ) ;
#5415 = CARTESIAN_POINT ( 'NONE',  ( 0.000000000000000000, 0.000000000000000000, 41.38025477438755928 ) ) ;
#5416 = DIRECTION ( 'NONE',  ( -0.7071067811865473507, 6.441404958702665783E-16, 0.7071067811865477948 ) ) ;
#5417 = CARTESIAN_POINT ( 'NONE',  ( 6.375108774214766072E-14, 31.11269837220806167, 2.000000000000001776 ) ) ;
#5418 = CIRCLE ( 'NONE', #24575, 299.9999999999999432 ) ;
#5419 = CARTESIAN_POINT ( 'NONE',  ( 151.1607415860635228, 52.90668588398089867, -74.55516125840486552 ) ) ;
#5420 = DIRECTION ( 'NONE',  ( 0.000000000000000000, 0.000000000000000000, 1.000000000000000000 ) ) ;
#5421 = ORIENTED_EDGE ( 'NONE', *, *, #32183, .T. ) ;
#5422 = CARTESIAN_POINT ( 'NONE',  ( -153.6931187576189188, 67.81270084382356345, -48.54057641887556684 ) ) ;
#5423 = ORIENTED_EDGE ( 'NONE', *, *, #38504, .T. ) ;
#5424 = ORIENTED_EDGE ( 'NONE', *, *, #44321, .T. ) ;
#5425 = VECTOR ( 'NONE', #3154, 1000.000000000000000 ) ;
#5426 = CARTESIAN_POINT ( 'NONE',  ( 69.48877314113910586, 15.30784187978995448, -12.58006891014075812 ) ) ;
#5427 = CARTESIAN_POINT ( 'NONE',  ( -79.61235761536671873, 23.76245710489568808, -50.07082761529047588 ) ) ;
#5428 = CARTESIAN_POINT ( 'NONE',  ( 117.6070629920123025, 32.44042087193796675, 89.33694317982141797 ) ) ;
#5429 = CARTESIAN_POINT ( 'NONE',  ( -154.6085044440278864, 69.98390342970672862, 5.873012740166642764 ) ) ;
#5430 = VECTOR ( 'NONE', #47117, 1000.000000000000000 ) ;
#5431 = FACE_OUTER_BOUND ( 'NONE', #59546, .T. ) ;
#5432 = DIRECTION ( 'NONE',  ( 1.000000000000000000, 0.000000000000000000, 0.000000000000000000 ) ) ;
#5433 = CARTESIAN_POINT ( 'NONE',  ( -152.2429173757935530, 67.87244971895253798, 84.90521448722901710 ) ) ;
#5434 = ORIENTED_EDGE ( 'NONE', *, *, #7493, .F. ) ;
#5435 = VERTEX_POINT ( 'NONE', #48109 ) ;
#5436 = EDGE_LOOP ( 'NONE', ( #5744, #64775 ) ) ;
#5437 = CARTESIAN_POINT ( 'NONE',  ( -10.23402954931276554, 7.059791383763807993, 17.87799841423737490 ) ) ;
#5438 = CARTESIAN_POINT ( 'NONE',  ( -109.0191069781766657, 36.33811634972921922, 94.99999999999866418 ) ) ;
#5439 = LINE ( 'NONE', #43057, #22524 ) ;
#5440 = CARTESIAN_POINT ( 'NONE',  ( -153.5002794404626627, 67.64160439471096709, -21.82117646152210000 ) ) ;
#5441 = ORIENTED_EDGE ( 'NONE', *, *, #53962, .F. ) ;
#5442 = CARTESIAN_POINT ( 'NONE',  ( -64.18058723658653264, 10.37664328995176888, 170.0000000000000000 ) ) ;
#5443 = DIRECTION ( 'NONE',  ( -0.000000000000000000, -0.000000000000000000, -1.000000000000000000 ) ) ;
#5444 = EDGE_CURVE ( 'NONE', #24127, #27835, #16111, .T. ) ;
#5445 = CARTESIAN_POINT ( 'NONE',  ( -68.11501976657811497, -31.41506934893937952, 170.0000000000000000 ) ) ;
#5446 = DIRECTION ( 'NONE',  ( 1.000000000000000000, 0.000000000000000000, 0.000000000000000000 ) ) ;
#5447 = DIRECTION ( 'NONE',  ( 0.000000000000000000, 0.000000000000000000, 1.000000000000000000 ) ) ;
#5448 = CARTESIAN_POINT ( 'NONE',  ( -442.6627218934913799, 394.9999999999998295, -132.7581352960343679 ) ) ;
#5449 = CARTESIAN_POINT ( 'NONE',  ( 21.75684465274324353, 6.764994602232766496, 68.92719249320558106 ) ) ;
#5450 = DIRECTION ( 'NONE',  ( 1.000000000000000000, 6.217248937900876626E-15, 0.000000000000000000 ) ) ;
#5451 = CARTESIAN_POINT ( 'NONE',  ( 9.823983574062868485, 6.382904402091121199, -74.43691175599163046 ) ) ;
#5452 = EDGE_LOOP ( 'NONE', ( #67645, #57659, #47326, #4085 ) ) ;
#5453 = CARTESIAN_POINT ( 'NONE',  ( -8.000000000000000000, 1.572549600175613627, -0.06894455525513029648 ) ) ;
#5454 = ITEM_DEFINED_TRANSFORMATION ( 'NONE', 'NONE', #34331,  #66832 ) ;
#5455 = CARTESIAN_POINT ( 'NONE',  ( 173.9288990958749537, 71.66475105971929338, 39.13067012050992588 ) ) ;
#5456 = CARTESIAN_POINT ( 'NONE',  ( -125.8938041572051105, 46.49392987655492959, -49.91370389823397602 ) ) ;
#5457 = DIRECTION ( 'NONE',  ( -0.04486483035050447404, -0.9989930665413151445, 0.000000000000000000 ) ) ;
#5458 = CARTESIAN_POINT ( 'NONE',  ( 55.51637278631174155, 12.08345311280958789, -70.57488892405791603 ) ) ;
#5459 = ORIENTED_EDGE ( 'NONE', *, *, #48172, .F. ) ;
#5460 = VERTEX_POINT ( 'NONE', #31954 ) ;
#5461 = EDGE_CURVE ( 'NONE', #17220, #64271, #10143, .T. ) ;
#5462 = CARTESIAN_POINT ( 'NONE',  ( -24.94151142167917001, 8.614613465433025752, -19.75076858682908920 ) ) ;
#5463 = CARTESIAN_POINT ( 'NONE',  ( 200.4574930424076058, 102.3536505870638393, 16.06672283762458875 ) ) ;
#5464 = ADVANCED_FACE ( 'NONE', ( #53384 ), #63275, .T. ) ;
#5465 = VERTEX_POINT ( 'NONE', #273 ) ;
#5466 = VERTEX_POINT ( 'NONE', #31603 ) ;
#5467 = CARTESIAN_POINT ( 'NONE',  ( 111.1767565371974626, 29.31586421952252408, 56.49927049809659252 ) ) ;
#5468 = ORIENTED_EDGE ( 'NONE', *, *, #11176, .F. ) ;
#5469 = CARTESIAN_POINT ( 'NONE',  ( 116.0822834687217266, 32.80169113915575707, 68.68829875601142021 ) ) ;
#5470 = CARTESIAN_POINT ( 'NONE',  ( 4.165045035621077751, -64.88046627338039229, 0.000000000000000000 ) ) ;
#5471 = AXIS2_PLACEMENT_3D ( 'NONE', #2293, #57141, #30065 ) ;
#5472 = CARTESIAN_POINT ( 'NONE',  ( 135.6793972494603224, 43.71805072851434204, 56.56519963210866564 ) ) ;
#5473 = DIRECTION ( 'NONE',  ( 1.000000000000000000, 0.000000000000000000, 0.000000000000000000 ) ) ;
#5474 = EDGE_CURVE ( 'NONE', #40228, #3230, #51002, .T. ) ;
#5475 = CARTESIAN_POINT ( 'NONE',  ( -95.86612279493098754, 29.64021615886203165, 41.91453243627326941 ) ) ;
#5476 = STYLED_ITEM ( 'NONE', ( #48551 ), #63846 ) ;
#5477 = CARTESIAN_POINT ( 'NONE',  ( 93.08533330311593090, 21.72562315962721158, -47.17107782753343770 ) ) ;
#5478 = FACE_OUTER_BOUND ( 'NONE', #49318, .T. ) ;
#5479 = ORIENTED_EDGE ( 'NONE', *, *, #19013, .F. ) ;
#5480 = EDGE_LOOP ( 'NONE', ( #45183, #46394, #64906, #1077 ) ) ;
#5481 = CARTESIAN_POINT ( 'NONE',  ( -125.4433371161043596, 46.19736518073187881, -8.069153307770243089 ) ) ;
#5482 = FACE_BOUND ( 'NONE', #19895, .T. ) ;
#5483 = EDGE_CURVE ( 'NONE', #40273, #57346, #32640, .T. ) ;
#5484 = CARTESIAN_POINT ( 'NONE',  ( -146.7404675333698378, 63.17262273741975065, -35.33834636302898957 ) ) ;
#5485 = CARTESIAN_POINT ( 'NONE',  ( -165.6208371326873703, 80.58821715390999429, -69.35434424568703093 ) ) ;
#5487 = EDGE_LOOP ( 'NONE', ( #6115, #65095, #7510, #30011 ) ) ;
#5486 = CARTESIAN_POINT ( 'NONE',  ( -149.0782809666403637, 63.81577337591402710, -49.81283053149199702 ) ) ;
#5488 = CARTESIAN_POINT ( 'NONE',  ( 59.94652978725889625, 13.01168383647461901, 17.31598363014413522 ) ) ;
#5489 = EDGE_CURVE ( 'NONE', #34109, #59711, #68551, .T. ) ;
#5490 = EDGE_CURVE ( 'NONE', #63292, #51274, #27269, .T. ) ;
#5491 = EDGE_LOOP ( 'NONE', ( #5106, #24890, #59631, #12168 ) ) ;
#5492 = LINE ( 'NONE', #24635, #69443 ) ;
#5493 = CARTESIAN_POINT ( 'NONE',  ( 31.22608597448339651, 41.16111765196011163, 26.66469066592269144 ) ) ;
#5494 = CARTESIAN_POINT ( 'NONE',  ( 82.74007713545064746, 18.13042311233562032, -22.89437781078106582 ) ) ;
#5495 = CARTESIAN_POINT ( 'NONE',  ( 86.62931800182293784, 19.42108912189599579, -62.66611478937537782 ) ) ;
#5496 = CARTESIAN_POINT ( 'NONE',  ( 76.57571471437145760, 0.000000000000000000, -30.00000000000000000 ) ) ;
#5497 = FACE_BOUND ( 'NONE', #67109, .T. ) ;
#5498 = CARTESIAN_POINT ( 'NONE',  ( -95.05546640093039912, 29.25972325950975517, -71.43887970864732040 ) ) ;
#5499 = EDGE_LOOP ( 'NONE', ( #1520, #5685, #65376, #32229 ) ) ;
#5500 = ORIENTED_EDGE ( 'NONE', *, *, #38822, .T. ) ;
#5501 = CARTESIAN_POINT ( 'NONE',  ( 0.000000000000000000, -6.928203230275505220, -4.000000000000007105 ) ) ;
#5502 = CARTESIAN_POINT ( 'NONE',  ( 9.290502160020464473, 6.379616279862538875, 33.76109296599172183 ) ) ;
#5503 = CARTESIAN_POINT ( 'NONE',  ( -37.04655464516844177, 53.85410457537858520, 3.125053320693551875E-16 ) ) ;
#5504 = AXIS2_PLACEMENT_3D ( 'NONE', #28343, #51459, #6548 ) ;
#5505 = DIRECTION ( 'NONE',  ( -0.000000000000000000, -0.000000000000000000, -1.000000000000000000 ) ) ;
#5506 = CARTESIAN_POINT ( 'NONE',  ( 104.4006536356074122, 27.36759527624478849, -74.99636480049218790 ) ) ;
#5507 = CARTESIAN_POINT ( 'NONE',  ( -72.78270026377325053, 21.23376443558121096, -64.78274740210713389 ) ) ;
#5508 = DIRECTION ( 'NONE',  ( -1.000000000000000000, 0.000000000000000000, 0.000000000000000000 ) ) ;
#5509 = CARTESIAN_POINT ( 'NONE',  ( -119.5404913382140109, 43.63271406506962080, 34.12591518711677452 ) ) ;
#5510 = DIRECTION ( 'NONE',  ( 0.000000000000000000, -0.000000000000000000, -1.000000000000000000 ) ) ;
#5511 = VERTEX_POINT ( 'NONE', #34038 ) ;
#5512 = CARTESIAN_POINT ( 'NONE',  ( -109.7647482398635503, 36.74843029291200480, -15.12249450503182935 ) ) ;
#5513 = ORIENTED_EDGE ( 'NONE', *, *, #56243, .F. ) ;
#5514 = CARTESIAN_POINT ( 'NONE',  ( -14.32241591711282247, 7.401556312061832621, -39.16318076575544893 ) ) ;
#5515 = CARTESIAN_POINT ( 'NONE',  ( -84.79701208522806155, 24.75216251823110269, 87.27508272618359797 ) ) ;
#5516 = CARTESIAN_POINT ( 'NONE',  ( 6.375108774214766072E-14, 31.11269837220806167, 85.00100000000000477 ) ) ;
#5517 = CARTESIAN_POINT ( 'NONE',  ( 149.9552318559267121, 52.03645904563055780, -16.75648080528598172 ) ) ;
#5518 = CARTESIAN_POINT ( 'NONE',  ( 32.03384598935271299, 8.576372641735996893, 12.03241481110506328 ) ) ;
#5519 = AXIS2_PLACEMENT_3D ( 'NONE', #49067, #10758, #32225 ) ;
#5520 = CARTESIAN_POINT ( 'NONE',  ( -95.52093927227217307, 30.58993121475388577, -66.09890349134650478 ) ) ;
#5521 = CARTESIAN_POINT ( 'NONE',  ( 188.9999999999999432, -57.00000000000007816, 72.99999999999998579 ) ) ;
#5522 = VECTOR ( 'NONE', #44921, 1000.000000000000000 ) ;
#5523 = VERTEX_POINT ( 'NONE', #49490 ) ;
#5524 = DIRECTION ( 'NONE',  ( 0.000000000000000000, 0.000000000000000000, 1.000000000000000000 ) ) ;
#5525 = CARTESIAN_POINT ( 'NONE',  ( -32.68347998332510684, -12.52158680757305298, 30.00000000000000000 ) ) ;
#5527 = ORIENTED_EDGE ( 'NONE', *, *, #40906, .T. ) ;
#5526 = EDGE_CURVE ( 'NONE', #15204, #59881, #42001, .T. ) ;
#5528 = FACE_OUTER_BOUND ( 'NONE', #23837, .T. ) ;
#5529 = CARTESIAN_POINT ( 'NONE',  ( 12.46490660984525789, 7.423426948220651411, -63.13552371036534794 ) ) ;
#5530 = DIRECTION ( 'NONE',  ( 0.000000000000000000, -0.000000000000000000, -1.000000000000000000 ) ) ;
#5531 = CARTESIAN_POINT ( 'NONE',  ( 45.35146934743634972, 10.27620685439441850, -65.37128321836291889 ) ) ;
#5532 = CARTESIAN_POINT ( 'NONE',  ( 283.3053295232375035, -21.67655155662104249, 3.765949955696215046 ) ) ;
#5533 = CARTESIAN_POINT ( 'NONE',  ( 412.3372781065085633, 179.4906275429376024, 111.5502958579881749 ) ) ;
#5534 = CARTESIAN_POINT ( 'NONE',  ( 94.12422088577032753, 23.19200960350636365, 90.45949129094441332 ) ) ;
#5535 = EDGE_CURVE ( 'NONE', #52890, #16495, #50210, .T. ) ;
#5536 = EDGE_LOOP ( 'NONE', ( #5362, #49166, #56506, #37143 ) ) ;
#5537 = CARTESIAN_POINT ( 'NONE',  ( 681.0906130828457208, 908.9915846175174465, 550.6483088597211690 ) ) ;
#5538 = CARTESIAN_POINT ( 'NONE',  ( 8.000000000000000000, -3.098204225878180118, -9.184209322808124298 ) ) ;
#5539 = CARTESIAN_POINT ( 'NONE',  ( -129.6165111262477296, 48.99406349865701316, 4.760252937733464584 ) ) ;
#5540 = CARTESIAN_POINT ( 'NONE',  ( -105.8879245385188739, 35.79035667534147791, 71.45643182967125995 ) ) ;
#5541 = CARTESIAN_POINT ( 'NONE',  ( -179.9997297618090784, 95.12611598520665268, 94.99999999999866418 ) ) ;
#5542 = ORIENTED_EDGE ( 'NONE', *, *, #16575, .T. ) ;
#5543 = CYLINDRICAL_SURFACE ( 'NONE', #36905, 7.500000000000013323 ) ;
#5544 = CARTESIAN_POINT ( 'NONE',  ( -3.868882431147342871, 6.665575841812233726, -22.44979996978308634 ) ) ;
#5545 = EDGE_CURVE ( 'NONE', #17804, #45879, #49845, .T. ) ;
#5546 = CARTESIAN_POINT ( 'NONE',  ( -156.8280449791103877, 70.64611012537017132, 90.24344703734034567 ) ) ;
#5547 = ADVANCED_FACE ( 'NONE', ( #6604 ), #28049, .F. ) ;
#5548 = SHAPE_REPRESENTATION ( 'driven pulley', ( #66832 ), #59007 ) ;
#5549 = CARTESIAN_POINT ( 'NONE',  ( 139.7928618793172859, 45.12615179300589574, 41.60106151571937261 ) ) ;
#5550 = EDGE_CURVE ( 'NONE', #63750, #6327, #16795, .T. ) ;
#5551 = ORIENTED_EDGE ( 'NONE', *, *, #32245, .T. ) ;
#5552 = DIRECTION ( 'NONE',  ( -0.000000000000000000, -0.000000000000000000, -1.000000000000000000 ) ) ;
#5553 = CARTESIAN_POINT ( 'NONE',  ( 82.12277968641507186, 18.98848723477813394, 16.38247655469762520 ) ) ;
#5554 = CARTESIAN_POINT ( 'NONE',  ( 209.9518228411288874, 0.000000000000000000, 31.43423095485942298 ) ) ;
#5555 = DIRECTION ( 'NONE',  ( 0.000000000000000000, 0.000000000000000000, -1.000000000000000000 ) ) ;
#5556 = EDGE_LOOP ( 'NONE', ( #119, #63196, #51370, #42776 ) ) ;
#5557 = CARTESIAN_POINT ( 'NONE',  ( 0.000000000000000000, 0.000000000000000000, 0.000000000000000000 ) ) ;
#5558 = ORIENTED_EDGE ( 'NONE', *, *, #20467, .F. ) ;
#5559 = CARTESIAN_POINT ( 'NONE',  ( -109.0297561673456386, 36.34391931706015555, -39.23453111580145958 ) ) ;
#5560 = CARTESIAN_POINT ( 'NONE',  ( 70.50372867914784081, 14.53505678900968867, -69.57474953973002130 ) ) ;
#5561 = CARTESIAN_POINT ( 'NONE',  ( -58.76005811686688673, 15.70653557534867595, 44.35498545959168837 ) ) ;
#5562 = CIRCLE ( 'NONE', #21286, 242.4895526022646379 ) ;
#5564 = VERTEX_POINT ( 'NONE', #55478 ) ;
#5563 = CARTESIAN_POINT ( 'NONE',  ( 0.000000000000000000, 0.000000000000000000, 161.3522585083728700 ) ) ;
#5565 = CARTESIAN_POINT ( 'NONE',  ( 158.3604774538084712, 58.34594647925810307, 44.36981973328110485 ) ) ;
#5566 = LINE ( 'NONE', #11886, #48501 ) ;
#5567 = EDGE_CURVE ( 'NONE', #17255, #41880, #27700, .T. ) ;
#5568 = EDGE_CURVE ( 'NONE', #9677, #15508, #53224, .T. ) ;
#5569 = AXIS2_PLACEMENT_3D ( 'NONE', #8247, #67349, #57472 ) ;
#5570 = DIRECTION ( 'NONE',  ( -0.000000000000000000, 1.000000000000000000, -0.000000000000000000 ) ) ;
#5571 = EDGE_LOOP ( 'NONE', ( #45400, #6325, #17133, #21972 ) ) ;
#5572 = EDGE_CURVE ( 'NONE', #49668, #69259, #2134, .T. ) ;
#5573 = CARTESIAN_POINT ( 'NONE',  ( -142.1451960690342560, 59.45765244009941597, -94.47710424355705072 ) ) ;
#5574 = DIRECTION ( 'NONE',  ( -1.000000000000000000, -0.000000000000000000, -0.000000000000000000 ) ) ;
#5575 = CARTESIAN_POINT ( 'NONE',  ( -172.7116702014380110, 86.67317892691259829, 45.82169460664105287 ) ) ;
#5576 = CARTESIAN_POINT ( 'NONE',  ( 126.7877523219523823, 38.47018873135926498, 66.41478141192939688 ) ) ;
#5577 = ORIENTED_EDGE ( 'NONE', *, *, #19439, .F. ) ;
#5578 = EDGE_LOOP ( 'NONE', ( #1690, #69065, #8868, #53921 ) ) ;
#5579 = EDGE_LOOP ( 'NONE', ( #67998, #13822, #65351, #59763 ) ) ;
#5580 = CARTESIAN_POINT ( 'NONE',  ( -24.07306039673040132, -53.14126562679988552, 27.58472315868179692 ) ) ;
#5581 = CARTESIAN_POINT ( 'NONE',  ( -107.7677210873465583, 36.80113675102404613, 6.039296874237338741 ) ) ;
#5582 = CARTESIAN_POINT ( 'NONE',  ( 48.11816970607237209, 43.69944786994017250, 170.0000000000000000 ) ) ;
#5583 = CARTESIAN_POINT ( 'NONE',  ( -109.6894192603215998, 36.70681195612597492, 90.49915744604948031 ) ) ;
#5584 = FACE_OUTER_BOUND ( 'NONE', #8189, .T. ) ;
#5585 = CARTESIAN_POINT ( 'NONE',  ( -7.825402957745087207, 6.891034867348159842, -35.41807073194381417 ) ) ;
#5586 = DIRECTION ( 'NONE',  ( -0.000000000000000000, -0.000000000000000000, 1.000000000000000000 ) ) ;
#5587 = ORIENTED_EDGE ( 'NONE', *, *, #8252, .T. ) ;
#5588 = LINE ( 'NONE', #59736, #24033 ) ;
#5589 = ORIENTED_EDGE ( 'NONE', *, *, #45424, .T. ) ;
#5590 = FACE_OUTER_BOUND ( 'NONE', #17343, .T. ) ;
#5591 = CARTESIAN_POINT ( 'NONE',  ( 210.0292194063021896, 113.9511645670926185, -65.39028459387030523 ) ) ;
#5592 = CARTESIAN_POINT ( 'NONE',  ( -84.49322488516129681, 0.000000000000000000, 43.58025477438756212 ) ) ;
#5593 = CARTESIAN_POINT ( 'NONE',  ( -447.6627218934913799, 370.0000000000002274, -141.4497041420117966 ) ) ;
#5594 = LINE ( 'NONE', #27394, #28903 ) ;
#5595 = CYLINDRICAL_SURFACE ( 'NONE', #50220, 7.500000000000013323 ) ;
#5596 = CARTESIAN_POINT ( 'NONE',  ( -422.6627218934914936, 399.9999999999998863, -141.4497041420118535 ) ) ;
#5597 = CIRCLE ( 'NONE', #40459, 5.000000000000018652 ) ;
#5598 = CARTESIAN_POINT ( 'NONE',  ( -15.67984581960975632, -63.08044415722883969, 170.0000000000000000 ) ) ;
#5599 = ORIENTED_EDGE ( 'NONE', *, *, #35041, .T. ) ;
#5600 = LINE ( 'NONE', #27054, #48745 ) ;
#5601 = DIRECTION ( 'NONE',  ( 0.000000000000000000, 0.000000000000000000, 1.000000000000000000 ) ) ;
#5602 = VERTEX_POINT ( 'NONE', #34738 ) ;
#5603 = ORIENTED_EDGE ( 'NONE', *, *, #8812, .T. ) ;
#5604 = CARTESIAN_POINT ( 'NONE',  ( -27.70185240367227308, 10.02491413133431486, -76.16892411189579093 ) ) ;
#5605 = CARTESIAN_POINT ( 'NONE',  ( 58.09607305250595033, 11.58497620657515981, -48.90344441354543648 ) ) ;
#5606 = DIRECTION ( 'NONE',  ( -0.000000000000000000, 1.000000000000000000, -0.000000000000000000 ) ) ;
#5607 = EDGE_CURVE ( 'NONE', #68856, #56615, #2720, .T. ) ;
#5608 = CARTESIAN_POINT ( 'NONE',  ( -45.00000000000002132, -20.00000000000000355, 2.000000000000015543 ) ) ;
#5609 = ORIENTED_EDGE ( 'NONE', *, *, #42487, .F. ) ;
#5610 = ORIENTED_EDGE ( 'NONE', *, *, #11689, .T. ) ;
#5611 = B_SPLINE_CURVE_WITH_KNOTS ( 'NONE', 3,
 ( #17562, #55188, #40404, #49911, #61851, #35130, #34104, #28824, #66469, #18260, #13001, #42133, #15406, #25282, #57285, #19292, #46721, #41453, #10122, #24597, #19643, #40749, #3815, #4504, #15061, #46029, #9787, #63252, #36172, #20330, #68194, #62206, #14022, #9099, #36515, #36864, #57631, #31249, #58305, #9441, #25965, #68525, #30897, #3470, #63597 ),
 .UNSPECIFIED., .F., .F.,
 ( 4, 2, 2, 2, 2, 2, 2, 2, 1, 2, 2, 2, 2, 2, 2, 2, 2, 2, 2, 2, 2, 2, 4 ),
 ( 1.734723475976807094E-18, 0.001467747071934227387, 0.002201620607901337828, 0.002935494143868448268, 0.004403241215802658308, 0.005870988287736867914, 0.007338735359671077520, 0.008072608895638166276, 0.008806482431605255901, 0.009540355967572345525, 0.01027422950353943515, 0.01174197657547365430, 0.01247585011144078382, 0.01320972364740791508, 0.01467747071934213422, 0.01541134425530924466, 0.01614521779127635337, 0.01761296486321053956, 0.01908071193514472574, 0.01981458547111182578, 0.02054845900707892581, 0.02201620607901315363, 0.02348395315094737451 ),
 .UNSPECIFIED. ) ;
#5612 = VECTOR ( 'NONE', #45632, 1000.000000000000000 ) ;
#5613 = CARTESIAN_POINT ( 'NONE',  ( -128.9843070188472325, 49.78011598923033887, 31.27109394439055734 ) ) ;
#5614 = EDGE_LOOP ( 'NONE', ( #66785, #60378, #47106, #7908 ) ) ;
#5615 = CARTESIAN_POINT ( 'NONE',  ( 205.1049299651095055, 106.9023875785545954, 17.36317014830576966 ) ) ;
#5616 = CARTESIAN_POINT ( 'NONE',  ( 0.3194001229792609031, 3.115132258397515397, -7.999999999999996447 ) ) ;
#5617 = CARTESIAN_POINT ( 'NONE',  ( 58.09607305250594322, 11.58497620657515803, 58.47475794830932472 ) ) ;
#5618 = DIRECTION ( 'NONE',  ( -1.000000000000000000, 0.000000000000000000, 0.000000000000000000 ) ) ;
#5619 = ADVANCED_FACE ( 'NONE', ( #24182 ), #19228, .F. ) ;
#5620 = SURFACE_STYLE_FILL_AREA ( #37284 ) ;
#5621 = DIRECTION ( 'NONE',  ( -0.000000000000000000, 1.000000000000000000, -0.000000000000000000 ) ) ;
#5622 = EDGE_CURVE ( 'NONE', #66616, #58443, #6222, .T. ) ;
#5623 = CARTESIAN_POINT ( 'NONE',  ( -149.5074843970971017, 65.50121172469319220, 3.876270649435370252 ) ) ;
#5624 = EDGE_LOOP ( 'NONE', ( #24042, #23283 ) ) ;
#5625 = EDGE_CURVE ( 'NONE', #25903, #20206, #65615, .T. ) ;
#5626 = VERTEX_POINT ( 'NONE', #67105 ) ;
#5627 = DIRECTION ( 'NONE',  ( 0.000000000000000000, 0.000000000000000000, 1.000000000000000000 ) ) ;
#5628 = DIRECTION ( 'NONE',  ( -1.000000000000000000, 0.000000000000000000, 0.000000000000000000 ) ) ;
#5629 = CARTESIAN_POINT ( 'NONE',  ( -8.000000000000000000, 4.618802153516996079, -9.500000000000000000 ) ) ;
#5630 = CARTESIAN_POINT ( 'NONE',  ( 89.99999999999998579, 0.000000000000000000, 7.000000000000000000 ) ) ;
#5631 = CARTESIAN_POINT ( 'NONE',  ( 68.95451040317568925, 14.12887482153123742, 41.91971055821581871 ) ) ;
#5632 = AXIS2_PLACEMENT_3D ( 'NONE', #45663, #56916, #51293 ) ;
#5633 = CARTESIAN_POINT ( 'NONE',  ( 19.27211902843862035, 7.644382812444131758, 84.55400850847075844 ) ) ;
#5634 = ADVANCED_FACE ( 'NONE', ( #18897, #62505, #55840 ), #7660, .T. ) ;
#5635 = VERTEX_POINT ( 'NONE', #42417 ) ;
#5636 = CARTESIAN_POINT ( 'NONE',  ( 450.2085304802404266, 0.000000000000000000, -250.0000000000000000 ) ) ;
#5637 = ORIENTED_EDGE ( 'NONE', *, *, #14756, .T. ) ;
#5638 = CARTESIAN_POINT ( 'NONE',  ( -76.77329340382468104, 21.60914066444074422, 45.19114480031347370 ) ) ;
#5639 = ORIENTED_EDGE ( 'NONE', *, *, #36868, .F. ) ;
#5640 = VERTEX_POINT ( 'NONE', #9729 ) ;
#5641 = DIRECTION ( 'NONE',  ( -0.9639628606958512425, -0.2660368455666826670, 0.000000000000000000 ) ) ;
#5642 = CARTESIAN_POINT ( 'NONE',  ( 429.8372781065087338, 400.0000000000067075, -123.9497041420121235 ) ) ;
#5643 = CARTESIAN_POINT ( 'NONE',  ( 37.76691715686636996, 29.79383981485516841, -24.99999999999999645 ) ) ;
#5644 = ORIENTED_EDGE ( 'NONE', *, *, #6081, .T. ) ;
#5645 = EDGE_CURVE ( 'NONE', #52559, #6514, #31915, .T. ) ;
#5646 = DIRECTION ( 'NONE',  ( 0.000000000000000000, 0.000000000000000000, 1.000000000000000000 ) ) ;
#5647 = CARTESIAN_POINT ( 'NONE',  ( 69.35866309798977625, 15.27376159675663203, 41.32255262261386264 ) ) ;
#5648 = CARTESIAN_POINT ( 'NONE',  ( -27.00000000000000355, 26.99999999999999289, 0.000000000000000000 ) ) ;
#5649 = CARTESIAN_POINT ( 'NONE',  ( 23.93060502292675196, 7.646171227524815706, 0.000000000000000000 ) ) ;
#5650 = CARTESIAN_POINT ( 'NONE',  ( -173.1211646369891355, -170.0000000000000000, -7.867406574286299303 ) ) ;
#5651 = CARTESIAN_POINT ( 'NONE',  ( -29.04258984626623530, 9.210213971636683539, 30.60543872389602171 ) ) ;
#5652 = CARTESIAN_POINT ( 'NONE',  ( -146.5230751932349165, 62.99205605665035534, -76.05256278801076064 ) ) ;
#5653 = VERTEX_POINT ( 'NONE', #15687 ) ;
#5654 = B_SPLINE_CURVE_WITH_KNOTS ( 'NONE', 3,
 ( #66629, #56062, #13500, #13159, #29327, #50776 ),
 .UNSPECIFIED., .F., .F.,
 ( 4, 2, 4 ),
 ( 0.03218932648122794365, 0.06469831129177422424, 0.09720729610232048401 ),
 .UNSPECIFIED. ) ;
#5655 = FACE_BOUND ( 'NONE', #7861, .T. ) ;
#5656 = CARTESIAN_POINT ( 'NONE',  ( -0.5780275525703881812, 6.527356703336900878, -71.70849423231535980 ) ) ;
#5657 = CARTESIAN_POINT ( 'NONE',  ( -180.6158171975815776, 97.47361786002630879, 64.84187048422768385 ) ) ;
#5658 = CARTESIAN_POINT ( 'NONE',  ( 44.74620900418437941, 37.43371647374308964, 27.58472315868181468 ) ) ;
#5659 = DIRECTION ( 'NONE',  ( 0.4738686624729965824, 0.8805955318567391110, 0.000000000000000000 ) ) ;
#5660 = CARTESIAN_POINT ( 'NONE',  ( -81.00768240531205322, 24.30850321514432366, 3.944436707959213084 ) ) ;
#5661 = FACE_OUTER_BOUND ( 'NONE', #23819, .T. ) ;
#5662 = LINE ( 'NONE', #55603, #65111 ) ;
#5663 = DIRECTION ( 'NONE',  ( -1.850169831522831466E-16, 1.000000000000000000, 1.110223024625156294E-16 ) ) ;
#5664 = CARTESIAN_POINT ( 'NONE',  ( 66.72974708835174340, 13.56459745268606376, 3.934091007171761412 ) ) ;
#5665 = CARTESIAN_POINT ( 'NONE',  ( -83.53167274806556009, 25.32068190668985608, 70.49144734754210617 ) ) ;
#5666 = CARTESIAN_POINT ( 'NONE',  ( 87.59078297315399197, 20.81577753000345155, -23.93050775134987163 ) ) ;
#5667 = ORIENTED_EDGE ( 'NONE', *, *, #47398, .F. ) ;
#5668 = CARTESIAN_POINT ( 'NONE',  ( -37.39246151129641760, 11.66872370876247800, 15.45975854931544546 ) ) ;
#5669 = ORIENTED_EDGE ( 'NONE', *, *, #18594, .F. ) ;
#5670 = CARTESIAN_POINT ( 'NONE',  ( 0.000000000000000000, 0.000000000000000000, 40.00000000000003553 ) ) ;
#5671 = EDGE_LOOP ( 'NONE', ( #40192, #35934, #36153, #9226 ) ) ;
#5672 = CARTESIAN_POINT ( 'NONE',  ( 79.54836217416615796, 18.17815803851260625, -72.65076421043085020 ) ) ;
#5673 = CARTESIAN_POINT ( 'NONE',  ( 105.4784409469015003, 27.83725412974951396, 84.96893711368112179 ) ) ;
#5674 = CARTESIAN_POINT ( 'NONE',  ( -142.9756886485677398, 60.11539876121631210, 61.37017874365231052 ) ) ;
#5675 = CARTESIAN_POINT ( 'NONE',  ( 66.30567821786759453, 13.45988234822861429, -9.631894463744744783 ) ) ;
#5676 = AXIS2_PLACEMENT_3D ( 'NONE', #13153, #67320, #40560 ) ;
#5677 = CARTESIAN_POINT ( 'NONE',  ( -5.066666666666671759, 0.000000000000000000, -11.86666666666666536 ) ) ;
#5678 = PRODUCT_DEFINITION_SHAPE ( 'NONE', 'NONE',  #69613 ) ;
#5679 = PRODUCT_RELATED_PRODUCT_CATEGORY ( 'part', '', ( #26510 ) ) ;
#5680 = CARTESIAN_POINT ( 'NONE',  ( -52.68206656346369243, 15.09776187114412593, -62.44128804069127625 ) ) ;
#5681 = MECHANICAL_DESIGN_GEOMETRIC_PRESENTATION_REPRESENTATION (  '', ( #61878 ), #13587 ) ;
#5682 = CARTESIAN_POINT ( 'NONE',  ( 0.000000000000000000, 35.00000000000000000, -22.00000000000000355 ) ) ;
#5683 = FACE_OUTER_BOUND ( 'NONE', #3275, .T. ) ;
#5684 = EDGE_LOOP ( 'NONE', ( #29474, #21632, #30647, #66868, #13949, #638, #26967, #48733, #66037, #63383, #37601 ) ) ;
#5685 = ORIENTED_EDGE ( 'NONE', *, *, #46043, .F. ) ;
#5686 = EDGE_CURVE ( 'NONE', #38444, #28906, #48354, .T. ) ;
#5687 = CARTESIAN_POINT ( 'NONE',  ( 39.40195752203892710, 9.424259417798131366, 56.75838489642694640 ) ) ;
#5688 = AXIS2_PLACEMENT_3D ( 'NONE', #62242, #23924, #39755 ) ;
#5689 = PRESENTATION_STYLE_ASSIGNMENT (( #49641 ) ) ;
#5690 = EDGE_CURVE ( 'NONE', #17818, #30657, #5124, .T. ) ;
#5691 = CARTESIAN_POINT ( 'NONE',  ( 133.1078597672272394, 42.14624897798367442, -89.71241211332299770 ) ) ;
#5692 = PRODUCT_DEFINITION_CONTEXT ( 'detailed design', #47573, 'design' ) ;
#5693 = VECTOR ( 'NONE', #9339, 999.9999999999998863 ) ;
#5694 = CARTESIAN_POINT ( 'NONE',  ( 63.83262973450582223, 13.89724595143439245, -89.44344974266579129 ) ) ;
#5695 = ORIENTED_EDGE ( 'NONE', *, *, #26987, .T. ) ;
#5696 = CARTESIAN_POINT ( 'NONE',  ( 87.11239765416381431, 20.65008247340817604, 17.86753698201565399 ) ) ;
#5697 = CARTESIAN_POINT ( 'NONE',  ( -8.320652113663527416, 6.923290556636831461, 71.96013162991091860 ) ) ;
#5698 = CARTESIAN_POINT ( 'NONE',  ( 211.3710169359754047, 117.8057917113659698, 6.428924886512843884 ) ) ;
#5699 = SHAPE_REPRESENTATION_RELATIONSHIP ( 'NONE' , 'NONE' ,  #52783, #13951 ) ;
#5700 = DIRECTION ( 'NONE',  ( 0.000000000000000000, 0.000000000000000000, 1.000000000000000000 ) ) ;
#5701 = DIRECTION ( 'NONE',  ( -0.000000000000000000, -0.000000000000000000, -1.000000000000000000 ) ) ;
#5702 = DIRECTION ( 'NONE',  ( -1.850169831522831466E-16, 1.000000000000000000, 1.110223024625156294E-16 ) ) ;
#5703 = CARTESIAN_POINT ( 'NONE',  ( 108.3860478234812064, 21.48288568141374810, -4.743631494308838015 ) ) ;
#5704 = FACE_OUTER_BOUND ( 'NONE', #22344, .T. ) ;
#5705 = EDGE_CURVE ( 'NONE', #59383, #9126, #28554, .T. ) ;
#5706 = VERTEX_POINT ( 'NONE', #32217 ) ;
#5707 = ADVANCED_FACE ( 'NONE', ( #63877 ), #46518, .T. ) ;
#5708 = FACE_OUTER_BOUND ( 'NONE', #25869, .T. ) ;
#5709 = CARTESIAN_POINT ( 'NONE',  ( 88.98064924903394513, 21.30386569031177046, -36.19564593720401291 ) ) ;
#5710 = B_SPLINE_CURVE_WITH_KNOTS ( 'NONE', 3,
 ( #45960, #58478, #57808, #40335, #4676, #68695, #9628, #31086, #56167, #41971, #2710, #52526, #7984, #29436, #3062, #15245, #45616, #61782, #47239, #24523, #8338, #13605, #35062, #29782, #68370, #36706, #58152, #9969, #31421, #52852, #22246, #21540, #10638, #48599, #48259, #33513, #59512, #38780 ),
 .UNSPECIFIED., .F., .F.,
 ( 4, 2, 2, 2, 2, 2, 2, 2, 2, 2, 2, 2, 2, 2, 2, 2, 2, 2, 4 ),
 ( 0.02546424207107604240, 0.02703543426729210220, 0.02782103036540016852, 0.02860662646350823485, 0.03017781865972442995, 0.03174901085594063199, 0.03332020305215682709, 0.03489139524837302220, 0.03646258744458922424, 0.03724818354269731485, 0.03803377964080539853, 0.03881937573891348914, 0.03960497183702157975, 0.04117616403323776098, 0.04274735622945394914, 0.04431854842567013730, 0.04588974062188632547, 0.04746093281810251363, 0.05060331721053488302 ),
 .UNSPECIFIED. ) ;
#5711 = CARTESIAN_POINT ( 'NONE',  ( -30.62628708973388569, 68.47330165179126027, 170.0000000000000000 ) ) ;
#5712 = LINE ( 'NONE', #26491, #61329 ) ;
#5713 = LINE ( 'NONE', #48956, #45316 ) ;
#5714 = CARTESIAN_POINT ( 'NONE',  ( -149.5074843970971301, -170.0000000000000000, -42.31283053149197571 ) ) ;
#5715 = ORIENTED_EDGE ( 'NONE', *, *, #45581, .T. ) ;
#5716 = CARTESIAN_POINT ( 'NONE',  ( 60.63507185982729197, 12.13307030573223955, 17.58473668013007796 ) ) ;
#5717 = CARTESIAN_POINT ( 'NONE',  ( -55.53469534616548486, 14.81076603075806197, 57.16187836339482686 ) ) ;
#5718 = EDGE_LOOP ( 'NONE', ( #31667, #35976, #1683, #31606, #32399, #42424, #44453, #22662, #11941 ) ) ;
#5719 = VERTEX_POINT ( 'NONE', #63531 ) ;
#5720 = CARTESIAN_POINT ( 'NONE',  ( 46.15699773797793881, 10.40307558352962580, 94.42940818875426601 ) ) ;
#5721 = CARTESIAN_POINT ( 'NONE',  ( -3.841371665203041630E-11, 0.000000000000000000, 10.00000000000000000 ) ) ;
#5722 = CARTESIAN_POINT ( 'NONE',  ( 106.0171289417044136, 26.97542621030656207, 43.31196261650080714 ) ) ;
#5723 = ORIENTED_EDGE ( 'NONE', *, *, #10930, .F. ) ;
#5724 = CARTESIAN_POINT ( 'NONE',  ( -62.54085973597663184, 16.81797209566546059, -70.05212444181948683 ) ) ;
#5725 = VECTOR ( 'NONE', #2109, 1000.000000000000000 ) ;
#5726 = CARTESIAN_POINT ( 'NONE',  ( 32.15641333221389431, 7.577415570152253643, -14.32268503797624604 ) ) ;
#5727 = CARTESIAN_POINT ( 'NONE',  ( 173.6737675136087091, 72.80308721038093722, -44.91943839559014151 ) ) ;
#5728 = CARTESIAN_POINT ( 'NONE',  ( -22.50000000000003197, 207.5000000000000284, 0.000000000000000000 ) ) ;
#5729 = CARTESIAN_POINT ( 'NONE',  ( 46.66904755831210139, -9.150666335777657423E-14, 2.000000000000001776 ) ) ;
#5730 = AXIS2_PLACEMENT_3D ( 'NONE', #1861, #22599, #60236 ) ;
#5731 = ORIENTED_EDGE ( 'NONE', *, *, #3644, .T. ) ;
#5732 = CIRCLE ( 'NONE', #61882, 4.999999999999997335 ) ;
#5733 = VECTOR ( 'NONE', #47729, 1000.000000000000000 ) ;
#5734 = CARTESIAN_POINT ( 'NONE',  ( -47.80251179448167420, 13.89045662648308976, -40.73231631372835437 ) ) ;
#5735 = DIRECTION ( 'NONE',  ( 0.000000000000000000, 0.000000000000000000, 1.000000000000000000 ) ) ;
#5736 = CARTESIAN_POINT ( 'NONE',  ( 12.03162622199372933, 7.415834979634796653, 44.01070327993329556 ) ) ;
#5737 = DIRECTION ( 'NONE',  ( 0.000000000000000000, 0.000000000000000000, -1.000000000000000000 ) ) ;
#5738 = FACE_OUTER_BOUND ( 'NONE', #46135, .T. ) ;
#5739 = DIRECTION ( 'NONE',  ( 0.000000000000000000, 0.000000000000000000, 1.000000000000000000 ) ) ;
#5741 = ORIENTED_EDGE ( 'NONE', *, *, #35158, .F. ) ;
#5740 = FACE_OUTER_BOUND ( 'NONE', #30395, .T. ) ;
#5742 = ORIENTED_EDGE ( 'NONE', *, *, #56209, .F. ) ;
#5743 = VECTOR ( 'NONE', #25173, 1000.000000000000000 ) ;
#5744 = ORIENTED_EDGE ( 'NONE', *, *, #30818, .T. ) ;
#5745 = CARTESIAN_POINT ( 'NONE',  ( -14.55390976651257162, 7.422979442794209959, -19.39586497985030888 ) ) ;
#5746 = CARTESIAN_POINT ( 'NONE',  ( -172.7861182744952941, 88.26094898553817814, 84.50184874253974954 ) ) ;
#5747 = CARTESIAN_POINT ( 'NONE',  ( 46.76173513940573656, -58.63736118510165340, 0.000000000000000000 ) ) ;
#5748 = DIRECTION ( 'NONE',  ( 0.000000000000000000, -0.000000000000000000, -1.000000000000000000 ) ) ;
#5749 = CARTESIAN_POINT ( 'NONE',  ( -56.96436614829624290, 16.24647150911285820, -49.97265642726394219 ) ) ;
#5750 = CARTESIAN_POINT ( 'NONE',  ( -14.33576511807126685, 8.413127487936186810, -12.31783428727917951 ) ) ;
#5751 = CARTESIAN_POINT ( 'NONE',  ( 156.5909039492010209, 56.96742803863248383, -62.96873488960130771 ) ) ;
#5752 = CARTESIAN_POINT ( 'NONE',  ( 23.03864809957654458, 6.841061756139156458, -14.23981446476811108 ) ) ;
#5753 = ORIENTED_EDGE ( 'NONE', *, *, #24618, .F. ) ;
#5754 = CARTESIAN_POINT ( 'NONE',  ( -156.1462053606562392, 70.02140399657012892, -38.81290798880835524 ) ) ;
#5755 = ORIENTED_EDGE ( 'NONE', *, *, #6077, .F. ) ;
#5756 = ORIENTED_EDGE ( 'NONE', *, *, #23587, .T. ) ;
#5757 = CARTESIAN_POINT ( 'NONE',  ( 183.2136430849848239, 6.000000000000000000, -9.435653166495541200 ) ) ;
#5758 = DIRECTION ( 'NONE',  ( -0.000000000000000000, -0.000000000000000000, -1.000000000000000000 ) ) ;
#5759 = CARTESIAN_POINT ( 'NONE',  ( 311.8713128290285113, 2.000000000000001776, 346.5826552340383842 ) ) ;
#5760 = CARTESIAN_POINT ( 'NONE',  ( -149.7268278745401631, 65.68859631971236013, 3.876270649435373361 ) ) ;
#5761 = EDGE_CURVE ( 'NONE', #56407, #18138, #10395, .T. ) ;
#5762 = DIRECTION ( 'NONE',  ( 0.000000000000000000, 0.000000000000000000, 1.000000000000000000 ) ) ;
#5763 = CARTESIAN_POINT ( 'NONE',  ( 22.52576749827963809, 6.809805260274345073, 34.18343812378846280 ) ) ;
#5764 = CARTESIAN_POINT ( 'NONE',  ( -156.8955115693747757, 72.07810529072631311, 90.57258849307295634 ) ) ;
#5765 = VERTEX_POINT ( 'NONE', #20272 ) ;
#5766 = ORIENTED_EDGE ( 'NONE', *, *, #50193, .F. ) ;
#5767 = EDGE_CURVE ( 'NONE', #59702, #34459, #42070, .T. ) ;
#5768 = EDGE_LOOP ( 'NONE', ( #13742, #63676, #32036, #66265 ) ) ;
#5769 = CARTESIAN_POINT ( 'NONE',  ( -154.7826623253030505, 70.14150242829521176, -20.80520620324490366 ) ) ;
#5770 = EDGE_CURVE ( 'NONE', #4597, #14754, #14650, .T. ) ;
#5771 = LINE ( 'NONE', #58542, #12839 ) ;
#5772 = APPLICATION_CONTEXT ( 'automotive_design' ) ;
#5773 = EDGE_CURVE ( 'NONE', #295, #34394, #69137, .T. ) ;
#5774 = CIRCLE ( 'NONE', #15927, 5.000000000000004441 ) ;
#5775 = CARTESIAN_POINT ( 'NONE',  ( -31.93184248720558216, 9.672312402099825235, 72.06100499665288339 ) ) ;
#5776 = CARTESIAN_POINT ( 'NONE',  ( -155.1355020251929488, 69.10372769512068203, -20.45101316398983116 ) ) ;
#5777 = ORIENTED_EDGE ( 'NONE', *, *, #40759, .F. ) ;
#5778 = CARTESIAN_POINT ( 'NONE',  ( 188.4365915667139006, 87.87248959723056885, 65.16220424045542359 ) ) ;
#5779 = CARTESIAN_POINT ( 'NONE',  ( -156.4841188516943191, 70.33041971808555104, 62.29890658327479258 ) ) ;
#5780 = VECTOR ( 'NONE', #26931, 1000.000000000000000 ) ;
#5781 = CARTESIAN_POINT ( 'NONE',  ( 278.7032261419851693, -21.46110313769844424, -4.839973237437567910 ) ) ;
#5782 =( LENGTH_UNIT ( ) NAMED_UNIT ( * ) SI_UNIT ( .MILLI., .METRE. ) );
#5783 = CARTESIAN_POINT ( 'NONE',  ( -4.999999999999936939, 36.11269837220805812, 0.000000000000000000 ) ) ;
#5784 = CARTESIAN_POINT ( 'NONE',  ( -83.51052366780668024, 24.22613130369187218, -36.88447773562854337 ) ) ;
#5785 = CARTESIAN_POINT ( 'NONE',  ( 23.03578842369135060, 6.840884649289439068, 62.41390671365888210 ) ) ;
#5786 = DIRECTION ( 'NONE',  ( -0.000000000000000000, 0.000000000000000000, -1.000000000000000000 ) ) ;
#5787 = CARTESIAN_POINT ( 'NONE',  ( 8.000000000000007105, 249.8719672152120381, -95.00000000000133582 ) ) ;
#5788 = CIRCLE ( 'NONE', #2448, 4.999999999999990230 ) ;
#5789 = EDGE_CURVE ( 'NONE', #9160, #55620, #187, .T. ) ;
#5790 = ORIENTED_EDGE ( 'NONE', *, *, #62827, .F. ) ;
#5791 = DIRECTION ( 'NONE',  ( 1.000000000000000000, -0.000000000000000000, 0.000000000000000000 ) ) ;
#5792 = ITEM_DEFINED_TRANSFORMATION ( 'NONE', 'NONE', #53415,  #66832 ) ;
#5793 = VECTOR ( 'NONE', #13746, 1000.000000000000000 ) ;
#5794 = CARTESIAN_POINT ( 'NONE',  ( 174.6176230994777825, 72.30829341023250834, 40.64789474444607009 ) ) ;
#5795 = CARTESIAN_POINT ( 'NONE',  ( -132.2199390322348904, 50.80243550247269013, -38.35397204430816487 ) ) ;
#5796 = CARTESIAN_POINT ( 'NONE',  ( 39.40195752203892710, 8.409560354027393103, -62.46436805589144114 ) ) ;
#5797 = CARTESIAN_POINT ( 'NONE',  ( 164.6046919270428930, -170.0000000000000000, -95.00000000000133582 ) ) ;
#5798 = ORIENTED_EDGE ( 'NONE', *, *, #18197, .T. ) ;
#5799 = EDGE_LOOP ( 'NONE', ( #66770, #47407, #20325 ) ) ;
#5800 = CARTESIAN_POINT ( 'NONE',  ( -25.81763596640060143, 8.735969132042855634, -20.94358112585581821 ) ) ;
#5801 = CARTESIAN_POINT ( 'NONE',  ( 174.0956405974778534, 71.82022412301054715, 93.22721250497485812 ) ) ;
#5802 = ORIENTED_EDGE ( 'NONE', *, *, #53599, .F. ) ;
#5803 = ORIENTED_EDGE ( 'NONE', *, *, #46794, .F. ) ;
#5804 = CARTESIAN_POINT ( 'NONE',  ( 184.9757174666826813, 84.09845285279330085, 30.39345074774602651 ) ) ;
#5805 = CYLINDRICAL_SURFACE ( 'NONE', #5471, 5.000000000000004441 ) ;
#5806 = ORIENTED_EDGE ( 'NONE', *, *, #10304, .T. ) ;
#5807 = PLANE ( 'NONE',  #12101 ) ;
#5808 = CARTESIAN_POINT ( 'NONE',  ( 103.6830219322541353, 27.05818465022135655, -93.45235881085721985 ) ) ;
#5809 = CARTESIAN_POINT ( 'NONE',  ( 134.7708899521910837, 43.15864772107689618, 56.40727709478612439 ) ) ;
#5810 = CARTESIAN_POINT ( 'NONE',  ( -73.09185868250601459, 20.27574131633382493, -37.57414808074971546 ) ) ;
#5811 = CARTESIAN_POINT ( 'NONE',  ( 83.53262254759448524, 18.38732384439404655, -90.16803647247536446 ) ) ;
#5812 = CARTESIAN_POINT ( 'NONE',  ( 94.06703982324147262, 22.09435144471462920, -42.32417742623751167 ) ) ;
#5813 = CARTESIAN_POINT ( 'NONE',  ( -84.49322488516129681, 0.000000000000000000, 43.58025477438756212 ) ) ;
#5814 = ORIENTED_EDGE ( 'NONE', *, *, #59443, .T. ) ;
#5815 = ORIENTED_EDGE ( 'NONE', *, *, #50680, .T. ) ;
#5816 = CARTESIAN_POINT ( 'NONE',  ( -417.6627218934913230, 179.4906275429376308, 113.5502958579881749 ) ) ;
#5817 = DIRECTION ( 'NONE',  ( 0.000000000000000000, 0.000000000000000000, 1.000000000000000000 ) ) ;
#5818 = CARTESIAN_POINT ( 'NONE',  ( -142.9843132609582597, 60.12226089556227748, -38.60248188077854081 ) ) ;
#5819 = CARTESIAN_POINT ( 'NONE',  ( -168.0052514572427356, 83.06849406765627464, -63.56670774126097001 ) ) ;
#5821 = ORIENTED_EDGE ( 'NONE', *, *, #25287, .T. ) ;
#5820 = FACE_OUTER_BOUND ( 'NONE', #11195, .T. ) ;
#5822 = CARTESIAN_POINT ( 'NONE',  ( 59.08202327466405279, 12.82375733818953734, 16.85878258424966702 ) ) ;
#5823 = VECTOR ( 'NONE', #69312, 1000.000000000000000 ) ;
#5824 = ORIENTED_EDGE ( 'NONE', *, *, #31478, .T. ) ;
#5826 = ADVANCED_FACE ( 'NONE', ( #47678 ), #52283, .T. ) ;
#5825 = FACE_OUTER_BOUND ( 'NONE', #5988, .T. ) ;
#5827 = FACE_OUTER_BOUND ( 'NONE', #21085, .T. ) ;
#5828 = PLANE ( 'NONE',  #42178 ) ;
#5829 = CIRCLE ( 'NONE', #63150, 74.95140232871122521 ) ;
#5830 = VECTOR ( 'NONE', #23562, 1000.000000000000000 ) ;
#5831 = CARTESIAN_POINT ( 'NONE',  ( 136.3292018078239778, 42.93753790426541883, -23.76329299397318096 ) ) ;
#5832 = LINE ( 'NONE', #27288, #40983 ) ;
#5833 = FACE_OUTER_BOUND ( 'NONE', #31509, .T. ) ;
#5834 = CARTESIAN_POINT ( 'NONE',  ( -96.78198318406110445, 30.07417864442859212, 6.050221078145685105 ) ) ;
#5835 = CARTESIAN_POINT ( 'NONE',  ( -96.78198318406114709, 30.07417864442863475, -74.48343069324536714 ) ) ;
#5836 = ORIENTED_EDGE ( 'NONE', *, *, #11076, .F. ) ;
#5837 = VERTEX_POINT ( 'NONE', #64212 ) ;
#5838 = AXIS2_PLACEMENT_3D ( 'NONE', #65367, #38269, #54083 ) ;
#5839 = DIRECTION ( 'NONE',  ( 0.000000000000000000, 0.000000000000000000, 1.000000000000000000 ) ) ;
#5840 = CIRCLE ( 'NONE', #39560, 25.00000000000296296 ) ;
#5841 = DIRECTION ( 'NONE',  ( 1.000000000000000000, 0.000000000000000000, 0.000000000000000000 ) ) ;
#5842 = LINE ( 'NONE', #43818, #8720 ) ;
#5843 = DIRECTION ( 'NONE',  ( -1.000000000000000000, 0.000000000000000000, -0.000000000000000000 ) ) ;
#5844 = CARTESIAN_POINT ( 'NONE',  ( 103.9685899589048006, 27.18106603025992385, -74.38333352377321717 ) ) ;
#5845 = CARTESIAN_POINT ( 'NONE',  ( 79.19345177405118363, 17.01649702043280499, 38.22266187991689179 ) ) ;
#5846 = CYLINDRICAL_SURFACE ( 'NONE', #21, 7.500000000000013323 ) ;
#5847 = CARTESIAN_POINT ( 'NONE',  ( 46.51377856795993182, 10.46037936279324754, -40.68832589467017158 ) ) ;
#5848 = DIRECTION ( 'NONE',  ( 1.000000000000000000, -0.000000000000000000, 0.000000000000000000 ) ) ;
#5849 = ORIENTED_EDGE ( 'NONE', *, *, #61635, .F. ) ;
#5850 = CARTESIAN_POINT ( 'NONE',  ( -31.43908319763711390, 10.61114334766715928, 18.37190381572551701 ) ) ;
#5851 = EDGE_CURVE ( 'NONE', #62932, #32718, #68792, .T. ) ;
#5852 = ORIENTED_EDGE ( 'NONE', *, *, #18118, .T. ) ;
#5853 = CARTESIAN_POINT ( 'NONE',  ( -12.77647591501652613, 7.263973827022342178, -48.57332611465309924 ) ) ;
#5854 = DIRECTION ( 'NONE',  ( 0.000000000000000000, 0.000000000000000000, 1.000000000000000000 ) ) ;
#5855 = CARTESIAN_POINT ( 'NONE',  ( 88.98064924903393091, 21.30386569031177402, 71.18255642465075539 ) ) ;
#5856 = CARTESIAN_POINT ( 'NONE',  ( 157.4703587214989113, 57.65129005721575339, -24.27963370867398396 ) ) ;
#5857 = CARTESIAN_POINT ( 'NONE',  ( 412.3372781065085633, 179.4906275429376024, 113.5502958579881749 ) ) ;
#5858 = CARTESIAN_POINT ( 'NONE',  ( -99.98584758882481083, 32.75338129098887663, -76.51518145783863645 ) ) ;
#5859 = EDGE_CURVE ( 'NONE', #1836, #10264, #48023, .T. ) ;
#5860 = CARTESIAN_POINT ( 'NONE',  ( 114.9572297719016092, 32.24508028227645440, -91.26492051213512013 ) ) ;
#5861 = ORIENTED_EDGE ( 'NONE', *, *, #61188, .F. ) ;
#5862 = DIRECTION ( 'NONE',  ( 1.000000000000000000, 0.000000000000000000, 0.000000000000000000 ) ) ;
#5863 = DIRECTION ( 'NONE',  ( 0.000000000000000000, 0.000000000000000000, 1.000000000000000000 ) ) ;
#5864 = EDGE_LOOP ( 'NONE', ( #18136, #41745, #25263, #35049 ) ) ;
#5865 = CARTESIAN_POINT ( 'NONE',  ( 422.4999999999999432, 207.5000000000000284, 0.000000000000000000 ) ) ;
#5866 = DIRECTION ( 'NONE',  ( 0.000000000000000000, -0.000000000000000000, -1.000000000000000000 ) ) ;
#5867 = DIRECTION ( 'NONE',  ( -0.3754025596372949636, 0.9268618657695261165, 0.000000000000000000 ) ) ;
#5868 = CARTESIAN_POINT ( 'NONE',  ( 74.94097818310312675, 1.250000000000011546, 41.38025477438755928 ) ) ;
#5869 = CARTESIAN_POINT ( 'NONE',  ( -0.5751131641471373124, 6.527254166626918597, 39.55046635746396788 ) ) ;
#5870 = CARTESIAN_POINT ( 'NONE',  ( -106.6781182590523258, 35.07133425426472684, -63.26553636263061975 ) ) ;
#5871 = EDGE_CURVE ( 'NONE', #8192, #55258, #21304, .T. ) ;
#5872 = ORIENTED_EDGE ( 'NONE', *, *, #30906, .F. ) ;
#5873 = DIRECTION ( 'NONE',  ( 9.930814532437947919E-15, -2.943307516198506266E-15, 0.9999999999999997780 ) ) ;
#5874 = CARTESIAN_POINT ( 'NONE',  ( -190.6985136298601731, 109.1272424661242582, -19.71767969763411799 ) ) ;
#5876 = EDGE_CURVE ( 'NONE', #13372, #34620, #52620, .T. ) ;
#5875 = CARTESIAN_POINT ( 'NONE',  ( 7.484861546145031852, 64.56761454192836425, 170.0000000000000000 ) ) ;
#5877 = CARTESIAN_POINT ( 'NONE',  ( -166.2065256787326746, 81.19093426984588291, -39.29294834308091566 ) ) ;
#5878 = CARTESIAN_POINT ( 'NONE',  ( 15.55634918610396511, -46.66904755831214402, 2.000000000000001776 ) ) ;
#5879 = ORIENTED_EDGE ( 'NONE', *, *, #50038, .T. ) ;
#5880 = LINE ( 'NONE', #58315, #33558 ) ;
#5881 = VECTOR ( 'NONE', #1006, 1000.000000000000000 ) ;
#5882 = CARTESIAN_POINT ( 'NONE',  ( 25.09133896793782981, -1.250000000000021982, 0.000000000000000000 ) ) ;
#5883 = CARTESIAN_POINT ( 'NONE',  ( 197.3119541548905715, 98.33923235143191732, -18.29545015563770960 ) ) ;
#5884 = CIRCLE ( 'NONE', #20449, 8.000000000000000000 ) ;
#5885 = CARTESIAN_POINT ( 'NONE',  ( -156.1201442861361386, 69.99755458545364206, 88.35662595570710209 ) ) ;
#5886 = DIRECTION ( 'NONE',  ( 1.000000000000000000, 0.000000000000000000, 0.000000000000000000 ) ) ;
#5887 = ORIENTED_EDGE ( 'NONE', *, *, #64559, .T. ) ;
#5888 = DIRECTION ( 'NONE',  ( -0.000000000000000000, -1.000000000000000000, -0.000000000000000000 ) ) ;
#5889 = CARTESIAN_POINT ( 'NONE',  ( 79.63513233364427890, 18.20496177163925111, 7.648485935142918635 ) ) ;
#5890 = DIRECTION ( 'NONE',  ( -1.000000000000000000, 0.000000000000000000, 0.000000000000000000 ) ) ;
#5891 = CIRCLE ( 'NONE', #12648, 74.95140232871122521 ) ;
#5892 = ORIENTED_EDGE ( 'NONE', *, *, #10677, .T. ) ;
#5893 = CARTESIAN_POINT ( 'NONE',  ( 177.0027897064244087, 75.97676392242543386, 69.96163413657492924 ) ) ;
#5894 = EDGE_LOOP ( 'NONE', ( #28372, #66726, #22629, #16537 ) ) ;
#5895 = ORIENTED_EDGE ( 'NONE', *, *, #37393, .F. ) ;
#5896 = CARTESIAN_POINT ( 'NONE',  ( -71.96390573417174608, 19.88067451234326555, -12.36759105974787154 ) ) ;
#5897 = CARTESIAN_POINT ( 'NONE',  ( 204.6977192012829789, -170.0000000000000000, 29.20772073876942088 ) ) ;
#5899 = ORIENTED_EDGE ( 'NONE', *, *, #35205, .T. ) ;
#5898 = CARTESIAN_POINT ( 'NONE',  ( 154.6530827109543225, 56.75509330623210502, 17.01932198663618223 ) ) ;
#5900 = CARTESIAN_POINT ( 'NONE',  ( 163.7607557204680404, 62.71181783708028235, 41.02505403109415028 ) ) ;
#5901 = DIRECTION ( 'NONE',  ( -0.2225209339563184452, 0.9749279121818226201, 0.000000000000000000 ) ) ;
#5902 = CARTESIAN_POINT ( 'NONE',  ( -5.767955557622883589E-14, -31.11269837220806878, 85.00100000000000477 ) ) ;
#5903 = ORIENTED_EDGE ( 'NONE', *, *, #61323, .T. ) ;
#5904 = EDGE_CURVE ( 'NONE', #66023, #20436, #10747, .T. ) ;
#5905 = CARTESIAN_POINT ( 'NONE',  ( -148.7135390649993667, 64.82294617398349601, -88.50193171241927814 ) ) ;
#5906 = EDGE_CURVE ( 'NONE', #52737, #43093, #57568, .T. ) ;
#5907 = CARTESIAN_POINT ( 'NONE',  ( -34.51918258780365534, 10.11719938103014726, -22.81536398408823274 ) ) ;
#5908 = CARTESIAN_POINT ( 'NONE',  ( -179.5109681715918555, 96.11572638569522553, 34.35669452023326187 ) ) ;
#5909 = CARTESIAN_POINT ( 'NONE',  ( -38.84150381976581201, 10.92416363971239157, -70.89272716398475893 ) ) ;
#5910 = VERTEX_POINT ( 'NONE', #26248 ) ;
#5911 = EDGE_LOOP ( 'NONE', ( #25814, #22824, #25180, #69077 ) ) ;
#5912 = ORIENTED_EDGE ( 'NONE', *, *, #51572, .F. ) ;
#5913 = VECTOR ( 'NONE', #66847, 1000.000000000000000 ) ;
#5914 = CARTESIAN_POINT ( 'NONE',  ( -49.44946307590714696, 13.25037070100582426, 86.51077810379730693 ) ) ;
#5915 = CARTESIAN_POINT ( 'NONE',  ( -450.6627218934913230, 217.8591479523843475, 78.55029585798814651 ) ) ;
#5916 = CIRCLE ( 'NONE', #19450, 97.99999999999994316 ) ;
#5917 = CARTESIAN_POINT ( 'NONE',  ( -156.9252506979472628, 70.73559306219776488, -70.30158766110032786 ) ) ;
#5918 = LINE ( 'NONE', #16828, #32555 ) ;
#5919 = PLANE ( 'NONE',  #17971 ) ;
#5920 = EDGE_CURVE ( 'NONE', #23284, #45155, #59903, .T. ) ;
#5921 = CARTESIAN_POINT ( 'NONE',  ( -17.50000000000002842, 207.5000000000000284, 378.0000000000000000 ) ) ;
#5923 = CARTESIAN_POINT ( 'NONE',  ( 49.35747016781629526, 44.78219207638765909, 34.48241824007786249 ) ) ;
#5922 = CIRCLE ( 'NONE', #32905, 10.00000000000000000 ) ;
#5924 = EDGE_CURVE ( 'NONE', #6748, #46944, #15146, .T. ) ;
#5925 = EDGE_LOOP ( 'NONE', ( #43965, #40597, #32006 ) ) ;
#5926 = LINE ( 'NONE', #38296, #48690 ) ;
#5927 = EDGE_LOOP ( 'NONE', ( #13537, #18254, #49283, #3262 ) ) ;
#5928 = CONICAL_SURFACE ( 'NONE', #50897, 8.000000000000000000, 1.047197551196600296 ) ;
#5929 = CARTESIAN_POINT ( 'NONE',  ( 63.01563776193091826, -170.0000000000000000, 10.46841034875760279 ) ) ;
#5930 = CARTESIAN_POINT ( 'NONE',  ( 186.2651679807462131, 84.00458780104314371, 31.36535250390706153 ) ) ;
#5931 = EDGE_CURVE ( 'NONE', #43885, #57004, #38522, .T. ) ;
#5932 = DIRECTION ( 'NONE',  ( -0.9989930665413151445, 0.04486483035050446017, 0.000000000000000000 ) ) ;
#5933 = CARTESIAN_POINT ( 'NONE',  ( -71.22878586122430988, 19.62649588091172248, 12.07173733644329516 ) ) ;
#5934 = DIRECTION ( 'NONE',  ( 1.000000000000000000, 0.000000000000000000, 0.000000000000000000 ) ) ;
#5935 = LINE ( 'NONE', #43575, #29982 ) ;
#5936 = CIRCLE ( 'NONE', #53086, 8.000000000000000000 ) ;
#5937 = EDGE_CURVE ( 'NONE', #68965, #62166, #22348, .T. ) ;
#5938 = LINE ( 'NONE', #15816, #48381 ) ;
#5939 = DIRECTION ( 'NONE',  ( -0.000000000000000000, -0.000000000000000000, -1.000000000000000000 ) ) ;
#5940 = CARTESIAN_POINT ( 'NONE',  ( 26.99999999999999289, -30.00000000000000355, 0.000000000000000000 ) ) ;
#5941 = VERTEX_POINT ( 'NONE', #6522 ) ;
#5942 = DIRECTION ( 'NONE',  ( -0.000000000000000000, -0.000000000000000000, -1.000000000000000000 ) ) ;
#5943 = CYLINDRICAL_SURFACE ( 'NONE', #44202, 7.500000000000013323 ) ;
#5944 = VERTEX_POINT ( 'NONE', #17776 ) ;
#5945 = ORIENTED_EDGE ( 'NONE', *, *, #16520, .T. ) ;
#5946 = CARTESIAN_POINT ( 'NONE',  ( -84.96580414052107244, 24.82184094495578464, 41.99606300715279872 ) ) ;
#5947 = FACE_OUTER_BOUND ( 'NONE', #36620, .T. ) ;
#5948 = DIRECTION ( 'NONE',  ( 1.000000000000000000, 0.000000000000000000, 0.000000000000000000 ) ) ;
#5949 = LINE ( 'NONE', #17200, #47356 ) ;
#5950 = B_SPLINE_CURVE_WITH_KNOTS ( 'NONE', 3,
 ( #17168, #10861, #27378, #60082, #11902, #59040, #33382, #28077, #60445, #12262, #48136, #32330, #53758, #5581, #30435, #8988, #66093, #60785, #46602, #17886, #46957, #52230, #49883, #30098, #62449, #45921, #1707, #67389, #14263, #51206, #68419, #57173, #39342, #63137, #56832, #12608, #44613, #8645, #51883, #35370, #51553, #19531, #30786, #25520 ),
 .UNSPECIFIED., .F., .F.,
 ( 4, 2, 2, 2, 2, 2, 2, 2, 2, 2, 2, 2, 2, 2, 2, 2, 2, 2, 2, 2, 2, 4 ),
 ( 0.02477387709520257816, 0.02633314402883776828, 0.02711277749565536160, 0.02789241096247295146, 0.02945167789610816933, 0.03023131136292576265, 0.03101094482974335598, 0.03257021176337854262, 0.03334984523019612207, 0.03412947869701370152, 0.03568874563064885347, 0.03646837909746643291, 0.03724801256428400542, 0.03802764603110158487, 0.03880727949791916431, 0.04036654643155432320, 0.04192581336518948210, 0.04348508029882463405, 0.04504434723245979988, 0.04660361416609495183, 0.04816288109973011766, 0.04972214803336526961 ),
 .UNSPECIFIED. ) ;
#5951 = CARTESIAN_POINT ( 'NONE',  ( 133.8566784816069628, 41.42467568809809819, -9.178760341931967659 ) ) ;
#5952 = EDGE_CURVE ( 'NONE', #6104, #67779, #27617, .T. ) ;
#5953 = VERTEX_POINT ( 'NONE', #33957 ) ;
#5954 = VERTEX_POINT ( 'NONE', #64566 ) ;
#5955 = EDGE_CURVE ( 'NONE', #18015, #1535, #16375, .T. ) ;
#5956 = ADVANCED_FACE ( 'NONE', ( #64918 ), #16713, .F. ) ;
#5957 = CYLINDRICAL_SURFACE ( 'NONE', #23378, 500.0000000000000000 ) ;
#5958 = ORIENTED_EDGE ( 'NONE', *, *, #36362, .F. ) ;
#5959 = CARTESIAN_POINT ( 'NONE',  ( 36.09469435220862010, 9.015003538710468334, -23.02428657931588063 ) ) ;
#5960 = CARTESIAN_POINT ( 'NONE',  ( -149.0764453401867513, 65.13297611514538232, 30.72082123989904545 ) ) ;
#5961 = DIRECTION ( 'NONE',  ( 0.000000000000000000, 0.000000000000000000, -1.000000000000000000 ) ) ;
#5962 = CARTESIAN_POINT ( 'NONE',  ( -0.8863172752569253854, 7.545240277686255048, 67.33728230589369446 ) ) ;
#5963 = CARTESIAN_POINT ( 'NONE',  ( -28.14339584226772928, 10.09086145081589159, -89.75580143143783118 ) ) ;
#5964 = DIRECTION ( 'NONE',  ( -0.000000000000000000, -0.000000000000000000, -1.000000000000000000 ) ) ;
#5965 = AXIS2_PLACEMENT_3D ( 'NONE', #10715, #12124, #49383 ) ;
#5966 = FACE_OUTER_BOUND ( 'NONE', #56010, .T. ) ;
#5967 = EDGE_LOOP ( 'NONE', ( #34676, #50085, #29193, #40551 ) ) ;
#5968 = ORIENTED_EDGE ( 'NONE', *, *, #49778, .T. ) ;
#5969 = CARTESIAN_POINT ( 'NONE',  ( 63.01563776193091826, -170.0000000000000000, -43.22069083216975116 ) ) ;
#5970 = DIRECTION ( 'NONE',  ( -1.000000000000000000, -0.000000000000000000, -0.000000000000000000 ) ) ;
#5971 = VECTOR ( 'NONE', #26457, 1000.000000000000000 ) ;
#5972 = CARTESIAN_POINT ( 'NONE',  ( -169.8791831685530838, 83.59058982490282119, -8.589682762458334508 ) ) ;
#5973 = CARTESIAN_POINT ( 'NONE',  ( 140.4586216751744701, 45.55624550472996503, -73.93575597659268794 ) ) ;
#5974 = CARTESIAN_POINT ( 'NONE',  ( 70.51484748609223630, 14.53801151001411718, 36.80098285481733456 ) ) ;
#5975 = CIRCLE ( 'NONE', #56554, 125.0000000000000000 ) ;
#5976 = ORIENTED_EDGE ( 'NONE', *, *, #41471, .T. ) ;
#5977 = CARTESIAN_POINT ( 'NONE',  ( -66.50000000000000000, 8.143901214329899974E-15, 85.00000000000000000 ) ) ;
#5978 = ORIENTED_EDGE ( 'NONE', *, *, #5245, .F. ) ;
#5979 = CIRCLE ( 'NONE', #21708, 5.000000000000004441 ) ;
#5980 = CARTESIAN_POINT ( 'NONE',  ( -71.43874587651170316, 19.69883891272894516, 35.89975146121849292 ) ) ;
#5981 = ORIENTED_EDGE ( 'NONE', *, *, #61492, .F. ) ;
#5982 = VECTOR ( 'NONE', #10217, 999.9999999999998863 ) ;
#5983 = VECTOR ( 'NONE', #67059, 1000.000000000000000 ) ;
#5984 = ORIENTED_EDGE ( 'NONE', *, *, #33057, .F. ) ;
#5985 = DIRECTION ( 'NONE',  ( 0.4738686624730094610, -0.8805955318567321166, 0.000000000000000000 ) ) ;
#5986 = CARTESIAN_POINT ( 'NONE',  ( 92.53566308513174477, 21.52138666710686365, 15.01619406867864903 ) ) ;
#5987 = PLANE ( 'NONE',  #26082 ) ;
#5988 = EDGE_LOOP ( 'NONE', ( #52983, #7010, #65966, #3563 ) ) ;
#5989 = DIRECTION ( 'NONE',  ( 0.8584487936018728726, -0.5128992774058949156, 0.000000000000000000 ) ) ;
#5990 = DIRECTION ( 'NONE',  ( 0.6246950475544236214, 0.000000000000000000, 0.7808688094430308313 ) ) ;
#5991 = EDGE_CURVE ( 'NONE', #38832, #12486, #8955, .T. ) ;
#5992 = CARTESIAN_POINT ( 'NONE',  ( 152.1190604254710195, 53.60705199010335065, 31.64870937947464924 ) ) ;
#5993 = CARTESIAN_POINT ( 'NONE',  ( -180.3161328724957571, 97.10341277064809162, -40.07322758584183475 ) ) ;
#5994 = LINE ( 'NONE', #36987, #7817 ) ;
#5995 = FACE_OUTER_BOUND ( 'NONE', #41690, .T. ) ;
#5996 = PLANE ( 'NONE',  #19250 ) ;
#5997 = ORIENTED_EDGE ( 'NONE', *, *, #63943, .T. ) ;
#5998 = CARTESIAN_POINT ( 'NONE',  ( 135.6793972494602656, 43.71805072851428520, -77.65755332020975743 ) ) ;
#5999 = DIRECTION ( 'NONE',  ( 1.000000000000000000, 0.000000000000000000, 0.000000000000000000 ) ) ;
#6000 = ORIENTED_EDGE ( 'NONE', *, *, #47399, .F. ) ;
#6001 = FACE_BOUND ( 'NONE', #25507, .T. ) ;
#6002 = CARTESIAN_POINT ( 'NONE',  ( -5.416136198635858712, 6.745992685878683837, -76.86935474192905815 ) ) ;
#6003 = CARTESIAN_POINT ( 'NONE',  ( -180.6021503146988607, 97.45669259943417728, 65.78653073592644773 ) ) ;
#6004 = PLANE ( 'NONE',  #15849 ) ;
#6005 = CARTESIAN_POINT ( 'NONE',  ( -120.0051930351106648, 43.92079660368833061, -37.76205108401183708 ) ) ;
#6006 = CARTESIAN_POINT ( 'NONE',  ( -81.01931326044685022, 24.31309346877660005, 18.19902748808744875 ) ) ;
#6007 = FACE_OUTER_BOUND ( 'NONE', #40693, .T. ) ;
#6008 = CARTESIAN_POINT ( 'NONE',  ( -149.5074843970971017, 64.17983161892348676, 3.876270649435373361 ) ) ;
#6009 = EDGE_CURVE ( 'NONE', #21211, #2336, #24787, .T. ) ;
#6010 = CARTESIAN_POINT ( 'NONE',  ( -120.1346137380982384, 44.00127440773567855, -74.06905664438973247 ) ) ;
#6011 = CARTESIAN_POINT ( 'NONE',  ( 67.56108154898468854, 13.77276756375644595, 16.45415915286800157 ) ) ;
#6012 = CARTESIAN_POINT ( 'NONE',  ( 164.8942204024298235, 63.66138186734712434, 11.16733468916308247 ) ) ;
#6013 = CARTESIAN_POINT ( 'NONE',  ( 93.72059824125564376, 23.03897520779757357, -13.98440811075808377 ) ) ;
#6014 = ORIENTED_EDGE ( 'NONE', *, *, #39684, .F. ) ;
#6015 = AXIS2_PLACEMENT_3D ( 'NONE', #62685, #18728, #40188 ) ;
#6016 = CARTESIAN_POINT ( 'NONE',  ( -33.83721310978698682, 11.01869210665940635, 3.761447440691132904 ) ) ;
#6017 = VERTEX_POINT ( 'NONE', #40958 ) ;
#6018 = LINE ( 'NONE', #11295, #50880 ) ;
#6019 = EDGE_CURVE ( 'NONE', #54796, #68965, #27476, .T. ) ;
#6020 = CARTESIAN_POINT ( 'NONE',  ( 79.12879321038293767, 18.04902206524926811, -69.93020897591220830 ) ) ;
#6021 = CARTESIAN_POINT ( 'NONE',  ( 112.7929653408798174, 31.19474750060521728, 83.73979164330758351 ) ) ;
#6022 = CARTESIAN_POINT ( 'NONE',  ( -142.0070007485041401, 59.34878529741516928, 64.79586851560435434 ) ) ;
#6023 = DIRECTION ( 'NONE',  ( 0.000000000000000000, 0.000000000000000000, 1.000000000000000000 ) ) ;
#6024 = CARTESIAN_POINT ( 'NONE',  ( -29.04400972079232446, 10.22852224114065045, -35.70569127779752705 ) ) ;
#6025 = CARTESIAN_POINT ( 'NONE',  ( -49.44484229820456989, 14.28460989390480051, -64.55669302136469412 ) ) ;
#6026 = VECTOR ( 'NONE', #14535, 1000.000000000000114 ) ;
#6027 = CYLINDRICAL_SURFACE ( 'NONE', #52139, 4.999999999999990230 ) ;
#6028 = CARTESIAN_POINT ( 'NONE',  ( 444.9999999999999432, -35.00000000000000000, -2.000000000000000000 ) ) ;
#6029 = ORIENTED_EDGE ( 'NONE', *, *, #21529, .T. ) ;
#6030 = CIRCLE ( 'NONE', #53220, 246.3582898394606957 ) ;
#6031 = ORIENTED_EDGE ( 'NONE', *, *, #38207, .F. ) ;
#6032 = CIRCLE ( 'NONE', #418, 72.99999999999998579 ) ;
#6033 = CARTESIAN_POINT ( 'NONE',  ( 33.75794032130629319, 8.754084575552406378, 69.22175981326891758 ) ) ;
#6034 = CARTESIAN_POINT ( 'NONE',  ( -166.2065256787326746, 81.19093426984591133, 68.08525401877383842 ) ) ;
#6035 = VECTOR ( 'NONE', #36197, 1000.000000000000000 ) ;
#6036 = CARTESIAN_POINT ( 'NONE',  ( -167.0073208999199323, 82.02183861952775601, -19.71965070342400494 ) ) ;
#6037 = VECTOR ( 'NONE', #41872, 1000.000000000000000 ) ;
#6038 = DIRECTION ( 'NONE',  ( -0.000000000000000000, -0.000000000000000000, 1.000000000000000000 ) ) ;
#6039 = ORIENTED_EDGE ( 'NONE', *, *, #52098, .T. ) ;
#6040 = ADVANCED_FACE ( 'NONE', ( #29036 ), #51855, .T. ) ;
#6041 = DIRECTION ( 'NONE',  ( 0.000000000000000000, 0.000000000000000000, -1.000000000000000000 ) ) ;
#6042 = CARTESIAN_POINT ( 'NONE',  ( -8.807541152391518580, 6.956521193351525412, 71.91155975037588632 ) ) ;
#6043 = CARTESIAN_POINT ( 'NONE',  ( 0.000000000000000000, 172.0000000000000284, 0.000000000000000000 ) ) ;
#6044 =( NAMED_UNIT ( * ) SI_UNIT ( $, .STERADIAN. ) SOLID_ANGLE_UNIT ( ) );
#6045 = CARTESIAN_POINT ( 'NONE',  ( 86.62931800182293784, -170.0000000000000000, -16.47701360844803986 ) ) ;
#6046 = CARTESIAN_POINT ( 'NONE',  ( 46.85206196242844356, 9.495795933269466360, -17.26884272364058504 ) ) ;
#6047 = CARTESIAN_POINT ( 'NONE',  ( 210.9506883977752807, 115.3310071214937693, -21.13087597562173414 ) ) ;
#6048 = DIRECTION ( 'NONE',  ( -0.000000000000000000, 1.000000000000000000, -0.000000000000000000 ) ) ;
#6049 = EDGE_CURVE ( 'NONE', #20617, #62854, #67021, .T. ) ;
#6050 = CARTESIAN_POINT ( 'NONE',  ( 162.8034185388970343, 63.22443559329414597, 58.45892248144684089 ) ) ;
#6051 = ORIENTED_EDGE ( 'NONE', *, *, #27779, .T. ) ;
#6052 = LINE ( 'NONE', #54591, #30147 ) ;
#6053 = CARTESIAN_POINT ( 'NONE',  ( -29.70166638324878150, -57.83280658984300970, 43.58025477438756923 ) ) ;
#6054 = CARTESIAN_POINT ( 'NONE',  ( -54.08488990389049178, 15.46443908526321742, 57.20895787309505920 ) ) ;
#6055 = CARTESIAN_POINT ( 'NONE',  ( 21.27121078971613244, 61.42097029141973508, 170.0000000000000000 ) ) ;
#6056 = CARTESIAN_POINT ( 'NONE',  ( -24.39249304643357519, -60.24953346690487166, 40.00000000000003553 ) ) ;
#6057 = CARTESIAN_POINT ( 'NONE',  ( -13.55164437043334402, 8.341947975718044361, 86.45009797131527307 ) ) ;
#6058 = VERTEX_POINT ( 'NONE', #3667 ) ;
#6059 = CARTESIAN_POINT ( 'NONE',  ( 442.3372781065085633, 369.9999999999999432, 108.5502958579885870 ) ) ;
#6060 = PLANE ( 'NONE',  #27073 ) ;
#6061 = ORIENTED_EDGE ( 'NONE', *, *, #12416, .T. ) ;
#6062 = ORIENTED_EDGE ( 'NONE', *, *, #9927, .F. ) ;
#6063 = VECTOR ( 'NONE', #200, 1000.000000000000000 ) ;
#6064 = CARTESIAN_POINT ( 'NONE',  ( 11.98601804829806383, 14.28438006995820508, 82.99999999999998579 ) ) ;
#6065 = CARTESIAN_POINT ( 'NONE',  ( -55.05276343752910151, -170.0000000000000000, -62.06087458892354647 ) ) ;
#6066 = CARTESIAN_POINT ( 'NONE',  ( 102.7551177910568470, 25.56939188780864214, 36.61368049026674498 ) ) ;
#6067 = ORIENTED_EDGE ( 'NONE', *, *, #59775, .F. ) ;
#6068 = CARTESIAN_POINT ( 'NONE',  ( 63.01563776193090405, 13.70579113808098271, 71.65751152968501003 ) ) ;
#6069 = TOROIDAL_SURFACE ( 'NONE', #61121, 20.30000000000000071, 0.3000000000000062061 ) ;
#6070 = CARTESIAN_POINT ( 'NONE',  ( 37.46254810722765427, 8.164772623042710009, -23.53660314867922665 ) ) ;
#6071 = CARTESIAN_POINT ( 'NONE',  ( 164.1338586910086406, 64.33646242148856231, 40.36181753565011121 ) ) ;
#6072 = CARTESIAN_POINT ( 'NONE',  ( 109.7782172510783596, 29.77507867835876709, 2.766663615273646570 ) ) ;
#6073 = DIRECTION ( 'NONE',  ( -1.000000000000000000, 0.000000000000000000, 0.000000000000000000 ) ) ;
#6074 = CIRCLE ( 'NONE', #45411, 0.3000000000000051514 ) ;
#6075 = CARTESIAN_POINT ( 'NONE',  ( -132.6811329440527061, 52.36246882380746115, 94.99999999999866418 ) ) ;
#6076 = AXIS2_PLACEMENT_3D ( 'NONE', #412, #39114, #12366 ) ;
#6077 = EDGE_CURVE ( 'NONE', #61540, #31482, #44849, .T. ) ;
#6078 = AXIS2_PLACEMENT_3D ( 'NONE', #18807, #40952, #41304 ) ;
#6079 = CARTESIAN_POINT ( 'NONE',  ( -51.34562532494749831, 14.75613283840037226, -36.17846625611093714 ) ) ;
#6080 = B_SPLINE_CURVE_WITH_KNOTS ( 'NONE', 3,
 ( #39150, #34911, #24003, #12056, #2206, #23658, #6774, #29278, #60589, #55305, #2548, #45098, #13110, #18374, #28220, #49670, #1498, #8169, #39829, #44407, #61289, #22959, #7125, #50726, #40180, #56349, #28583, #1866, #23320, #52113, #3931, #4280, #68304, #41219, #40519, #62680, #8524, #19761, #41560, #19409, #20107, #25403, #63014, #3577 ),
 .UNSPECIFIED., .F., .F.,
 ( 4, 2, 2, 2, 2, 2, 2, 2, 2, 2, 2, 2, 1, 2, 2, 2, 2, 2, 2, 1, 2, 2, 4 ),
 ( 0.02381751147647563974, 0.02531129726520769604, 0.02605819015957372767, 0.02680508305393975582, 0.02829886884267181907, 0.02979265463140388231, 0.03053954752576990353, 0.03128644042013592474, 0.03278022620886795330, 0.03427401199759998879, 0.03576779778633201734, 0.03651469068069804202, 0.03726158357506405283, 0.03800847646943007058, 0.03875536936379608832, 0.04024915515252812381, 0.04174294094126016624, 0.04323672672999220867, 0.04398361962435821948, 0.04473051251872424416, 0.04547740541309025497, 0.04622429830745627966, 0.04771808409618832902 ),
 .UNSPECIFIED. ) ;
#6081 = EDGE_CURVE ( 'NONE', #61817, #9471, #14712, .T. ) ;
#6082 = AXIS2_PLACEMENT_3D ( 'NONE', #36546, #16462, #5555 ) ;
#6083 = DIRECTION ( 'NONE',  ( 0.000000000000000000, 1.000000000000000000, -0.000000000000000000 ) ) ;
#6084 = DIRECTION ( 'NONE',  ( 0.000000000000000000, 0.000000000000000000, 1.000000000000000000 ) ) ;
#6085 = FACE_OUTER_BOUND ( 'NONE', #8427, .T. ) ;
#6086 = CARTESIAN_POINT ( 'NONE',  ( -85.84807893108717280, 26.27917891747323864, 93.79365355873615329 ) ) ;
#6088 = ORIENTED_EDGE ( 'NONE', *, *, #65385, .T. ) ;
#6087 = CYLINDRICAL_SURFACE ( 'NONE', #32050, 5.000000000000004441 ) ;
#6089 = ORIENTED_EDGE ( 'NONE', *, *, #12217, .F. ) ;
#6090 = VERTEX_POINT ( 'NONE', #59791 ) ;
#6091 = CARTESIAN_POINT ( 'NONE',  ( -15.31363169557738857, 7.494880774892000552, -16.56097040027614398 ) ) ;
#6092 = CARTESIAN_POINT ( 'NONE',  ( -168.3977227042350364, 83.48347000932561457, 86.17750987296554399 ) ) ;
#6093 = DIRECTION ( 'NONE',  ( 1.000000000000000000, 0.000000000000000000, 0.000000000000000000 ) ) ;
#6094 = DIRECTION ( 'NONE',  ( -0.000000000000000000, 0.000000000000000000, -1.000000000000000000 ) ) ;
#6095 = ADVANCED_FACE ( 'NONE', ( #31440 ), #33082, .T. ) ;
#6096 = CARTESIAN_POINT ( 'NONE',  ( -38.80621507254813451, 11.94263265896520210, 66.02956010511333318 ) ) ;
#6097 = DIRECTION ( 'NONE',  ( -0.000000000000000000, -0.7071067811865474617, -0.7071067811865474617 ) ) ;
#6098 = CARTESIAN_POINT ( 'NONE',  ( -2.699999999999990408, 0.000000000000000000, 0.000000000000000000 ) ) ;
#6099 = CARTESIAN_POINT ( 'NONE',  ( 22.30016284075437127, 6.796348835713777348, -12.42137258383503173 ) ) ;
#6100 = ORIENTED_EDGE ( 'NONE', *, *, #66117, .F. ) ;
#6101 = CARTESIAN_POINT ( 'NONE',  ( 15.68296563925494702, 63.09411298019766434, 170.0000000000000000 ) ) ;
#6102 = ORIENTED_EDGE ( 'NONE', *, *, #58756, .F. ) ;
#6103 = EDGE_CURVE ( 'NONE', #19020, #46372, #57484, .T. ) ;
#6104 = VERTEX_POINT ( 'NONE', #65088 ) ;
#6105 = EDGE_CURVE ( 'NONE', #33757, #8652, #8374, .T. ) ;
#6106 = DIRECTION ( 'NONE',  ( -0.000000000000000000, -0.000000000000000000, -1.000000000000000000 ) ) ;
#6107 = DIRECTION ( 'NONE',  ( -0.5508969814521065267, 0.8345732537212999791, 0.000000000000000000 ) ) ;
#6108 = DIRECTION ( 'NONE',  ( 0.000000000000000000, 0.000000000000000000, -1.000000000000000000 ) ) ;
#6109 = CARTESIAN_POINT ( 'NONE',  ( -8.000000000000000000, 4.618802153516996079, -0.7145311798163263006 ) ) ;
#6110 = CARTESIAN_POINT ( 'NONE',  ( -109.5025362253418706, 36.60371748273998094, 13.26117751266643197 ) ) ;
#6111 = CARTESIAN_POINT ( 'NONE',  ( 18.89064107370903045, 6.619789970027398773, 44.34734594329952273 ) ) ;
#6112 = CARTESIAN_POINT ( 'NONE',  ( 136.7690435008551049, 44.39743995805024923, -23.59407883755694257 ) ) ;
#6113 = ORIENTED_EDGE ( 'NONE', *, *, #6819, .T. ) ;
#6114 = EDGE_LOOP ( 'NONE', ( #32174, #38694, #18164, #14461 ) ) ;
#6115 = ORIENTED_EDGE ( 'NONE', *, *, #51628, .T. ) ;
#6116 = VECTOR ( 'NONE', #38276, 1000.000000000000000 ) ;
#6117 = FACE_OUTER_BOUND ( 'NONE', #68741, .T. ) ;
#6118 = CARTESIAN_POINT ( 'NONE',  ( -150.3850953947692517, 66.25368649589886161, -8.006832433699385021 ) ) ;
#6119 = CARTESIAN_POINT ( 'NONE',  ( 31.95163392065795804, 8.568192436298499359, -44.11143406309549420 ) ) ;
#6120 = DIRECTION ( 'NONE',  ( -0.7071067811865474617, 9.422489238170280455E-15, 0.7071067811865475727 ) ) ;
#6121 = DIRECTION ( 'NONE',  ( 0.000000000000000000, 0.000000000000000000, 1.000000000000000000 ) ) ;
#6122 = ORIENTED_EDGE ( 'NONE', *, *, #52932, .F. ) ;
#6123 = AXIS2_PLACEMENT_3D ( 'NONE', #5017, #4669, #53879 ) ;
#6124 = DIRECTION ( 'NONE',  ( 4.314083075427411048E-32, 1.000000000000000000, 6.123233995736763571E-17 ) ) ;
#6125 = CARTESIAN_POINT ( 'NONE',  ( -155.1355020251929204, 69.10372769512068203, 60.08263860740119355 ) ) ;
#6126 = LINE ( 'NONE', #59938, #12679 ) ;
#6127 = CARTESIAN_POINT ( 'NONE',  ( 102.7435092758398127, 25.56449004647817702, 10.53745896246627467 ) ) ;
#6128 = CARTESIAN_POINT ( 'NONE',  ( 86.62931800182293784, -170.0000000000000000, -97.01066537983908233 ) ) ;
#6129 = LINE ( 'NONE', #64891, #46370 ) ;
#6130 = VECTOR ( 'NONE', #23542, 1000.000000000000000 ) ;
#6132 = EDGE_CURVE ( 'NONE', #29614, #23495, #3741, .T. ) ;
#6131 = DIRECTION ( 'NONE',  ( -1.000000000000000000, 0.000000000000000000, 0.000000000000000000 ) ) ;
#6133 = CARTESIAN_POINT ( 'NONE',  ( 109.9975424824652634, 295.8720703627916464, 535.5371946177799600 ) ) ;
#6134 = CARTESIAN_POINT ( 'NONE',  ( 9.288975942802419894, 6.379608420846962780, -66.11257998586452800 ) ) ;
#6135 = AXIS2_PLACEMENT_3D ( 'NONE', #10751, #4448, #36807 ) ;
#6136 = VECTOR ( 'NONE', #68467, 1000.000000000000000 ) ;
#6137 = ORIENTED_EDGE ( 'NONE', *, *, #4375, .T. ) ;
#6138 = CARTESIAN_POINT ( 'NONE',  ( 209.3223706822284100, 190.0000000000000000, 31.44247402469554942 ) ) ;
#6139 = SHAPE_DEFINITION_REPRESENTATION ( #7501, #15003 ) ;
#6140 = FACE_OUTER_BOUND ( 'NONE', #41466, .T. ) ;
#6141 = CARTESIAN_POINT ( 'NONE',  ( -133.3926783185152090, 51.63401075114365568, -42.11240704302350935 ) ) ;
#6142 = CARTESIAN_POINT ( 'NONE',  ( 10.55634918610406281, 15.55634918610400241, 0.000000000000000000 ) ) ;
#6143 = DIRECTION ( 'NONE',  ( 0.000000000000000000, 0.000000000000000000, -1.000000000000000000 ) ) ;
#6144 = ORIENTED_EDGE ( 'NONE', *, *, #18397, .F. ) ;
#6145 = EDGE_LOOP ( 'NONE', ( #2439, #4920, #47219, #8611 ) ) ;
#6146 = PLANE ( 'NONE',  #6687 ) ;
#6147 = CARTESIAN_POINT ( 'NONE',  ( 0.000000000000000000, 0.000000000000000000, 170.0000000000000000 ) ) ;
#6148 = VERTEX_POINT ( 'NONE', #9291 ) ;
#6149 = ORIENTED_EDGE ( 'NONE', *, *, #34558, .F. ) ;
#6150 = DIRECTION ( 'NONE',  ( 0.000000000000000000, 0.000000000000000000, 1.000000000000000000 ) ) ;
#6151 = DIRECTION ( 'NONE',  ( -0.000000000000000000, 0.9989683093773507050, 0.04541273895899431562 ) ) ;
#6152 = ORIENTED_EDGE ( 'NONE', *, *, #29172, .T. ) ;
#6153 = CARTESIAN_POINT ( 'NONE',  ( 116.9197133427646804, 33.22079464767577406, 60.50180823940809915 ) ) ;
#6154 = CARTESIAN_POINT ( 'NONE',  ( 136.7507824285648894, 44.38599729999916121, 70.77785851943963280 ) ) ;
#6155 = CARTESIAN_POINT ( 'NONE',  ( -71.16584859396995455, 19.60484997908767113, -42.38048587538112599 ) ) ;
#6157 = EDGE_CURVE ( 'NONE', #35238, #63173, #22176, .T. ) ;
#6156 = CARTESIAN_POINT ( 'NONE',  ( -100.4262673593280226, 31.84860241619272969, 45.30150371153577282 ) ) ;
#6158 = CARTESIAN_POINT ( 'NONE',  ( 23.05216796272336666, 9.986758404124199018, 3.061616997868437868E-16 ) ) ;
#6159 = EDGE_CURVE ( 'NONE', #61576, #36681, #9645, .T. ) ;
#6160 = CARTESIAN_POINT ( 'NONE',  ( -53.38065169970959545, 15.27943072477081721, -8.556598799231236896 ) ) ;
#6161 = B_SPLINE_CURVE_WITH_KNOTS ( 'NONE', 3,
 ( #13636, #46326, #35091, #23508, #35442, #2397, #40024, #29466, #23855, #2056, #3095, #56542, #66779, #3429, #61134, #24206, #44949, #41065, #51621, #2741, #8372, #24894, #62524, #18568, #56196, #61484, #67131, #13304, #8014, #24555, #45990, #50925, #66436, #39674, #67460, #19252, #62161, #67802, #14339, #35793, #57242, #9057, #30507, #53320, #42771, #42094, #68155, #16048 ),
 .UNSPECIFIED., .F., .F.,
 ( 4, 2, 2, 2, 2, 2, 2, 2, 2, 2, 2, 2, 2, 2, 2, 2, 2, 2, 2, 2, 2, 2, 2, 4 ),
 ( 6.938893903907228378E-18, 0.001591515129442212751, 0.003183030258884418564, 0.003978787823605516374, 0.004774545388326614619, 0.006366060517768862281, 0.007957575647211110811, 0.009549090776653357607, 0.01034484834137448794, 0.01114060590609561828, 0.01193636347081674862, 0.01273212103553787895, 0.01432363616498013963, 0.01591515129442239856, 0.01671090885914353064, 0.01750666642386466271, 0.01830242398858579131, 0.01909818155330691991, 0.02068969668274923610, 0.02148545424747039592, 0.02228121181219155922, 0.02387272694163382336, 0.02466848450635492421, 0.02546424207107602852 ),
 .UNSPECIFIED. ) ;
#6162 = ADVANCED_FACE ( 'NONE', ( #5043 ), #19853, .F. ) ;
#6163 = ORIENTED_EDGE ( 'NONE', *, *, #4998, .F. ) ;
#6164 = CARTESIAN_POINT ( 'NONE',  ( -35.00000000000002842, -35.00000000000000000, 378.0000000000000000 ) ) ;
#6165 = VECTOR ( 'NONE', #60540, 1000.000000000000000 ) ;
#6166 = EDGE_CURVE ( 'NONE', #44138, #3913, #52873, .T. ) ;
#6167 = FACE_BOUND ( 'NONE', #54986, .T. ) ;
#6168 = CARTESIAN_POINT ( 'NONE',  ( -144.2038301586456157, 61.09856042007389476, -47.63804030527379041 ) ) ;
#6169 = CARTESIAN_POINT ( 'NONE',  ( -166.0031475600388831, 80.98114714564768235, -66.67602937550397257 ) ) ;
#6170 = AXIS2_PLACEMENT_3D ( 'NONE', #8294, #46253, #41679 ) ;
#6172 = ORIENTED_EDGE ( 'NONE', *, *, #10339, .T. ) ;
#6171 = CARTESIAN_POINT ( 'NONE',  ( -133.3913294106239391, 51.63304446851032026, 91.41765249869638410 ) ) ;
#6173 = CARTESIAN_POINT ( 'NONE',  ( 58.46823952472683317, 12.69204591816734684, 16.45271400437258080 ) ) ;
#6174 = EDGE_CURVE ( 'NONE', #10843, #21469, #37057, .T. ) ;
#6175 = VECTOR ( 'NONE', #41501, 1000.000000000000000 ) ;
#6176 = VECTOR ( 'NONE', #2021, 1000.000000000000000 ) ;
#6177 = ORIENTED_EDGE ( 'NONE', *, *, #34254, .T. ) ;
#6178 = DIRECTION ( 'NONE',  ( 0.000000000000000000, -0.4999999999999998890, 0.8660254037844387076 ) ) ;
#6179 = CARTESIAN_POINT ( 'NONE',  ( -56.02358673658416421, 14.94347049174936970, -23.32432881613157960 ) ) ;
#6180 = CARTESIAN_POINT ( 'NONE',  ( 0.000000000000000000, 0.000000000000000000, -10.00000000000000000 ) ) ;
#6181 =( GEOMETRIC_REPRESENTATION_CONTEXT ( 3 ) GLOBAL_UNCERTAINTY_ASSIGNED_CONTEXT ( ( #62024 ) ) GLOBAL_UNIT_ASSIGNED_CONTEXT ( ( #51907, #14959, #58221 ) ) REPRESENTATION_CONTEXT ( 'NONE', 'WORKASPACE' ) );
#6183 = CARTESIAN_POINT ( 'NONE',  ( 184.3941060377211727, 82.01604625189465025, -23.62510121971022414 ) ) ;
#6182 = VECTOR ( 'NONE', #34667, 1000.000000000000000 ) ;
#6184 = CARTESIAN_POINT ( 'NONE',  ( 80.73012746365749592, 17.49169339352364005, -11.81929625901135417 ) ) ;
#6185 = CARTESIAN_POINT ( 'NONE',  ( 94.12811352634518869, 22.11743943276049507, -70.69009586073259754 ) ) ;
#6186 = DIRECTION ( 'NONE',  ( 0.000000000000000000, -1.000000000000000000, 0.000000000000000000 ) ) ;
#6187 = VECTOR ( 'NONE', #64225, 1000.000000000000000 ) ;
#6188 = CARTESIAN_POINT ( 'NONE',  ( -99.98930671699734773, 31.63190627461931470, 4.017523108268790999 ) ) ;
#6189 = CARTESIAN_POINT ( 'NONE',  ( 5.000000000000000888, 6.123233995736767268E-16, -9.474599999999998801 ) ) ;
#6190 = ORIENTED_EDGE ( 'NONE', *, *, #19312, .T. ) ;
#6191 = ADVANCED_FACE ( 'NONE', ( #11607 ), #56673, .T. ) ;
#6192 = ORIENTED_EDGE ( 'NONE', *, *, #9056, .T. ) ;
#6193 = ADVANCED_FACE ( 'NONE', ( #36026 ), #4019, .T. ) ;
#6194 = B_SPLINE_CURVE_WITH_KNOTS ( 'NONE', 3,
 ( #22551, #33475, #32419, #12001, #392, #1448, #13397, #24308, #39775, #40466, #39426, #7071, #46087, #66529, #8467, #40812, #8114, #67556, #34166, #55604, #18675, #3195, #44710, #29564, #23948, #34859, #50673, #24652, #2495, #18320, #29226, #12351, #33808, #7434, #50337, #29919, #35192, #45397, #60877, #61585, #66877, #45750, #13060 ),
 .UNSPECIFIED., .F., .F.,
 ( 4, 2, 2, 2, 2, 2, 2, 2, 1, 2, 2, 2, 2, 2, 2, 2, 2, 2, 2, 2, 2, 4 ),
 ( 1.734723475976807094E-18, 0.001466540241398130986, 0.002199810362097197672, 0.002933080482796264141, 0.004399620724194394476, 0.005866160965592523945, 0.007332701206990653413, 0.008065971327689720749, 0.008799241448388787218, 0.009532511569087855421, 0.01026578168978692363, 0.01173232193118506177, 0.01319886217258319644, 0.01466540241398133111, 0.01539867253468040278, 0.01613194265537947619, 0.01759848289677760913, 0.01906502313817574901, 0.01979829325887481201, 0.02053156337957388194, 0.02199810362097201488, 0.02346464386237014782 ),
 .UNSPECIFIED. ) ;
#6195 = DIRECTION ( 'NONE',  ( -0.000000000000000000, 0.000000000000000000, -1.000000000000000000 ) ) ;
#6196 = CARTESIAN_POINT ( 'NONE',  ( 10.83418588031599583, 6.392467435475930770, 31.86208434653760335 ) ) ;
#6197 = PLANE ( 'NONE',  #24495 ) ;
#6198 = FACE_OUTER_BOUND ( 'NONE', #21474, .T. ) ;
#6199 = LINE ( 'NONE', #22379, #31098 ) ;
#6200 = DIRECTION ( 'NONE',  ( -0.000000000000000000, 0.000000000000000000, -1.000000000000000000 ) ) ;
#6201 = CARTESIAN_POINT ( 'NONE',  ( -7.825402957745087207, -170.0000000000000000, -42.91807073194382838 ) ) ;
#6202 = CARTESIAN_POINT ( 'NONE',  ( 43.35536254672140188, 9.973606330917817786, -49.49790769984580407 ) ) ;
#6203 = FACE_OUTER_BOUND ( 'NONE', #4052, .T. ) ;
#6204 = VERTEX_POINT ( 'NONE', #20190 ) ;
#6205 = CARTESIAN_POINT ( 'NONE',  ( -26.88635117726413171, 9.904687797303028063, 16.85200533244904619 ) ) ;
#6206 = EDGE_LOOP ( 'NONE', ( #52112, #47625, #22210, #62990 ) ) ;
#6207 = CARTESIAN_POINT ( 'NONE',  ( -15.27748264047829885, 7.491388194171919146, -41.93772705272429846 ) ) ;
#6208 = CARTESIAN_POINT ( 'NONE',  ( -85.35521056349260505, 24.98314685266450752, 94.99999999999866418 ) ) ;
#6209 = CARTESIAN_POINT ( 'NONE',  ( 89.20981392318256553, 21.38519354635262459, 71.10286512656854541 ) ) ;
#6210 = CARTESIAN_POINT ( 'NONE',  ( 153.4268936273268764, 54.57409659828382331, -23.10063676753390283 ) ) ;
#6211 = CARTESIAN_POINT ( 'NONE',  ( 9.737557066527559257, 192.0000000000000000, 2.275957463600585040 ) ) ;
#6212 = LINE ( 'NONE', #66033, #10927 ) ;
#6213 = CARTESIAN_POINT ( 'NONE',  ( 110.6336604720866035, 30.17285371011658057, -89.61153874658104712 ) ) ;
#6214 = CYLINDRICAL_SURFACE ( 'NONE', #57367, 7.500000000000013323 ) ;
#6215 = DIRECTION ( 'NONE',  ( 1.387778780781446169E-16, -1.000000000000000000, -3.469446951953615421E-17 ) ) ;
#6216 = ORIENTED_EDGE ( 'NONE', *, *, #53042, .F. ) ;
#6217 = CARTESIAN_POINT ( 'NONE',  ( -783.0172411895269988, -622.0000000000060254, 10.00000000000000000 ) ) ;
#6218 = CARTESIAN_POINT ( 'NONE',  ( -29.49620345460274606, 9.280093073089046740, 18.13254437223945459 ) ) ;
#6219 = CARTESIAN_POINT ( 'NONE',  ( 46.80475532923159676, 10.50744084852537341, -71.19293443510808572 ) ) ;
#6220 = CARTESIAN_POINT ( 'NONE',  ( 283.9749324730389048, -21.78918450429459241, 3.050527833458462457 ) ) ;
#6221 = DIRECTION ( 'NONE',  ( -1.000000000000000000, 0.000000000000000000, 0.000000000000000000 ) ) ;
#6222 = B_SPLINE_CURVE_WITH_KNOTS ( 'NONE', 3,
 ( #13959, #51601, #62848, #56886, #3409, #24868 ),
 .UNSPECIFIED., .F., .F.,
 ( 4, 2, 4 ),
 ( 0.03218953612796865427, 0.06469846386257042947, 0.09720739159717220468 ),
 .UNSPECIFIED. ) ;
#6223 = CARTESIAN_POINT ( 'NONE',  ( 90.94525594974463445, 22.00941049511687098, 84.75862509362771391 ) ) ;
#6224 = VECTOR ( 'NONE', #52718, 1000.000000000000227 ) ;
#6225 = VERTEX_POINT ( 'NONE', #41647 ) ;
#6226 = VECTOR ( 'NONE', #63406, 1000.000000000000000 ) ;
#6227 = DIRECTION ( 'NONE',  ( -8.461431852934138533E-15, 4.601003589644306329E-15, -1.000000000000000000 ) ) ;
#6228 = LINE ( 'NONE', #12562, #10461 ) ;
#6229 = CARTESIAN_POINT ( 'NONE',  ( -132.8123438040339579, 51.22132183644640691, 14.18276217007199946 ) ) ;
#6230 = CARTESIAN_POINT ( 'NONE',  ( -168.7329347389696181, 83.83901812802758968, -48.31275808947942352 ) ) ;
#6231 = CARTESIAN_POINT ( 'NONE',  ( -180.1266724401835688, 95.28036793547788363, 89.30961988341643121 ) ) ;
#6232 = ORIENTED_EDGE ( 'NONE', *, *, #63129, .F. ) ;
#6234 = CARTESIAN_POINT ( 'NONE',  ( 8.828807734115068584, -74.48902371486708773, 170.0000000000000000 ) ) ;
#6233 = VECTOR ( 'NONE', #49492, 1000.000000000000114 ) ;
#6235 = AXIS2_PLACEMENT_3D ( 'NONE', #796, #54594, #6418 ) ;
#6236 = CARTESIAN_POINT ( 'NONE',  ( -49.77357484059193382, 41.82599373102802076, 0.000000000000000000 ) ) ;
#6237 = AXIS2_PLACEMENT_3D ( 'NONE', #4508, #52005, #37199 ) ;
#6238 = CARTESIAN_POINT ( 'NONE',  ( 198.4059165548112560, 99.71594270191988585, -12.89058402406104342 ) ) ;
#6239 = VECTOR ( 'NONE', #30416, 1000.000000000000000 ) ;
#6240 = CARTESIAN_POINT ( 'NONE',  ( -4.072522659361693442, 7.683023425615343349, -76.26080512505431841 ) ) ;
#6241 = CONICAL_SURFACE ( 'NONE', #62393, 73.43826238111391547, 0.6747409422235518539 ) ;
#6242 = CARTESIAN_POINT ( 'NONE',  ( -16.20761945673107363, 34.73915175314249382, 13.32819299319723605 ) ) ;
#6243 = ORIENTED_EDGE ( 'NONE', *, *, #19527, .T. ) ;
#6244 = DIRECTION ( 'NONE',  ( 0.000000000000000000, -0.000000000000000000, -1.000000000000000000 ) ) ;
#6245 = DIRECTION ( 'NONE',  ( 0.000000000000000000, 1.000000000000000000, -1.224646799147353207E-16 ) ) ;
#6246 = CARTESIAN_POINT ( 'NONE',  ( -96.76336539645315327, 31.18045094643427362, 32.91415803190486855 ) ) ;
#6247 = CARTESIAN_POINT ( 'NONE',  ( 112.3013380801408658, 388.0000000000065938, -133.9497041420121377 ) ) ;
#6249 = EDGE_LOOP ( 'NONE', ( #30382, #9819, #17773, #59788 ) ) ;
#6248 = CARTESIAN_POINT ( 'NONE',  ( 113.4418023215250457, 31.50656691678298316, 3.466527937886946464 ) ) ;
#6250 = DIRECTION ( 'NONE',  ( 0.000000000000000000, 0.000000000000000000, -1.000000000000000000 ) ) ;
#6251 = EDGE_CURVE ( 'NONE', #24023, #32779, #3903, .T. ) ;
#6252 = EDGE_LOOP ( 'NONE', ( #19238, #2485, #27981, #3587 ) ) ;
#6253 = ORIENTED_EDGE ( 'NONE', *, *, #37228, .F. ) ;
#6254 = LINE ( 'NONE', #65360, #24437 ) ;
#6255 = DIRECTION ( 'NONE',  ( 1.000000000000000000, 0.000000000000000000, -2.220446049250313081E-16 ) ) ;
#6257 = ORIENTED_EDGE ( 'NONE', *, *, #45589, .F. ) ;
#6256 = CARTESIAN_POINT ( 'NONE',  ( -78.66644367742111399, -170.0000000000000000, -69.46000122218158879 ) ) ;
#6258 = CARTESIAN_POINT ( 'NONE',  ( 162.7921669283191761, 61.91024532638673605, 31.61904728604499226 ) ) ;
#6259 = EDGE_CURVE ( 'NONE', #22131, #59849, #36371, .T. ) ;
#6260 = CARTESIAN_POINT ( 'NONE',  ( 0.2727178028659107412, 0.000000000000000000, 0.000000000000000000 ) ) ;
#6261 = LINE ( 'NONE', #28414, #36185 ) ;
#6262 = ORIENTED_EDGE ( 'NONE', *, *, #363, .F. ) ;
#6263 = DIRECTION ( 'NONE',  ( -1.000000000000000000, 0.000000000000000000, 0.000000000000000000 ) ) ;
#6264 = AXIS2_PLACEMENT_3D ( 'NONE', #45732, #66859, #18998 ) ;
#6265 = CARTESIAN_POINT ( 'NONE',  ( 39.40195752203892710, 8.409560354027373563, 3.069283715499574683 ) ) ;
#6266 = CYLINDRICAL_SURFACE ( 'NONE', #25796, 25.00000000000000000 ) ;
#6267 = CARTESIAN_POINT ( 'NONE',  ( -37.92511097250854846, 10.74631978746600325, -65.88783957002343072 ) ) ;
#6268 = CARTESIAN_POINT ( 'NONE',  ( 20.35964562795319566, 7.697260051881318788, 70.32522021214651886 ) ) ;
#6269 = EDGE_CURVE ( 'NONE', #24463, #24269, #18512, .T. ) ;
#6270 = ORIENTED_EDGE ( 'NONE', *, *, #4897, .F. ) ;
#6271 = EDGE_LOOP ( 'NONE', ( #58574, #4451 ) ) ;
#6272 = VECTOR ( 'NONE', #35114, 1000.000000000000000 ) ;
#6273 = VERTEX_POINT ( 'NONE', #68715 ) ;
#6274 = CARTESIAN_POINT ( 'NONE',  ( -27.33809837083532557, -60.78020170929433874, 34.48241795236666007 ) ) ;
#6275 = DIRECTION ( 'NONE',  ( 0.000000000000000000, -1.000000000000000000, 0.000000000000000000 ) ) ;
#6276 = AXIS2_PLACEMENT_3D ( 'NONE', #34371, #7282, #28735 ) ;
#6277 = CONICAL_SURFACE ( 'NONE', #41143, 185.0000000000000000, 1.279339532317029793 ) ;
#6278 = DIRECTION ( 'NONE',  ( 0.000000000000000000, 1.000000000000000000, -1.224646799147353207E-16 ) ) ;
#6279 = CARTESIAN_POINT ( 'NONE',  ( -38.69577193929646342, 10.89562623693160326, -44.77552114323132315 ) ) ;
#6280 = CARTESIAN_POINT ( 'NONE',  ( -94.77322158248860262, 29.12812870088611561, 91.80393034221229698 ) ) ;
#6281 = PRODUCT_DEFINITION_FORMATION_WITH_SPECIFIED_SOURCE ( 'ANY', '', #66481, .NOT_KNOWN. ) ;
#6282 = CARTESIAN_POINT ( 'NONE',  ( -20.55634918610400419, 20.55634918610405748, 0.000000000000000000 ) ) ;
#6283 = DIRECTION ( 'NONE',  ( -0.000000000000000000, -0.000000000000000000, -1.000000000000000000 ) ) ;
#6284 = CARTESIAN_POINT ( 'NONE',  ( -47.56904557163428393, 13.83539285446097189, 90.91553801162412185 ) ) ;
#6285 = VECTOR ( 'NONE', #38101, 1000.000000000000000 ) ;
#6286 = CARTESIAN_POINT ( 'NONE',  ( 79.23200707685337818, 17.02828389812517784, 65.31902592513927175 ) ) ;
#6287 = ORIENTED_EDGE ( 'NONE', *, *, #13678, .F. ) ;
#6289 = AXIS2_PLACEMENT_3D ( 'NONE', #60274, #2238, #7521 ) ;
#6288 = LINE ( 'NONE', #48826, #31905 ) ;
#6290 = VERTEX_POINT ( 'NONE', #47592 ) ;
#6291 = CARTESIAN_POINT ( 'NONE',  ( 209.3223706822284100, 172.0000000000000284, 31.44247402469554942 ) ) ;
#6292 =( REPRESENTATION_RELATIONSHIP ('NONE','NONE', #40274, #64096 ) REPRESENTATION_RELATIONSHIP_WITH_TRANSFORMATION ( #44206 )SHAPE_REPRESENTATION_RELATIONSHIP( ) );
#6293 = CARTESIAN_POINT ( 'NONE',  ( 210.1954643503415525, 114.1986276268024056, -65.56311968808857671 ) ) ;
#6294 = FACE_OUTER_BOUND ( 'NONE', #48770, .T. ) ;
#6295 = CARTESIAN_POINT ( 'NONE',  ( -71.16770070143910232, 19.60548673929829988, 10.54887064238381456 ) ) ;
#6296 = LINE ( 'NONE', #21431, #27776 ) ;
#6297 = CARTESIAN_POINT ( 'NONE',  ( -53.38256734720888375, 14.24001356352780689, 3.657108157446994134 ) ) ;
#6298 = CARTESIAN_POINT ( 'NONE',  ( -15.55634918610408945, -26.11269837220804035, 2.000000000000001776 ) ) ;
#6299 = CARTESIAN_POINT ( 'NONE',  ( 103.0463737467386665, 26.78595250599333255, -95.00000000000133582 ) ) ;
#6300 = VERTEX_POINT ( 'NONE', #69051 ) ;
#6301 = LINE ( 'NONE', #17555, #9469 ) ;
#6302 = DIRECTION ( 'NONE',  ( -0.000000000000000000, 1.000000000000000000, -0.000000000000000000 ) ) ;
#6303 = ORIENTED_EDGE ( 'NONE', *, *, #5241, .T. ) ;
#6304 = DIRECTION ( 'NONE',  ( -0.000000000000000000, 1.000000000000000000, -0.000000000000000000 ) ) ;
#6305 = CARTESIAN_POINT ( 'NONE',  ( -1.068536297472280960, -51.65427651052054614, 26.66469066592268433 ) ) ;
#6306 = ORIENTED_EDGE ( 'NONE', *, *, #9062, .F. ) ;
#6307 = CARTESIAN_POINT ( 'NONE',  ( -80.55742067659893735, 23.05042616197511762, 30.64490407056336707 ) ) ;
#6308 = CARTESIAN_POINT ( 'NONE',  ( 155.7265855639938650, 57.57443315515121895, -77.77659484219802266 ) ) ;
#6309 = CARTESIAN_POINT ( 'NONE',  ( 0.000000000000000000, 0.000000000000000000, 170.0000000000000000 ) ) ;
#6310 = CARTESIAN_POINT ( 'NONE',  ( -23.93880457192868860, 8.479983864459175180, 64.80067904941660117 ) ) ;
#6311 = CARTESIAN_POINT ( 'NONE',  ( 127.2397149628677653, 37.56999625068102944, -13.11060947991069447 ) ) ;
#6312 = ORIENTED_EDGE ( 'NONE', *, *, #52411, .F. ) ;
#6313 = ORIENTED_EDGE ( 'NONE', *, *, #24718, .F. ) ;
#6314 = CARTESIAN_POINT ( 'NONE',  ( -31.43908319763709969, 9.591432048623765638, 3.371903815725488585 ) ) ;
#6315 = ORIENTED_EDGE ( 'NONE', *, *, #50891, .F. ) ;
#6316 = LINE ( 'NONE', #16174, #20001 ) ;
#6317 = CARTESIAN_POINT ( 'NONE',  ( 0.000000000000000000, 0.000000000000000000, 170.0000000000000000 ) ) ;
#6318 = CARTESIAN_POINT ( 'NONE',  ( 208.9781236209185522, 112.4006213943319352, 42.88291611263555581 ) ) ;
#6319 = EDGE_CURVE ( 'NONE', #67501, #23678, #48190, .T. ) ;
#6320 = CARTESIAN_POINT ( 'NONE',  ( -5.879983509979055611, 7.779504553499496211, 57.20031220924396820 ) ) ;
#6321 = PRODUCT ( 'driven pulley', 'driven pulley', '', ( #46640 ) ) ;
#6322 =( NAMED_UNIT ( * ) SI_UNIT ( $, .STERADIAN. ) SOLID_ANGLE_UNIT ( ) );
#6323 = EDGE_CURVE ( 'NONE', #30445, #36476, #50644, .T. ) ;
#6324 = VECTOR ( 'NONE', #43029, 1000.000000000000000 ) ;
#6325 = ORIENTED_EDGE ( 'NONE', *, *, #65862, .F. ) ;
#6326 = DIRECTION ( 'NONE',  ( -0.000000000000000000, -0.000000000000000000, -1.000000000000000000 ) ) ;
#6327 = VERTEX_POINT ( 'NONE', #29198 ) ;
#6328 = ORIENTED_EDGE ( 'NONE', *, *, #10795, .T. ) ;
#6329 = CARTESIAN_POINT ( 'NONE',  ( 158.3595886390531575, 58.34525996025799799, -24.23990596987918877 ) ) ;
#6330 = PLANE ( 'NONE',  #40632 ) ;
#6331 = CIRCLE ( 'NONE', #36672, 65.00000000000000000 ) ;
#6332 = CARTESIAN_POINT ( 'NONE',  ( -71.96466849523078224, 21.15771699336999845, 170.0000000000000000 ) ) ;
#6333 = CARTESIAN_POINT ( 'NONE',  ( -132.5858388588929131, 52.29441124308996791, -92.68433720153500133 ) ) ;
#6334 = DIRECTION ( 'NONE',  ( 0.000000000000000000, 0.000000000000000000, 1.000000000000000000 ) ) ;
#6335 = AXIS2_PLACEMENT_3D ( 'NONE', #10289, #16265, #4347 ) ;
#6336 = ORIENTED_EDGE ( 'NONE', *, *, #37384, .F. ) ;
#6337 = FACE_OUTER_BOUND ( 'NONE', #63369, .T. ) ;
#6338 = EDGE_CURVE ( 'NONE', #16525, #37239, #59168, .T. ) ;
#6339 = CARTESIAN_POINT ( 'NONE',  ( 84.27368848767926579, 18.63026910897605859, 3.230755797320154610 ) ) ;
#6340 = ORIENTED_EDGE ( 'NONE', *, *, #27885, .T. ) ;
#6341 = EDGE_CURVE ( 'NONE', #42528, #57773, #66837, .T. ) ;
#6342 = DIRECTION ( 'NONE',  ( -4.270088556250601699E-16, -0.000000000000000000, -1.000000000000000000 ) ) ;
#6343 = EDGE_LOOP ( 'NONE', ( #7440, #64244, #49324, #19712 ) ) ;
#6344 = AXIS2_PLACEMENT_3D ( 'NONE', #44362, #23279, #17644 ) ;
#6345 = CARTESIAN_POINT ( 'NONE',  ( 19.25636590080467769, -33.14646233425818878, 13.32819299319722894 ) ) ;
#6346 = ORIENTED_EDGE ( 'NONE', *, *, #46476, .T. ) ;
#6347 = DIRECTION ( 'NONE',  ( -4.270088556250601699E-16, -0.000000000000000000, -1.000000000000000000 ) ) ;
#6348 = EDGE_CURVE ( 'NONE', #66136, #22496, #2466, .T. ) ;
#6349 = CARTESIAN_POINT ( 'NONE',  ( 87.58098510096633049, 19.74745174099416190, 2.912695539183820514 ) ) ;
#6350 = FACE_OUTER_BOUND ( 'NONE', #25484, .T. ) ;
#6351 = VERTEX_POINT ( 'NONE', #22521 ) ;
#6352 = CARTESIAN_POINT ( 'NONE',  ( 61.62594073580542897, 21.79346734965000820, 6.377659838150158269E-18 ) ) ;
#6353 = FILL_AREA_STYLE_COLOUR ( '', #5328 ) ;
#6354 = CARTESIAN_POINT ( 'NONE',  ( 38.91512155099544401, 9.360679678889633593, 29.91383430596324899 ) ) ;
#6355 = CARTESIAN_POINT ( 'NONE',  ( 3.000000000000028866, 2.999999999999969802, 0.000000000000000000 ) ) ;
#6356 = CARTESIAN_POINT ( 'NONE',  ( -131.2803255164624829, 50.14412978403780841, -10.34452356867482870 ) ) ;
#6357 = LINE ( 'NONE', #32055, #17698 ) ;
#6358 = CARTESIAN_POINT ( 'NONE',  ( -84.49322488516129681, 0.000000000000000000, 43.58025477438756212 ) ) ;
#6359 = ADVANCED_FACE ( 'NONE', ( #33781 ), #61552, .F. ) ;
#6360 = ORIENTED_EDGE ( 'NONE', *, *, #47873, .F. ) ;
#6361 = CARTESIAN_POINT ( 'NONE',  ( 133.8566784816069344, 42.60093787723652525, -77.86786152285937135 ) ) ;
#6362 = FACE_OUTER_BOUND ( 'NONE', #36222, .T. ) ;
#6363 = ORIENTED_EDGE ( 'NONE', *, *, #5405, .T. ) ;
#6364 = EDGE_CURVE ( 'NONE', #37468, #45637, #17234, .T. ) ;
#6365 = EDGE_CURVE ( 'NONE', #64051, #48012, #7400, .T. ) ;
#6366 = FACE_BOUND ( 'NONE', #12452, .T. ) ;
#6367 = CARTESIAN_POINT ( 'NONE',  ( -1.314022807222069877, 6.554273999800678929, -66.00870565782550159 ) ) ;
#6368 = CARTESIAN_POINT ( 'NONE',  ( -179.5186635612084274, 96.12511541314945873, 69.11882369886130562 ) ) ;
#6369 = CARTESIAN_POINT ( 'NONE',  ( -450.6627218934913230, 177.8591479523843475, -111.4497041420117966 ) ) ;
#6370 = DIRECTION ( 'NONE',  ( -1.000000000000000000, 0.000000000000000000, 0.000000000000000000 ) ) ;
#6371 = CARTESIAN_POINT ( 'NONE',  ( -4.502148936856956496, 7.704491846230413721, 44.35705480072686413 ) ) ;
#6372 = DIRECTION ( 'NONE',  ( 1.000000000000000000, 0.000000000000000000, 0.000000000000000000 ) ) ;
#6373 = CARTESIAN_POINT ( 'NONE',  ( 115.0001299725262811, 22.00002953920830606, 0.3279435515783862276 ) ) ;
#6374 = CARTESIAN_POINT ( 'NONE',  ( -125.8938041572051389, 47.69968343338778283, -76.75825448869764500 ) ) ;
#6375 = CARTESIAN_POINT ( 'NONE',  ( -14.84452950307166041, 8.460866451887698148, 34.96186735029871073 ) ) ;
#6376 = CARTESIAN_POINT ( 'NONE',  ( 160.5141379054754225, 60.05651755415394177, 16.93420630349488931 ) ) ;
#6377 = CARTESIAN_POINT ( 'NONE',  ( 43.68116950786570385, 10.02170697302967461, -90.63548873402001504 ) ) ;
#6378 = ORIENTED_EDGE ( 'NONE', *, *, #64654, .T. ) ;
#6379 = VECTOR ( 'NONE', #25784, 1000.000000000000000 ) ;
#6380 = DIRECTION ( 'NONE',  ( 0.000000000000000000, 1.000000000000000000, 0.000000000000000000 ) ) ;
#6381 = EDGE_LOOP ( 'NONE', ( #3291, #63257 ) ) ;
#6382 = CARTESIAN_POINT ( 'NONE',  ( -50.00000000000001421, 19.99999999999996447, 1.999999999999984457 ) ) ;
#6383 = LINE ( 'NONE', #66198, #11852 ) ;
#6384 = CARTESIAN_POINT ( 'NONE',  ( 39.88971011078925955, 8.472992116645420069, 56.75838489642695350 ) ) ;
#6385 = CARTESIAN_POINT ( 'NONE',  ( 563.4809901518626702, 2.000000000000001776, 57.79371821540657095 ) ) ;
#6386 = CARTESIAN_POINT ( 'NONE',  ( 70.50372867914782660, 14.53505678900966913, -15.88564835880266024 ) ) ;
#6387 = CARTESIAN_POINT ( 'NONE',  ( -31.43908319763709969, 10.61114334766715928, -50.31719736520186359 ) ) ;
#6388 = AXIS2_PLACEMENT_3D ( 'NONE', #14557, #51162, #19139 ) ;
#6389 = CARTESIAN_POINT ( 'NONE',  ( -53.13788504024113024, 15.21566150156365183, -76.82833932811897171 ) ) ;
#6390 = ORIENTED_EDGE ( 'NONE', *, *, #36540, .T. ) ;
#6392 = CIRCLE ( 'NONE', #41248, 23.97499999999999787 ) ;
#6391 = CARTESIAN_POINT ( 'NONE',  ( -75.76674366953606921, 22.30988704043531712, -89.37459560296670702 ) ) ;
#6393 = CARTESIAN_POINT ( 'NONE',  ( -118.6302575928420424, 43.07263081214306055, -13.68204589171926244 ) ) ;
#6394 = ORIENTED_EDGE ( 'NONE', *, *, #52016, .T. ) ;
#6395 = ORIENTED_EDGE ( 'NONE', *, *, #53817, .T. ) ;
#6396 = CARTESIAN_POINT ( 'NONE',  ( 36.08914434112043779, 9.014684630517852071, 70.99154541230063842 ) ) ;
#6397 = CARTESIAN_POINT ( 'NONE',  ( 180.6710448012268557, 78.18844465372404784, 56.15314469597509373 ) ) ;
#6398 = DIRECTION ( 'NONE',  ( 1.000000000000000000, -0.000000000000000000, -0.000000000000000000 ) ) ;
#6399 = AXIS2_PLACEMENT_3D ( 'NONE', #58013, #42520, #46760 ) ;
#6400 = CARTESIAN_POINT ( 'NONE',  ( -168.7329347389695897, 83.83901812802758968, -21.46820749901573677 ) ) ;
#6401 = PRODUCT_DEFINITION_CONTEXT ( 'detailed design', #3140, 'design' ) ;
#6402 = CARTESIAN_POINT ( 'NONE',  ( -59.09450113343203270, -27.07101652673575032, 170.0000000000000000 ) ) ;
#6403 = ORIENTED_EDGE ( 'NONE', *, *, #61855, .T. ) ;
#6404 = CARTESIAN_POINT ( 'NONE',  ( 92.53033045403535084, 22.59263332688196257, 5.712192295102347828 ) ) ;
#6405 = CARTESIAN_POINT ( 'NONE',  ( -15.13254930056756464, 7.477527548005404867, 66.16798222535943808 ) ) ;
#6406 = CARTESIAN_POINT ( 'NONE',  ( -83.69653436244857403, 24.30167057287991028, -10.20239559727127165 ) ) ;
#6407 = CARTESIAN_POINT ( 'NONE',  ( 45.82394788922869822, -46.11928342727429708, 43.58025477438756923 ) ) ;
#6408 = CARTESIAN_POINT ( 'NONE',  ( 41.35041461497707616, 8.670465437677201237, -9.016052168402659106 ) ) ;
#6409 = CARTESIAN_POINT ( 'NONE',  ( 208.6132326550593916, 111.8685719053116543, -10.57063359225124799 ) ) ;
#6410 = ADVANCED_FACE ( 'NONE', ( #50308 ), #22872, .F. ) ;
#6411 = FACE_BOUND ( 'NONE', #28187, .T. ) ;
#6412 = CARTESIAN_POINT ( 'NONE',  ( -62.54085973597666026, 16.81797209566546414, -43.20757385135579653 ) ) ;
#6413 = EDGE_CURVE ( 'NONE', #16646, #34225, #39401, .T. ) ;
#6414 = ORIENTED_EDGE ( 'NONE', *, *, #3817, .T. ) ;
#6415 = PLANE ( 'NONE',  #61463 ) ;
#6416 = CARTESIAN_POINT ( 'NONE',  ( 93.72687053612523300, 23.04134601640627977, -45.79658200368525911 ) ) ;
#6417 = LINE ( 'NONE', #48954, #36381 ) ;
#6418 = DIRECTION ( 'NONE',  ( -1.000000000000000000, 0.000000000000000000, 0.000000000000000000 ) ) ;
#6419 = CARTESIAN_POINT ( 'NONE',  ( 212.1913428512247037, 119.0779339498137688, 63.19771715593021355 ) ) ;
#6420 = CARTESIAN_POINT ( 'NONE',  ( 196.9999999999999716, 2.999999999999969802, 0.000000000000000000 ) ) ;
#6421 = AXIS2_PLACEMENT_3D ( 'NONE', #57042, #65428, #64729 ) ;
#6422 = ORIENTED_EDGE ( 'NONE', *, *, #18455, .T. ) ;
#6424 = EDGE_CURVE ( 'NONE', #26839, #37838, #31963, .T. ) ;
#6423 = FACE_OUTER_BOUND ( 'NONE', #23439, .T. ) ;
#6425 = DIRECTION ( 'NONE',  ( 1.000000000000000000, -4.565061778886334783E-18, 0.000000000000000000 ) ) ;
#6426 = ORIENTED_EDGE ( 'NONE', *, *, #48732, .T. ) ;
#6427 = EDGE_CURVE ( 'NONE', #50950, #65355, #5135, .T. ) ;
#6428 = VECTOR ( 'NONE', #48833, 1000.000000000000000 ) ;
#6429 = EDGE_LOOP ( 'NONE', ( #43842, #33122, #54627, #18006 ) ) ;
#6430 = EDGE_CURVE ( 'NONE', #7966, #38444, #21856, .T. ) ;
#6431 = CARTESIAN_POINT ( 'NONE',  ( 0.000000000000000000, 190.0000000000000000, 380.0000000000000000 ) ) ;
#6432 = DIRECTION ( 'NONE',  ( -0.000000000000000000, -0.000000000000000000, -1.000000000000000000 ) ) ;
#6433 = CARTESIAN_POINT ( 'NONE',  ( 102.7435092758398127, 25.56449004647817702, 37.38200955292992944 ) ) ;
#6434 = EDGE_LOOP ( 'NONE', ( #43960, #21401, #58839, #66124, #25080, #24775, #21189, #501, #27098 ) ) ;
#6435 = EDGE_CURVE ( 'NONE', #43624, #59231, #39062, .T. ) ;
#6436 = VECTOR ( 'NONE', #45427, 1000.000000000000000 ) ;
#6437 = ORIENTED_EDGE ( 'NONE', *, *, #19264, .T. ) ;
#6438 = DIRECTION ( 'NONE',  ( -0.000000000000000000, 1.000000000000000000, -0.000000000000000000 ) ) ;
#6439 = CARTESIAN_POINT ( 'NONE',  ( -18.89790202299119315, -62.20684691518632548, 170.0000000000000000 ) ) ;
#6440 = AXIS2_PLACEMENT_3D ( 'NONE', #30238, #19673, #62600 ) ;
#6441 = CARTESIAN_POINT ( 'NONE',  ( -156.0209085498132424, 71.27066046086521567, -72.91444613903827587 ) ) ;
#6442 = CARTESIAN_POINT ( 'NONE',  ( 69.36287815987334682, 15.27486453472191741, 6.465547984870822162 ) ) ;
#6443 = CARTESIAN_POINT ( 'NONE',  ( 5.690023276062394331, 5.952467836904149934, -9.369346954796190730 ) ) ;
#6444 = AXIS2_PLACEMENT_3D ( 'NONE', #32738, #60159, #39408 ) ;
#6445 = CARTESIAN_POINT ( 'NONE',  ( -47.65155309726505806, 13.85482731128120015, -43.95499868855683445 ) ) ;
#6446 = CARTESIAN_POINT ( 'NONE',  ( -48.23766733091050440, 13.99378332280058679, 14.11372853788430426 ) ) ;
#6447 = CARTESIAN_POINT ( 'NONE',  ( 280.0000000000000000, -22.00000000000000000, 0.000000000000000000 ) ) ;
#6448 = CARTESIAN_POINT ( 'NONE',  ( -154.7858533099351632, 70.14406136060938479, -90.65412252175239871 ) ) ;
#6449 = CARTESIAN_POINT ( 'NONE',  ( 64.62779760674203544, 13.05212430187077288, -89.57393277581095958 ) ) ;
#6450 = CARTESIAN_POINT ( 'NONE',  ( 80.45890692537896882, 17.40706746439065000, 86.62450930750821954 ) ) ;
#6452 = ORIENTED_EDGE ( 'NONE', *, *, #43333, .T. ) ;
#6451 = CARTESIAN_POINT ( 'NONE',  ( 0.000000000000000000, 0.000000000000000000, 0.000000000000000000 ) ) ;
#6453 = VERTEX_POINT ( 'NONE', #25317 ) ;
#6454 = EDGE_CURVE ( 'NONE', #47540, #5410, #43085, .T. ) ;
#6455 = EDGE_CURVE ( 'NONE', #24735, #28455, #61192, .T. ) ;
#6456 = ORIENTED_EDGE ( 'NONE', *, *, #54218, .F. ) ;
#6457 = CARTESIAN_POINT ( 'NONE',  ( -14.76369745117753141, 7.442560531763926512, -13.19444848579071028 ) ) ;
#6458 = CARTESIAN_POINT ( 'NONE',  ( -165.6311038533940234, 80.59874732648039242, 91.58102387426585267 ) ) ;
#6459 = CARTESIAN_POINT ( 'NONE',  ( 0.000000000000000000, 0.000000000000000000, -20.00000000000000000 ) ) ;
#6460 = FACE_OUTER_BOUND ( 'NONE', #38844, .T. ) ;
#6461 = EDGE_CURVE ( 'NONE', #60670, #23191, #10490, .T. ) ;
#6462 = CARTESIAN_POINT ( 'NONE',  ( -58.76099769480629220, 16.75353773354894216, -36.19268434689433889 ) ) ;
#6463 = PLANE ( 'NONE',  #38849 ) ;
#6464 = CARTESIAN_POINT ( 'NONE',  ( -76.78936026062119424, 21.61552955137053544, -76.72525579395438911 ) ) ;
#6465 = CARTESIAN_POINT ( 'NONE',  ( 4.360227613243417011, 41.50064055034692956, 13.79046412288134249 ) ) ;
#6466 = ORIENTED_EDGE ( 'NONE', *, *, #31873, .F. ) ;
#6467 = DIRECTION ( 'NONE',  ( 0.000000000000000000, -0.000000000000000000, 1.000000000000000000 ) ) ;
#6468 = ORIENTED_EDGE ( 'NONE', *, *, #15494, .T. ) ;
#6469 = ORIENTED_EDGE ( 'NONE', *, *, #66181, .T. ) ;
#6470 = LINE ( 'NONE', #27563, #69136 ) ;
#6471 = CARTESIAN_POINT ( 'NONE',  ( -61.71208512347170938, 17.61895039024948417, -92.92744643277735861 ) ) ;
#6472 = DIRECTION ( 'NONE',  ( -0.000000000000000000, 1.000000000000000000, -0.000000000000000000 ) ) ;
#6473 = CARTESIAN_POINT ( 'NONE',  ( 117.7417271423230147, 33.63613196344606138, -16.04272938009505012 ) ) ;
#6475 = CARTESIAN_POINT ( 'NONE',  ( -109.0297561673455817, 36.34391931706015555, 14.45457006512591036 ) ) ;
#6474 = AXIS2_PLACEMENT_3D ( 'NONE', #7658, #66411, #6945 ) ;
#6476 = CARTESIAN_POINT ( 'NONE',  ( -7.825402957745087207, -170.0000000000000000, 37.61558103944720699 ) ) ;
#6477 = CARTESIAN_POINT ( 'NONE',  ( 139.7883986595927581, 46.32091287009613723, -21.27522919412053071 ) ) ;
#6478 = ORIENTED_EDGE ( 'NONE', *, *, #62336, .F. ) ;
#6479 = ORIENTED_EDGE ( 'NONE', *, *, #26766, .F. ) ;
#6480 = ORIENTED_EDGE ( 'NONE', *, *, #50724, .F. ) ;
#6481 = AXIS2_PLACEMENT_3D ( 'NONE', #44370, #17652, #1829 ) ;
#6482 = CARTESIAN_POINT ( 'NONE',  ( -62.66631205405185057, 18.59153367093362874, 6.377659838150142862E-18 ) ) ;
#6483 = CARTESIAN_POINT ( 'NONE',  ( -12.78015296493257758, 7.264294661536300879, 16.42255799229593549 ) ) ;
#6484 = CARTESIAN_POINT ( 'NONE',  ( 32.15641333221390141, 7.577415570152255420, -68.01178621890366571 ) ) ;
#6485 = CARTESIAN_POINT ( 'NONE',  ( 61.10129719786242219, 12.23677173834304988, -9.120487640209377744 ) ) ;
#6486 = AXIS2_PLACEMENT_3D ( 'NONE', #11579, #27769, #7377 ) ;
#6487 = CARTESIAN_POINT ( 'NONE',  ( -35.99432170610150195, 10.38324794858010236, 58.58295102095021178 ) ) ;
#6488 = CARTESIAN_POINT ( 'NONE',  ( -8.000000000000000000, -3.867591403079189583, -9.002324684675413025 ) ) ;
#6489 = ORIENTED_EDGE ( 'NONE', *, *, #62229, .T. ) ;
#6490 = COLOUR_RGB ( '',0.7921568627450980005, 0.8196078431372548767, 0.9333333333333333481 ) ;
#6491 = CARTESIAN_POINT ( 'NONE',  ( 188.2091813586561670, 87.61952156613882892, 66.01175409503154867 ) ) ;
#6492 = CARTESIAN_POINT ( 'NONE',  ( -157.0077369422017739, 70.81157624963286423, 64.78427050012133748 ) ) ;
#6493 = CARTESIAN_POINT ( 'NONE',  ( -2.177337698256109899, 7.595833446947582779, -37.95934834430985916 ) ) ;
#6494 = CARTESIAN_POINT ( 'NONE',  ( 106.6228877857910788, 27.24245963308693419, 16.85254313621388533 ) ) ;
#6495 = CARTESIAN_POINT ( 'NONE',  ( -168.9758607987575090, 82.62968668822608720, -89.63544783193323440 ) ) ;
#6496 = CARTESIAN_POINT ( 'NONE',  ( -81.01337222286376516, 23.22902179892323460, -49.75485830830231038 ) ) ;
#6497 = FACE_BOUND ( 'NONE', #30299, .T. ) ;
#6498 = DIRECTION ( 'NONE',  ( -0.5508969814521065267, 0.8345732537212999791, 0.000000000000000000 ) ) ;
#6499 = CARTESIAN_POINT ( 'NONE',  ( 8.683531412707431230, 6.377173148747124820, -67.44837463207127826 ) ) ;
#6500 = CIRCLE ( 'NONE', #58164, 242.4895526022646379 ) ;
#6501 = EDGE_CURVE ( 'NONE', #6937, #3371, #65968, .T. ) ;
#6502 = EDGE_LOOP ( 'NONE', ( #46809, #4929, #29957, #22277 ) ) ;
#6503 = LINE ( 'NONE', #1222, #13627 ) ;
#6504 = FACE_OUTER_BOUND ( 'NONE', #40019, .T. ) ;
#6505 = CARTESIAN_POINT ( 'NONE',  ( -130.5740389938243311, 49.65308610043483384, -36.53356454646863938 ) ) ;
#6506 = CARTESIAN_POINT ( 'NONE',  ( 46.90222083990963853, 9.503928413859245694, -69.72417923928249195 ) ) ;
#6507 = CARTESIAN_POINT ( 'NONE',  ( -417.6627218934913230, 179.4906275429376308, 111.5502958579881749 ) ) ;
#6508 = EDGE_LOOP ( 'NONE', ( #61200, #15158, #29974, #33 ) ) ;
#6509 = ORIENTED_EDGE ( 'NONE', *, *, #37316, .F. ) ;
#6511 = EDGE_CURVE ( 'NONE', #37709, #13713, #64309, .T. ) ;
#6510 = CARTESIAN_POINT ( 'NONE',  ( -129.1194034443450107, 48.65405036159125984, -89.31855732894304367 ) ) ;
#6512 = CARTESIAN_POINT ( 'NONE',  ( -15.47041015649658391, 73.39774458108210808, 170.0000000000000000 ) ) ;
#6513 = VERTEX_POINT ( 'NONE', #63630 ) ;
#6514 = VERTEX_POINT ( 'NONE', #4534 ) ;
#6515 = CARTESIAN_POINT ( 'NONE',  ( 173.6012773665503914, 71.36035397668605640, -44.31334785685113076 ) ) ;
#6516 = EDGE_CURVE ( 'NONE', #6225, #40175, #1686, .T. ) ;
#6517 = CARTESIAN_POINT ( 'NONE',  ( 0.000000000000000000, 0.000000000000000000, 170.0000000000000000 ) ) ;
#6518 = ORIENTED_EDGE ( 'NONE', *, *, #67134, .F. ) ;
#6519 = CARTESIAN_POINT ( 'NONE',  ( 112.1100957124161539, 30.86846953551570394, 56.67668910139203575 ) ) ;
#6520 = ADVANCED_FACE ( 'NONE', ( #4872 ), #68881, .F. ) ;
#6521 = CARTESIAN_POINT ( 'NONE',  ( -37.98601804829807094, 14.28438006995821219, -38.01398195170192906 ) ) ;
#6522 = CARTESIAN_POINT ( 'NONE',  ( 60.40479419793764038, 24.00543350795394915, 40.00000000000003553 ) ) ;
#6523 = DIRECTION ( 'NONE',  ( -1.000000000000000000, 0.000000000000000000, 0.000000000000000000 ) ) ;
#6524 = CARTESIAN_POINT ( 'NONE',  ( 0.2727178028659107412, 0.000000000000000000, 21.02500000000000213 ) ) ;
#6525 = CARTESIAN_POINT ( 'NONE',  ( -189.3111515777349894, 107.1887855376296699, 39.51096003599841566 ) ) ;
#6526 = B_SPLINE_CURVE_WITH_KNOTS ( 'NONE', 3,
 ( #40331, #35059, #7981, #12923, #3059, #29432, #35760, #2022 ),
 .UNSPECIFIED., .F., .F.,
 ( 4, 2, 2, 4 ),
 ( 0.004673709593152156581, 0.005837709341827646004, 0.007001709090503134558, 0.009329708587854115137 ),
 .UNSPECIFIED. ) ;
#6527 = EDGE_LOOP ( 'NONE', ( #17045, #8583, #48179, #6821 ) ) ;
#6528 = CIRCLE ( 'NONE', #28993, 24.99999999999985434 ) ;
#6529 = CARTESIAN_POINT ( 'NONE',  ( -7.329206686002009974E-14, -46.66904755831211560, 85.00100000000000477 ) ) ;
#6530 = CARTESIAN_POINT ( 'NONE',  ( 30.12852347772543737, -74.98256102853682137, 133.5802547743875550 ) ) ;
#6531 = DIRECTION ( 'NONE',  ( 1.000000000000000000, 0.000000000000000000, 0.000000000000000000 ) ) ;
#6532 = CIRCLE ( 'NONE', #45855, 65.00000000000000000 ) ;
#6533 = CARTESIAN_POINT ( 'NONE',  ( 100.0000000000000284, 5.000000000000000000, 18.50000000000000000 ) ) ;
#6535 = ORIENTED_EDGE ( 'NONE', *, *, #1558, .F. ) ;
#6534 = CARTESIAN_POINT ( 'NONE',  ( -126.5249622811510619, 46.90973041002839494, 84.31430626055380628 ) ) ;
#6536 = CARTESIAN_POINT ( 'NONE',  ( -20.55634918610408945, -31.11269837220804035, 0.000000000000000000 ) ) ;
#6537 = AXIS2_PLACEMENT_3D ( 'NONE', #33889, #28246, #60266 ) ;
#6538 = ORIENTED_EDGE ( 'NONE', *, *, #17367, .T. ) ;
#6539 = CARTESIAN_POINT ( 'NONE',  ( -133.3392045760936924, 51.59583146030206535, 37.06569111768722280 ) ) ;
#6540 = CARTESIAN_POINT ( 'NONE',  ( -173.1211646369891355, -170.0000000000000000, 38.32169460664103156 ) ) ;
#6541 = CARTESIAN_POINT ( 'NONE',  ( -5.066666666666671759, 8.000000000000000000, -11.86666666666666536 ) ) ;
#6542 = EDGE_CURVE ( 'NONE', #45708, #47842, #22923, .T. ) ;
#6543 = CARTESIAN_POINT ( 'NONE',  ( 90.30840373526896769, 21.77864858272154081, 30.67197374571127000 ) ) ;
#6544 = CARTESIAN_POINT ( 'NONE',  ( 84.05098130332766004, 18.55728792516086756, -9.429979211940626271 ) ) ;
#6545 = CIRCLE ( 'NONE', #22259, 65.00000000000000000 ) ;
#6546 = CARTESIAN_POINT ( 'NONE',  ( 2.112947028649122760, -24.91054906769651112, 0.000000000000000000 ) ) ;
#6547 = CARTESIAN_POINT ( 'NONE',  ( 89.21005684773501798, 20.31770592753386850, -77.21217177953165844 ) ) ;
#6548 = DIRECTION ( 'NONE',  ( -1.000000000000000000, 0.000000000000000000, 0.000000000000000000 ) ) ;
#6549 = DIRECTION ( 'NONE',  ( -0.000000000000000000, -0.000000000000000000, -1.000000000000000000 ) ) ;
#6550 = EDGE_LOOP ( 'NONE', ( #10957, #9468 ) ) ;
#6551 = EDGE_LOOP ( 'NONE', ( #58643, #8070, #32987, #39910 ) ) ;
#6552 = DIRECTION ( 'NONE',  ( -0.3930250316539278810, 0.9195277725514489076, 0.000000000000000000 ) ) ;
#6553 = DIRECTION ( 'NONE',  ( -0.000000000000000000, 1.000000000000000000, -0.000000000000000000 ) ) ;
#6554 = DIRECTION ( 'NONE',  ( 0.000000000000000000, -0.000000000000000000, 1.000000000000000000 ) ) ;
#6555 = CARTESIAN_POINT ( 'NONE',  ( -25.03927893945753169, 61.76276428842881216, 34.48241795236666718 ) ) ;
#6556 = CARTESIAN_POINT ( 'NONE',  ( 212.1913428512246469, 119.0779339498137688, -44.18048520592454054 ) ) ;
#6557 = CARTESIAN_POINT ( 'NONE',  ( 34.76618902119740540, 54.93755186520760958, 0.000000000000000000 ) ) ;
#6558 = CARTESIAN_POINT ( 'NONE',  ( -103.2129897037410586, 33.25684593987698889, 72.31981736734853428 ) ) ;
#6559 = LINE ( 'NONE', #26464, #41857 ) ;
#6560 = DIRECTION ( 'NONE',  ( -0.000000000000000000, -0.000000000000000000, -1.000000000000000000 ) ) ;
#6561 = EDGE_LOOP ( 'NONE', ( #54504, #19764, #6061, #47746 ) ) ;
#6562 = CARTESIAN_POINT ( 'NONE',  ( -30.46358361599562414, 10.45190018822945177, 18.32402868574788712 ) ) ;
#6563 = ORIENTED_EDGE ( 'NONE', *, *, #33056, .F. ) ;
#6564 = FACE_OUTER_BOUND ( 'NONE', #55655, .T. ) ;
#6565 = CARTESIAN_POINT ( 'NONE',  ( 110.2429982417149574, -170.0000000000000000, -97.11153874658106133 ) ) ;
#6566 = CARTESIAN_POINT ( 'NONE',  ( 141.9165763529819344, -52.00000000000000711, 108.9999999999999858 ) ) ;
#6567 = DIRECTION ( 'NONE',  ( -0.000000000000000000, 1.000000000000000000, -0.000000000000000000 ) ) ;
#6568 = CARTESIAN_POINT ( 'NONE',  ( 36.08914434112045200, 9.014684630517862729, 17.30244423137330045 ) ) ;
#6569 = DIRECTION ( 'NONE',  ( 1.000000000000000000, 0.000000000000000000, 0.000000000000000000 ) ) ;
#6570 = FACE_OUTER_BOUND ( 'NONE', #48929, .T. ) ;
#6571 = DIRECTION ( 'NONE',  ( -1.000000000000000000, 0.000000000000000000, 0.000000000000000000 ) ) ;
#6572 = DIRECTION ( 'NONE',  ( 0.000000000000000000, 0.000000000000000000, 1.000000000000000000 ) ) ;
#6573 = PLANE ( 'NONE',  #21847 ) ;
#6574 = EDGE_LOOP ( 'NONE', ( #32144, #13566 ) ) ;
#6575 = CYLINDRICAL_SURFACE ( 'NONE', #36283, 10.00000000000000178 ) ;
#6576 = CARTESIAN_POINT ( 'NONE',  ( 86.62931800182293784, 20.48449268398422518, 29.71208757247930521 ) ) ;
#6577 = CARTESIAN_POINT ( 'NONE',  ( 14.59045944429442443, -20.30070179093305427, 0.000000000000000000 ) ) ;
#6578 = EDGE_CURVE ( 'NONE', #4364, #56202, #63506, .T. ) ;
#6580 = EDGE_CURVE ( 'NONE', #8790, #22641, #69045, .T. ) ;
#6579 = FACE_OUTER_BOUND ( 'NONE', #7176, .T. ) ;
#6581 = CARTESIAN_POINT ( 'NONE',  ( 6.400000000000000355, 9.237604307034018802, 0.000000000000000000 ) ) ;
#6582 = VECTOR ( 'NONE', #12041, 1000.000000000000000 ) ;
#6583 = CARTESIAN_POINT ( 'NONE',  ( 91.46693946628187177, 22.19998770144037437, 85.16047213861423870 ) ) ;
#6584 = EDGE_CURVE ( 'NONE', #24735, #41495, #13935, .T. ) ;
#6585 = AXIS2_PLACEMENT_3D ( 'NONE', #17131, #49136, #38250 ) ;
#6586 = ORIENTED_EDGE ( 'NONE', *, *, #29227, .T. ) ;
#6587 = CARTESIAN_POINT ( 'NONE',  ( 628.9470371893255560, 913.1618578752636495, 756.5041024077358998 ) ) ;
#6588 = CARTESIAN_POINT ( 'NONE',  ( 63.69186821587179281, -39.51023455020688857, 41.38025477438755928 ) ) ;
#6589 = CARTESIAN_POINT ( 'NONE',  ( -133.1093894320206061, 51.43221067881451347, 9.158613437822465286 ) ) ;
#6590 = DIRECTION ( 'NONE',  ( -0.000000000000000000, 1.000000000000000000, 1.877893248421448789E-16 ) ) ;
#6591 = AXIS2_PLACEMENT_3D ( 'NONE', #32062, #49259, #21492 ) ;
#6592 = CARTESIAN_POINT ( 'NONE',  ( -132.8257891167039872, 52.46553896898736724, -39.53870018935421626 ) ) ;
#6593 = ORIENTED_EDGE ( 'NONE', *, *, #1514, .T. ) ;
#6594 = DIRECTION ( 'NONE',  ( -0.6910626489868685329, 0.7227948638273878901, 0.000000000000000000 ) ) ;
#6595 = CYLINDRICAL_SURFACE ( 'NONE', #32964, 7.500000000000013323 ) ;
#6596 = CARTESIAN_POINT ( 'NONE',  ( -145.5261806899007127, 60.87473129144527917, -21.82853397724819544 ) ) ;
#6597 = CARTESIAN_POINT ( 'NONE',  ( -1.095583923122883663, 7.553030873957008673, -66.44300051098797155 ) ) ;
#6598 = ADVANCED_FACE ( 'NONE', ( #19914 ), #68769, .T. ) ;
#6599 = CARTESIAN_POINT ( 'NONE',  ( -444.4229916354184979, 400.0000000000064801, 96.05029585798874336 ) ) ;
#6600 = ORIENTED_EDGE ( 'NONE', *, *, #51176, .T. ) ;
#6601 = CARTESIAN_POINT ( 'NONE',  ( -60.64199216239837398, 17.30050036439947547, 5.965679938627520329 ) ) ;
#6602 = CARTESIAN_POINT ( 'NONE',  ( 200.8410151090926377, 101.2014854111317703, -37.37915825681574233 ) ) ;
#6603 = EDGE_CURVE ( 'NONE', #47682, #48865, #11766, .T. ) ;
#6604 = FACE_OUTER_BOUND ( 'NONE', #60316, .T. ) ;
#6605 = CARTESIAN_POINT ( 'NONE',  ( 23.09784929786603058, 6.844738137842332648, -41.32192824243960416 ) ) ;
#6607 = ORIENTED_EDGE ( 'NONE', *, *, #8676, .F. ) ;
#6606 = CARTESIAN_POINT ( 'NONE',  ( 116.5100763992442694, 33.01539745157280237, 14.39398281521365064 ) ) ;
#6608 = DIRECTION ( 'NONE',  ( -0.000000000000000000, -0.000000000000000000, 1.000000000000000000 ) ) ;
#6609 = ORIENTED_EDGE ( 'NONE', *, *, #51552, .T. ) ;
#6610 = ORIENTED_EDGE ( 'NONE', *, *, #41999, .T. ) ;
#6611 = CARTESIAN_POINT ( 'NONE',  ( 180.6713229637342693, 79.61878926895388986, 29.30859410551139987 ) ) ;
#6612 = CARTESIAN_POINT ( 'NONE',  ( -34.92258123724119656, 11.21139125453447072, -89.86097876557430197 ) ) ;
#6614 = EDGE_LOOP ( 'NONE', ( #86, #12869, #17143, #25315 ) ) ;
#6613 = CARTESIAN_POINT ( 'NONE',  ( -13.47517652744368633, 8.334971000693560228, -64.80585601353286052 ) ) ;
#6615 = CARTESIAN_POINT ( 'NONE',  ( 0.000000000000000000, 0.000000000000000000, 0.000000000000000000 ) ) ;
#6616 = CARTESIAN_POINT ( 'NONE',  ( 69.77839676787897361, -27.52340539439948586, 170.0000000000000000 ) ) ;
#6617 = CARTESIAN_POINT ( 'NONE',  ( 50.97490815085634352, 6.000000000000000000, -41.68900338898716740 ) ) ;
#6618 = ORIENTED_EDGE ( 'NONE', *, *, #67910, .T. ) ;
#6619 = CARTESIAN_POINT ( 'NONE',  ( 0.000000000000000000, 0.000000000000000000, 170.0000000000000000 ) ) ;
#6620 = CARTESIAN_POINT ( 'NONE',  ( -33.36721086971962080, 9.915747831546610769, -8.720602974680872421 ) ) ;
#6621 = CARTESIAN_POINT ( 'NONE',  ( 152.9731052498706276, 54.23675565345623539, -91.29877024755251114 ) ) ;
#6622 = CARTESIAN_POINT ( 'NONE',  ( -132.4776673493542489, 52.21763813822158085, 7.674206648579892764 ) ) ;
#6623 = CARTESIAN_POINT ( 'NONE',  ( 19.75315861330098599, 7.667327050329334703, 57.98827929678517989 ) ) ;
#6624 = ORIENTED_EDGE ( 'NONE', *, *, #2486, .F. ) ;
#6625 = AXIS2_PLACEMENT_3D ( 'NONE', #17410, #38887, #56101 ) ;
#6626 = VECTOR ( 'NONE', #7830, 1000.000000000000000 ) ;
#6627 = ORIENTED_EDGE ( 'NONE', *, *, #14136, .F. ) ;
#6628 = ORIENTED_EDGE ( 'NONE', *, *, #65770, .F. ) ;
#6629 = CARTESIAN_POINT ( 'NONE',  ( 6.400000000000000355, 9.237604307034018802, 0.000000000000000000 ) ) ;
#6630 = CARTESIAN_POINT ( 'NONE',  ( 447.3372781065085633, 399.9999999999998863, 113.5502958579882034 ) ) ;
#6631 = CARTESIAN_POINT ( 'NONE',  ( 112.3013380801407521, 388.0000000000077307, 96.05029585798746439 ) ) ;
#6632 = CARTESIAN_POINT ( 'NONE',  ( -38.54881010929333485, 10.86689971295294299, -40.37941364402734479 ) ) ;
#6633 = CARTESIAN_POINT ( 'NONE',  ( 63.01563776193090405, 12.67277567978497643, 17.96841034875761878 ) ) ;
#6634 = CARTESIAN_POINT ( 'NONE',  ( 141.9165763529819344, -52.00000000000000711, 108.9999999999999858 ) ) ;
#6635 = PLANE ( 'NONE',  #50738 ) ;
#6636 = CARTESIAN_POINT ( 'NONE',  ( -72.78270026377323632, 21.23376443558119675, -11.09364622117974264 ) ) ;
#6637 = CARTESIAN_POINT ( 'NONE',  ( 31.89651141207616192, -56.63578868294582946, 170.0000000000000000 ) ) ;
#6638 = ORIENTED_EDGE ( 'NONE', *, *, #37538, .F. ) ;
#6639 = CARTESIAN_POINT ( 'NONE',  ( 307.2575771313985342, 20.00000000000003197, 256.6193948016162381 ) ) ;
#6640 = FILL_AREA_STYLE_COLOUR ( '', #26224 ) ;
#6641 = EDGE_LOOP ( 'NONE', ( #22876, #55136, #43742, #23512 ) ) ;
#6642 = CARTESIAN_POINT ( 'NONE',  ( 211.5175447467295839, 116.1901475271413631, -67.53534590373220681 ) ) ;
#6643 = CARTESIAN_POINT ( 'NONE',  ( -5.000000000000000000, 0.000000000000000000, 2.000000000000001776 ) ) ;
#6644 = CARTESIAN_POINT ( 'NONE',  ( -75.43044859198181484, 21.11535168543637653, 17.84392632519180921 ) ) ;
#6645 = LINE ( 'NONE', #17549, #47949 ) ;
#6646 = CARTESIAN_POINT ( 'NONE',  ( -50.14771795543005339, 13.42081263859818385, 5.278126018137767161 ) ) ;
#6647 = CARTESIAN_POINT ( 'NONE',  ( -4.613603609465520172, 74.86839895266042788, 170.0000000000000000 ) ) ;
#6648 = EDGE_CURVE ( 'NONE', #36476, #52936, #41005, .T. ) ;
#6649 = DIRECTION ( 'NONE',  ( -0.000000000000000000, -0.000000000000000000, -1.000000000000000000 ) ) ;
#6650 = EDGE_LOOP ( 'NONE', ( #56529, #21988, #47611, #58341 ) ) ;
#6651 = DIRECTION ( 'NONE',  ( -1.000000000000000000, 0.000000000000000000, 0.000000000000000000 ) ) ;
#6652 = DIRECTION ( 'NONE',  ( -0.000000000000000000, 1.000000000000000000, -0.000000000000000000 ) ) ;
#6653 = ORIENTED_EDGE ( 'NONE', *, *, #64872, .F. ) ;
#6654 = CARTESIAN_POINT ( 'NONE',  ( 0.000000000000000000, 0.000000000000000000, 40.00000000000003553 ) ) ;
#6655 = DIRECTION ( 'NONE',  ( -0.000000000000000000, 1.000000000000000000, -0.000000000000000000 ) ) ;
#6656 = EDGE_LOOP ( 'NONE', ( #30988, #55051, #251, #3624 ) ) ;
#6657 = LINE ( 'NONE', #22839, #1058 ) ;
#6659 = EDGE_CURVE ( 'NONE', #54476, #2896, #67975, .T. ) ;
#6658 = CARTESIAN_POINT ( 'NONE',  ( -29.03891846981454705, 10.22741474064055822, -76.78417915649073677 ) ) ;
#6660 = CARTESIAN_POINT ( 'NONE',  ( 45.76553115525426563, 10.34124506813255095, 33.43704435240822903 ) ) ;
#6661 = DIRECTION ( 'NONE',  ( 0.000000000000000000, 1.000000000000000000, -0.000000000000000000 ) ) ;
#6662 = ADVANCED_FACE ( 'NONE', ( #62473 ), #14963, .T. ) ;
#6663 = VERTEX_POINT ( 'NONE', #63169 ) ;
#6664 = EDGE_CURVE ( 'NONE', #6513, #7998, #51913, .T. ) ;
#6665 = ORIENTED_EDGE ( 'NONE', *, *, #33922, .F. ) ;
#6666 = VECTOR ( 'NONE', #17877, 1000.000000000000000 ) ;
#6667 = DIRECTION ( 'NONE',  ( -0.000000000000000000, -0.000000000000000000, 1.000000000000000000 ) ) ;
#6668 = ORIENTED_EDGE ( 'NONE', *, *, #20192, .T. ) ;
#6669 = CARTESIAN_POINT ( 'NONE',  ( 34.82939798935585429, 8.870855050008911391, -10.31006242790380512 ) ) ;
#6670 = CARTESIAN_POINT ( 'NONE',  ( 5.799999999999999822, -9.237604307034018802, 0.000000000000000000 ) ) ;
#6671 = CARTESIAN_POINT ( 'NONE',  ( -9.119248870808011276, 0.000000000000000000, 4.103571619000548232 ) ) ;
#6672 = CARTESIAN_POINT ( 'NONE',  ( 139.5357843740262069, 46.15750388987612496, 85.78907572748585153 ) ) ;
#6673 = CARTESIAN_POINT ( 'NONE',  ( 198.7583180600454966, 100.1639442742712589, -92.92991841917546481 ) ) ;
#6674 = CARTESIAN_POINT ( 'NONE',  ( 410.0000000000000000, 190.0000000000000000, 2.000000000000000000 ) ) ;
#6675 = VERTEX_POINT ( 'NONE', #14289 ) ;
#6676 = ADVANCED_FACE ( 'NONE', ( #24511 ), #56856, .T. ) ;
#6677 = CARTESIAN_POINT ( 'NONE',  ( -118.9649285217356010, 42.09781191014327106, -72.14050056521936938 ) ) ;
#6678 = ORIENTED_EDGE ( 'NONE', *, *, #37088, .T. ) ;
#6679 = AXIS2_PLACEMENT_3D ( 'NONE', #31791, #27540, #16640 ) ;
#6680 = ORIENTED_EDGE ( 'NONE', *, *, #55858, .T. ) ;
#6681 = CARTESIAN_POINT ( 'NONE',  ( 164.4728833318992542, 63.30716077995683833, -14.07991251278742695 ) ) ;
#6682 = DIRECTION ( 'NONE',  ( -1.000000000000000000, 0.000000000000000000, 0.000000000000000000 ) ) ;
#6683 = CARTESIAN_POINT ( 'NONE',  ( 433.3728120124415568, 400.0000000000067075, -132.4852380479448755 ) ) ;
#6685 = CARTESIAN_POINT ( 'NONE',  ( 137.3861614007145704, 44.78548268714478553, 16.78755531203335138 ) ) ;
#6684 = B_SPLINE_CURVE_WITH_KNOTS ( 'NONE', 3,
 ( #27698, #54416, #64299, #37563, #15429, #43523, #31600, #42157, #4864, #5213, #32639, #69225, #59015, #26671, #48107, #21054, #16794, #5889, #59697, #42501, #21384, #58665, #42827, #16108, #37214, #10831, #32300, #48786, #11509, #43176, #32982, #48434, #37915, #53730, #5553, #271, #631, #27006, #59360, #22082, #65001, #28762, #55477, #6946 ),
 .UNSPECIFIED., .F., .F.,
 ( 4, 2, 2, 2, 2, 2, 2, 2, 2, 2, 2, 2, 2, 2, 2, 2, 2, 2, 2, 2, 2, 4 ),
 ( 0.02416815208377491586, 0.02567033257376879346, 0.02642142281876572879, 0.02717251306376266759, 0.02867469355375654519, 0.02942578379875346664, 0.03017687404375039156, 0.03167905453374424141, 0.03318123502373808431, 0.03393232526873500576, 0.03468341551373193415, 0.03618559600372578400, 0.03693668624872270545, 0.03768777649371962690, 0.03918995698371346287, 0.04069213747370729883, 0.04219431796370114174, 0.04369649845369498464, 0.04444758869869190610, 0.04519867894368882061, 0.04670085943368269821, 0.04820303992367657581 ),
 .UNSPECIFIED. ) ;
#6686 = DIRECTION ( 'NONE',  ( 0.6234898018587431423, -0.7818314824680220321, 0.000000000000000000 ) ) ;
#6687 = AXIS2_PLACEMENT_3D ( 'NONE', #17042, #33947, #27958 ) ;
#6688 = VERTEX_POINT ( 'NONE', #35749 ) ;
#6689 = LINE ( 'NONE', #25571, #26039 ) ;
#6690 = VERTEX_POINT ( 'NONE', #8674 ) ;
#6691 = CARTESIAN_POINT ( 'NONE',  ( 432.4999999999999432, -18.06806526123148160, -2.000000000000000000 ) ) ;
#6692 = VERTEX_POINT ( 'NONE', #30812 ) ;
#6693 = DIRECTION ( 'NONE',  ( 1.000000000000000000, 0.000000000000000000, 0.000000000000000000 ) ) ;
#6694 = ORIENTED_EDGE ( 'NONE', *, *, #28577, .T. ) ;
#6695 = CARTESIAN_POINT ( 'NONE',  ( 6.686525924292799239, -5.377136764700172655, -0.3167204509598466888 ) ) ;
#6696 = AXIS2_PLACEMENT_3D ( 'NONE', #35794, #24207, #57244 ) ;
#6697 = CARTESIAN_POINT ( 'NONE',  ( 92.51858280840788495, 21.51505926344913533, 5.696835879890508991 ) ) ;
#6698 = CARTESIAN_POINT ( 'NONE',  ( -17.36794314067741496, 70.00000000000000000, 24.46128678263259815 ) ) ;
#6699 = ORIENTED_EDGE ( 'NONE', *, *, #35581, .T. ) ;
#6700 = CARTESIAN_POINT ( 'NONE',  ( 8.000000000000007105, 249.8719672152120381, 94.99999999999866418 ) ) ;
#6701 = CARTESIAN_POINT ( 'NONE',  ( 69.36122620657974380, 15.27447566922079858, 94.99999999999866418 ) ) ;
#6702 = CARTESIAN_POINT ( 'NONE',  ( 32.30062460741315533, 8.603096374765343057, 34.98847621939621888 ) ) ;
#6703 = CARTESIAN_POINT ( 'NONE',  ( 67.55199883153194662, 14.80832170058783070, 31.32067154591900504 ) ) ;
#6704 = CARTESIAN_POINT ( 'NONE',  ( -180.4951058960675709, 97.32429862471644810, -94.40723590757134787 ) ) ;
#6705 = DIRECTION ( 'NONE',  ( -0.000000000000000000, -0.000000000000000000, -1.000000000000000000 ) ) ;
#6706 =( REPRESENTATION_RELATIONSHIP ('NONE','NONE', #40274, #19523 ) REPRESENTATION_RELATIONSHIP_WITH_TRANSFORMATION ( #526 )SHAPE_REPRESENTATION_RELATIONSHIP( ) );
#6707 = CARTESIAN_POINT ( 'NONE',  ( 46.68215785206009372, 190.0000000000000000, -77.29788463846088575 ) ) ;
#6708 = VERTEX_POINT ( 'NONE', #9348 ) ;
#6709 = CARTESIAN_POINT ( 'NONE',  ( 141.1220430186941996, 47.19066702031172866, -68.48793956740368571 ) ) ;
#6710 = CARTESIAN_POINT ( 'NONE',  ( -146.1140637052940008, 62.65471088530804877, -75.86152977379298079 ) ) ;
#6711 = VERTEX_POINT ( 'NONE', #47309 ) ;
#6712 = FACE_BOUND ( 'NONE', #67341, .T. ) ;
#6713 = CARTESIAN_POINT ( 'NONE',  ( -7.825402957745087207, 6.891034867348160731, -62.26262132240749736 ) ) ;
#6714 = CARTESIAN_POINT ( 'NONE',  ( 0.000000000000000000, 0.000000000000000000, 43.58025477438756212 ) ) ;
#6715 = CARTESIAN_POINT ( 'NONE',  ( -143.7133518487516710, 60.70463114991426323, -10.69940592156271997 ) ) ;
#6716 = FACE_OUTER_BOUND ( 'NONE', #43158, .T. ) ;
#6717 = ADVANCED_FACE ( 'NONE', ( #19558 ), #41706, .F. ) ;
#6718 = CYLINDRICAL_SURFACE ( 'NONE', #15271, 7.500000000000013323 ) ;
#6719 = CARTESIAN_POINT ( 'NONE',  ( 24.36509522348982060, 70.94296747916789059, 43.58025477438756212 ) ) ;
#6720 = CARTESIAN_POINT ( 'NONE',  ( 112.5093869099859063, 21.56904524376771093, 4.337160898883480442 ) ) ;
#6721 = CARTESIAN_POINT ( 'NONE',  ( -119.5404913382139966, 43.63271406506957817, -73.25228717473794404 ) ) ;
#6722 = CARTESIAN_POINT ( 'NONE',  ( -13.79190010541703337, 8.363435739308565431, 42.18623782823312496 ) ) ;
#6723 = CARTESIAN_POINT ( 'NONE',  ( 162.8142581494935541, 61.92799983924231100, 15.34889811814740490 ) ) ;
#6724 = CARTESIAN_POINT ( 'NONE',  ( 15.55634918610411610, 51.66904755831205875, 2.000000000000001776 ) ) ;
#6725 = ORIENTED_EDGE ( 'NONE', *, *, #53176, .F. ) ;
#6726 = CARTESIAN_POINT ( 'NONE',  ( -38.93938005333174601, 11.96888249046460118, 11.11159176475013766 ) ) ;
#6727 = ORIENTED_EDGE ( 'NONE', *, *, #2556, .F. ) ;
#6728 = DIRECTION ( 'NONE',  ( 0.000000000000000000, 0.000000000000000000, 1.000000000000000000 ) ) ;
#6729 = CARTESIAN_POINT ( 'NONE',  ( 80.16761386260782274, 18.37011649821943848, -74.00622491332923403 ) ) ;
#6730 = CARTESIAN_POINT ( 'NONE',  ( 117.7396772390111437, 33.63508787755782947, 90.38373562684182616 ) ) ;
#6731 = DIRECTION ( 'NONE',  ( -0.000000000000000000, -0.000000000000000000, -1.000000000000000000 ) ) ;
#6732 = CARTESIAN_POINT ( 'NONE',  ( -14.97251655505445633, 7.462297851175272889, 89.00806855038318588 ) ) ;
#6734 = CARTESIAN_POINT ( 'NONE',  ( -25.80443741485378695, 9.749985135376004308, -37.84319293131525797 ) ) ;
#6733 = AXIS2_PLACEMENT_3D ( 'NONE', #63708, #15519, #68627 ) ;
#6735 = CARTESIAN_POINT ( 'NONE',  ( 6.400000000000000355, 9.797174393178825657E-16, -8.000000000000000000 ) ) ;
#6736 = CARTESIAN_POINT ( 'NONE',  ( 117.4396227366912626, -170.0000000000000000, -95.00000000000133582 ) ) ;
#6737 = CARTESIAN_POINT ( 'NONE',  ( -4.610955605663495938, 74.80943656680578613, 41.38025477438755928 ) ) ;
#6738 = VERTEX_POINT ( 'NONE', #22012 ) ;
#6739 = ORIENTED_EDGE ( 'NONE', *, *, #61159, .T. ) ;
#6741 = EDGE_CURVE ( 'NONE', #2171, #45327, #32909, .T. ) ;
#6740 = CARTESIAN_POINT ( 'NONE',  ( 36.30999198706538778, 9.040534725358945423, 71.09571704279858295 ) ) ;
#6742 = CARTESIAN_POINT ( 'NONE',  ( 174.6176230994777825, 72.30829341023250834, 67.49244533490978881 ) ) ;
#6743 = PLANE ( 'NONE',  #28937 ) ;
#6744 = CARTESIAN_POINT ( 'NONE',  ( -166.7050147108374460, 81.70694330787515014, -11.44399333260963303 ) ) ;
#6745 = EDGE_CURVE ( 'NONE', #61117, #57624, #65271, .T. ) ;
#6746 = AXIS2_PLACEMENT_3D ( 'NONE', #10254, #41, #48555 ) ;
#6747 = DIRECTION ( 'NONE',  ( -0.000000000000000000, -0.000000000000000000, -1.000000000000000000 ) ) ;
#6748 = VERTEX_POINT ( 'NONE', #908 ) ;
#6749 = CARTESIAN_POINT ( 'NONE',  ( 106.6181401479172308, 28.34160787025144046, -36.85221939481564135 ) ) ;
#6750 = CARTESIAN_POINT ( 'NONE',  ( -12.39701069459754912, 7.231688578592716077, 58.49449396597306361 ) ) ;
#6751 = DIRECTION ( 'NONE',  ( -1.000000000000000000, 0.000000000000000000, 0.000000000000000000 ) ) ;
#6752 = LINE ( 'NONE', #54222, #44139 ) ;
#6753 = CARTESIAN_POINT ( 'NONE',  ( -51.66904755831212981, -15.55634918610397222, 85.00100000000000477 ) ) ;
#6754 = CARTESIAN_POINT ( 'NONE',  ( 212.0739503583954217, 117.0412199804969617, -18.37996829939370613 ) ) ;
#6755 = FACE_BOUND ( 'NONE', #26345, .T. ) ;
#6756 = CARTESIAN_POINT ( 'NONE',  ( -56.97107423601134002, 15.20373812575556727, -49.98290253789251381 ) ) ;
#6757 = ADVANCED_FACE ( 'NONE', ( #38184 ), #17062, .F. ) ;
#6758 = ORIENTED_EDGE ( 'NONE', *, *, #52575, .T. ) ;
#6759 = CARTESIAN_POINT ( 'NONE',  ( 563.4809901518626702, 188.0000000000000000, 57.79371821540657095 ) ) ;
#6760 = DIRECTION ( 'NONE',  ( 1.000000000000000000, 0.000000000000000000, 0.000000000000000000 ) ) ;
#6761 = CARTESIAN_POINT ( 'NONE',  ( 309.8720357909272707, 0.000000000000000000, 256.6193948016162381 ) ) ;
#6762 = CARTESIAN_POINT ( 'NONE',  ( -180.6215424137752166, 97.48070480470859422, 11.78308709916989550 ) ) ;
#6763 = CARTESIAN_POINT ( 'NONE',  ( 155.2910738464914004, 55.97560547655808705, 2.874285109824962881 ) ) ;
#6764 = AXIS2_PLACEMENT_3D ( 'NONE', #9599, #31061, #56396 ) ;
#6765 = ADVANCED_FACE ( 'NONE', ( #11104 ), #20978, .T. ) ;
#6766 = EDGE_CURVE ( 'NONE', #41218, #23252, #59978, .T. ) ;
#6767 = PLANE ( 'NONE',  #54681 ) ;
#6768 = ORIENTED_EDGE ( 'NONE', *, *, #56706, .F. ) ;
#6769 = CARTESIAN_POINT ( 'NONE',  ( 55.52750043885183828, 11.05966813607792254, 9.978530875651303589 ) ) ;
#6770 = CARTESIAN_POINT ( 'NONE',  ( 0.000000000000000000, 0.000000000000000000, 170.0000000000000000 ) ) ;
#6771 = ORIENTED_EDGE ( 'NONE', *, *, #43046, .T. ) ;
#6772 = ORIENTED_EDGE ( 'NONE', *, *, #9851, .T. ) ;
#6773 = DIRECTION ( 'NONE',  ( -1.000000000000000000, 0.000000000000000000, 0.000000000000000000 ) ) ;
#6774 = CARTESIAN_POINT ( 'NONE',  ( -57.65574514524055871, 16.43983577669856189, -22.90970587626445365 ) ) ;
#6775 = CARTESIAN_POINT ( 'NONE',  ( 103.8317086685000135, 26.02720265156214197, 41.01109807538037444 ) ) ;
#6776 = EDGE_LOOP ( 'NONE', ( #2142, #56466, #43071, #32842 ) ) ;
#6777 = VERTEX_POINT ( 'NONE', #37148 ) ;
#6778 = CARTESIAN_POINT ( 'NONE',  ( 0.000000000000000000, 0.000000000000000000, 41.38025477438755928 ) ) ;
#6779 = PLANE ( 'NONE',  #31489 ) ;
#6780 = CIRCLE ( 'NONE', #216, 4.171999999999999709 ) ;
#6781 = LINE ( 'NONE', #22968, #54070 ) ;
#6782 = CARTESIAN_POINT ( 'NONE',  ( 67.93317348534930034, 14.90531593353391848, 16.15235655697943429 ) ) ;
#6783 = DIRECTION ( 'NONE',  ( -1.000000000000000000, -1.850474763383843014E-16, 1.697708136181793677E-16 ) ) ;
#6784 = CARTESIAN_POINT ( 'NONE',  ( -50.53243683205840853, 14.55237037207940709, -36.71190027716730242 ) ) ;
#6785 = CARTESIAN_POINT ( 'NONE',  ( 15.78827728214693416, -170.0000000000000000, -69.86349468914949057 ) ) ;
#6786 = CYLINDRICAL_SURFACE ( 'NONE', #59485, 65.00000000000000000 ) ;
#6787 = DIRECTION ( 'NONE',  ( -0.000000000000000000, -0.000000000000000000, -1.000000000000000000 ) ) ;
#6788 = CARTESIAN_POINT ( 'NONE',  ( -31.11269837220809364, -10.55634918610397932, 0.000000000000000000 ) ) ;
#6789 = CYLINDRICAL_SURFACE ( 'NONE', #9624, 65.36598343705435354 ) ;
#6791 = ORIENTED_EDGE ( 'NONE', *, *, #24005, .T. ) ;
#6790 = DIRECTION ( 'NONE',  ( -1.000000000000000000, 0.000000000000000000, 0.000000000000000000 ) ) ;
#6792 = VERTEX_POINT ( 'NONE', #47691 ) ;
#6793 = VECTOR ( 'NONE', #65656, 1000.000000000000227 ) ;
#6794 = VERTEX_POINT ( 'NONE', #69156 ) ;
#6795 = LINE ( 'NONE', #22985, #3189 ) ;
#6796 = CARTESIAN_POINT ( 'NONE',  ( -170.5404825127988033, 85.78476310886819078, 84.96378268994482141 ) ) ;
#6797 = CARTESIAN_POINT ( 'NONE',  ( -48.56549579811110817, 13.03742088415615896, -12.07592667915758611 ) ) ;
#6798 = EDGE_CURVE ( 'NONE', #1784, #51862, #11794, .T. ) ;
#6799 = CARTESIAN_POINT ( 'NONE',  ( 108.3819860115547300, 28.02992728837240932, -23.85848975555797580 ) ) ;
#6800 = CARTESIAN_POINT ( 'NONE',  ( -62.06231780744544579, 17.72446026058424806, -40.03704603771073778 ) ) ;
#6801 = CARTESIAN_POINT ( 'NONE',  ( -34.47910341156048020, 23.50544998411836772, 13.79046412380261621 ) ) ;
#6802 = CARTESIAN_POINT ( 'NONE',  ( -71.16584859396995455, 19.60484997908768179, -69.22503646584482340 ) ) ;
#6803 = CARTESIAN_POINT ( 'NONE',  ( 21.44031696305385282, 6.747195267824409370, -11.22020411404090012 ) ) ;
#6805 = ORIENTED_EDGE ( 'NONE', *, *, #19457, .F. ) ;
#6804 = ADVANCED_FACE ( 'NONE', ( #52968 ), #26260, .F. ) ;
#6806 = PLANE ( 'NONE',  #63259 ) ;
#6808 = EDGE_CURVE ( 'NONE', #52737, #49963, #59288, .T. ) ;
#6807 = EDGE_LOOP ( 'NONE', ( #20423, #68819, #14156, #34926 ) ) ;
#6809 = ORIENTED_EDGE ( 'NONE', *, *, #6511, .F. ) ;
#6810 = LINE ( 'NONE', #39523, #32095 ) ;
#6811 = CARTESIAN_POINT ( 'NONE',  ( -58.54432058204184841, 16.69162069828844253, -89.76429277260994866 ) ) ;
#6812 = CARTESIAN_POINT ( 'NONE',  ( 0.000000000000000000, -52.00000000000000711, 0.000000000000000000 ) ) ;
#6813 = VECTOR ( 'NONE', #11142, 1000.000000000000000 ) ;
#6814 = CARTESIAN_POINT ( 'NONE',  ( 116.0963032583227914, 32.80867113471307306, -21.29345617767813437 ) ) ;
#6815 = LINE ( 'NONE', #28265, #39439 ) ;
#6816 = DIRECTION ( 'NONE',  ( -0.000000000000000000, -0.000000000000000000, 1.000000000000000000 ) ) ;
#6817 = CARTESIAN_POINT ( 'NONE',  ( 137.3861614007144851, 44.78548268714477132, -10.05699527843033181 ) ) ;
#6818 = EDGE_LOOP ( 'NONE', ( #40697, #28804, #34762, #10078 ) ) ;
#6819 = EDGE_CURVE ( 'NONE', #44163, #59279, #55688, .T. ) ;
#6820 = ORIENTED_EDGE ( 'NONE', *, *, #36756, .T. ) ;
#6821 = ORIENTED_EDGE ( 'NONE', *, *, #45518, .F. ) ;
#6822 = EDGE_CURVE ( 'NONE', #42101, #40754, #62676, .T. ) ;
#6823 = CARTESIAN_POINT ( 'NONE',  ( 0.000000000000000000, -27.00000000000000355, 15.00000000000000000 ) ) ;
#6824 = DIRECTION ( 'NONE',  ( 0.000000000000000000, 0.000000000000000000, 1.000000000000000000 ) ) ;
#6825 = DIRECTION ( 'NONE',  ( -0.000000000000000000, -0.000000000000000000, 1.000000000000000000 ) ) ;
#6826 = CARTESIAN_POINT ( 'NONE',  ( 61.09275639403235658, 12.23448398202909715, -23.64161583801792688 ) ) ;
#6827 = ADVANCED_FACE ( 'NONE', ( #60689 ), #54706, .T. ) ;
#6828 = EDGE_CURVE ( 'NONE', #58537, #67063, #12507, .T. ) ;
#6829 = LINE ( 'NONE', #44467, #23697 ) ;
#6830 = DIRECTION ( 'NONE',  ( 0.000000000000000000, -1.224646799147351975E-16, 1.000000000000000000 ) ) ;
#6831 = ORIENTED_EDGE ( 'NONE', *, *, #1246, .T. ) ;
#6832 = CARTESIAN_POINT ( 'NONE',  ( 186.2680729609084551, 85.48839327635664631, 58.21274974874516772 ) ) ;
#6833 = CARTESIAN_POINT ( 'NONE',  ( 197.6341357773624736, 98.74251867088338486, -68.13172239288054755 ) ) ;
#6834 = CARTESIAN_POINT ( 'NONE',  ( 0.000000000000000000, -31.50328976398030534, -9.999999999999998224 ) ) ;
#6835 = LINE ( 'NONE', #32189, #53156 ) ;
#6836 = CARTESIAN_POINT ( 'NONE',  ( -165.6393662153604112, 79.16886183052817216, 12.08284213267020846 ) ) ;
#6837 = PLANE ( 'NONE',  #43037 ) ;
#6838 = FACE_BOUND ( 'NONE', #9492, .T. ) ;
#6839 = FACE_OUTER_BOUND ( 'NONE', #47891, .T. ) ;
#6840 = EDGE_CURVE ( 'NONE', #10412, #60955, #55768, .T. ) ;
#6841 = ORIENTED_EDGE ( 'NONE', *, *, #46881, .T. ) ;
#6842 = CARTESIAN_POINT ( 'NONE',  ( 122.2516123306975402, 190.0000000000000000, -21.28179539054375624 ) ) ;
#6843 = CIRCLE ( 'NONE', #67521, 4.999999999999990230 ) ;
#6844 = CARTESIAN_POINT ( 'NONE',  ( -132.9109786433856755, 51.29129389542018913, -66.59759312975943146 ) ) ;
#6845 = CARTESIAN_POINT ( 'NONE',  ( -103.8932886509197004, 34.74144483217663293, -76.68729370199592665 ) ) ;
#6846 = ADVANCED_FACE ( 'NONE', ( #23062 ), #39246, .T. ) ;
#6847 = DIRECTION ( 'NONE',  ( -0.000000000000000000, -0.000000000000000000, -1.000000000000000000 ) ) ;
#6848 = EDGE_CURVE ( 'NONE', #34711, #44967, #33965, .T. ) ;
#6849 = CARTESIAN_POINT ( 'NONE',  ( 62.04382205963241148, 13.48099884269680793, -62.61244101702975939 ) ) ;
#6850 = ORIENTED_EDGE ( 'NONE', *, *, #7053, .T. ) ;
#6851 = PRODUCT_DEFINITION_SHAPE ( 'NONE', 'NONE',  #69626 ) ;
#6852 = AXIS2_PLACEMENT_3D ( 'NONE', #35683, #2980, #8249 ) ;
#6853 = ORIENTED_EDGE ( 'NONE', *, *, #17658, .T. ) ;
#6854 = CARTESIAN_POINT ( 'NONE',  ( 5.260074602449203133E-16, -0.7818963811860513147, -8.000000000000000000 ) ) ;
#6855 = CARTESIAN_POINT ( 'NONE',  ( 183.4744593358819031, 81.05536227200067856, 83.38285715921820440 ) ) ;
#6856 = VERTEX_POINT ( 'NONE', #18479 ) ;
#6857 = VECTOR ( 'NONE', #3338, 1000.000000000000000 ) ;
#6858 = ORIENTED_EDGE ( 'NONE', *, *, #8268, .F. ) ;
#6859 = CARTESIAN_POINT ( 'NONE',  ( 181.0840389613909736, 78.60582251573003987, -36.22505766587961062 ) ) ;
#6860 = CARTESIAN_POINT ( 'NONE',  ( 157.4703587214989113, 58.92748579479261650, 29.40946747225336466 ) ) ;
#6861 = CARTESIAN_POINT ( 'NONE',  ( -20.55634918610403261, 2.818925648462311528E-14, 85.00100000000000477 ) ) ;
#6862 = ORIENTED_EDGE ( 'NONE', *, *, #67221, .T. ) ;
#6863 = CARTESIAN_POINT ( 'NONE',  ( 110.2429982417149432, 29.99119854320847267, 56.45576479620100940 ) ) ;
#6864 = CARTESIAN_POINT ( 'NONE',  ( 138.2136629441929472, 45.30947856186676859, 57.73192867322060806 ) ) ;
#6865 = CARTESIAN_POINT ( 'NONE',  ( -72.76696720809545127, 20.16136115364207626, -37.95795318151130004 ) ) ;
#6866 = VECTOR ( 'NONE', #7852, 1000.000000000000000 ) ;
#6867 = LINE ( 'NONE', #1958, #67456 ) ;
#6868 = CARTESIAN_POINT ( 'NONE',  ( 54.16779028252168615, 21.66464678626688567, 27.58472369380032774 ) ) ;
#6869 = CARTESIAN_POINT ( 'NONE',  ( -3.306248862503413655, 500.0000000000000000, -91.64566090791306863 ) ) ;
#6870 = ORIENTED_EDGE ( 'NONE', *, *, #38442, .T. ) ;
#6871 = CARTESIAN_POINT ( 'NONE',  ( 116.5096233816161941, 31.89062767870469273, -47.55059037069165129 ) ) ;
#6872 = CARTESIAN_POINT ( 'NONE',  ( -72.21889834709580214, 21.03534256744168829, 14.93684858560963136 ) ) ;
#6873 = CARTESIAN_POINT ( 'NONE',  ( -142.0227972901369071, 59.36121938936276621, -42.86931618990738713 ) ) ;
#6874 = CARTESIAN_POINT ( 'NONE',  ( 32.06997139192709056, 56.95813133885486934, 6.377659838150122832E-18 ) ) ;
#6876 = ORIENTED_EDGE ( 'NONE', *, *, #42110, .F. ) ;
#6875 = CARTESIAN_POINT ( 'NONE',  ( -128.1931195763440883, 48.02619254066235044, 84.66445025086169096 ) ) ;
#6877 = CARTESIAN_POINT ( 'NONE',  ( 62.52762183777208094, 13.59210632617624803, 17.96841034875761878 ) ) ;
#6878 = ORIENTED_EDGE ( 'NONE', *, *, #37544, .T. ) ;
#6879 = CARTESIAN_POINT ( 'NONE',  ( -128.7810612886106298, 48.42424427998344783, 31.19417675835600434 ) ) ;
#6880 = CARTESIAN_POINT ( 'NONE',  ( 22.91085886047801168, 30.73415265233982296, 13.32819299319723605 ) ) ;
#6881 = LINE ( 'NONE', #39596, #14118 ) ;
#6882 = CARTESIAN_POINT ( 'NONE',  ( 182.7720841008444097, 80.32850885226591231, -24.19120961474466114 ) ) ;
#6883 = CARTESIAN_POINT ( 'NONE',  ( 138.2204650371259049, 44.12203217345470563, -10.56042420382598834 ) ) ;
#6884 = DIRECTION ( 'NONE',  ( -0.000000000000000000, -0.000000000000000000, -1.000000000000000000 ) ) ;
#6885 = CARTESIAN_POINT ( 'NONE',  ( 91.13361825170458985, 21.00701373666981198, -64.14955825547987445 ) ) ;
#6886 = EDGE_CURVE ( 'NONE', #52688, #18508, #29046, .T. ) ;
#6887 = CARTESIAN_POINT ( 'NONE',  ( 89.99999999999998579, 0.000000000000000000, -7.000000000000000000 ) ) ;
#6888 = CARTESIAN_POINT ( 'NONE',  ( 50.98853755884156413, 400.0000000000065938, -133.9497041420122798 ) ) ;
#6889 = ORIENTED_EDGE ( 'NONE', *, *, #66647, .F. ) ;
#6890 = ORIENTED_EDGE ( 'NONE', *, *, #63616, .F. ) ;
#6891 = VECTOR ( 'NONE', #43073, 1000.000000000000000 ) ;
#6892 = CARTESIAN_POINT ( 'NONE',  ( 44.35071890818839790, 9.104600422692273654, 43.07060720302936829 ) ) ;
#6893 = CARTESIAN_POINT ( 'NONE',  ( 0.3167204509598363082, 5.377136764700156668, 6.686525924292793022 ) ) ;
#6894 = DIRECTION ( 'NONE',  ( 0.000000000000000000, 0.000000000000000000, -1.000000000000000000 ) ) ;
#6895 = CYLINDRICAL_SURFACE ( 'NONE', #34070, 7.500000000000013323 ) ;
#6896 = CARTESIAN_POINT ( 'NONE',  ( 210.0122310839192039, 115.7355030290287488, -38.51083372022162621 ) ) ;
#6897 = VECTOR ( 'NONE', #42343, 1000.000000000000000 ) ;
#6898 = LINE ( 'NONE', #28354, #23633 ) ;
#6899 = CARTESIAN_POINT ( 'NONE',  ( -125.8938041572051105, 46.49392987655494380, -34.91370389823391918 ) ) ;
#6900 = CARTESIAN_POINT ( 'NONE',  ( -30.46060138092287062, 9.432375387772216513, -35.36506637325409486 ) ) ;
#6901 = DIRECTION ( 'NONE',  ( -0.8118923937861950435, -0.5838071093367415143, 0.000000000000000000 ) ) ;
#6902 = EDGE_CURVE ( 'NONE', #50073, #34263, #55055, .T. ) ;
#6903 = PRODUCT_DEFINITION_SHAPE ( 'NONE', 'NONE',  #69594 ) ;
#6904 = ORIENTED_EDGE ( 'NONE', *, *, #54962, .F. ) ;
#6905 = CARTESIAN_POINT ( 'NONE',  ( 0.000000000000000000, 0.000000000000000000, 170.0000000000000000 ) ) ;
#6906 = VERTEX_POINT ( 'NONE', #12865 ) ;
#6907 = VECTOR ( 'NONE', #42934, 1000.000000000000114 ) ;
#6908 =( GEOMETRIC_REPRESENTATION_CONTEXT ( 3 ) GLOBAL_UNCERTAINTY_ASSIGNED_CONTEXT ( ( #62733 ) ) GLOBAL_UNIT_ASSIGNED_CONTEXT ( ( #68183, #44094, #12455 ) ) REPRESENTATION_CONTEXT ( 'NONE', 'WORKASPACE' ) );
#6909 = DIRECTION ( 'NONE',  ( 1.387778780781446169E-16, -1.000000000000000000, -3.469446951953615421E-17 ) ) ;
#6910 = CARTESIAN_POINT ( 'NONE',  ( 7.484861546145031852, 64.56761454192836425, 73.58025477438756923 ) ) ;
#6911 = ADVANCED_FACE ( 'NONE', ( #2649 ), #7925, .F. ) ;
#6912 = CARTESIAN_POINT ( 'NONE',  ( -84.96580414052105823, 24.82184094495580240, 68.84061359761649612 ) ) ;
#6913 = CARTESIAN_POINT ( 'NONE',  ( 129.5225439633633755, 40.02995148249141266, 30.87120519579052313 ) ) ;
#6914 = CARTESIAN_POINT ( 'NONE',  ( -25.99999999999994671, 0.000000000000000000, -104.9999999999999858 ) ) ;
#6915 = ADVANCED_FACE ( 'NONE', ( #28326, #45549 ), #67035, .T. ) ;
#6916 = CARTESIAN_POINT ( 'NONE',  ( -452.6627218934914367, 399.9999999999998863, -111.4497041420118251 ) ) ;
#6917 = AXIS2_PLACEMENT_3D ( 'NONE', #37014, #46877, #9940 ) ;
#6918 = CARTESIAN_POINT ( 'NONE',  ( -102.2801239173131194, 33.91021738430207222, -23.17002667451225406 ) ) ;
#6919 = B_SPLINE_CURVE_WITH_KNOTS ( 'NONE', 3,
 ( #19338, #14419, #3509, #24979, #3176, #40110, #8802, #46411, #56629, #34843, #29902, #40450, #35871, #13382, #61895, #30595, #40794, #62249 ),
 .UNSPECIFIED., .F., .F.,
 ( 4, 2, 2, 2, 2, 2, 2, 2, 4 ),
 ( 0.000000000000000000, 0.001360351328785557685, 0.002040526993178300424, 0.002720702657571043813, 0.004081053986356537530, 0.005441405315142032115, 0.006801756643927526699, 0.008162107972713021284, 0.01088281063028401045 ),
 .UNSPECIFIED. ) ;
#6920 = CARTESIAN_POINT ( 'NONE',  ( 32.23328838621442571, -26.50150695468921214, 13.79046412417416789 ) ) ;
#6921 = CARTESIAN_POINT ( 'NONE',  ( 0.000000000000000000, 0.000000000000000000, 41.38025477438755928 ) ) ;
#6922 = DIRECTION ( 'NONE',  ( 0.000000000000000000, 0.000000000000000000, 1.000000000000000000 ) ) ;
#6923 = ORIENTED_EDGE ( 'NONE', *, *, #62743, .F. ) ;
#6924 = DIRECTION ( 'NONE',  ( 0.000000000000000000, 1.000000000000000000, -1.479221584281239571E-31 ) ) ;
#6925 = SURFACE_STYLE_FILL_AREA ( #22753 ) ;
#6926 = CARTESIAN_POINT ( 'NONE',  ( -8.810383862755523765, 7.965311326754785703, 18.22247569387398158 ) ) ;
#6927 = CARTESIAN_POINT ( 'NONE',  ( -65.36598343705435354, 0.000000000000000000, 41.38025477438755928 ) ) ;
#6928 = DIRECTION ( 'NONE',  ( -0.8090169943749506709, 0.5877852522924686962, 0.000000000000000000 ) ) ;
#6929 = CARTESIAN_POINT ( 'NONE',  ( -95.07081908554464178, 29.26686063496962120, -94.08517559775140171 ) ) ;
#6930 = ORIENTED_EDGE ( 'NONE', *, *, #17658, .F. ) ;
#6931 = PRODUCT_CONTEXT ( 'NONE', #28708, 'mechanical' ) ;
#6932 = CARTESIAN_POINT ( 'NONE',  ( 20.89850557012451659, -13.94239061780404043, 0.000000000000000000 ) ) ;
#6933 = CARTESIAN_POINT ( 'NONE',  ( -38.17232309348612773, 11.81874355808867705, -39.47676223961260433 ) ) ;
#6934 = EDGE_CURVE ( 'NONE', #15138, #69105, #23030, .T. ) ;
#6935 = CARTESIAN_POINT ( 'NONE',  ( -168.0003605155415016, 83.06333427281273885, -47.69718177220133271 ) ) ;
#6936 = CARTESIAN_POINT ( 'NONE',  ( -165.8118651643725059, 79.34448671302054379, 90.28955021999587416 ) ) ;
#6937 = VERTEX_POINT ( 'NONE', #8966 ) ;
#6938 = DIRECTION ( 'NONE',  ( -0.000000000000000000, -0.000000000000000000, -1.000000000000000000 ) ) ;
#6939 = DIRECTION ( 'NONE',  ( -1.734723475976805517E-15, 0.000000000000000000, -1.000000000000000000 ) ) ;
#6940 = ADVANCED_FACE ( 'NONE', ( #8277 ), #14917, .T. ) ;
#6941 = PLANE ( 'NONE',  #35866 ) ;
#6942 = CARTESIAN_POINT ( 'NONE',  ( -2.172839205444465627, 7.595638683704374117, -74.71678878236892274 ) ) ;
#6943 = DIRECTION ( 'NONE',  ( -1.000000000000000000, 0.000000000000000000, 0.000000000000000000 ) ) ;
#6944 = VERTEX_POINT ( 'NONE', #68400 ) ;
#6945 = DIRECTION ( 'NONE',  ( -1.000000000000000000, 0.000000000000000000, 0.000000000000000000 ) ) ;
#6946 = CARTESIAN_POINT ( 'NONE',  ( 86.62931800182293784, 20.48449268398423584, 17.86753698201564688 ) ) ;
#6947 = CARTESIAN_POINT ( 'NONE',  ( -96.02159028238557426, 30.82695531378848486, 42.15941767080024505 ) ) ;
#6948 = AXIS2_PLACEMENT_3D ( 'NONE', #19833, #41289, #36353 ) ;
#6949 = LINE ( 'NONE', #18898, #5612 ) ;
#6950 = CIRCLE ( 'NONE', #48438, 243.4957430088094839 ) ;
#6952 = ORIENTED_EDGE ( 'NONE', *, *, #12726, .F. ) ;
#6951 = CARTESIAN_POINT ( 'NONE',  ( -4.999999999999936939, 31.11269837220806167, 2.000000000000001776 ) ) ;
#6953 = DIRECTION ( 'NONE',  ( -1.000000000000000000, -0.000000000000000000, -0.000000000000000000 ) ) ;
#6954 = ORIENTED_EDGE ( 'NONE', *, *, #54151, .F. ) ;
#6955 = AXIS2_PLACEMENT_3D ( 'NONE', #53845, #5663, #38379 ) ;
#6956 = EDGE_LOOP ( 'NONE', ( #35684, #60493, #21224, #39983 ) ) ;
#6957 = CARTESIAN_POINT ( 'NONE',  ( -118.5480034463614629, 41.84363520065495123, -94.51110357902348369 ) ) ;
#6959 = CARTESIAN_POINT ( 'NONE',  ( -38.78626392836186909, 11.93872315530319916, -95.00000000000133582 ) ) ;
#6958 = AXIS2_PLACEMENT_3D ( 'NONE', #48119, #36556, #41489 ) ;
#6961 = ORIENTED_EDGE ( 'NONE', *, *, #32632, .F. ) ;
#6960 = CARTESIAN_POINT ( 'NONE',  ( -7.825402957745087207, 7.899365992529248537, -62.26262132240749736 ) ) ;
#6962 = CARTESIAN_POINT ( 'NONE',  ( 164.3577270662354408, 63.21061577643033758, 33.92876650929636639 ) ) ;
#6963 = CLOSED_SHELL ( 'NONE', ( #60211, #67512, #40431, #9371, #67043, #24788, #37880, #33756, #65184, #28841, #896, #68548, #35695, #21448, #68969, #49345, #68203, #15940, #5619 ) ) ;
#6964 = DIRECTION ( 'NONE',  ( 1.000000000000000000, 0.000000000000000000, 0.000000000000000000 ) ) ;
#6965 = CARTESIAN_POINT ( 'NONE',  ( -74.81012118577224612, 5.477980300262961677, 170.0000000000000000 ) ) ;
#6966 = PRODUCT_RELATED_PRODUCT_CATEGORY ( 'part', '', ( #38327 ) ) ;
#6967 = VERTEX_POINT ( 'NONE', #51533 ) ;
#6968 = FACE_OUTER_BOUND ( 'NONE', #36495, .T. ) ;
#6969 = EDGE_CURVE ( 'NONE', #24447, #26335, #36538, .T. ) ;
#6970 = CARTESIAN_POINT ( 'NONE',  ( -34.06864996337442619, 10.03773626259442153, -8.944471349985661845 ) ) ;
#6971 = ADVANCED_FACE ( 'NONE', ( #9304 ), #40616, .F. ) ;
#6972 = CARTESIAN_POINT ( 'NONE',  ( 0.000000000000000000, 6.000000000000000000, -46.99999999999997158 ) ) ;
#6973 = CARTESIAN_POINT ( 'NONE',  ( -133.1640943168118554, 52.70734926280009347, 13.13691334606962613 ) ) ;
#6974 = CARTESIAN_POINT ( 'NONE',  ( 23.28809538736929241, 7.864824219997537114, 64.85145018203481015 ) ) ;
#6975 = ORIENTED_EDGE ( 'NONE', *, *, #42870, .T. ) ;
#6976 = ORIENTED_EDGE ( 'NONE', *, *, #57804, .T. ) ;
#6977 = VERTEX_POINT ( 'NONE', #62430 ) ;
#6978 = CARTESIAN_POINT ( 'NONE',  ( 86.62931800182293784, -170.0000000000000000, 44.71208757247933363 ) ) ;
#6979 = CARTESIAN_POINT ( 'NONE',  ( 181.0840389613909736, 78.60582251573005408, -63.06960825634327961 ) ) ;
#6980 = PLANE ( 'NONE',  #36971 ) ;
#6981 = CARTESIAN_POINT ( 'NONE',  ( -1.224646799147352468E-15, 19.01593100277520421, 6.196318915105386793 ) ) ;
#6982 = CARTESIAN_POINT ( 'NONE',  ( -100.8462079694196945, 32.05831806546150631, 84.34044455310514365 ) ) ;
#6983 = CARTESIAN_POINT ( 'NONE',  ( -31.11269837220804035, 15.55634918610408945, 85.00100000000000477 ) ) ;
#6984 = CARTESIAN_POINT ( 'NONE',  ( -133.3958821919893012, 51.63629593114586669, 64.45030094466832793 ) ) ;
#6985 = CARTESIAN_POINT ( 'NONE',  ( -75.00452312211126582, 22.03104735285382176, -22.32063719065431329 ) ) ;
#6986 = EDGE_CURVE ( 'NONE', #6690, #44138, #3676, .T. ) ;
#6987 = ORIENTED_EDGE ( 'NONE', *, *, #48024, .F. ) ;
#6988 = CARTESIAN_POINT ( 'NONE',  ( 80.72161230109723817, 17.48902961068032980, 59.40974494857174193 ) ) ;
#6989 = ORIENTED_EDGE ( 'NONE', *, *, #4518, .F. ) ;
#6990 = CARTESIAN_POINT ( 'NONE',  ( 32.90953848114693869, 7.653665824624196645, 33.65092423327369175 ) ) ;
#6991 = EDGE_CURVE ( 'NONE', #27549, #62345, #36388, .T. ) ;
#6992 = VERTEX_POINT ( 'NONE', #36041 ) ;
#6993 = CARTESIAN_POINT ( 'NONE',  ( 185.1802655733641245, 82.84606286178494372, 43.10721277487510150 ) ) ;
#6994 = CARTESIAN_POINT ( 'NONE',  ( 39.40195752203892710, 9.424259417798131366, -23.77526687496409608 ) ) ;
#6995 = EDGE_CURVE ( 'NONE', #34341, #41500, #19660, .T. ) ;
#6996 = LINE ( 'NONE', #34089, #60070 ) ;
#6997 = CARTESIAN_POINT ( 'NONE',  ( -118.8691191306315034, 43.21907118237572121, 67.60517970726668580 ) ) ;
#6998 = CARTESIAN_POINT ( 'NONE',  ( -50.13771638889895144, 13.41835215703894235, 16.65896950491509898 ) ) ;
#6999 = VECTOR ( 'NONE', #38253, 1000.000000000000000 ) ;
#7000 = CARTESIAN_POINT ( 'NONE',  ( 150.0433793199863430, 52.09973307442955814, -44.70445035943132694 ) ) ;
#7001 = CARTESIAN_POINT ( 'NONE',  ( -4.000000000000009770, -6.928203230275505220, -9.500000000000000000 ) ) ;
#7002 = EDGE_LOOP ( 'NONE', ( #5421, #66848, #37262, #64584 ) ) ;
#7003 = VECTOR ( 'NONE', #56273, 1000.000000000000000 ) ;
#7004 = DIRECTION ( 'NONE',  ( 0.000000000000000000, 0.000000000000000000, -1.000000000000000000 ) ) ;
#7005 = CARTESIAN_POINT ( 'NONE',  ( 0.000000000000000000, 0.000000000000000000, 0.000000000000000000 ) ) ;
#7006 = ORIENTED_EDGE ( 'NONE', *, *, #51305, .T. ) ;
#7007 = LINE ( 'NONE', #23545, #56715 ) ;
#7008 = DIRECTION ( 'NONE',  ( -0.000000000000000000, 1.000000000000000000, -0.000000000000000000 ) ) ;
#7009 = CARTESIAN_POINT ( 'NONE',  ( 26.11269837220806167, -6.375108774214766072E-14, 85.00100000000000477 ) ) ;
#7010 = ORIENTED_EDGE ( 'NONE', *, *, #52782, .T. ) ;
#7011 = DIRECTION ( 'NONE',  ( 1.000000000000000000, 0.000000000000000000, 0.000000000000000000 ) ) ;
#7012 = CARTESIAN_POINT ( 'NONE',  ( 150.4722669492348643, 53.65054032737663192, -73.17996140608711642 ) ) ;
#7013 = CARTESIAN_POINT ( 'NONE',  ( 44.34362023773823580, 10.12115849931653244, 31.75035674218548820 ) ) ;
#7014 = VECTOR ( 'NONE', #55877, 999.9999999999998863 ) ;
#7015 = CARTESIAN_POINT ( 'NONE',  ( -24.94151142167915935, 8.614613465433023975, 60.78288318456196038 ) ) ;
#7016 = ORIENTED_EDGE ( 'NONE', *, *, #17879, .T. ) ;
#7017 = ORIENTED_EDGE ( 'NONE', *, *, #941, .T. ) ;
#7018 = LINE ( 'NONE', #12296, #51437 ) ;
#7019 = VERTEX_POINT ( 'NONE', #14245 ) ;
#7020 = CARTESIAN_POINT ( 'NONE',  ( 33.44035656425387515, 8.720466003183668491, -11.69816230808393875 ) ) ;
#7021 = CARTESIAN_POINT ( 'NONE',  ( -31.11269837220801193, 31.11269837220812207, 2.000000000000001776 ) ) ;
#7022 = CARTESIAN_POINT ( 'NONE',  ( -31.43908319763709969, 9.591432048623765638, -77.16174795566554678 ) ) ;
#7023 = EDGE_CURVE ( 'NONE', #8320, #22148, #29755, .T. ) ;
#7024 = CARTESIAN_POINT ( 'NONE',  ( -25.26048095167901053, 9.674257073897546633, -92.24941411008894931 ) ) ;
#7025 =( LENGTH_UNIT ( ) NAMED_UNIT ( * ) SI_UNIT ( .MILLI., .METRE. ) );
#7026 = ORIENTED_EDGE ( 'NONE', *, *, #34004, .T. ) ;
#7027 = CARTESIAN_POINT ( 'NONE',  ( 8.000000000000000000, 1.572549600175624063, -0.06894455525513173977 ) ) ;
#7028 = EDGE_LOOP ( 'NONE', ( #6437, #50230, #48154, #1980 ) ) ;
#7029 = ORIENTED_EDGE ( 'NONE', *, *, #45012, .F. ) ;
#7030 = DIRECTION ( 'NONE',  ( 1.000000000000000000, 0.000000000000000000, -0.000000000000000000 ) ) ;
#7031 = LINE ( 'NONE', #30231, #38423 ) ;
#7032 = LINE ( 'NONE', #5629, #47556 ) ;
#7033 = CARTESIAN_POINT ( 'NONE',  ( -127.9466635691204033, 49.07377124385244826, -88.87715223634489803 ) ) ;
#7034 = FACE_OUTER_BOUND ( 'NONE', #25684, .T. ) ;
#7035 = ORIENTED_EDGE ( 'NONE', *, *, #33293, .T. ) ;
#7036 = EDGE_LOOP ( 'NONE', ( #18856, #65533, #68042 ) ) ;
#7037 = DIRECTION ( 'NONE',  ( -0.000000000000000000, 1.000000000000000000, -0.000000000000000000 ) ) ;
#7038 = ORIENTED_EDGE ( 'NONE', *, *, #66322, .T. ) ;
#7039 = DIRECTION ( 'NONE',  ( -0.000000000000000000, -0.000000000000000000, 1.000000000000000000 ) ) ;
#7040 = ORIENTED_EDGE ( 'NONE', *, *, #43748, .F. ) ;
#7041 = CARTESIAN_POINT ( 'NONE',  ( -125.6703656163501677, 47.55170550253211559, 3.775397282693374379 ) ) ;
#7042 = CARTESIAN_POINT ( 'NONE',  ( 91.51282003084288874, 21.14522045960332619, 16.08068469543150059 ) ) ;
#7043 = EDGE_CURVE ( 'NONE', #58885, #58406, #45602, .T. ) ;
#7044 = DIRECTION ( 'NONE',  ( -0.9639628606958513535, -0.2660368455666826670, 0.000000000000000000 ) ) ;
#7045 = ORIENTED_EDGE ( 'NONE', *, *, #49743, .F. ) ;
#7046 = DIRECTION ( 'NONE',  ( 0.000000000000000000, -6.779273404243065824E-32, 1.000000000000000000 ) ) ;
#7047 = EDGE_CURVE ( 'NONE', #45363, #9869, #62339, .T. ) ;
#7048 = EDGE_CURVE ( 'NONE', #60623, #47253, #47609, .T. ) ;
#7049 = VECTOR ( 'NONE', #39546, 1000.000000000000000 ) ;
#7050 = CARTESIAN_POINT ( 'NONE',  ( 70.36689301615740533, 15.53981654908576715, 92.52592592651693337 ) ) ;
#7051 = CARTESIAN_POINT ( 'NONE',  ( 37.45439421541016856, 9.177432671831381228, 44.67329806592552899 ) ) ;
#7052 = LINE ( 'NONE', #7418, #38717 ) ;
#7053 = EDGE_CURVE ( 'NONE', #68618, #30662, #37622, .T. ) ;
#7054 = DIRECTION ( 'NONE',  ( 0.000000000000000000, 1.000000000000000000, 0.000000000000000000 ) ) ;
#7055 = VECTOR ( 'NONE', #11401, 1000.000000000000000 ) ;
#7056 = CARTESIAN_POINT ( 'NONE',  ( -148.7068999155605127, 63.50299517929035176, -88.53389495002838316 ) ) ;
#7057 = CARTESIAN_POINT ( 'NONE',  ( 133.8566784816069628, 41.42467568809806977, -62.86786152285933582 ) ) ;
#7058 = ORIENTED_EDGE ( 'NONE', *, *, #59330, .T. ) ;
#7059 = CARTESIAN_POINT ( 'NONE',  ( 136.9822423813093053, 44.53121110416871886, -77.18959649595817041 ) ) ;
#7060 = LINE ( 'NONE', #59811, #35527 ) ;
#7061 = EDGE_LOOP ( 'NONE', ( #11577, #29186, #63939, #24140 ) ) ;
#7062 = ADVANCED_FACE ( 'NONE', ( #27195 ), #25304, .T. ) ;
#7063 = DIRECTION ( 'NONE',  ( 0.000000000000000000, 0.000000000000000000, 1.000000000000000000 ) ) ;
#7064 = LINE ( 'NONE', #33103, #61226 ) ;
#7065 = CARTESIAN_POINT ( 'NONE',  ( -37.39246151129640339, 11.66872370876246201, 42.30430913977911445 ) ) ;
#7066 = CARTESIAN_POINT ( 'NONE',  ( -146.1140637052938303, 62.65471088530801325, -22.17242859286556822 ) ) ;
#7067 = CARTESIAN_POINT ( 'NONE',  ( 5.000000000000000888, 0.000000000000000000, -25.03750572909317285 ) ) ;
#7068 = CARTESIAN_POINT ( 'NONE',  ( 49.76301652092167416, 41.81676920493115546, 40.00000000000003553 ) ) ;
#7069 = CARTESIAN_POINT ( 'NONE',  ( -9.503708068039186330, 7.005809988361353824, -89.28523705486915674 ) ) ;
#7070 = CARTESIAN_POINT ( 'NONE',  ( -54.56693200831791302, 14.55131601960338728, -62.06087458892353226 ) ) ;
#7071 = CARTESIAN_POINT ( 'NONE',  ( -2.177337698256113896, 7.595833446947585443, -11.11479775384615287 ) ) ;
#7072 = CARTESIAN_POINT ( 'NONE',  ( -12.78319349481551015, 8.274445259016799170, 43.26445497206980662 ) ) ;
#7073 = CARTESIAN_POINT ( 'NONE',  ( 112.7784411285248751, 30.07270878825235272, 3.204304144210361915 ) ) ;
#7074 = CARTESIAN_POINT ( 'NONE',  ( -49.10775795518740949, 14.20291014622890913, -91.82781261574977805 ) ) ;
#7075 = ORIENTED_EDGE ( 'NONE', *, *, #19264, .F. ) ;
#7076 = CARTESIAN_POINT ( 'NONE',  ( -100.4440683050664518, 32.98184228837416043, -35.22808132192965758 ) ) ;
#7077 = ORIENTED_EDGE ( 'NONE', *, *, #12957, .F. ) ;
#7078 = DIRECTION ( 'NONE',  ( 0.2660368455666687892, 0.9639628606958550172, 5.102127870520021999E-18 ) ) ;
#7079 = ADVANCED_FACE ( 'NONE', ( #21573 ), #11361, .F. ) ;
#7080 = CARTESIAN_POINT ( 'NONE',  ( 79.18180043629686793, 18.06526831600452354, -71.18470387585151116 ) ) ;
#7081 = B_SPLINE_CURVE_WITH_KNOTS ( 'NONE', 3,
 ( #52052, #20728, #9491, #67545, #14759, #29907, #63303, #19690, #52397, #40799, #41844, #47110, #57331, #24984, #58348, #46074, #67895, #62253, #68574, #15458, #9837, #51707, #30599, #36910, #51366, #3181, #42524, #38907, #33975, #23432, #55415, #43806, #12515, #11808, #38194, #1609, #65639, #6543, #33286, #28701, #17432, #4890, #27640, #64940, #65280 ),
 .UNSPECIFIED., .F., .F.,
 ( 4, 2, 2, 2, 2, 2, 2, 2, 2, 2, 2, 1, 2, 2, 2, 2, 2, 2, 2, 2, 2, 2, 4 ),
 ( 0.000000000000000000, 0.001510509505235996860, 0.002265764257853974690, 0.003021019010471952086, 0.004531528515707860909, 0.005286783268325837871, 0.006042038020943815702, 0.007552547526179744473, 0.009063057031415674980, 0.01057356653665160462, 0.01132882128926957117, 0.01208407604188753426, 0.01283933079450549734, 0.01359458554712346216, 0.01510509505235941782, 0.01586034980497739652, 0.01661560455759537175, 0.01812611406283131180, 0.01963662356806725184, 0.02039187832068520972, 0.02114713307330316414, 0.02265764257853903826, 0.02416815208377490892 ),
 .UNSPECIFIED. ) ;
#7082 = CARTESIAN_POINT ( 'NONE',  ( 46.84183314611287585, 9.494161546644495075, 65.23765100148109752 ) ) ;
#7083 = DIRECTION ( 'NONE',  ( -1.000000000000000000, 0.000000000000000000, 0.000000000000000000 ) ) ;
#7084 = CARTESIAN_POINT ( 'NONE',  ( 15.55634918610409656, 31.11269837220803325, 2.000000000000001776 ) ) ;
#7085 = DIRECTION ( 'NONE',  ( -1.000000000000000000, 0.000000000000000000, 0.000000000000000000 ) ) ;
#7086 = CARTESIAN_POINT ( 'NONE',  ( -73.27510762699375846, 21.40833250163870360, -91.07236566172743153 ) ) ;
#7087 = CARTESIAN_POINT ( 'NONE',  ( -3.865535754268288660, 58.21137395544315751, 27.58472369367945376 ) ) ;
#7088 = EDGE_LOOP ( 'NONE', ( #22506, #12483, #32040, #52088 ) ) ;
#7089 = VERTEX_POINT ( 'NONE', #32140 ) ;
#7090 = FACE_OUTER_BOUND ( 'NONE', #27961, .T. ) ;
#7091 = DIRECTION ( 'NONE',  ( 1.000000000000000000, 0.000000000000000000, 0.000000000000000000 ) ) ;
#7092 = CARTESIAN_POINT ( 'NONE',  ( -84.49322488516129681, 0.000000000000000000, 43.58025477438756212 ) ) ;
#7093 = CARTESIAN_POINT ( 'NONE',  ( -167.4860113959264822, 82.52233889531186151, 70.12209724409757428 ) ) ;
#7094 = AXIS2_PLACEMENT_3D ( 'NONE', #23196, #17913, #53178 ) ;
#7095 = CARTESIAN_POINT ( 'NONE',  ( -166.9992034932274976, 82.01285191063135471, -11.00469205210656476 ) ) ;
#7096 = AXIS2_PLACEMENT_3D ( 'NONE', #32587, #11821, #54011 ) ;
#7097 = FACE_OUTER_BOUND ( 'NONE', #42212, .T. ) ;
#7098 = ORIENTED_EDGE ( 'NONE', *, *, #44235, .F. ) ;
#7099 = CARTESIAN_POINT ( 'NONE',  ( 94.02499804464930833, 23.15433260743127164, 11.63953833574553798 ) ) ;
#7100 = DIRECTION ( 'NONE',  ( 0.000000000000000000, 0.000000000000000000, 1.000000000000000000 ) ) ;
#7101 = CARTESIAN_POINT ( 'NONE',  ( -85.91089317961403538, 25.21459833389209848, -17.77817569153331334 ) ) ;
#7102 = VECTOR ( 'NONE', #45225, 1000.000000000000000 ) ;
#7103 = CARTESIAN_POINT ( 'NONE',  ( -102.2801239173131052, 32.78103895658057354, 30.51907450641510522 ) ) ;
#7104 = DIRECTION ( 'NONE',  ( 0.000000000000000000, 0.000000000000000000, 1.000000000000000000 ) ) ;
#7105 = FACE_BOUND ( 'NONE', #59118, .T. ) ;
#7106 = AXIS2_PLACEMENT_3D ( 'NONE', #61590, #12706, #13064 ) ;
#7107 = CARTESIAN_POINT ( 'NONE',  ( 157.4703587214989113, 58.92748579479258808, 56.25401806271706562 ) ) ;
#7108 = CIRCLE ( 'NONE', #14983, 5.000000000000018652 ) ;
#7109 = AXIS2_PLACEMENT_3D ( 'NONE', #17385, #52177, #56771 ) ;
#7110 = VERTEX_POINT ( 'NONE', #53228 ) ;
#7111 = DIRECTION ( 'NONE',  ( 0.000000000000000000, 1.000000000000000000, 0.000000000000000000 ) ) ;
#7112 = LINE ( 'NONE', #56337, #35024 ) ;
#7113 = CARTESIAN_POINT ( 'NONE',  ( -52.00092620775819796, 14.92276858858357080, 57.80656622093086128 ) ) ;
#7114 = CARTESIAN_POINT ( 'NONE',  ( 427.4999999999999432, -18.06806526123148160, 0.000000000000000000 ) ) ;
#7115 = CARTESIAN_POINT ( 'NONE',  ( 0.000000000000000000, 0.000000000000000000, 0.000000000000000000 ) ) ;
#7116 = CARTESIAN_POINT ( 'NONE',  ( -7.345652830558763391, 4.996589667937367807, -0.4964154566687925541 ) ) ;
#7117 = EDGE_CURVE ( 'NONE', #62102, #66740, #10329, .T. ) ;
#7118 = ORIENTED_EDGE ( 'NONE', *, *, #12947, .F. ) ;
#7119 = DIRECTION ( 'NONE',  ( -0.000000000000000000, -0.000000000000000000, -1.000000000000000000 ) ) ;
#7120 = LINE ( 'NONE', #38431, #45059 ) ;
#7121 = ORIENTED_EDGE ( 'NONE', *, *, #22252, .F. ) ;
#7122 = CARTESIAN_POINT ( 'NONE',  ( 44.99999999999995737, -25.00000000000000000, 1.999999999999984457 ) ) ;
#7123 = ORIENTED_EDGE ( 'NONE', *, *, #20168, .F. ) ;
#7124 = CARTESIAN_POINT ( 'NONE',  ( 123.4242852856285566, 10.00000000000000000, -20.00000000000000000 ) ) ;
#7125 = CARTESIAN_POINT ( 'NONE',  ( -62.54086041493278714, 17.86944394914986844, -15.38065428761472297 ) ) ;
#7126 = CARTESIAN_POINT ( 'NONE',  ( 88.98820631332496589, 21.30618275724809507, -77.30172795873590985 ) ) ;
#7127 = EDGE_LOOP ( 'NONE', ( #23271, #45642, #57596, #10332 ) ) ;
#7128 = VERTEX_POINT ( 'NONE', #21920 ) ;
#7129 = CARTESIAN_POINT ( 'NONE',  ( 42.03719354205840375, 9.783015072457470040, 71.28445026601322354 ) ) ;
#7130 = CARTESIAN_POINT ( 'NONE',  ( 162.7963212667073378, 63.21900188423068556, 42.19573780102387417 ) ) ;
#7131 = CARTESIAN_POINT ( 'NONE',  ( -156.6862310659955142, 71.88416263379568250, -66.91380956130490176 ) ) ;
#7132 = CARTESIAN_POINT ( 'NONE',  ( 64.93224207568370332, 14.16036304753835751, 17.72345651798445232 ) ) ;
#7133 = CARTESIAN_POINT ( 'NONE',  ( 88.30010642107259855, 19.99780058782973668, 44.52758616833133942 ) ) ;
#7134 = ORIENTED_EDGE ( 'NONE', *, *, #30790, .T. ) ;
#7135 = B_SPLINE_CURVE_WITH_KNOTS ( 'NONE', 3,
 ( #38532, #11792, #2307, #23420, #45901, #45201, #49770, #66683, #18477, #13206, #61385, #1596, #29721, #23060, #39927, #6872, #18822, #35003, #33623, #12863, #34671, #55053, #28684, #56107, #33963, #51185, #7923, #44512, #17416, #39585, #65987, #28324, #61037, #29376, #18132, #50139, #12505, #50828, #34317, #1963, #56447, #2647, #24110, #17787, #67033 ),
 .UNSPECIFIED., .F., .F.,
 ( 4, 2, 2, 2, 2, 2, 2, 2, 2, 2, 2, 1, 2, 2, 2, 2, 2, 2, 2, 2, 2, 2, 4 ),
 ( 0.000000000000000000, 0.001512548138464662540, 0.002268822207696996520, 0.003025096276929330717, 0.004537644415393961815, 0.005293918484626292977, 0.006050192553858625005, 0.007562740692323284726, 0.009075288830787947916, 0.01058783696925261197, 0.01134411103848494314, 0.01210038510771727083, 0.01285665917694960199, 0.01361293324618192968, 0.01512548138464658333, 0.01588175545387890755, 0.01663802952311123351, 0.01815057766157588195, 0.01966312580004053387, 0.02041939986927285983, 0.02117567393850518578, 0.02268822207696979953, 0.02420077021543441328 ),
 .UNSPECIFIED. ) ;
#7136 = ADVANCED_FACE ( 'NONE', ( #37403 ), #15619, .F. ) ;
#7137 = DIRECTION ( 'NONE',  ( 0.8805955318567391110, -0.4738686624729965824, 0.000000000000000000 ) ) ;
#7138 = VECTOR ( 'NONE', #50452, 1000.000000000000000 ) ;
#7139 = CARTESIAN_POINT ( 'NONE',  ( -128.7724923851857284, 49.63576597317771899, -8.639783561551448443 ) ) ;
#7140 = DIRECTION ( 'NONE',  ( -1.000000000000000000, 0.000000000000000000, 0.000000000000000000 ) ) ;
#7141 = CARTESIAN_POINT ( 'NONE',  ( 116.8937673311173029, 32.08228998570054102, -20.05360614510496831 ) ) ;
#7142 = CARTESIAN_POINT ( 'NONE',  ( 79.53586065807786554, 17.12142427614169549, 88.44133967985683853 ) ) ;
#7144 = ORIENTED_EDGE ( 'NONE', *, *, #58200, .F. ) ;
#7143 = CARTESIAN_POINT ( 'NONE',  ( -15.55634918610408945, -26.11269837220804035, 85.00100000000000477 ) ) ;
#7145 = ORIENTED_EDGE ( 'NONE', *, *, #29514, .T. ) ;
#7146 = AXIS2_PLACEMENT_3D ( 'NONE', #23872, #2077, #66801 ) ;
#7147 = EDGE_CURVE ( 'NONE', #60092, #3228, #23810, .T. ) ;
#7148 = ORIENTED_EDGE ( 'NONE', *, *, #62973, .T. ) ;
#7149 = VECTOR ( 'NONE', #29398, 1000.000000000000000 ) ;
#7150 = CARTESIAN_POINT ( 'NONE',  ( -14.19493007850031674, 7.389842975086043708, -20.04074768020527486 ) ) ;
#7151 = CARTESIAN_POINT ( 'NONE',  ( 175.8947993867357411, 74.90689716047910451, 4.528190670890809955 ) ) ;
#7152 = CARTESIAN_POINT ( 'NONE',  ( -54.56693200831794144, 14.55131601960339260, -8.371773407996172978 ) ) ;
#7153 = CARTESIAN_POINT ( 'NONE',  ( 103.1653143050726271, 25.74301230421574971, -14.04530181743896300 ) ) ;
#7154 = VECTOR ( 'NONE', #61070, 1000.000000000000000 ) ;
#7155 = CARTESIAN_POINT ( 'NONE',  ( -56.01329802674222691, 15.98369420723829215, -50.17033095554772615 ) ) ;
#7156 = VECTOR ( 'NONE', #24769, 1000.000000000000000 ) ;
#7157 = DIRECTION ( 'NONE',  ( 0.000000000000000000, 1.000000000000000000, 0.000000000000000000 ) ) ;
#7158 = CYLINDRICAL_SURFACE ( 'NONE', #45507, 25.00000000000000000 ) ;
#7159 = CARTESIAN_POINT ( 'NONE',  ( 417.3372781065083359, 395.0000000000041496, 83.55029585798409641 ) ) ;
#7160 = ORIENTED_EDGE ( 'NONE', *, *, #39490, .F. ) ;
#7161 = VECTOR ( 'NONE', #65081, 999.9999999999998863 ) ;
#7162 = DIRECTION ( 'NONE',  ( -0.000000000000000000, -0.000000000000000000, -1.000000000000000000 ) ) ;
#7163 = ORIENTED_EDGE ( 'NONE', *, *, #8617, .F. ) ;
#7164 = ORIENTED_EDGE ( 'NONE', *, *, #59844, .T. ) ;
#7165 = EDGE_CURVE ( 'NONE', #45847, #62711, #39167, .T. ) ;
#7166 = CARTESIAN_POINT ( 'NONE',  ( -142.0227972901369071, 59.36121938936275910, 10.81978499101997926 ) ) ;
#7167 = B_SPLINE_CURVE_WITH_KNOTS ( 'NONE', 3,
 ( #43265, #11611, #6695, #16891, #59451, #54515 ),
 .UNSPECIFIED., .F., .F.,
 ( 4, 2, 4 ),
 ( 2.380731629547626167E-07, 0.002336973833157547729, 0.004673709593152140102 ),
 .UNSPECIFIED. ) ;
#7168 = LINE ( 'NONE', #1906, #66495 ) ;
#7169 = VECTOR ( 'NONE', #47823, 1000.000000000000114 ) ;
#7170 = CARTESIAN_POINT ( 'NONE',  ( -166.7136514167008841, 81.71618216218793407, 34.41466395245560506 ) ) ;
#7171 = CARTESIAN_POINT ( 'NONE',  ( 113.4418023215250741, 31.50656691678298316, -23.37802265257673184 ) ) ;
#7172 = CARTESIAN_POINT ( 'NONE',  ( -104.5730787903383145, 33.96058035148152499, 18.33112389144127263 ) ) ;
#7173 = CARTESIAN_POINT ( 'NONE',  ( 173.9832054143776077, -170.0000000000000000, -95.00000000000133582 ) ) ;
#7174 = CARTESIAN_POINT ( 'NONE',  ( 134.0849965622594198, 42.73957449886182758, -24.17876034193199786 ) ) ;
#7175 = ORIENTED_EDGE ( 'NONE', *, *, #69066, .F. ) ;
#7176 = EDGE_LOOP ( 'NONE', ( #35574, #21592, #8229, #16800 ) ) ;
#7177 = ORIENTED_EDGE ( 'NONE', *, *, #28666, .T. ) ;
#7178 = CARTESIAN_POINT ( 'NONE',  ( 15.55634918610397399, -31.11269837220809364, 0.000000000000000000 ) ) ;
#7179 = CARTESIAN_POINT ( 'NONE',  ( -11.78792974237933322, 7.181513757308655599, 4.398590650106096511 ) ) ;
#7180 = CYLINDRICAL_SURFACE ( 'NONE', #3091, 5.000000000000004441 ) ;
#7181 = CARTESIAN_POINT ( 'NONE',  ( 93.74127541358416238, 23.04685498098406171, -94.59213288005628328 ) ) ;
#7182 = UNCERTAINTY_MEASURE_WITH_UNIT (LENGTH_MEASURE( 1.000000000000000082E-05 ), #26664, 'distance_accuracy_value', 'NONE');
#7183 = CARTESIAN_POINT ( 'NONE',  ( -447.6627218934913799, 0.000000000000000000, -136.4497041420118251 ) ) ;
#7184 = CARTESIAN_POINT ( 'NONE',  ( 197.6341357773624736, 98.74251867088341328, 66.09103055943789684 ) ) ;
#7185 = ORIENTED_EDGE ( 'NONE', *, *, #60905, .F. ) ;
#7186 = CARTESIAN_POINT ( 'NONE',  ( 65.35403040894466642, 1.250000000000011546, 41.38025477438755928 ) ) ;
#7187 = CARTESIAN_POINT ( 'NONE',  ( 197.8598785550297521, 99.02620879292950917, -73.76648511621989712 ) ) ;
#7188 = CARTESIAN_POINT ( 'NONE',  ( -7.336630171688596214, 7.867399454768214895, -50.41807073194386390 ) ) ;
#7189 = LINE ( 'NONE', #7550, #25133 ) ;
#7190 = CARTESIAN_POINT ( 'NONE',  ( -165.9111709580270428, 79.44576090485632847, 13.56375512218778567 ) ) ;
#7191 = CARTESIAN_POINT ( 'NONE',  ( 79.40386128751609363, 18.13359811229536689, -95.00000000000133582 ) ) ;
#7192 = FACE_BOUND ( 'NONE', #64297, .T. ) ;
#7193 = CARTESIAN_POINT ( 'NONE',  ( 45.80999061969644970, -170.0000000000000000, 94.99999999999866418 ) ) ;
#7194 = VECTOR ( 'NONE', #13454, 1000.000000000000000 ) ;
#7195 = B_SPLINE_CURVE_WITH_KNOTS ( 'NONE', 3,
 ( #35590, #8158, #45441, #24351 ),
 .UNSPECIFIED., .F., .F.,
 ( 4, 4 ),
 ( 9.900409499100981944E-07, 0.05658314289920116785 ),
 .UNSPECIFIED. ) ;
#7196 = ORIENTED_EDGE ( 'NONE', *, *, #3358, .F. ) ;
#7198 = CARTESIAN_POINT ( 'NONE',  ( 198.4999999999999716, 4.499999999999984901, -3.000000000000030198 ) ) ;
#7197 = VECTOR ( 'NONE', #47640, 1000.000000000000114 ) ;
#7199 = CARTESIAN_POINT ( 'NONE',  ( -129.6001310305488801, 48.98284622040322489, -62.73388853355896089 ) ) ;
#7200 = CARTESIAN_POINT ( 'NONE',  ( -105.4487797565984266, 35.55724615608639994, -76.17295365369301408 ) ) ;
#7201 = DIRECTION ( 'NONE',  ( -9.110201094255651812E-19, -5.020134576618378958E-18, -1.000000000000000000 ) ) ;
#7202 = DIRECTION ( 'NONE',  ( 1.000000000000000000, 0.000000000000000000, 0.000000000000000000 ) ) ;
#7203 = VECTOR ( 'NONE', #69, 1000.000000000000000 ) ;
#7204 = ADVANCED_FACE ( 'NONE', ( #29291 ), #18387, .F. ) ;
#7205 = ORIENTED_EDGE ( 'NONE', *, *, #29454, .F. ) ;
#7206 = AXIS2_PLACEMENT_3D ( 'NONE', #32689, #60109, #28101 ) ;
#7207 = CARTESIAN_POINT ( 'NONE',  ( -132.5824930541232902, 51.05842456469446944, -92.67789068422645471 ) ) ;
#7208 = VECTOR ( 'NONE', #61197, 1000.000000000000000 ) ;
#7209 = CARTESIAN_POINT ( 'NONE',  ( 188.3847560247618276, 86.31304713945776541, 88.76876813952972611 ) ) ;
#7210 = ORIENTED_EDGE ( 'NONE', *, *, #63302, .F. ) ;
#7211 = EDGE_CURVE ( 'NONE', #22641, #28657, #50745, .T. ) ;
#7212 = ORIENTED_EDGE ( 'NONE', *, *, #15410, .T. ) ;
#7213 = DIRECTION ( 'NONE',  ( -0.000000000000000000, 1.000000000000000000, -0.000000000000000000 ) ) ;
#7214 = CARTESIAN_POINT ( 'NONE',  ( 152.2924710224605462, 54.98503313872890175, 42.34074644621131966 ) ) ;
#7215 = CARTESIAN_POINT ( 'NONE',  ( 10.55634918610400419, -10.55634918610406281, 0.000000000000000000 ) ) ;
#7216 = ORIENTED_EDGE ( 'NONE', *, *, #52976, .T. ) ;
#7217 = CARTESIAN_POINT ( 'NONE',  ( 63.01563776193091826, -170.0000000000000000, -43.22069083216975116 ) ) ;
#7218 = CARTESIAN_POINT ( 'NONE',  ( -180.6209440844958181, 95.88392769199009535, 11.79712387883822267 ) ) ;
#7219 = CARTESIAN_POINT ( 'NONE',  ( -73.81689110552362365, 20.53332132481501304, -48.34183327519426143 ) ) ;
#7220 = VECTOR ( 'NONE', #55627, 1000.000000000000114 ) ;
#7221 = CARTESIAN_POINT ( 'NONE',  ( 26.11269837220812562, 31.11269837220800483, 0.000000000000000000 ) ) ;
#7222 = CARTESIAN_POINT ( 'NONE',  ( 424.8372781065087906, 400.0000000000044906, 91.05029585798442326 ) ) ;
#7223 = CARTESIAN_POINT ( 'NONE',  ( -190.3074740493607067, 108.5764897054613272, 34.54018387887567343 ) ) ;
#7224 = EDGE_CURVE ( 'NONE', #9825, #52425, #2564, .T. ) ;
#7225 = ORIENTED_EDGE ( 'NONE', *, *, #31683, .T. ) ;
#7226 = ADVANCED_FACE ( 'NONE', ( #44782 ), #6789, .T. ) ;
#7227 = DIRECTION ( 'NONE',  ( 0.000000000000000000, -1.000000000000000000, 0.000000000000000000 ) ) ;
#7228 = CARTESIAN_POINT ( 'NONE',  ( -442.6627218934913799, 0.000000000000000000, -141.4497041420118251 ) ) ;
#7229 =( REPRESENTATION_RELATIONSHIP ('NONE','NONE', #40274, #64096 ) REPRESENTATION_RELATIONSHIP_WITH_TRANSFORMATION ( #65333 )SHAPE_REPRESENTATION_RELATIONSHIP( ) );
#7230 = CARTESIAN_POINT ( 'NONE',  ( -147.1538409485623049, 63.51600817366545471, -49.43746523392897529 ) ) ;
#7231 = CARTESIAN_POINT ( 'NONE',  ( -29.70166638324878150, -57.83280658984300970, 170.0000000000000000 ) ) ;
#7233 = EDGE_LOOP ( 'NONE', ( #68377, #7605 ) ) ;
#7232 = CARTESIAN_POINT ( 'NONE',  ( -133.4012376778782141, 51.64011534538437331, 91.75614716867997345 ) ) ;
#7234 = CARTESIAN_POINT ( 'NONE',  ( 80.30232379693109124, 17.35837133860830761, -47.35644897165359168 ) ) ;
#7235 = EDGE_CURVE ( 'NONE', #28864, #10266, #16985, .T. ) ;
#7236 = EDGE_CURVE ( 'NONE', #21145, #17425, #50034, .T. ) ;
#7237 = ORIENTED_EDGE ( 'NONE', *, *, #40186, .F. ) ;
#7238 = DIRECTION ( 'NONE',  ( -0.000000000000000000, 1.000000000000000000, -0.000000000000000000 ) ) ;
#7239 = CARTESIAN_POINT ( 'NONE',  ( 79.63513233364426469, 18.20496177163924045, 34.49303652560662670 ) ) ;
#7240 = LINE ( 'NONE', #28699, #52325 ) ;
#7241 = DIRECTION ( 'NONE',  ( 1.000000000000000000, 0.000000000000000000, 0.000000000000000000 ) ) ;
#7242 = CARTESIAN_POINT ( 'NONE',  ( 136.9934874058117771, 43.35050367224291534, -9.850568217420210715 ) ) ;
#7243 = CARTESIAN_POINT ( 'NONE',  ( 65.02478361689782105, -37.39438481343979959, 170.0000000000000000 ) ) ;
#7244 = CARTESIAN_POINT ( 'NONE',  ( -176.3763474213711504, 92.36993073950279154, -22.13818532828629770 ) ) ;
#7245 = AXIS2_PLACEMENT_3D ( 'NONE', #45288, #18914, #67453 ) ;
#7246 = CARTESIAN_POINT ( 'NONE',  ( -53.38065169970958124, 15.27943072477081721, 45.13250238169609929 ) ) ;
#7247 = ORIENTED_EDGE ( 'NONE', *, *, #41042, .T. ) ;
#7248 = VERTEX_POINT ( 'NONE', #31031 ) ;
#7249 = EDGE_CURVE ( 'NONE', #9445, #46646, #28705, .T. ) ;
#7250 = CARTESIAN_POINT ( 'NONE',  ( 39.89571693415782505, 8.473773298340390170, 44.91383430596326320 ) ) ;
#7251 = DIRECTION ( 'NONE',  ( -0.000000000000000000, -0.000000000000000000, -1.000000000000000000 ) ) ;
#7252 = CARTESIAN_POINT ( 'NONE',  ( 159.2319614735956463, 59.03334608081209467, 56.45037870953245829 ) ) ;
#7254 = EDGE_CURVE ( 'NONE', #2382, #10473, #24021, .T. ) ;
#7253 = FACE_OUTER_BOUND ( 'NONE', #26699, .T. ) ;
#7255 = EDGE_CURVE ( 'NONE', #30161, #33967, #41236, .T. ) ;
#7256 = EDGE_CURVE ( 'NONE', #55692, #12765, #68319, .T. ) ;
#7257 = VECTOR ( 'NONE', #66815, 1000.000000000000000 ) ;
#7258 = CARTESIAN_POINT ( 'NONE',  ( 205.5130322755755117, 109.1888880665735257, -36.32593103262158252 ) ) ;
#7259 = CARTESIAN_POINT ( 'NONE',  ( -74.18622060908360538, 21.73430079572374041, -75.49420155812906330 ) ) ;
#7260 = LINE ( 'NONE', #23091, #57337 ) ;
#7261 = AXIS2_PLACEMENT_3D ( 'NONE', #41099, #35475, #30205 ) ;
#7262 = CARTESIAN_POINT ( 'NONE',  ( -28.13266652174639049, 9.071935854491421480, -36.08090444528406238 ) ) ;
#7263 = CARTESIAN_POINT ( 'NONE',  ( 164.6406716478538499, 63.44801348349339776, -72.68468498746710793 ) ) ;
#7264 = ORIENTED_EDGE ( 'NONE', *, *, #62105, .F. ) ;
#7265 = VECTOR ( 'NONE', #12636, 1000.000000000000114 ) ;
#7266 = ORIENTED_EDGE ( 'NONE', *, *, #23821, .T. ) ;
#7267 = CARTESIAN_POINT ( 'NONE',  ( -84.49322488516129681, 0.000000000000000000, 43.58025477438756212 ) ) ;
#7268 = VECTOR ( 'NONE', #48702, 1000.000000000000000 ) ;
#7269 = DIRECTION ( 'NONE',  ( -0.000000000000000000, 1.000000000000000000, -0.000000000000000000 ) ) ;
#7270 = DIRECTION ( 'NONE',  ( 0.000000000000000000, 0.000000000000000000, 1.000000000000000000 ) ) ;
#7271 = CARTESIAN_POINT ( 'NONE',  ( 46.66904755831212981, 15.55634918610394379, 0.000000000000000000 ) ) ;
#7272 = CARTESIAN_POINT ( 'NONE',  ( 109.3447482101068289, -21.43190799616912301, -4.967656235065421200 ) ) ;
#7273 = LINE ( 'NONE', #1639, #60353 ) ;
#7274 = CARTESIAN_POINT ( 'NONE',  ( -94.78138776532237841, 30.24234841992713285, -15.13398054818980398 ) ) ;
#7275 = PLANE ( 'NONE',  #36813 ) ;
#7276 = CARTESIAN_POINT ( 'NONE',  ( 36.21730804119342650, 8.016524789962645059, 84.30459139221660791 ) ) ;
#7277 = CARTESIAN_POINT ( 'NONE',  ( 56.42997683260104225, 32.25922681454269991, 40.00000000000003553 ) ) ;
#7278 = ORIENTED_EDGE ( 'NONE', *, *, #15260, .T. ) ;
#7279 = LINE ( 'NONE', #23466, #21652 ) ;
#7280 = CARTESIAN_POINT ( 'NONE',  ( 74.94097818310312675, 1.250000000000011546, 41.38025477438755928 ) ) ;
#7281 = CARTESIAN_POINT ( 'NONE',  ( -13.79190010541703160, 8.363435739308561878, 15.34168723776943821 ) ) ;
#7282 = DIRECTION ( 'NONE',  ( -0.000000000000000000, -0.000000000000000000, -1.000000000000000000 ) ) ;
#7283 = CARTESIAN_POINT ( 'NONE',  ( -53.60725281709914469, 37.40286400928249577, 3.125053320693569132E-16 ) ) ;
#7284 = CARTESIAN_POINT ( 'NONE',  ( 0.000000000000000000, -26.09918303830819397, 0.000000000000000000 ) ) ;
#7285 = ORIENTED_EDGE ( 'NONE', *, *, #58832, .F. ) ;
#7286 = DIRECTION ( 'NONE',  ( 8.714307882523350462E-15, -3.617454073391957233E-15, 1.000000000000000000 ) ) ;
#7287 = DIRECTION ( 'NONE',  ( -0.000000000000000000, -0.000000000000000000, -1.000000000000000000 ) ) ;
#7288 = CARTESIAN_POINT ( 'NONE',  ( -38.93938005333174601, 11.96888249046460651, -42.57750941617720741 ) ) ;
#7289 = CARTESIAN_POINT ( 'NONE',  ( -172.3038663181179686, 87.72015621195183144, -34.71195716474998960 ) ) ;
#7290 = CARTESIAN_POINT ( 'NONE',  ( -28.32746765835430836, -69.45586423092646555, 170.0000000000000000 ) ) ;
#7291 = ORIENTED_EDGE ( 'NONE', *, *, #27232, .F. ) ;
#7292 = CARTESIAN_POINT ( 'NONE',  ( -119.5267374018686581, 42.44190186039714519, -38.41742699949217155 ) ) ;
#7293 = DIRECTION ( 'NONE',  ( 1.000000000000000000, -9.109522253334613014E-16, 0.000000000000000000 ) ) ;
#7294 = CARTESIAN_POINT ( 'NONE',  ( 0.000000000000000000, 0.000000000000000000, 0.000000000000000000 ) ) ;
#7295 = EDGE_CURVE ( 'NONE', #47869, #1332, #15453, .T. ) ;
#7296 = VECTOR ( 'NONE', #42362, 1000.000000000000000 ) ;
#7297 = CARTESIAN_POINT ( 'NONE',  ( -10.96274578891778084, 22.46815979931508167, 0.000000000000000000 ) ) ;
#7298 = ORIENTED_EDGE ( 'NONE', *, *, #52571, .F. ) ;
#7299 = CARTESIAN_POINT ( 'NONE',  ( -173.1211646369891355, 88.63826465341152527, 45.82169460664104577 ) ) ;
#7300 = CARTESIAN_POINT ( 'NONE',  ( 197.1974290009105459, 96.59277840252784131, -44.14995505087879479 ) ) ;
#7301 = CIRCLE ( 'NONE', #6170, 23.97499999999999787 ) ;
#7302 = DIRECTION ( 'NONE',  ( 0.000000000000000000, 1.000000000000000000, -0.000000000000000000 ) ) ;
#7303 = CARTESIAN_POINT ( 'NONE',  ( 21.75684465274326129, 6.764994602232770049, -38.45100986864918013 ) ) ;
#7304 = CONICAL_SURFACE ( 'NONE', #54470, 65.00000000000000000, 0.7853981633974497223 ) ;
#7305 = AXIS2_PLACEMENT_3D ( 'NONE', #42807, #17110, #5867 ) ;
#7307 = VERTEX_POINT ( 'NONE', #14154 ) ;
#7306 = CARTESIAN_POINT ( 'NONE',  ( 112.5537757279407032, 31.07998172410696469, 17.41770588639016282 ) ) ;
#7308 = AXIS2_PLACEMENT_3D ( 'NONE', #55891, #7709, #49903 ) ;
#7309 = EDGE_CURVE ( 'NONE', #16185, #25573, #56561, .T. ) ;
#7310 = CARTESIAN_POINT ( 'NONE',  ( 59.29597493004737885, 11.84030339376941043, 43.84378064322283564 ) ) ;
#7311 = ADVANCED_FACE ( 'NONE', ( #16563 ), #6241, .F. ) ;
#7312 = AXIS2_PLACEMENT_3D ( 'NONE', #27017, #26344, #5225 ) ;
#7313 = ORIENTED_EDGE ( 'NONE', *, *, #28692, .F. ) ;
#7315 = ORIENTED_EDGE ( 'NONE', *, *, #54651, .F. ) ;
#7314 = ADVANCED_FACE ( 'NONE', ( #10934 ), #42153, .T. ) ;
#7316 = CARTESIAN_POINT ( 'NONE',  ( -119.2006376716276037, 42.24203504200470860, -92.71035546800322891 ) ) ;
#7317 = AXIS2_PLACEMENT_3D ( 'NONE', #58860, #10002, #69423 ) ;
#7318 = CARTESIAN_POINT ( 'NONE',  ( 21.98745393275192583, 71.71550996510526943, 133.5802547743875550 ) ) ;
#7319 = EDGE_CURVE ( 'NONE', #52964, #41204, #17945, .T. ) ;
#7321 = VERTEX_POINT ( 'NONE', #49602 ) ;
#7320 = PLANE ( 'NONE',  #25348 ) ;
#7322 = CARTESIAN_POINT ( 'NONE',  ( -96.46475761760915191, 31.03789227780931981, 86.96133435859920269 ) ) ;
#7323 = DIRECTION ( 'NONE',  ( -1.000000000000000000, 0.000000000000000000, 0.000000000000000000 ) ) ;
#7324 = EDGE_CURVE ( 'NONE', #42425, #30796, #49253, .T. ) ;
#7325 = FACE_BOUND ( 'NONE', #65276, .T. ) ;
#7326 = VERTEX_POINT ( 'NONE', #740 ) ;
#7327 = CARTESIAN_POINT ( 'NONE',  ( 207.4610690199662031, 111.9701171077052209, -63.68629331923244052 ) ) ;
#7328 = CARTESIAN_POINT ( 'NONE',  ( -38.89042640463648581, 10.93374343663408865, -14.98468536607676960 ) ) ;
#7329 = CARTESIAN_POINT ( 'NONE',  ( 209.3223706822284100, 0.000000000000000000, 277.8007638641562380 ) ) ;
#7330 = CARTESIAN_POINT ( 'NONE',  ( -126.3453033442920628, 47.99870040347945377, 3.775397282693373047 ) ) ;
#7331 = CARTESIAN_POINT ( 'NONE',  ( 15.78827728214693416, 7.507518794609588042, 56.85925826316891829 ) ) ;
#7332 = EDGE_LOOP ( 'NONE', ( #29634, #1904, #39614, #32845 ) ) ;
#7333 = ORIENTED_EDGE ( 'NONE', *, *, #46538, .F. ) ;
#7334 = ORIENTED_EDGE ( 'NONE', *, *, #7996, .T. ) ;
#7336 = EDGE_CURVE ( 'NONE', #55844, #22362, #1086, .T. ) ;
#7335 = DIRECTION ( 'NONE',  ( -0.000000000000000000, -0.000000000000000000, -1.000000000000000000 ) ) ;
#7337 = EDGE_CURVE ( 'NONE', #4215, #59386, #23596, .T. ) ;
#7338 = SURFACE_STYLE_USAGE ( .BOTH. , #29476 ) ;
#7339 = CARTESIAN_POINT ( 'NONE',  ( -34.74740905761646559, 10.15745573515589228, -36.06853344480607149 ) ) ;
#7340 = CARTESIAN_POINT ( 'NONE',  ( -96.46749073287921306, 29.92475971289336556, 86.95816172513350750 ) ) ;
#7341 = ADVANCED_FACE ( 'NONE', ( #39766 ), #66178, .F. ) ;
#7342 = CARTESIAN_POINT ( 'NONE',  ( -142.0902782307735208, 58.13494170555998863, 37.07437729448285779 ) ) ;
#7343 = CARTESIAN_POINT ( 'NONE',  ( -132.6161619568759988, 51.08240647571220450, 61.62853753731319983 ) ) ;
#7344 = CARTESIAN_POINT ( 'NONE',  ( -71.97658551692140350, 20.95070248419150261, -19.17076785925019777 ) ) ;
#7345 = VERTEX_POINT ( 'NONE', #65106 ) ;
#7346 = CARTESIAN_POINT ( 'NONE',  ( 80.16939877002756987, 17.31693935407226448, 67.89906232374367789 ) ) ;
#7347 = EDGE_LOOP ( 'NONE', ( #15337, #14138, #8915, #52146 ) ) ;
#7348 = VECTOR ( 'NONE', #12333, 999.9999999999998863 ) ;
#7349 = CARTESIAN_POINT ( 'NONE',  ( 31.90217595456441302, 7.552213897210509508, 37.90790274029890128 ) ) ;
#7350 = FACE_OUTER_BOUND ( 'NONE', #64510, .T. ) ;
#7351 = VERTEX_POINT ( 'NONE', #61223 ) ;
#7352 = CARTESIAN_POINT ( 'NONE',  ( 181.0840389613909736, 78.60582251573003987, 44.30859410551141764 ) ) ;
#7353 = LINE ( 'NONE', #62192, #7457 ) ;
#7355 = DIRECTION ( 'NONE',  ( -1.387778780781445922E-16, 1.000000000000000000, 1.232595164407830946E-32 ) ) ;
#7354 = VECTOR ( 'NONE', #23359, 1000.000000000000000 ) ;
#7356 = CARTESIAN_POINT ( 'NONE',  ( -122.8011284400168250, 45.68452922414294193, 58.11634083775930293 ) ) ;
#7357 = CARTESIAN_POINT ( 'NONE',  ( -53.13004807512037786, 14.17398740785108480, 18.23844739916169289 ) ) ;
#7358 = CARTESIAN_POINT ( 'NONE',  ( 155.2910738464913152, 55.97560547655806573, -50.81481607110237775 ) ) ;
#7360 = CARTESIAN_POINT ( 'NONE',  ( 160.5018603162735076, 61.33906090758085838, -77.34339245626459558 ) ) ;
#7359 = VECTOR ( 'NONE', #17917, 1000.000000000000000 ) ;
#7361 = AXIS2_PLACEMENT_3D ( 'NONE', #30135, #58233, #63515 ) ;
#7362 = VERTEX_POINT ( 'NONE', #48899 ) ;
#7363 = FACE_BOUND ( 'NONE', #15953, .T. ) ;
#7364 = CARTESIAN_POINT ( 'NONE',  ( -155.7433525314458791, 69.65452735858369238, -11.29319091142111375 ) ) ;
#7365 = EDGE_LOOP ( 'NONE', ( #54260, #47878 ) ) ;
#7366 = CARTESIAN_POINT ( 'NONE',  ( -7.825402957745087207, -170.0000000000000000, 37.61558103944720699 ) ) ;
#7367 = CARTESIAN_POINT ( 'NONE',  ( -29.47687737404459085, 68.96458294135867106, 43.58025477438756212 ) ) ;
#7368 = DIRECTION ( 'NONE',  ( -0.000000000000000000, -0.000000000000000000, 1.000000000000000000 ) ) ;
#7369 = ORIENTED_EDGE ( 'NONE', *, *, #50014, .F. ) ;
#7370 = B_SPLINE_CURVE_WITH_KNOTS ( 'NONE', 3,
 ( #25011, #52423, #64010, #4245, #52749, #41871 ),
 .UNSPECIFIED., .F., .F.,
 ( 4, 2, 4 ),
 ( 0.03218935267740795358, 0.06469833035354465023, 0.09720730802968134687 ),
 .UNSPECIFIED. ) ;
#7371 = CARTESIAN_POINT ( 'NONE',  ( -85.09761763353360209, 24.87634954265997678, 41.78514032919718346 ) ) ;
#7372 = CARTESIAN_POINT ( 'NONE',  ( 151.3136733342016669, 54.26417151662143112, -66.17808903341922644 ) ) ;
#7373 = CARTESIAN_POINT ( 'NONE',  ( 45.89232972084001005, 10.36128169546909916, 33.64739044171249560 ) ) ;
#7374 = CARTESIAN_POINT ( 'NONE',  ( 141.3403471770512851, 46.13063628128488602, -44.08590368907992030 ) ) ;
#7375 = AXIS2_PLACEMENT_3D ( 'NONE', #31806, #5064, #26872 ) ;
#7376 = EDGE_LOOP ( 'NONE', ( #17858, #25912, #30020, #37099 ) ) ;
#7377 = DIRECTION ( 'NONE',  ( 1.000000000000000000, 0.000000000000000000, 0.000000000000000000 ) ) ;
#7378 = EDGE_LOOP ( 'NONE', ( #21724, #53130, #68863, #58672, #15806, #61886, #10687, #5005, #35671, #19994 ) ) ;
#7379 = CARTESIAN_POINT ( 'NONE',  ( 0.7145311798163228589, 4.618802153517005848, 8.000000000000000000 ) ) ;
#7380 = DIRECTION ( 'NONE',  ( -1.000000000000000000, 0.000000000000000000, 0.000000000000000000 ) ) ;
#7381 = CARTESIAN_POINT ( 'NONE',  ( -0.8863173716723049544, 7.545240407187534970, 13.64818108344007719 ) ) ;
#7382 = CARTESIAN_POINT ( 'NONE',  ( -0.3740447803642787949, 7.527031846085009192, 63.47620538581821847 ) ) ;
#7383 = LINE ( 'NONE', #44998, #11093 ) ;
#7384 = FILL_AREA_STYLE ('',( #43944 ) ) ;
#7385 = ADVANCED_FACE ( 'NONE', ( #13051, #33099 ), #22539, .T. ) ;
#7386 = CARTESIAN_POINT ( 'NONE',  ( -125.8938041572051105, 46.49392987655492959, -76.75825448869764500 ) ) ;
#7387 = VERTEX_POINT ( 'NONE', #60169 ) ;
#7388 = CARTESIAN_POINT ( 'NONE',  ( 164.6499013411309420, 63.45576988183554334, -14.59376700924564219 ) ) ;
#7389 = LINE ( 'NONE', #67188, #45152 ) ;
#7390 = CARTESIAN_POINT ( 'NONE',  ( 63.49940197359693883, 12.78497925206076324, 56.65751152968497451 ) ) ;
#7391 = PLANE ( 'NONE',  #13086 ) ;
#7392 = LINE ( 'NONE', #60144, #13886 ) ;
#7393 = ORIENTED_EDGE ( 'NONE', *, *, #11513, .F. ) ;
#7394 = EDGE_CURVE ( 'NONE', #51881, #42885, #28154, .T. ) ;
#7395 = ORIENTED_EDGE ( 'NONE', *, *, #7023, .F. ) ;
#7396 = CYLINDRICAL_SURFACE ( 'NONE', #22759, 21.00000000000000355 ) ;
#7397 = ORIENTED_EDGE ( 'NONE', *, *, #58407, .T. ) ;
#7398 = VECTOR ( 'NONE', #8286, 1000.000000000000000 ) ;
#7399 = CARTESIAN_POINT ( 'NONE',  ( 64.93224207568368911, 14.16036304753835218, 71.41255769891185423 ) ) ;
#7400 = LINE ( 'NONE', #17950, #12898 ) ;
#7401 = ADVANCED_FACE ( 'NONE', ( #39082 ), #33796, .F. ) ;
#7402 = EDGE_CURVE ( 'NONE', #11928, #12092, #39946, .T. ) ;
#7403 = AXIS2_PLACEMENT_3D ( 'NONE', #41940, #22560, #12359 ) ;
#7404 = VERTEX_POINT ( 'NONE', #35877 ) ;
#7405 = CARTESIAN_POINT ( 'NONE',  ( 15.55634918610411610, 51.66904755831205875, 85.00100000000000477 ) ) ;
#7406 = CARTESIAN_POINT ( 'NONE',  ( 88.99522780200240391, 20.24180937454203999, 17.48863613379957371 ) ) ;
#7407 = EDGE_CURVE ( 'NONE', #8775, #26863, #45567, .T. ) ;
#7408 = CARTESIAN_POINT ( 'NONE',  ( 164.6499013411307999, 63.45576988183551492, -41.43831759970928630 ) ) ;
#7409 = VECTOR ( 'NONE', #10719, 1000.000000000000000 ) ;
#7410 = ORIENTED_EDGE ( 'NONE', *, *, #12813, .T. ) ;
#7411 = B_SPLINE_CURVE_WITH_KNOTS ( 'NONE', 3,
 ( #22498, #33760, #44992, #55195 ),
 .UNSPECIFIED., .F., .F.,
 ( 4, 4 ),
 ( 0.1259919275528359750, 0.1829744153748750768 ),
 .UNSPECIFIED. ) ;
#7412 = AXIS2_PLACEMENT_3D ( 'NONE', #56590, #30216, #8412 ) ;
#7413 = CARTESIAN_POINT ( 'NONE',  ( -447.6627218934918915, 390.0000000000064801, -141.4497041420121377 ) ) ;
#7415 = CARTESIAN_POINT ( 'NONE',  ( 57.92895196976683536, 12.57818278445338755, 85.48064400023716303 ) ) ;
#7414 = SHAPE_REPRESENTATION ( 'pulley', ( #66832 ), #23071 ) ;
#7416 = CARTESIAN_POINT ( 'NONE',  ( 36.99999522780156980, 9.122638774496635961, 30.30464867167598797 ) ) ;
#7417 = VECTOR ( 'NONE', #60964, 1000.000000000000000 ) ;
#7418 = CARTESIAN_POINT ( 'NONE',  ( 30.12852347772543027, 58.62603998952764783, 73.58025477438759765 ) ) ;
#7419 = CARTESIAN_POINT ( 'NONE',  ( -179.6145635655384183, 96.24253679848490606, -92.13970873418386986 ) ) ;
#7420 = LINE ( 'NONE', #8453, #39043 ) ;
#7421 = CARTESIAN_POINT ( 'NONE',  ( 132.0582325211145189, 40.34869848118184166, -63.07262740430937242 ) ) ;
#7422 = VERTEX_POINT ( 'NONE', #34849 ) ;
#7423 = CARTESIAN_POINT ( 'NONE',  ( 141.3586046882815594, 47.34625111366353423, -70.87675768225021500 ) ) ;
#7424 = CARTESIAN_POINT ( 'NONE',  ( 0.000000000000000000, 0.000000000000000000, 40.00000000000003553 ) ) ;
#7425 = EDGE_LOOP ( 'NONE', ( #6600, #59641, #25600, #28610 ) ) ;
#7426 = CARTESIAN_POINT ( 'NONE',  ( -156.4966862384868307, 71.70877417666511633, -39.54005476914262829 ) ) ;
#7427 = CARTESIAN_POINT ( 'NONE',  ( 8.904582680624310242, -23.36040254969760355, 0.000000000000000000 ) ) ;
#7428 = CARTESIAN_POINT ( 'NONE',  ( -32.40928421737412179, 10.77259363352673383, 30.26336764027513482 ) ) ;
#7429 = CARTESIAN_POINT ( 'NONE',  ( -168.7187482717113483, 82.35796501763486788, -48.30229039519385736 ) ) ;
#7430 = CARTESIAN_POINT ( 'NONE',  ( -5.417282889646088506, 7.753782747238991746, 44.72272311776506371 ) ) ;
#7431 = DIRECTION ( 'NONE',  ( 0.000000000000000000, 0.000000000000000000, -1.000000000000000000 ) ) ;
#7432 = EDGE_CURVE ( 'NONE', #19424, #25857, #61573, .T. ) ;
#7433 = CARTESIAN_POINT ( 'NONE',  ( -52.45215874217874585, 13.99961488531758391, -76.59970130483547734 ) ) ;
#7434 = CARTESIAN_POINT ( 'NONE',  ( -3.253130881186329759, 7.643323950922367160, -22.03867337319629627 ) ) ;
#7435 = CARTESIAN_POINT ( 'NONE',  ( -14.56631729561072142, 8.434645566888205437, 40.94015154958498215 ) ) ;
#7436 = CARTESIAN_POINT ( 'NONE',  ( 113.8748103246145433, 30.59837980920002209, 16.84643264326143708 ) ) ;
#7437 = DIRECTION ( 'NONE',  ( 0.000000000000000000, -1.000000000000000000, 0.000000000000000000 ) ) ;
#7438 = ORIENTED_EDGE ( 'NONE', *, *, #22139, .T. ) ;
#7439 = CARTESIAN_POINT ( 'NONE',  ( -95.86163447241557378, 30.75089131639703410, -46.42652761453075527 ) ) ;
#7440 = ORIENTED_EDGE ( 'NONE', *, *, #69569, .F. ) ;
#7441 = CARTESIAN_POINT ( 'NONE',  ( 109.7724924842965777, 28.66436020578542099, -62.76698815611733551 ) ) ;
#7442 = CARTESIAN_POINT ( 'NONE',  ( 45.89232972084000295, 10.36128169546909383, -20.04171073921484947 ) ) ;
#7443 = CARTESIAN_POINT ( 'NONE',  ( 45.90693067088657386, 9.344800815249321602, 68.02348139506582925 ) ) ;
#7444 = CARTESIAN_POINT ( 'NONE',  ( 6.933333333333335347, 8.000000000000000000, 43.13333333333333286 ) ) ;
#7445 = FACE_OUTER_BOUND ( 'NONE', #49043, .T. ) ;
#7446 = LINE ( 'NONE', #55976, #54640 ) ;
#7447 = CARTESIAN_POINT ( 'NONE',  ( 266.9165763529819628, 242.0000000000000000, 108.9999999999999858 ) ) ;
#7448 = CARTESIAN_POINT ( 'NONE',  ( -118.3918229753714968, 42.92682904595257298, -16.07878825854773552 ) ) ;
#7449 = ORIENTED_EDGE ( 'NONE', *, *, #35496, .T. ) ;
#7450 = ORIENTED_EDGE ( 'NONE', *, *, #20809, .T. ) ;
#7451 = CARTESIAN_POINT ( 'NONE',  ( 290.0000000000000568, -5.000000000000000888, 18.50000000000000000 ) ) ;
#7452 = CARTESIAN_POINT ( 'NONE',  ( 181.0840389613909736, 78.60582251573006829, 71.15314469597512925 ) ) ;
#7453 = DIRECTION ( 'NONE',  ( 1.000000000000000000, 0.000000000000000000, 0.000000000000000000 ) ) ;
#7454 = AXIS2_PLACEMENT_3D ( 'NONE', #27203, #32837, #54268 ) ;
#7455 = CARTESIAN_POINT ( 'NONE',  ( 107.2614272668148914, 28.62909081796205868, 70.84170775330584036 ) ) ;
#7456 = DIRECTION ( 'NONE',  ( -1.000000000000000000, 0.000000000000000000, 0.000000000000000000 ) ) ;
#7457 = VECTOR ( 'NONE', #29149, 1000.000000000000227 ) ;
#7458 = DIRECTION ( 'NONE',  ( 1.000000000000000000, -0.000000000000000000, -0.000000000000000000 ) ) ;
#7459 = ORIENTED_EDGE ( 'NONE', *, *, #5767, .T. ) ;
#7460 = CARTESIAN_POINT ( 'NONE',  ( 91.50468583833760761, 22.21368636549395958, 4.646999254352490283 ) ) ;
#7461 = VECTOR ( 'NONE', #32886, 1000.000000000000114 ) ;
#7462 = VECTOR ( 'NONE', #26412, 1000.000000000000000 ) ;
#7463 = EDGE_CURVE ( 'NONE', #12451, #43150, #55952, .T. ) ;
#7464 = CARTESIAN_POINT ( 'NONE',  ( -14.32120159453989672, 7.401444311907543927, 60.70308768940526534 ) ) ;
#7465 = CARTESIAN_POINT ( 'NONE',  ( -81.90020664963800812, 23.57971581008655804, -22.54224771583843534 ) ) ;
#7466 = CARTESIAN_POINT ( 'NONE',  ( 149.0250918491436494, 6.000000000000000000, -36.68900338898720292 ) ) ;
#7467 = CARTESIAN_POINT ( 'NONE',  ( 18.62350602913453201, 0.000000000000000000, 23.51946052065798298 ) ) ;
#7468 = FACE_BOUND ( 'NONE', #43662, .T. ) ;
#7469 = AXIS2_PLACEMENT_3D ( 'NONE', #26990, #59680, #43159 ) ;
#7470 = EDGE_CURVE ( 'NONE', #64129, #56353, #61901, .T. ) ;
#7471 = CIRCLE ( 'NONE', #49967, 2.999999999999999112 ) ;
#7472 = EDGE_CURVE ( 'NONE', #28358, #37085, #8102, .T. ) ;
#7473 = CIRCLE ( 'NONE', #20911, 4.999999999999990230 ) ;
#7474 = EDGE_CURVE ( 'NONE', #6290, #68152, #37550, .T. ) ;
#7475 = VERTEX_POINT ( 'NONE', #46418 ) ;
#7476 = CARTESIAN_POINT ( 'NONE',  ( 86.62931800182292363, 19.42108912189599224, -89.51066537983906812 ) ) ;
#7477 = PLANE ( 'NONE',  #30552 ) ;
#7478 = CARTESIAN_POINT ( 'NONE',  ( 32.90051628396145134, 8.664124555952431805, -73.73572960565718404 ) ) ;
#7479 = FACE_OUTER_BOUND ( 'NONE', #46124, .T. ) ;
#7480 = CARTESIAN_POINT ( 'NONE',  ( 156.5977259323289275, 56.97512126940429766, 2.602768280174560633 ) ) ;
#7481 = CARTESIAN_POINT ( 'NONE',  ( -6.686525924292793022, 5.377136764700151339, -0.3167204509598375850 ) ) ;
#7482 = VERTEX_POINT ( 'NONE', #2483 ) ;
#7483 = CARTESIAN_POINT ( 'NONE',  ( 58.47673920847984164, 11.66523265296355483, 4.477951416689838204 ) ) ;
#7484 = CARTESIAN_POINT ( 'NONE',  ( 198.7129816317745679, 100.1061386900355785, -39.29776229674419596 ) ) ;
#7485 = VERTEX_POINT ( 'NONE', #7766 ) ;
#7486 = CARTESIAN_POINT ( 'NONE',  ( -56.55682276332724712, 14.31196085009922569, 27.58472369374502264 ) ) ;
#7487 = ORIENTED_EDGE ( 'NONE', *, *, #33804, .T. ) ;
#7488 = DIRECTION ( 'NONE',  ( -0.000000000000000000, -0.000000000000000000, -1.000000000000000000 ) ) ;
#7489 = CARTESIAN_POINT ( 'NONE',  ( -20.55634918610396866, 36.11269837220808654, 85.00100000000000477 ) ) ;
#7490 = CARTESIAN_POINT ( 'NONE',  ( 94.11733320392092139, 23.18939451097131155, -70.65979286123472036 ) ) ;
#7491 = ADVANCED_FACE ( 'NONE', ( #14425 ), #9146, .T. ) ;
#7492 = ORIENTED_EDGE ( 'NONE', *, *, #1164, .F. ) ;
#7493 = EDGE_CURVE ( 'NONE', #40620, #6748, #58952, .T. ) ;
#7494 = EDGE_LOOP ( 'NONE', ( #35220, #61141, #17764, #20602 ) ) ;
#7495 = DIRECTION ( 'NONE',  ( 0.6234898018587318180, 0.7818314824680311359, 0.000000000000000000 ) ) ;
#7496 = CARTESIAN_POINT ( 'NONE',  ( 161.7031777507227162, 62.31724004902782355, 43.11786657228953601 ) ) ;
#7497 = DIRECTION ( 'NONE',  ( 1.000000000000000000, -0.000000000000000000, 0.000000000000000000 ) ) ;
#7498 = PLANE ( 'NONE',  #46322 ) ;
#7499 = CARTESIAN_POINT ( 'NONE',  ( -41.31727360890798906, 62.59299402909750398, 43.58025477438756212 ) ) ;
#7500 = EDGE_LOOP ( 'NONE', ( #22265, #17521, #54700, #58872 ) ) ;
#7501 = PRODUCT_DEFINITION_SHAPE ( 'NONE', 'NONE',  #58101 ) ;
#7502 = CARTESIAN_POINT ( 'NONE',  ( -52.00092620775819796, 14.92276858858357258, -49.57163614092388570 ) ) ;
#7503 = VECTOR ( 'NONE', #581, 1000.000000000000000 ) ;
#7504 = CARTESIAN_POINT ( 'NONE',  ( -54.56685407443680447, 15.59259313022788440, 18.47277718246750311 ) ) ;
#7505 = CARTESIAN_POINT ( 'NONE',  ( -15.15117926080556465, 8.490099586177995761, -95.00000000000133582 ) ) ;
#7506 = CARTESIAN_POINT ( 'NONE',  ( -155.6741333259783460, 70.95299863499437265, -91.72665331470490457 ) ) ;
#7507 = CARTESIAN_POINT ( 'NONE',  ( -5.066666666666664653, 8.000000000000000000, 43.13333333333333286 ) ) ;
#7508 = CARTESIAN_POINT ( 'NONE',  ( 84.09769155791593676, 18.57180883336368638, 83.81111254107904074 ) ) ;
#7510 = ORIENTED_EDGE ( 'NONE', *, *, #52002, .F. ) ;
#7509 = DIRECTION ( 'NONE',  ( 1.000000000000000000, 0.000000000000000000, 0.000000000000000000 ) ) ;
#7511 = VERTEX_POINT ( 'NONE', #11113 ) ;
#7512 = VECTOR ( 'NONE', #9429, 1000.000000000000000 ) ;
#7513 = ORIENTED_EDGE ( 'NONE', *, *, #35651, .T. ) ;
#7514 = CARTESIAN_POINT ( 'NONE',  ( 46.41758729921141935, 9.425975226414244901, 7.906304787334934581 ) ) ;
#7515 = CARTESIAN_POINT ( 'NONE',  ( -177.7741424253921707, 94.02182498476740591, 86.12237327923784846 ) ) ;
#7516 = CARTESIAN_POINT ( 'NONE',  ( -47.95193882091085413, 12.89180642785319542, -18.33614611382470017 ) ) ;
#7517 = CARTESIAN_POINT ( 'NONE',  ( 106.0171289417044136, 26.97542621030655852, -10.37713856442654503 ) ) ;
#7518 = CARTESIAN_POINT ( 'NONE',  ( -130.2071229607963119, 50.62285182196875866, 44.27336784337931164 ) ) ;
#7519 = CARTESIAN_POINT ( 'NONE',  ( 200.4600337307565496, 100.7087439352121123, 16.06857715856459734 ) ) ;
#7520 = CARTESIAN_POINT ( 'NONE',  ( 209.7104118037933347, 115.2827355935552873, 84.81015762066461150 ) ) ;
#7521 = DIRECTION ( 'NONE',  ( 1.000000000000000000, 0.000000000000000000, 0.000000000000000000 ) ) ;
#7522 = CARTESIAN_POINT ( 'NONE',  ( -73.63346300764936814, 20.46798018699518806, -75.02584359677265979 ) ) ;
#7523 = DIRECTION ( 'NONE',  ( 0.000000000000000000, 0.000000000000000000, 1.000000000000000000 ) ) ;
#7524 = EDGE_LOOP ( 'NONE', ( #62360, #26646, #4807, #34209 ) ) ;
#7525 = VECTOR ( 'NONE', #52717, 1000.000000000000000 ) ;
#7526 = CARTESIAN_POINT ( 'NONE',  ( 12.03162622199373288, 7.415834979634795765, -9.678397900994031744 ) ) ;
#7527 = VERTEX_POINT ( 'NONE', #33287 ) ;
#7528 = ORIENTED_EDGE ( 'NONE', *, *, #64229, .F. ) ;
#7529 = CARTESIAN_POINT ( 'NONE',  ( -146.7404675333697810, 63.17262273741977907, 18.35075481789837681 ) ) ;
#7530 = CARTESIAN_POINT ( 'NONE',  ( -452.6627218934913230, 217.8591479523843475, 78.55029585798814651 ) ) ;
#7531 = CARTESIAN_POINT ( 'NONE',  ( 0.000000000000000000, 0.000000000000000000, -60.00000000000000000 ) ) ;
#7532 = CARTESIAN_POINT ( 'NONE',  ( 3.318518101603014525, 7.321656987762867885, -9.500000000000005329 ) ) ;
#7533 = DIRECTION ( 'NONE',  ( -0.000000000000000000, 0.7071067811865475727, 0.7071067811865475727 ) ) ;
#7534 = DIRECTION ( 'NONE',  ( -0.000000000000000000, 1.000000000000000000, -0.000000000000000000 ) ) ;
#7535 = CARTESIAN_POINT ( 'NONE',  ( 140.0820590176526252, 46.51134312115245706, -20.86892350826419573 ) ) ;
#7536 = ORIENTED_EDGE ( 'NONE', *, *, #62668, .T. ) ;
#7537 = VERTEX_POINT ( 'NONE', #53319 ) ;
#7538 = LINE ( 'NONE', #25100, #28234 ) ;
#7539 = CARTESIAN_POINT ( 'NONE',  ( -9.771516655894551207, 7.025139475821123192, 3.511394494525364784 ) ) ;
#7540 = CARTESIAN_POINT ( 'NONE',  ( -17.54261641588776754, 37.86253240666081865, 13.79046412320003689 ) ) ;
#7541 = CARTESIAN_POINT ( 'NONE',  ( 58.47673920847984874, 11.66523265296357614, -22.36659917377383522 ) ) ;
#7542 = CARTESIAN_POINT ( 'NONE',  ( -47.95193882091083992, 12.89180642785318653, 35.35295506710262714 ) ) ;
#7543 = CARTESIAN_POINT ( 'NONE',  ( 203.9203998321607685, 106.9845510704142271, 71.02229316225890443 ) ) ;
#7544 = VERTEX_POINT ( 'NONE', #32920 ) ;
#7545 = DIRECTION ( 'NONE',  ( -1.000000000000000000, 0.000000000000000000, -0.000000000000000000 ) ) ;
#7546 = LINE ( 'NONE', #39204, #27864 ) ;
#7547 = CARTESIAN_POINT ( 'NONE',  ( 179.4207200232661137, 76.93724985992176357, -63.20564937983176890 ) ) ;
#7548 = CARTESIAN_POINT ( 'NONE',  ( -164.2385321673937142, -16.13521868445280560, 306.6706262528896332 ) ) ;
#7549 = CARTESIAN_POINT ( 'NONE',  ( 276.2352375355092704, -21.75137027410912438, -3.306356075928093219 ) ) ;
#7550 = CARTESIAN_POINT ( 'NONE',  ( 100.0000000000000284, 5.000000000000000000, 18.50000000000000000 ) ) ;
#7551 = CARTESIAN_POINT ( 'NONE',  ( -167.0043730366751902, 80.56812533391482134, -91.53196777109012316 ) ) ;
#7552 = DIRECTION ( 'NONE',  ( 0.000000000000000000, 0.000000000000000000, -1.000000000000000000 ) ) ;
#7553 = LINE ( 'NONE', #44477, #68985 ) ;
#7554 = CARTESIAN_POINT ( 'NONE',  ( -189.5883860598227670, 107.5728846252917066, 94.41119403186252157 ) ) ;
#7555 = EDGE_CURVE ( 'NONE', #50199, #22455, #66118, .T. ) ;
#7556 = CIRCLE ( 'NONE', #14274, 243.4957430088094839 ) ;
#7557 = EDGE_CURVE ( 'NONE', #37405, #15400, #40924, .T. ) ;
#7558 = DIRECTION ( 'NONE',  ( 0.000000000000000000, 0.000000000000000000, 1.000000000000000000 ) ) ;
#7559 = VERTEX_POINT ( 'NONE', #34335 ) ;
#7560 = CIRCLE ( 'NONE', #60310, 65.00000000000000000 ) ;
#7561 = CARTESIAN_POINT ( 'NONE',  ( 276.0273295991593727, 21.78875652052167311, 3.053836096979974268 ) ) ;
#7562 = ADVANCED_FACE ( 'NONE', ( #29056 ), #56119, .T. ) ;
#7563 = CARTESIAN_POINT ( 'NONE',  ( -128.9786047358386440, 48.55852351614670681, -62.41807552428025474 ) ) ;
#7564 = DIRECTION ( 'NONE',  ( 0.000000000000000000, 0.000000000000000000, 1.000000000000000000 ) ) ;
#7565 = DIRECTION ( 'NONE',  ( -0.3930250316539278255, 0.9195277725514487965, 0.000000000000000000 ) ) ;
#7566 = CARTESIAN_POINT ( 'NONE',  ( -17.50000000000000000, -17.50000000000000000, 0.000000000000000000 ) ) ;
#7567 = AXIS2_PLACEMENT_3D ( 'NONE', #3164, #56974, #8791 ) ;
#7568 = AXIS2_PLACEMENT_3D ( 'NONE', #42209, #4570, #4237 ) ;
#7569 = VERTEX_POINT ( 'NONE', #65640 ) ;
#7570 = CARTESIAN_POINT ( 'NONE',  ( -188.6739852773920347, 108.2139733222100517, 13.28364116741142809 ) ) ;
#7571 = CARTESIAN_POINT ( 'NONE',  ( 175.7669052691647664, 73.39379665792895935, 85.19702012587089257 ) ) ;
#7572 = VERTEX_POINT ( 'NONE', #17800 ) ;
#7573 = AXIS2_PLACEMENT_3D ( 'NONE', #64586, #28334, #69502 ) ;
#7574 = ORIENTED_EDGE ( 'NONE', *, *, #3834, .F. ) ;
#7575 = CYLINDRICAL_SURFACE ( 'NONE', #3848, 7.500000000000013323 ) ;
#7576 = CARTESIAN_POINT ( 'NONE',  ( 150.2805372522807090, 53.51147386362156055, 39.06112697484593355 ) ) ;
#7577 = CARTESIAN_POINT ( 'NONE',  ( 0.000000000000000000, 0.000000000000000000, 0.000000000000000000 ) ) ;
#7578 = EDGE_CURVE ( 'NONE', #28503, #49819, #29809, .T. ) ;
#7579 = ORIENTED_EDGE ( 'NONE', *, *, #40483, .F. ) ;
#7580 = DIRECTION ( 'NONE',  ( 0.000000000000000000, -0.000000000000000000, -1.000000000000000000 ) ) ;
#7581 = CARTESIAN_POINT ( 'NONE',  ( -177.1540936177023298, 91.73126115633627364, 5.138615071113800781 ) ) ;
#7582 = CARTESIAN_POINT ( 'NONE',  ( -55.05276343752910151, -170.0000000000000000, 10.97277718246748890 ) ) ;
#7583 = CARTESIAN_POINT ( 'NONE',  ( -78.66644367742111399, 23.39876645725287219, 30.41820113967310490 ) ) ;
#7584 = CARTESIAN_POINT ( 'NONE',  ( -26.88635117726413526, 9.904687797303056485, -9.992545258014629894 ) ) ;
#7585 = CARTESIAN_POINT ( 'NONE',  ( -54.08488990389050599, 15.46443908526321565, -23.32469389829597617 ) ) ;
#7586 = ORIENTED_EDGE ( 'NONE', *, *, #16733, .T. ) ;
#7587 = CARTESIAN_POINT ( 'NONE',  ( 196.9999999999999716, 4.499999999999984901, -48.49999999999998579 ) ) ;
#7588 = DIRECTION ( 'NONE',  ( -0.000000000000000000, 1.000000000000000000, -0.000000000000000000 ) ) ;
#7589 = CYLINDRICAL_SURFACE ( 'NONE', #29305, 21.99999999999998579 ) ;
#7590 = DIRECTION ( 'NONE',  ( -1.020422603260505347E-14, 1.000000000000000000, 5.551115123125782702E-17 ) ) ;
#7592 = EDGE_LOOP ( 'NONE', ( #55217, #67911, #28990, #60492 ) ) ;
#7591 = CARTESIAN_POINT ( 'NONE',  ( -127.9171280854046699, 47.84023031960693118, 84.58149700715385677 ) ) ;
#7593 = CARTESIAN_POINT ( 'NONE',  ( 82.13067365723604496, 17.93447087949267527, -49.34213147692616275 ) ) ;
#7594 = ORIENTED_EDGE ( 'NONE', *, *, #39222, .T. ) ;
#7595 = CARTESIAN_POINT ( 'NONE',  ( -148.4259959918497884, 63.26767374754764717, 72.49016198256882149 ) ) ;
#7596 = VECTOR ( 'NONE', #28483, 1000.000000000000000 ) ;
#7597 = CARTESIAN_POINT ( 'NONE',  ( 84.27937148876357298, 19.69225537006224513, 30.08568434253633228 ) ) ;
#7598 = CARTESIAN_POINT ( 'NONE',  ( -38.02163356681019479, 10.76490728754187032, 94.99999999999866418 ) ) ;
#7599 = CARTESIAN_POINT ( 'NONE',  ( 188.4904153916304779, 86.42965364612511792, -18.09992457417106237 ) ) ;
#7600 = CARTESIAN_POINT ( 'NONE',  ( 141.3403471770513420, 46.13063628128487892, -17.24135309861619803 ) ) ;
#7601 = CIRCLE ( 'NONE', #40176, 65.36598343705435354 ) ;
#7602 = CYLINDRICAL_SURFACE ( 'NONE', #44338, 7.500000000000027534 ) ;
#7603 = CARTESIAN_POINT ( 'NONE',  ( 19.03725708678846118, 7.633457022989709628, -89.93545773326505355 ) ) ;
#7604 = CARTESIAN_POINT ( 'NONE',  ( -155.6759163077703363, 69.59305396324219828, -91.70819391566057277 ) ) ;
#7605 = ORIENTED_EDGE ( 'NONE', *, *, #31141, .F. ) ;
#7606 = ORIENTED_EDGE ( 'NONE', *, *, #43316, .T. ) ;
#7607 = AXIS2_PLACEMENT_3D ( 'NONE', #45506, #54043, #11486 ) ;
#7608 = CARTESIAN_POINT ( 'NONE',  ( 105.8022841538863901, 26.88074187880707910, 57.89262865156256055 ) ) ;
#7609 = DIRECTION ( 'NONE',  ( 2.998955517602045729E-18, 4.127708154724775106E-18, -1.000000000000000000 ) ) ;
#7610 = DIRECTION ( 'NONE',  ( 1.850371928290090422E-16, -1.000000000000000000, -1.110223024625156171E-16 ) ) ;
#7611 = VECTOR ( 'NONE', #14241, 1000.000000000000000 ) ;
#7612 = CARTESIAN_POINT ( 'NONE',  ( -452.6627218934913230, 1.665334536937734811E-13, 78.55029585798817493 ) ) ;
#7613 = EDGE_CURVE ( 'NONE', #12229, #61561, #8473, .T. ) ;
#7614 = CARTESIAN_POINT ( 'NONE',  ( 34.41143668122415988, 66.58502636910522199, 41.38025477438755928 ) ) ;
#7615 = AXIS2_PLACEMENT_3D ( 'NONE', #17959, #33788, #11978 ) ;
#7616 = CARTESIAN_POINT ( 'NONE',  ( -108.1144194775597498, 35.84457139767600609, 60.12441792465978807 ) ) ;
#7617 = FACE_OUTER_BOUND ( 'NONE', #49306, .T. ) ;
#7618 = DIRECTION ( 'NONE',  ( -1.000000000000000000, -1.232595164407830946E-32, 1.387778780781445676E-15 ) ) ;
#7619 = VERTEX_POINT ( 'NONE', #18144 ) ;
#7620 = ORIENTED_EDGE ( 'NONE', *, *, #4045, .T. ) ;
#7621 = ORIENTED_EDGE ( 'NONE', *, *, #46703, .F. ) ;
#7623 = AXIS2_PLACEMENT_3D ( 'NONE', #12347, #50333, #60872 ) ;
#7622 = DIRECTION ( 'NONE',  ( 0.3881301971180111110, 0.000000000000000000, 0.9216045519012663334 ) ) ;
#7624 = FACE_OUTER_BOUND ( 'NONE', #448, .T. ) ;
#7625 = CARTESIAN_POINT ( 'NONE',  ( -83.12901536265223967, 24.07178615860086168, 70.79554670785140047 ) ) ;
#7626 = CARTESIAN_POINT ( 'NONE',  ( 126.7877523219522971, 38.47018873135922945, 39.57023082146568527 ) ) ;
#7627 = CARTESIAN_POINT ( 'NONE',  ( 106.2352375355091993, -21.75137027410914214, -3.306356075928058580 ) ) ;
#7628 = CARTESIAN_POINT ( 'NONE',  ( 181.0840389613909736, 80.03940679743416808, 29.30859410551139277 ) ) ;
#7629 = FACE_OUTER_BOUND ( 'NONE', #68479, .T. ) ;
#7630 = CARTESIAN_POINT ( 'NONE',  ( 34.84173759613682364, 7.859847277726514925, 70.23282494151600019 ) ) ;
#7631 = CARTESIAN_POINT ( 'NONE',  ( 200.0000000000000000, 2.449293598294706434E-14, -7.000000000000000000 ) ) ;
#7632 = ORIENTED_EDGE ( 'NONE', *, *, #13053, .T. ) ;
#7633 = CARTESIAN_POINT ( 'NONE',  ( -6.851003965218993130, 6.829052369041588300, -50.37077420520065374 ) ) ;
#7634 = DIRECTION ( 'NONE',  ( 1.000000000000000000, 0.000000000000000000, -0.000000000000000000 ) ) ;
#7635 = CARTESIAN_POINT ( 'NONE',  ( -452.6627218934913230, 1.665334536937734811E-13, 113.5502958579881749 ) ) ;
#7636 = EDGE_CURVE ( 'NONE', #54401, #31358, #61841, .T. ) ;
#7637 = CARTESIAN_POINT ( 'NONE',  ( -142.8450945664715164, 58.72815783657286914, 14.83098911521528862 ) ) ;
#7638 = CARTESIAN_POINT ( 'NONE',  ( 280.6590877922806158, -21.43203852822545130, -4.967093445758824721 ) ) ;
#7639 = CARTESIAN_POINT ( 'NONE',  ( -109.7647482398635503, 36.74843029291201901, -68.81159568595916198 ) ) ;
#7640 = ADVANCED_FACE ( 'NONE', ( #46950 ), #37664, .T. ) ;
#7641 = CARTESIAN_POINT ( 'NONE',  ( 128.0540543950622521, 39.18660671946769014, -11.90031528999368504 ) ) ;
#7642 = ORIENTED_EDGE ( 'NONE', *, *, #62280, .F. ) ;
#7643 = DIRECTION ( 'NONE',  ( 1.000661541931880295E-14, -4.348748082286655982E-15, 1.000000000000000000 ) ) ;
#7644 = EDGE_CURVE ( 'NONE', #16629, #65265, #45914, .T. ) ;
#7645 = CARTESIAN_POINT ( 'NONE',  ( 112.3013380801408658, 400.0000000000066507, -128.9497041420121093 ) ) ;
#7646 = CARTESIAN_POINT ( 'NONE',  ( -32.40928421737412890, 10.77259363352673205, -50.27028413111590055 ) ) ;
#7647 = DIRECTION ( 'NONE',  ( 0.000000000000000000, 0.000000000000000000, -1.000000000000000000 ) ) ;
#7648 = CARTESIAN_POINT ( 'NONE',  ( -171.2728242145607283, 85.09337373898185319, 84.72424543254817308 ) ) ;
#7649 = ORIENTED_EDGE ( 'NONE', *, *, #12554, .T. ) ;
#7650 = CARTESIAN_POINT ( 'NONE',  ( -118.9649285217356010, 42.09781191014327817, -45.29594997475566487 ) ) ;
#7651 = CARTESIAN_POINT ( 'NONE',  ( -144.2188519266540254, 59.82027639618912929, -20.79196203645875940 ) ) ;
#7652 = CARTESIAN_POINT ( 'NONE',  ( -35.00000000000002842, -35.00000000000000000, -2.000000000000000000 ) ) ;
#7653 = CIRCLE ( 'NONE', #58191, 65.36598343705435354 ) ;
#7654 =( REPRESENTATION_RELATIONSHIP ('NONE','NONE', #40274, #52783 ) REPRESENTATION_RELATIONSHIP_WITH_TRANSFORMATION ( #970 )SHAPE_REPRESENTATION_RELATIONSHIP( ) );
#7655 = CARTESIAN_POINT ( 'NONE',  ( 151.5196126176748805, 54.41511917384920594, 86.02076705022442127 ) ) ;
#7656 = EDGE_CURVE ( 'NONE', #50694, #18800, #36054, .T. ) ;
#7657 = ORIENTED_EDGE ( 'NONE', *, *, #40365, .F. ) ;
#7658 = CARTESIAN_POINT ( 'NONE',  ( 0.000000000000000000, 0.000000000000000000, 41.38025477438755928 ) ) ;
#7659 = DIRECTION ( 'NONE',  ( 0.3090169943749582759, -0.9510565162951499785, 0.000000000000000000 ) ) ;
#7660 = PLANE ( 'NONE',  #62237 ) ;
#7661 = EDGE_CURVE ( 'NONE', #16146, #17510, #62442, .T. ) ;
#7662 = EDGE_CURVE ( 'NONE', #34612, #36801, #57508, .T. ) ;
#7663 = CARTESIAN_POINT ( 'NONE',  ( 18.89064107370902690, 6.619789970027398773, -36.18630582809151264 ) ) ;
#7665 = ORIENTED_EDGE ( 'NONE', *, *, #18623, .T. ) ;
#7664 = FACE_OUTER_BOUND ( 'NONE', #66882, .T. ) ;
#7666 = CARTESIAN_POINT ( 'NONE',  ( 57.39674746172461539, 11.43903079040058834, 42.30479512360005856 ) ) ;
#7667 = VERTEX_POINT ( 'NONE', #19524 ) ;
#7668 = VERTEX_POINT ( 'NONE', #57850 ) ;
#7669 = AXIS2_PLACEMENT_3D ( 'NONE', #35372, #13230, #12525 ) ;
#7670 = CARTESIAN_POINT ( 'NONE',  ( 174.1422537179815038, 73.24254491731254291, 33.95503749249008507 ) ) ;
#7671 = CARTESIAN_POINT ( 'NONE',  ( 23.09784929786603414, 6.844738137842331760, -68.16647883290328025 ) ) ;
#7673 = ORIENTED_EDGE ( 'NONE', *, *, #59054, .T. ) ;
#7672 = CARTESIAN_POINT ( 'NONE',  ( -12.77550690612892659, 8.273784096785062658, -75.41817604663297914 ) ) ;
#7674 = CARTESIAN_POINT ( 'NONE',  ( 26.99999999999999289, 26.99999999999999645, 12.00000000000000000 ) ) ;
#7675 = CARTESIAN_POINT ( 'NONE',  ( 209.9518228411288874, -1.426547569622074412E-15, 31.43423095485942298 ) ) ;
#7676 = FACE_BOUND ( 'NONE', #25045, .T. ) ;
#7677 = EDGE_LOOP ( 'NONE', ( #51285, #13075 ) ) ;
#7678 = CARTESIAN_POINT ( 'NONE',  ( 210.9631450001601252, 117.1791136960929265, -74.83007442223710370 ) ) ;
#7679 = LINE ( 'NONE', #51281, #67959 ) ;
#7680 = CARTESIAN_POINT ( 'NONE',  ( 153.9530329262830435, 54.96668088430648424, -90.67854091719155463 ) ) ;
#7681 = CARTESIAN_POINT ( 'NONE',  ( -127.6881387055492922, 48.89937523111242967, 3.989620345208920504 ) ) ;
#7682 = DIRECTION ( 'NONE',  ( -0.000000000000000000, -0.000000000000000000, -1.000000000000000000 ) ) ;
#7683 = EDGE_LOOP ( 'NONE', ( #65023, #50621 ) ) ;
#7684 = ORIENTED_EDGE ( 'NONE', *, *, #20480, .T. ) ;
#7685 = ORIENTED_EDGE ( 'NONE', *, *, #32000, .T. ) ;
#7686 = LINE ( 'NONE', #55872, #9265 ) ;
#7687 = DIRECTION ( 'NONE',  ( 0.9839295885986295565, 0.1785568947986370392, 0.000000000000000000 ) ) ;
#7688 = DIRECTION ( 'NONE',  ( 0.000000000000000000, 1.000000000000000000, 0.000000000000000000 ) ) ;
#7689 = ADVANCED_FACE ( 'NONE', ( #9317 ), #25512, .F. ) ;
#7690 = LINE ( 'NONE', #23520, #39296 ) ;
#7691 = CARTESIAN_POINT ( 'NONE',  ( -142.8450945664714880, 58.72815783657286204, 41.67553970567896471 ) ) ;
#7692 = CARTESIAN_POINT ( 'NONE',  ( 86.62931800182293784, 19.42108912189599579, -62.66611478937537782 ) ) ;
#7693 = CARTESIAN_POINT ( 'NONE',  ( -75.43271753227887189, 22.18711452892410918, -8.986709910220804787 ) ) ;
#7694 = ORIENTED_EDGE ( 'NONE', *, *, #26148, .T. ) ;
#7695 = DIRECTION ( 'NONE',  ( -1.604841615724188478E-15, -1.000000000000000000, -1.236108373964834415E-14 ) ) ;
#7696 = ORIENTED_EDGE ( 'NONE', *, *, #35097, .F. ) ;
#7697 = AXIS2_PLACEMENT_3D ( 'NONE', #38245, #42146, #53030 ) ;
#7698 = ADVANCED_FACE ( 'NONE', ( #31464 ), #4389, .F. ) ;
#7699 = CARTESIAN_POINT ( 'NONE',  ( 31.95008798096001712, 7.556925044648907352, 38.39634584779201987 ) ) ;
#7700 = CYLINDRICAL_SURFACE ( 'NONE', #43072, 75.31295361348099959 ) ;
#7701 = DIRECTION ( 'NONE',  ( 0.000000000000000000, 1.000000000000000000, 0.000000000000000000 ) ) ;
#7702 = LINE ( 'NONE', #28809, #8561 ) ;
#7703 = CIRCLE ( 'NONE', #64983, 65.00000000000000000 ) ;
#7704 = CARTESIAN_POINT ( 'NONE',  ( -102.2801239173131052, 32.78103895658058065, 72.36362509687883460 ) ) ;
#7705 = CARTESIAN_POINT ( 'NONE',  ( -120.4666325602656087, 44.20829586446608772, 59.78203764639147266 ) ) ;
#7706 = CARTESIAN_POINT ( 'NONE',  ( -7.825402957745081878, 7.899365992529270741, -50.41807073194384259 ) ) ;
#7707 = CARTESIAN_POINT ( 'NONE',  ( -452.6627218934859229, 390.0000000000064801, -136.4497041420121661 ) ) ;
#7708 = VERTEX_POINT ( 'NONE', #8980 ) ;
#7709 = DIRECTION ( 'NONE',  ( 0.000000000000000000, 0.000000000000000000, 1.000000000000000000 ) ) ;
#7710 = CARTESIAN_POINT ( 'NONE',  ( 7.762887554996211747E-14, 51.66904755831208718, 85.00100000000000477 ) ) ;
#7711 = ORIENTED_EDGE ( 'NONE', *, *, #44198, .F. ) ;
#7712 = DIRECTION ( 'NONE',  ( 0.9195277725514487965, 0.3930250316539278255, 0.000000000000000000 ) ) ;
#7713 = CARTESIAN_POINT ( 'NONE',  ( -58.32502757340552080, 16.62877055630751499, 57.89620646628114287 ) ) ;
#7714 = CARTESIAN_POINT ( 'NONE',  ( 39.40195752203892710, -170.0000000000000000, 91.10293548689062959 ) ) ;
#7715 = ORIENTED_EDGE ( 'NONE', *, *, #26960, .F. ) ;
#7716 = EDGE_CURVE ( 'NONE', #10774, #9838, #42015, .T. ) ;
#7717 = FACE_OUTER_BOUND ( 'NONE', #45172, .T. ) ;
#7718 = CARTESIAN_POINT ( 'NONE',  ( 150.0278556977734752, 53.32860603304212077, -69.39036461173597559 ) ) ;
#7719 = CARTESIAN_POINT ( 'NONE',  ( -36.37371824399144060, 10.45334302951138739, 32.04685305616742852 ) ) ;
#7720 = EDGE_CURVE ( 'NONE', #52493, #3111, #52900, .T. ) ;
#7721 = CARTESIAN_POINT ( 'NONE',  ( 141.2366329129480675, 46.06278879703612006, -44.88589907137630064 ) ) ;
#7722 = EDGE_CURVE ( 'NONE', #5837, #45785, #53480, .T. ) ;
#7723 = EDGE_LOOP ( 'NONE', ( #48333, #42067, #60467, #8377 ) ) ;
#7724 = DIRECTION ( 'NONE',  ( -1.000000000000000000, 0.000000000000000000, 0.000000000000000000 ) ) ;
#7725 = ORIENTED_EDGE ( 'NONE', *, *, #8877, .T. ) ;
#7726 = CARTESIAN_POINT ( 'NONE',  ( 32.15613847490628530, 8.588587416860168133, -18.22703462462936486 ) ) ;
#7727 = DIRECTION ( 'NONE',  ( -1.000000000000000000, 0.000000000000000000, 0.000000000000000000 ) ) ;
#7728 = CARTESIAN_POINT ( 'NONE',  ( -156.9402586331177361, -170.0000000000000000, -95.00000000000133582 ) ) ;
#7729 = CARTESIAN_POINT ( 'NONE',  ( 88.98408042523108463, 20.23787745328938215, 56.93183881311599492 ) ) ;
#7730 = DIRECTION ( 'NONE',  ( -0.000000000000000000, 1.000000000000000000, -0.000000000000000000 ) ) ;
#7731 = DIRECTION ( 'NONE',  ( 0.2660368455666687892, 0.9639628606958550172, 0.000000000000000000 ) ) ;
#7732 = B_SPLINE_CURVE_WITH_KNOTS ( 'NONE', 3,
 ( #37324, #25418, #4628, #31034 ),
 .UNSPECIFIED., .F., .F.,
 ( 4, 4 ),
 ( 0.1259919275528360860, 0.1829744153748753543 ),
 .UNSPECIFIED. ) ;
#7733 = DIRECTION ( 'NONE',  ( 0.9749279121818226201, 0.2225209339563184452, 0.000000000000000000 ) ) ;
#7734 = VERTEX_POINT ( 'NONE', #53587 ) ;
#7735 = CARTESIAN_POINT ( 'NONE',  ( 159.2389084450350083, 59.03884018680377466, -9.477483402660668688 ) ) ;
#7736 = DIRECTION ( 'NONE',  ( 0.000000000000000000, 0.000000000000000000, 1.000000000000000000 ) ) ;
#7737 = CARTESIAN_POINT ( 'NONE',  ( 70.26722489419888973, 14.47234958177329389, 62.17998598294791890 ) ) ;
#7738 = CARTESIAN_POINT ( 'NONE',  ( 139.1353280997809634, 44.70436000187871883, -65.03450818519148413 ) ) ;
#7739 = CARTESIAN_POINT ( 'NONE',  ( 73.79471914489722906, 13.39176710989777952, 43.58025477438756212 ) ) ;
#7740 = EDGE_CURVE ( 'NONE', #67838, #11106, #32839, .T. ) ;
#7741 = ADVANCED_FACE ( 'NONE', ( #10341 ), #11032, .T. ) ;
#7742 = ORIENTED_EDGE ( 'NONE', *, *, #31957, .T. ) ;
#7743 = ADVANCED_FACE ( 'NONE', ( #48296 ), #26532, .T. ) ;
#7744 = B_SPLINE_CURVE_WITH_KNOTS ( 'NONE', 3,
 ( #19448, #56051, #68921, #34949, #24048, #9856 ),
 .UNSPECIFIED., .F., .F.,
 ( 4, 2, 4 ),
 ( 0.008690415895085791889, 0.01102883710845594875, 0.01336725832182610388 ),
 .UNSPECIFIED. ) ;
#7745 = CARTESIAN_POINT ( 'NONE',  ( 162.0812592823604916, 62.62783216273700049, -10.84498442540020413 ) ) ;
#7746 = CARTESIAN_POINT ( 'NONE',  ( 8.540853903193188046, 6.376814430361483765, 39.46023411190206787 ) ) ;
#7747 = ORIENTED_EDGE ( 'NONE', *, *, #10645, .T. ) ;
#7748 = CARTESIAN_POINT ( 'NONE',  ( 63.99027454648602031, 13.93445177372598742, 56.70534288924221755 ) ) ;
#7749 = CARTESIAN_POINT ( 'NONE',  ( 128.9313283535441599, 38.52887643767397918, -91.54200002570384243 ) ) ;
#7750 = CIRCLE ( 'NONE', #69485, 65.00000000000000000 ) ;
#7751 = EDGE_LOOP ( 'NONE', ( #37065, #32453, #22846, #15459 ) ) ;
#7752 = CARTESIAN_POINT ( 'NONE',  ( 158.3636111008086687, 59.62671916656142201, -36.12418429913763163 ) ) ;
#7753 = CARTESIAN_POINT ( 'NONE',  ( -149.5074843970971017, 65.50121172469319220, -22.96827994102830317 ) ) ;
#7754 = DIRECTION ( 'NONE',  ( -0.000000000000000000, 0.000000000000000000, -1.000000000000000000 ) ) ;
#7755 = VECTOR ( 'NONE', #58395, 1000.000000000000000 ) ;
#7756 = CARTESIAN_POINT ( 'NONE',  ( 26.69682282325710787, 59.27986298182224800, 43.58025477438756923 ) ) ;
#7757 = ORIENTED_EDGE ( 'NONE', *, *, #62641, .T. ) ;
#7758 = DIRECTION ( 'NONE',  ( 1.000000000000000000, 0.000000000000000000, 0.000000000000000000 ) ) ;
#7759 = CARTESIAN_POINT ( 'NONE',  ( 0.000000000000000000, 0.000000000000000000, 40.00000000000003553 ) ) ;
#7760 = CARTESIAN_POINT ( 'NONE',  ( 33.31166872005966439, 8.707041209322246900, 33.02990241366695301 ) ) ;
#7761 = CARTESIAN_POINT ( 'NONE',  ( 84.27937148876361562, 19.69225537006224869, -23.60341683839102345 ) ) ;
#7762 = CARTESIAN_POINT ( 'NONE',  ( -130.5740389938243027, 49.65308610043482673, -9.689013956004959738 ) ) ;
#7763 = CARTESIAN_POINT ( 'NONE',  ( 35.45122521384750058, 8.940329117834592054, -90.37916076915726649 ) ) ;
#7764 = CARTESIAN_POINT ( 'NONE',  ( 131.6005058089755266, 40.07838125795769457, -77.53578642827864087 ) ) ;
#7765 = ORIENTED_EDGE ( 'NONE', *, *, #14723, .T. ) ;
#7766 = CARTESIAN_POINT ( 'NONE',  ( -64.97888516016270444, -7.103257987406320417, 41.38025477438755928 ) ) ;
#7767 = DIRECTION ( 'NONE',  ( 1.000000000000000000, -0.000000000000000000, -0.000000000000000000 ) ) ;
#7768 = ORIENTED_EDGE ( 'NONE', *, *, #47234, .T. ) ;
#7769 = CARTESIAN_POINT ( 'NONE',  ( -155.2836587093739524, 70.59655508952971559, -47.10335330728528902 ) ) ;
#7770 = CARTESIAN_POINT ( 'NONE',  ( 13.02837879071828198, -36.05214194840069553, 13.32819299319723072 ) ) ;
#7771 = CARTESIAN_POINT ( 'NONE',  ( -38.16652041892307778, 11.81761816422916311, 34.36470182406579710 ) ) ;
#7772 = CARTESIAN_POINT ( 'NONE',  ( -0.8863172752569277169, 7.545240277686256825, 40.49273171542998284 ) ) ;
#7773 = DIRECTION ( 'NONE',  ( -0.000000000000000000, -0.000000000000000000, 1.000000000000000000 ) ) ;
#7774 = CARTESIAN_POINT ( 'NONE',  ( -55.05276343752909440, 14.68156374112638929, -77.06087458892358200 ) ) ;
#7775 = CARTESIAN_POINT ( 'NONE',  ( -44.39004539972346208, 1.224646799147353059E-15, 5.000000000000000000 ) ) ;
#7776 = CARTESIAN_POINT ( 'NONE',  ( -15.32495246574475267, 8.506829480038510027, 37.11362200784080301 ) ) ;
#7777 = CARTESIAN_POINT ( 'NONE',  ( -62.49130718206700408, 16.80297926264071151, 9.982333063200602652 ) ) ;
#7778 = ORIENTED_EDGE ( 'NONE', *, *, #45908, .F. ) ;
#7779 = EDGE_CURVE ( 'NONE', #44138, #63882, #58869, .T. ) ;
#7780 = CARTESIAN_POINT ( 'NONE',  ( -94.78138776532242105, 30.24234841992715417, -41.97853113865350139 ) ) ;
#7781 = ORIENTED_EDGE ( 'NONE', *, *, #17137, .T. ) ;
#7782 = CARTESIAN_POINT ( 'NONE',  ( 311.9975424824652350, 179.2896996249788799, 369.5505932007772003 ) ) ;
#7783 = CARTESIAN_POINT ( 'NONE',  ( 46.51679720856117228, 10.46086439153924097, -18.69848944342430030 ) ) ;
#7784 = CARTESIAN_POINT ( 'NONE',  ( 46.89006465517228861, 9.501960077668741178, 64.74722328374446079 ) ) ;
#7785 = CARTESIAN_POINT ( 'NONE',  ( 290.0000000000000568, 5.000000000000000888, 19.36491673103706290 ) ) ;
#7786 = CARTESIAN_POINT ( 'NONE',  ( -15.30839993758081263, 7.494375438621725394, 91.90590778965562890 ) ) ;
#7787 = VECTOR ( 'NONE', #19090, 999.9999999999998863 ) ;
#7788 = DIRECTION ( 'NONE',  ( 0.000000000000000000, 0.000000000000000000, 1.000000000000000000 ) ) ;
#7789 = CARTESIAN_POINT ( 'NONE',  ( 63.01563776193090405, 13.70579113808096672, -89.40979201309708913 ) ) ;
#7790 = CARTESIAN_POINT ( 'NONE',  ( -25.99999999999998934, 0.000000000000000000, -50.00000000000000000 ) ) ;
#7791 = ORIENTED_EDGE ( 'NONE', *, *, #54955, .F. ) ;
#7792 = ORIENTED_EDGE ( 'NONE', *, *, #33532, .T. ) ;
#7793 = EDGE_CURVE ( 'NONE', #20799, #36282, #3921, .T. ) ;
#7794 = FACE_BOUND ( 'NONE', #49270, .T. ) ;
#7795 = DIRECTION ( 'NONE',  ( -1.000000000000000000, 0.000000000000000000, 0.000000000000000000 ) ) ;
#7796 = CARTESIAN_POINT ( 'NONE',  ( -36.11269837220806522, 5.594483210025202879E-14, 2.000000000000001776 ) ) ;
#7797 = LINE ( 'NONE', #50700, #3590 ) ;
#7798 = CARTESIAN_POINT ( 'NONE',  ( -6.802008071587399840, 24.18409554641266368, 3.061616997868437868E-16 ) ) ;
#7799 = EDGE_CURVE ( 'NONE', #3462, #61751, #2578, .T. ) ;
#7800 = AXIS2_PLACEMENT_3D ( 'NONE', #47017, #41741, #61888 ) ;
#7801 = EDGE_CURVE ( 'NONE', #32122, #46342, #69151, .T. ) ;
#7802 = CARTESIAN_POINT ( 'NONE',  ( 59.94652978725889625, 13.01168383647462790, -9.528566960319547974 ) ) ;
#7803 = ORIENTED_EDGE ( 'NONE', *, *, #49798, .T. ) ;
#7804 = CIRCLE ( 'NONE', #25785, 5.000000000000004441 ) ;
#7805 = CARTESIAN_POINT ( 'NONE',  ( 105.2529848321548229, 27.73895015262024089, -49.02683151908587433 ) ) ;
#7806 = CARTESIAN_POINT ( 'NONE',  ( -14.94265033805045917, 7.459411036484910440, 62.04421683837972523 ) ) ;
#7807 = CARTESIAN_POINT ( 'NONE',  ( 11.21312910819262321, 7.403355431336986037, 58.39587251282808467 ) ) ;
#7808 = PLANE ( 'NONE',  #52124 ) ;
#7809 = CARTESIAN_POINT ( 'NONE',  ( 211.8476521439973794, 116.6941316755177525, -14.69380237910506715 ) ) ;
#7810 = FACE_BOUND ( 'NONE', #28442, .T. ) ;
#7811 = EDGE_LOOP ( 'NONE', ( #57220, #47137, #53766, #56814, #30774 ) ) ;
#7812 = CARTESIAN_POINT ( 'NONE',  ( 0.000000000000000000, 0.000000000000000000, 170.0000000000000000 ) ) ;
#7813 = CARTESIAN_POINT ( 'NONE',  ( -15.76129977463437015, -63.43731725181460490, 6.377659838150115899E-18 ) ) ;
#7814 = CARTESIAN_POINT ( 'NONE',  ( 74.99999999999998579, 0.000000000000000000, 25.00000000000007816 ) ) ;
#7815 = CARTESIAN_POINT ( 'NONE',  ( -178.5750994113944614, 94.98114813978524751, 6.304711435512811768 ) ) ;
#7816 = CARTESIAN_POINT ( 'NONE',  ( 210.0055645826033697, 115.7254585628714096, 58.23048686943388219 ) ) ;
#7817 = VECTOR ( 'NONE', #28, 1000.000000000000000 ) ;
#7818 = ADVANCED_FACE ( 'NONE', ( #45477 ), #22635, .T. ) ;
#7819 = LINE ( 'NONE', #16957, #43428 ) ;
#7820 = ORIENTED_EDGE ( 'NONE', *, *, #55941, .T. ) ;
#7821 = EDGE_CURVE ( 'NONE', #58090, #989, #27627, .T. ) ;
#7822 = DIRECTION ( 'NONE',  ( -1.000000000000000000, -1.387778780781448141E-16, 5.551115123125781716E-16 ) ) ;
#7823 = CARTESIAN_POINT ( 'NONE',  ( 199.3764173596862577, 100.9540560740992277, -49.13558951988117229 ) ) ;
#7824 = ORIENTED_EDGE ( 'NONE', *, *, #59236, .T. ) ;
#7825 =( BOUNDED_CURVE ( )  B_SPLINE_CURVE ( 3, ( #27691, #33341, #17487, #29102 ),
 .UNSPECIFIED., .F., .F. ) 
 B_SPLINE_CURVE_WITH_KNOTS ( ( 4, 4 ),
 ( 1.570796326794896558, 3.141592653589793116 ),
 .UNSPECIFIED. ) 
 CURVE ( )  GEOMETRIC_REPRESENTATION_ITEM ( )  RATIONAL_B_SPLINE_CURVE ( ( 1.000000000000000000, 0.8047378541243649375, 0.8047378541243649375, 1.000000000000000000 ) ) 
 REPRESENTATION_ITEM ( '' )  );
#7826 = FACE_OUTER_BOUND ( 'NONE', #51753, .T. ) ;
#7827 = VERTEX_POINT ( 'NONE', #12089 ) ;
#7828 = CARTESIAN_POINT ( 'NONE',  ( -83.69653436244854561, 24.30167057287989962, -63.89149677819863626 ) ) ;
#7829 = CYLINDRICAL_SURFACE ( 'NONE', #28638, 30.00000000000000000 ) ;
#7830 = DIRECTION ( 'NONE',  ( -0.000000000000000000, 1.000000000000000000, -0.000000000000000000 ) ) ;
#7831 = ORIENTED_EDGE ( 'NONE', *, *, #22808, .T. ) ;
#7832 = EDGE_LOOP ( 'NONE', ( #653, #10988, #66625, #15834 ) ) ;
#7833 = CARTESIAN_POINT ( 'NONE',  ( 46.23113030541875901, 10.41513832761375546, 67.36843900475240332 ) ) ;
#7834 = AXIS2_PLACEMENT_3D ( 'NONE', #47808, #36233, #21092 ) ;
#7835 = CARTESIAN_POINT ( 'NONE',  ( -105.5471966583786099, 35.60982465102040351, -89.44928979052285456 ) ) ;
#7836 = CARTESIAN_POINT ( 'NONE',  ( 110.2429982417149574, 29.99119854320843714, 17.76666361527367499 ) ) ;
#7837 = VERTEX_POINT ( 'NONE', #39516 ) ;
#7838 = FACE_OUTER_BOUND ( 'NONE', #5130, .T. ) ;
#7839 = CARTESIAN_POINT ( 'NONE',  ( 59.72647370436681769, 12.96353798836694615, -36.47598787309180324 ) ) ;
#7840 = CARTESIAN_POINT ( 'NONE',  ( -13.74877239730504286, 8.359278534280710105, -91.92798095535714253 ) ) ;
#7841 = CARTESIAN_POINT ( 'NONE',  ( 111.1868021579656869, 29.32055685204858619, -9.122472411873387088 ) ) ;
#7842 = B_SPLINE_CURVE_WITH_KNOTS ( 'NONE', 3,
 ( #10268, #31730, #3284, #52500, #24742, #25783, #46177, #67651, #19447, #47210, #62365, #14180, #57093, #8906, #51810, #25088, #46525, #43654, #21862, #53165, #405, #6022, #49276, #38391, #16587, #48570, #69364, #59141, #5674, #33127, #22217, #42629, #10611, #21183, #48923, #43305, #15898, #64086, #32430, #64429, #54199, #42958, #27137, #4997, #763, #53857 ),
 .UNSPECIFIED., .F., .F.,
 ( 4, 2, 2, 2, 2, 2, 2, 2, 2, 2, 2, 2, 2, 2, 2, 2, 2, 2, 2, 2, 2, 2, 4 ),
 ( 0.000000000000000000, 0.003373244802897216229, 0.004216556003621520395, 0.005059867204345824994, 0.006746489605794432458, 0.007589800806518737057, 0.008433112007243040789, 0.009276423207967343654, 0.01011973440869164999, 0.01180635681014026439, 0.01349297921158888053, 0.01433629041231318686, 0.01517960161303749493, 0.01686622401448609199, 0.01770953521521038618, 0.01855284641593467690, 0.02023946881738333120, 0.02108278001810763233, 0.02192609121883193346, 0.02361271362028053572, 0.02445602482100480909, 0.02529933602172908594, 0.02698595842317762922 ),
 .UNSPECIFIED. ) ;
#7843 = VECTOR ( 'NONE', #52125, 1000.000000000000000 ) ;
#7844 = CARTESIAN_POINT ( 'NONE',  ( 92.81079987519940744, 21.62352428699447771, 86.64070398657467820 ) ) ;
#7846 = ORIENTED_EDGE ( 'NONE', *, *, #15818, .T. ) ;
#7845 = CARTESIAN_POINT ( 'NONE',  ( -45.00000000000002132, 20.00000000000000355, 2.000000000000015543 ) ) ;
#7847 = EDGE_LOOP ( 'NONE', ( #39035, #6466 ) ) ;
#7848 = AXIS2_PLACEMENT_3D ( 'NONE', #13443, #34905, #25043 ) ;
#7850 = ORIENTED_EDGE ( 'NONE', *, *, #19845, .F. ) ;
#7849 = PRODUCT_RELATED_PRODUCT_CATEGORY ( 'part', '', ( #25383 ) ) ;
#7851 = CARTESIAN_POINT ( 'NONE',  ( 46.76970795284344717, 9.482505412758841956, 12.03441307903643498 ) ) ;
#7852 = DIRECTION ( 'NONE',  ( -0.000000000000000000, 1.000000000000000000, -0.000000000000000000 ) ) ;
#7853 = CARTESIAN_POINT ( 'NONE',  ( -47.68742944762958302, 12.82957801017946409, -14.39326825997502901 ) ) ;
#7854 = DIRECTION ( 'NONE',  ( 1.000000000000000000, 0.000000000000000000, 0.000000000000000000 ) ) ;
#7855 = CARTESIAN_POINT ( 'NONE',  ( 198.7084915431530874, 98.47675983942194478, 5.340935046836625233 ) ) ;
#7856 = CARTESIAN_POINT ( 'NONE',  ( 212.1850009103741570, 119.0680341029749485, 91.03128498463323126 ) ) ;
#7857 = EDGE_CURVE ( 'NONE', #3570, #34941, #44074, .T. ) ;
#7858 = FACE_OUTER_BOUND ( 'NONE', #56705, .T. ) ;
#7859 = CARTESIAN_POINT ( 'NONE',  ( -85.10909119100207931, 25.97025675005452072, 60.89070622084423690 ) ) ;
#7860 = CARTESIAN_POINT ( 'NONE',  ( -14.76369756425703805, 7.442560416198674034, 40.49465273683735234 ) ) ;
#7861 = EDGE_LOOP ( 'NONE', ( #16126, #1375 ) ) ;
#7862 = ADVANCED_FACE ( 'NONE', ( #65558 ), #24036, .F. ) ;
#7863 = CARTESIAN_POINT ( 'NONE',  ( 9.819093282782491272, 7.389085782749407194, -11.60726699437242715 ) ) ;
#7864 = ORIENTED_EDGE ( 'NONE', *, *, #36472, .T. ) ;
#7865 = EDGE_LOOP ( 'NONE', ( #21923, #11913, #4394 ) ) ;
#7866 = DIRECTION ( 'NONE',  ( 1.000000000000000000, 0.000000000000000000, 2.775557561562796688E-15 ) ) ;
#7867 = CARTESIAN_POINT ( 'NONE',  ( 188.0094179620990928, 87.39792407168457089, -73.46270491724961005 ) ) ;
#7868 = CARTESIAN_POINT ( 'NONE',  ( -30.80792614961258380, 10.50774217500252483, 83.92525404607846440 ) ) ;
#7869 = VECTOR ( 'NONE', #62960, 1000.000000000000000 ) ;
#7870 = CARTESIAN_POINT ( 'NONE',  ( 100.0000000000000284, 5.000000000000000000, 18.50000000000000000 ) ) ;
#7871 = CARTESIAN_POINT ( 'NONE',  ( -31.43908319763710679, -170.0000000000000000, 64.56100499665288339 ) ) ;
#7872 = CARTESIAN_POINT ( 'NONE',  ( 13.84704553156521456, 7.452804552247569880, -50.26752412725904406 ) ) ;
#7873 = CARTESIAN_POINT ( 'NONE',  ( 132.0582325211144905, 40.34869848118183455, -36.22807681384569634 ) ) ;
#7874 = ORIENTED_EDGE ( 'NONE', *, *, #48965, .T. ) ;
#7875 = VERTEX_POINT ( 'NONE', #23687 ) ;
#7876 = CARTESIAN_POINT ( 'NONE',  ( 188.5503229283306439, 87.99928427996027835, 89.75865996300565541 ) ) ;
#7877 = LINE ( 'NONE', #61339, #37506 ) ;
#7878 = CARTESIAN_POINT ( 'NONE',  ( -3.841371665203041630E-11, 0.000000000000000000, 10.00000000000000000 ) ) ;
#7879 = CARTESIAN_POINT ( 'NONE',  ( 59.08638499266954369, 11.79550614876704095, -22.76912641790571712 ) ) ;
#7880 = ADVANCED_FACE ( 'NONE', ( #45130 ), #61315, .F. ) ;
#7881 = ADVANCED_FACE ( 'NONE', ( #1528 ), #6463, .F. ) ;
#7882 = UNCERTAINTY_MEASURE_WITH_UNIT (LENGTH_MEASURE( 1.000000000000000082E-05 ), #14926, 'distance_accuracy_value', 'NONE');
#7883 = DIRECTION ( 'NONE',  ( 0.000000000000000000, -7.395570986446983486E-32, -1.000000000000000000 ) ) ;
#7884 = VECTOR ( 'NONE', #4400, 1000.000000000000000 ) ;
#7885 = CARTESIAN_POINT ( 'NONE',  ( 60.74750367560205433, 24.13405452624938263, 41.38025477438755928 ) ) ;
#7886 = ORIENTED_EDGE ( 'NONE', *, *, #16289, .F. ) ;
#7887 = CARTESIAN_POINT ( 'NONE',  ( -24.98026281234599821, -0.9932118737290694943, 0.000000000000000000 ) ) ;
#7888 = CARTESIAN_POINT ( 'NONE',  ( -57.89360549284272395, 16.50663738101750511, -62.60719078153508121 ) ) ;
#7889 = CARTESIAN_POINT ( 'NONE',  ( 198.7123879174244507, 100.1053816708572270, -75.19790834202754581 ) ) ;
#7890 = CARTESIAN_POINT ( 'NONE',  ( 276.0266963907629361, -21.78888161821124569, 3.052770673153777814 ) ) ;
#7891 = CARTESIAN_POINT ( 'NONE',  ( 209.9999999999999716, -57.00000000000007816, 72.99999999999998579 ) ) ;
#7892 = CARTESIAN_POINT ( 'NONE',  ( -166.9969673948021693, 80.56076768517785069, 15.81477353917873785 ) ) ;
#7893 = FACE_OUTER_BOUND ( 'NONE', #22120, .T. ) ;
#7894 = FACE_BOUND ( 'NONE', #26965, .T. ) ;
#7895 = LINE ( 'NONE', #7193, #51248 ) ;
#7896 = CARTESIAN_POINT ( 'NONE',  ( -6.840981040171499217, 6.828436339979226055, 71.91165652771135797 ) ) ;
#7897 = ORIENTED_EDGE ( 'NONE', *, *, #23089, .F. ) ;
#7898 = CARTESIAN_POINT ( 'NONE',  ( 279.6730658560643974, 21.42428528562853884, -4.999999999999992006 ) ) ;
#7899 = CARTESIAN_POINT ( 'NONE',  ( 150.4722669492348359, 53.65054032737662482, 61.04279154623130665 ) ) ;
#7900 = DIRECTION ( 'NONE',  ( 1.000000000000000000, 0.000000000000000000, 0.000000000000000000 ) ) ;
#7901 = DIRECTION ( 'NONE',  ( -0.000000000000000000, 1.000000000000000000, 1.877893248421448789E-16 ) ) ;
#7902 = CIRCLE ( 'NONE', #51730, 5.000000000000000888 ) ;
#7903 = DIRECTION ( 'NONE',  ( 0.000000000000000000, 0.000000000000000000, -1.000000000000000000 ) ) ;
#7904 = ORIENTED_EDGE ( 'NONE', *, *, #34403, .F. ) ;
#7905 = SURFACE_STYLE_USAGE ( .BOTH. , #29353 ) ;
#7906 = CARTESIAN_POINT ( 'NONE',  ( 0.000000000000000000, 0.000000000000000000, 41.38025477438755928 ) ) ;
#7907 = ORIENTED_EDGE ( 'NONE', *, *, #42027, .T. ) ;
#7908 = ORIENTED_EDGE ( 'NONE', *, *, #5906, .F. ) ;
#7909 = DIRECTION ( 'NONE',  ( 0.000000000000000000, 0.000000000000000000, 1.000000000000000000 ) ) ;
#7910 = CARTESIAN_POINT ( 'NONE',  ( 149.9883446984744921, 53.30011109831374938, 36.32171926678490337 ) ) ;
#7911 = LINE ( 'NONE', #18466, #44802 ) ;
#7912 = ORIENTED_EDGE ( 'NONE', *, *, #206, .T. ) ;
#7913 = DIRECTION ( 'NONE',  ( 1.000000000000000000, 0.000000000000000000, -0.000000000000000000 ) ) ;
#7914 = CARTESIAN_POINT ( 'NONE',  ( -177.1539090641758207, 91.73101548694631902, 17.81618785780625558 ) ) ;
#7915 = CARTESIAN_POINT ( 'NONE',  ( -0.3734056954813061990, 6.520221844775924147, 11.74911637933309372 ) ) ;
#7916 = VECTOR ( 'NONE', #15980, 1000.000000000000114 ) ;
#7917 = CARTESIAN_POINT ( 'NONE',  ( 55.64941011647476898, 12.11006142851271328, -41.74712242361913894 ) ) ;
#7918 = CARTESIAN_POINT ( 'NONE',  ( -79.14094329813315198, 23.58034730000057877, 30.41820113967311201 ) ) ;
#7919 = CARTESIAN_POINT ( 'NONE',  ( -26.88234027341226096, 9.904106450608203716, -21.94961641608552227 ) ) ;
#7920 = CARTESIAN_POINT ( 'NONE',  ( 139.6359093656973300, 45.02518919224739591, 14.95245080739227994 ) ) ;
#7921 = ORIENTED_EDGE ( 'NONE', *, *, #53261, .T. ) ;
#7922 = CARTESIAN_POINT ( 'NONE',  ( 117.7447573007802646, 32.50990724960316669, -42.93223025960289618 ) ) ;
#7923 = CARTESIAN_POINT ( 'NONE',  ( -71.42007367207963853, 20.75704712149298814, 9.074083910195316349 ) ) ;
#7924 = CARTESIAN_POINT ( 'NONE',  ( 41.35041461497704773, 8.670465437677199461, -35.86060275886635651 ) ) ;
#7925 = PLANE ( 'NONE',  #15187 ) ;
#7927 = ORIENTED_EDGE ( 'NONE', *, *, #36685, .T. ) ;
#7926 = CARTESIAN_POINT ( 'NONE',  ( -118.3864707679337016, 41.74547427441078895, 91.72959842008201292 ) ) ;
#7928 = CARTESIAN_POINT ( 'NONE',  ( 83.37786665291103816, 18.33670623396829313, -36.54571592794794554 ) ) ;
#7929 = EDGE_CURVE ( 'NONE', #3613, #32490, #29306, .T. ) ;
#7930 = ORIENTED_EDGE ( 'NONE', *, *, #15029, .T. ) ;
#7931 = DIRECTION ( 'NONE',  ( -1.000000000000000000, 0.000000000000000000, -0.000000000000000000 ) ) ;
#7932 = CARTESIAN_POINT ( 'NONE',  ( 79.18180043629686793, 18.06526831600444893, 36.19349848600327846 ) ) ;
#7933 = CYLINDRICAL_SURFACE ( 'NONE', #11850, 125.0000000000000000 ) ;
#7934 = CARTESIAN_POINT ( 'NONE',  ( 188.2133404574782958, 86.12414067617879709, -14.53428918749921017 ) ) ;
#7935 = EDGE_CURVE ( 'NONE', #49581, #14060, #22990, .T. ) ;
#7936 = CARTESIAN_POINT ( 'NONE',  ( 209.9518228411288874, 170.0000000000000284, 31.43423095485942298 ) ) ;
#7937 = LINE ( 'NONE', #49785, #59100 ) ;
#7938 = CARTESIAN_POINT ( 'NONE',  ( -173.5422248620772621, 89.11126078969417108, -7.867406574286299303 ) ) ;
#7939 = EDGE_CURVE ( 'NONE', #21445, #26335, #17360, .T. ) ;
#7940 = DIRECTION ( 'NONE',  ( -0.000000000000000000, 0.000000000000000000, 1.000000000000000000 ) ) ;
#7941 = ORIENTED_EDGE ( 'NONE', *, *, #41756, .F. ) ;
#7942 = ORIENTED_EDGE ( 'NONE', *, *, #68285, .T. ) ;
#7943 = EDGE_CURVE ( 'NONE', #26420, #56407, #39177, .T. ) ;
#7944 = CARTESIAN_POINT ( 'NONE',  ( 103.0103829243729052, 25.67737053862328978, 66.00548782892786903 ) ) ;
#7945 = FACE_OUTER_BOUND ( 'NONE', #52953, .T. ) ;
#7946 = DIRECTION ( 'NONE',  ( 0.000000000000000000, 0.000000000000000000, 1.000000000000000000 ) ) ;
#7947 = EDGE_CURVE ( 'NONE', #10403, #44678, #50066, .T. ) ;
#7948 = CARTESIAN_POINT ( 'NONE',  ( 188.4359598230020367, 86.36951380984527304, -45.23692044763556197 ) ) ;
#7949 = DIRECTION ( 'NONE',  ( -0.000000000000000000, -0.000000000000000000, -1.000000000000000000 ) ) ;
#7950 = LINE ( 'NONE', #29402, #36235 ) ;
#7951 = CARTESIAN_POINT ( 'NONE',  ( 157.9130201331580849, 57.99550255803047349, -77.96873488960136456 ) ) ;
#7952 = ORIENTED_EDGE ( 'NONE', *, *, #23621, .T. ) ;
#7953 = VERTEX_POINT ( 'NONE', #23351 ) ;
#7954 = ORIENTED_EDGE ( 'NONE', *, *, #20668, .F. ) ;
#7955 = CARTESIAN_POINT ( 'NONE',  ( -78.66644367742111399, -170.0000000000000000, -50.11545063171791270 ) ) ;
#7956 = CARTESIAN_POINT ( 'NONE',  ( -80.81202825120918476, 23.15032834068050249, 84.41426225767527569 ) ) ;
#7957 = DIRECTION ( 'NONE',  ( -0.000000000000000000, 1.000000000000000000, -0.000000000000000000 ) ) ;
#7958 = ADVANCED_FACE ( 'NONE', ( #7858 ), #50757, .F. ) ;
#7959 = LINE ( 'NONE', #38569, #15229 ) ;
#7960 = FACE_OUTER_BOUND ( 'NONE', #31655, .T. ) ;
#7961 = CARTESIAN_POINT ( 'NONE',  ( -60.64199216239839529, 17.30050036439947903, 32.81023052909118576 ) ) ;
#7962 = VECTOR ( 'NONE', #11060, 1000.000000000000000 ) ;
#7963 = CARTESIAN_POINT ( 'NONE',  ( -8.000000000000000000, -4.618802153517023612, -9.500000000000000000 ) ) ;
#7964 = CARTESIAN_POINT ( 'NONE',  ( 61.08522853873727598, 13.26388801693371455, 44.57671891123612795 ) ) ;
#7965 = DIRECTION ( 'NONE',  ( -0.000000000000000000, -1.000000000000000000, -0.000000000000000000 ) ) ;
#7966 = VERTEX_POINT ( 'NONE', #3960 ) ;
#7967 = CARTESIAN_POINT ( 'NONE',  ( -1.857619870843145948, 6.575690665396235701, -38.34909718101288689 ) ) ;
#7968 = LINE ( 'NONE', #18180, #3771 ) ;
#7969 = CARTESIAN_POINT ( 'NONE',  ( -15.32584732649904247, 8.506915958926390076, 11.25943598086905872 ) ) ;
#7970 = CARTESIAN_POINT ( 'NONE',  ( -148.4259959918497316, 63.26767374754767559, 18.80106080164143378 ) ) ;
#7971 = CARTESIAN_POINT ( 'NONE',  ( 284.9681307937125894, -21.99268844340181417, -0.6535439379101346535 ) ) ;
#7972 = CARTESIAN_POINT ( 'NONE',  ( 197.6145711261844724, 97.10888456119688783, 61.00577141233620182 ) ) ;
#7973 = VECTOR ( 'NONE', #8628, 1000.000000000000000 ) ;
#7974 = CARTESIAN_POINT ( 'NONE',  ( 130.3281282802763315, 40.49854652972194913, -23.31374654723702378 ) ) ;
#7975 = B_SPLINE_CURVE_WITH_KNOTS ( 'NONE', 3,
 ( #11381, #42708, #32849, #21597, #38837, #37428, #49708, #43044, #15978, #28262, #32505, #38121, #16668, #64516, #60285, #846, #27218, #54286, #49009, #27920, #49358, #22298, #1191, #17358, #33568, #1539, #58879, #7868, #40220, #61669, #60629, #23696, #12445, #66969, #45487, #50077, #39868, #13827, #13487, #50766, #61326, #2249, #30014, #24047, #1907, #66619, #13151, #2587, #67317, #44806, #62009, #8563, #56745, #34948, #55700, #33905 ),
 .UNSPECIFIED., .F., .F.,
 ( 4, 2, 2, 2, 2, 2, 2, 2, 2, 2, 2, 2, 2, 2, 2, 2, 2, 2, 2, 1, 2, 2, 2, 2, 2, 2, 1, 2, 4 ),
 ( 0.000000000000000000, 0.001942337377849021095, 0.002913506066773531751, 0.003884674755698042190, 0.004855843444622553497, 0.005827012133547063502, 0.006798180822471573508, 0.007769349511396084380, 0.009711686889245072299, 0.01068285557816955368, 0.01165402426709403680, 0.01262519295601851992, 0.01359636164494300303, 0.01456753033386748615, 0.01553869902279196927, 0.01748103640064091469, 0.01845220508956538566, 0.01942337377848985316, 0.02039454246741432067, 0.02136571115633879164, 0.02233687984526325915, 0.02330804853418772665, 0.02525038591203665472, 0.02622155460096109794, 0.02719272328988554463, 0.02816389197880998785, 0.02913506066773443454, 0.03010622935665888122, 0.03107739804558332444 ),
 .UNSPECIFIED. ) ;
#7976 = EDGE_LOOP ( 'NONE', ( #6270, #47375, #12404, #6426 ) ) ;
#7977 = DIRECTION ( 'NONE',  ( 9.145108480375273253E-15, -4.225426482089628201E-15, 0.9999999999999997780 ) ) ;
#7978 = VECTOR ( 'NONE', #16221, 1000.000000000000000 ) ;
#7979 = DIRECTION ( 'NONE',  ( -0.3930250316539278255, 0.9195277725514487965, 0.000000000000000000 ) ) ;
#7980 = CARTESIAN_POINT ( 'NONE',  ( -452.6627218934913230, 399.9999999999997726, 83.55029585798818914 ) ) ;
#7981 = CARTESIAN_POINT ( 'NONE',  ( 0.01688885742776972607, -7.321065037175430668, -3.319543390096033164 ) ) ;
#7982 = CARTESIAN_POINT ( 'NONE',  ( -172.0255068454375476, 85.91730236827989131, 84.58687643171798243 ) ) ;
#7983 = ORIENTED_EDGE ( 'NONE', *, *, #21537, .T. ) ;
#7984 = CARTESIAN_POINT ( 'NONE',  ( 128.0882145863933772, 39.20607399008170546, 5.346544642291981120 ) ) ;
#7985 = LINE ( 'NONE', #19220, #15675 ) ;
#7986 = CARTESIAN_POINT ( 'NONE',  ( 201.5987353083856135, 103.8544727311227547, 3.019891354123939831 ) ) ;
#7987 = CARTESIAN_POINT ( 'NONE',  ( 160.4971326318155604, 61.33565791516289778, 83.72971345548070587 ) ) ;
#7988 = EDGE_LOOP ( 'NONE', ( #45962, #24395 ) ) ;
#7989 = CARTESIAN_POINT ( 'NONE',  ( -36.11269837220812207, -31.11269837220801193, 85.00100000000000477 ) ) ;
#7990 = DIRECTION ( 'NONE',  ( 1.000000000000000000, 0.000000000000000000, 0.000000000000000000 ) ) ;
#7991 = DIRECTION ( 'NONE',  ( -0.000000000000000000, 0.000000000000000000, -1.000000000000000000 ) ) ;
#7992 = CARTESIAN_POINT ( 'NONE',  ( -102.2801239173131194, -170.0000000000000000, 57.36362509687880618 ) ) ;
#7993 = CARTESIAN_POINT ( 'NONE',  ( 82.74007713545067588, 18.13042311233562742, 3.950172779682598723 ) ) ;
#7995 = EDGE_LOOP ( 'NONE', ( #44128, #15177, #1749, #23395, #45298, #66615, #7298, #16890, #21287 ) ) ;
#7994 = LINE ( 'NONE', #67442, #11765 ) ;
#7996 = EDGE_CURVE ( 'NONE', #57426, #65931, #13813, .T. ) ;
#7997 = LINE ( 'NONE', #14657, #63208 ) ;
#7998 = VERTEX_POINT ( 'NONE', #41585 ) ;
#7999 = ORIENTED_EDGE ( 'NONE', *, *, #11286, .F. ) ;
#8000 = CARTESIAN_POINT ( 'NONE',  ( -168.1839487819771080, 83.25723186408066567, 17.12777191623586859 ) ) ;
#8001 = LINE ( 'NONE', #29456, #37178 ) ;
#8003 = VERTEX_POINT ( 'NONE', #30347 ) ;
#8002 = CYLINDRICAL_SURFACE ( 'NONE', #10702, 7.500000000000013323 ) ;
#8004 = CARTESIAN_POINT ( 'NONE',  ( -94.77617431038508755, 30.23990705277885382, 91.48307754187669616 ) ) ;
#8005 = CIRCLE ( 'NONE', #25993, 246.3582898394606957 ) ;
#8006 = CARTESIAN_POINT ( 'NONE',  ( -25.79929641484369185, 9.749255553662436569, 32.74771463646250425 ) ) ;
#8007 = FACE_BOUND ( 'NONE', #31326, .T. ) ;
#8008 = ORIENTED_EDGE ( 'NONE', *, *, #15902, .T. ) ;
#8009 = CIRCLE ( 'NONE', #47305, 24.99999999999985434 ) ;
#8010 = CARTESIAN_POINT ( 'NONE',  ( 212.1978255065450583, 119.0880569674902603, -70.32159165902619691 ) ) ;
#8011 = EDGE_CURVE ( 'NONE', #4848, #60490, #46866, .T. ) ;
#8012 = CIRCLE ( 'NONE', #30506, 20.00000000000000000 ) ;
#8013 = STYLED_ITEM ( 'NONE', ( #62553 ), #17204 ) ;
#8014 = CARTESIAN_POINT ( 'NONE',  ( 140.4769819293527462, 46.76840769395177944, 33.47658864813747925 ) ) ;
#8015 = CARTESIAN_POINT ( 'NONE',  ( 116.0963032583227772, 32.80867113471310148, 32.39564500324919294 ) ) ;
#8016 = CARTESIAN_POINT ( 'NONE',  ( -132.5976199670998881, 52.30296609017644727, 7.902498531389648306 ) ) ;
#8017 = CARTESIAN_POINT ( 'NONE',  ( 67.93154431625914924, 14.90489441944787785, -75.75106977084269033 ) ) ;
#8018 = VERTEX_POINT ( 'NONE', #51800 ) ;
#8019 = VERTEX_POINT ( 'NONE', #68332 ) ;
#8020 = ORIENTED_EDGE ( 'NONE', *, *, #29314, .F. ) ;
#8021 = EDGE_CURVE ( 'NONE', #64121, #47461, #45830, .T. ) ;
#8022 = DIRECTION ( 'NONE',  ( -0.000000000000000000, -0.000000000000000000, -1.000000000000000000 ) ) ;
#8023 = SURFACE_STYLE_FILL_AREA ( #55511 ) ;
#8024 = CARTESIAN_POINT ( 'NONE',  ( 36.30976089643145599, -12.29214613588890437, 13.32819299319724315 ) ) ;
#8025 = CARTESIAN_POINT ( 'NONE',  ( -34.29440389294403246, 17.09499999999999886, 4.000000000000000000 ) ) ;
#8026 = CARTESIAN_POINT ( 'NONE',  ( 74.62299871641495486, 5.461138973199058277, 170.0000000000000000 ) ) ;
#8027 = CARTESIAN_POINT ( 'NONE',  ( -133.1093894320205209, 51.43221067881453479, 62.84771461874985476 ) ) ;
#8028 = CARTESIAN_POINT ( 'NONE',  ( -73.10086105983762650, 21.34631349770504016, -10.71955127705281896 ) ) ;
#8029 = ORIENTED_EDGE ( 'NONE', *, *, #37873, .F. ) ;
#8030 = DIRECTION ( 'NONE',  ( -0.000000000000000000, 1.000000000000000000, -0.000000000000000000 ) ) ;
#8031 = ORIENTED_EDGE ( 'NONE', *, *, #32572, .T. ) ;
#8032 = CARTESIAN_POINT ( 'NONE',  ( 37.70762885381311946, 8.195134395012281914, 44.72399686281225684 ) ) ;
#8033 = DIRECTION ( 'NONE',  ( 0.000000000000000000, 0.000000000000000000, 1.000000000000000000 ) ) ;
#8034 = VERTEX_POINT ( 'NONE', #20468 ) ;
#8035 = CARTESIAN_POINT ( 'NONE',  ( 182.7789203043889756, 80.33475476315290109, 44.12694607665732605 ) ) ;
#8036 = EDGE_CURVE ( 'NONE', #41448, #36497, #2923, .T. ) ;
#8037 = LINE ( 'NONE', #40391, #6272 ) ;
#8038 =( LENGTH_UNIT ( ) NAMED_UNIT ( * ) SI_UNIT ( .MILLI., .METRE. ) );
#8039 = DIRECTION ( 'NONE',  ( -0.000000000000000000, -0.000000000000000000, 1.000000000000000000 ) ) ;
#8040 = CARTESIAN_POINT ( 'NONE',  ( -5.000000000000000888, 6.123233995736767268E-16, -25.03750572909317285 ) ) ;
#8041 = EDGE_CURVE ( 'NONE', #52276, #25055, #57623, .T. ) ;
#8042 = CARTESIAN_POINT ( 'NONE',  ( 157.4703587214989113, 57.65129005721576760, -51.12418429913766005 ) ) ;
#8043 = ORIENTED_EDGE ( 'NONE', *, *, #46385, .T. ) ;
#8044 = DIRECTION ( 'NONE',  ( -0.000000000000000000, -0.000000000000000000, -1.000000000000000000 ) ) ;
#8045 = CARTESIAN_POINT ( 'NONE',  ( -154.6171773099879658, 68.63761944777706958, -9.973008346805338320 ) ) ;
#8046 = EDGE_LOOP ( 'NONE', ( #68631, #28224, #7212, #49726 ) ) ;
#8047 = DIRECTION ( 'NONE',  ( 0.000000000000000000, 1.000000000000000000, 0.000000000000000000 ) ) ;
#8048 = CARTESIAN_POINT ( 'NONE',  ( -55.05276343752909440, 15.72344139423348430, 57.16187836339483397 ) ) ;
#8049 = CYLINDRICAL_SURFACE ( 'NONE', #49921, 7.500000000000020428 ) ;
#8050 = VERTEX_POINT ( 'NONE', #9236 ) ;
#8051 = LINE ( 'NONE', #44987, #53562 ) ;
#8052 = CARTESIAN_POINT ( 'NONE',  ( 39.40195752203891999, 9.424259417798145577, 18.06928371549960133 ) ) ;
#8053 = CARTESIAN_POINT ( 'NONE',  ( -35.99019277275120743, 10.38248800679342132, 43.69771462296589704 ) ) ;
#8054 = CARTESIAN_POINT ( 'NONE',  ( 139.1353280997809634, 44.70436000187871173, -38.18995759472777252 ) ) ;
#8055 =( REPRESENTATION_RELATIONSHIP ('NONE','NONE', #40274, #46031 ) REPRESENTATION_RELATIONSHIP_WITH_TRANSFORMATION ( #21177 )SHAPE_REPRESENTATION_RELATIONSHIP( ) );
#8056 = ORIENTED_EDGE ( 'NONE', *, *, #22313, .F. ) ;
#8057 = CARTESIAN_POINT ( 'NONE',  ( -150.3831389294225858, 66.25266777263978213, 57.61345155406902308 ) ) ;
#8058 = DIRECTION ( 'NONE',  ( 0.000000000000000000, 0.000000000000000000, 1.000000000000000000 ) ) ;
#8059 = ORIENTED_EDGE ( 'NONE', *, *, #60836, .F. ) ;
#8060 = FACE_OUTER_BOUND ( 'NONE', #47092, .T. ) ;
#8061 = CARTESIAN_POINT ( 'NONE',  ( 182.7789203043889756, 80.33475476315292951, 17.28239548619366062 ) ) ;
#8062 = VECTOR ( 'NONE', #5399, 1000.000000000000000 ) ;
#8063 = CARTESIAN_POINT ( 'NONE',  ( 87.58098510096635891, 19.74745174099416545, 56.60179672011121710 ) ) ;
#8064 = PRODUCT ( 'frame_Default<As Welded>', 'frame_Default<As Welded>', '', ( #42401 ) ) ;
#8065 = DIRECTION ( 'NONE',  ( 1.000000000000000000, 0.000000000000000000, 0.000000000000000000 ) ) ;
#8066 = CIRCLE ( 'NONE', #51896, 65.36598343705435354 ) ;
#8068 = AXIS2_PLACEMENT_3D ( 'NONE', #25370, #68274, #68936 ) ;
#8067 = DIRECTION ( 'NONE',  ( -0.000000000000000000, 0.000000000000000000, 1.000000000000000000 ) ) ;
#8069 = LINE ( 'NONE', #52019, #34673 ) ;
#8070 = ORIENTED_EDGE ( 'NONE', *, *, #18337, .F. ) ;
#8071 = CARTESIAN_POINT ( 'NONE',  ( -149.5074843970971017, 65.50121172469319220, 30.72082123989904545 ) ) ;
#8072 = CARTESIAN_POINT ( 'NONE',  ( -34.29440389294403246, -17.09499999999999886, 4.000000000000000000 ) ) ;
#8073 = CARTESIAN_POINT ( 'NONE',  ( 70.46452034227868921, 14.52462608639673292, 63.15238888589277622 ) ) ;
#8074 = CARTESIAN_POINT ( 'NONE',  ( 139.1306635769909690, 45.89653412152166823, 4.827772763954556901 ) ) ;
#8075 = LINE ( 'NONE', #9466, #16183 ) ;
#8076 = CLOSED_SHELL ( 'NONE', ( #37480, #10315, #4132, #35670, #17211, #17781, #51490, #4050, #57996, #4458, #3784, #15788, #54123, #26352, #31839, #51393, #39881, #55191, #16444 ) ) ;
#8077 = ORIENTED_EDGE ( 'NONE', *, *, #28923, .T. ) ;
#8078 = EDGE_CURVE ( 'NONE', #41137, #60705, #62355, .T. ) ;
#8079 = CARTESIAN_POINT ( 'NONE',  ( 163.1370549780984049, 63.50181104276887822, -21.71851364603849532 ) ) ;
#8080 = CARTESIAN_POINT ( 'NONE',  ( 8.336031647119270360, 6.376437040857335425, 38.49332896737825394 ) ) ;
#8081 = ORIENTED_EDGE ( 'NONE', *, *, #9301, .F. ) ;
#8082 = EDGE_CURVE ( 'NONE', #34211, #69123, #37682, .T. ) ;
#8083 = CARTESIAN_POINT ( 'NONE',  ( 65.40383840050411379, 14.27443447873227278, 57.03128338250952112 ) ) ;
#8084 = CARTESIAN_POINT ( 'NONE',  ( 126.3606262338561379, 37.07877897843705028, 90.26304925273296931 ) ) ;
#8085 = EDGE_LOOP ( 'NONE', ( #35440, #41087, #18841, #5790 ) ) ;
#8086 = CARTESIAN_POINT ( 'NONE',  ( -146.5268141329886760, 61.69196909035589726, -62.27134214804291901 ) ) ;
#8087 = LINE ( 'NONE', #52633, #52708 ) ;
#8088 = LINE ( 'NONE', #14058, #18215 ) ;
#8089 = CARTESIAN_POINT ( 'NONE',  ( 175.0857681883884140, -170.0000000000000000, 94.99999999999866418 ) ) ;
#8090 = ORIENTED_EDGE ( 'NONE', *, *, #46995, .F. ) ;
#8091 = CARTESIAN_POINT ( 'NONE',  ( -96.77705718164448001, 31.18700926299571563, 16.29415678444673787 ) ) ;
#8092 = EDGE_CURVE ( 'NONE', #16646, #35238, #29964, .T. ) ;
#8093 = EDGE_CURVE ( 'NONE', #30336, #59608, #10600, .T. ) ;
#8094 = CARTESIAN_POINT ( 'NONE',  ( 58.70125406583569827, 12.74196547173361616, 84.85832636372359161 ) ) ;
#8095 = DIRECTION ( 'NONE',  ( -3.081487911019579554E-32, -1.000000000000000000, -3.469446951953612956E-17 ) ) ;
#8096 = CARTESIAN_POINT ( 'NONE',  ( 85.68197636629476222, 20.16141071296263121, -23.93233960346654143 ) ) ;
#8097 = CARTESIAN_POINT ( 'NONE',  ( -171.4867114763004849, 85.32693843184998173, 30.99019746422447241 ) ) ;
#8098 = CARTESIAN_POINT ( 'NONE',  ( -142.0747101610765242, 58.12276061064464017, -95.00000000000133582 ) ) ;
#8099 = CARTESIAN_POINT ( 'NONE',  ( 127.1040286383415321, 37.49395136275127527, -73.64177352694797207 ) ) ;
#8101 = ORIENTED_EDGE ( 'NONE', *, *, #24848, .F. ) ;
#8100 = ADVANCED_FACE ( 'NONE', ( #15550 ), #58440, .F. ) ;
#8102 = LINE ( 'NONE', #3183, #60118 ) ;
#8103 = CARTESIAN_POINT ( 'NONE',  ( -15.27733754929849752, 8.502213909106947298, 65.43888028898012976 ) ) ;
#8104 = ORIENTED_EDGE ( 'NONE', *, *, #5325, .F. ) ;
#8105 = CIRCLE ( 'NONE', #49656, 0.3000000000000051514 ) ;
#8106 = EDGE_CURVE ( 'NONE', #22374, #22712, #21502, .T. ) ;
#8107 = CARTESIAN_POINT ( 'NONE',  ( -156.0209085498131856, 71.27066046086520146, -46.06989554857462110 ) ) ;
#8108 = CARTESIAN_POINT ( 'NONE',  ( 0.000000000000000000, 0.000000000000000000, 2.000000000000001776 ) ) ;
#8109 = CARTESIAN_POINT ( 'NONE',  ( -33.12994257348896809, 10.89587983539684934, 30.40543924679923293 ) ) ;
#8110 = VECTOR ( 'NONE', #48451, 1000.000000000000000 ) ;
#8111 = CARTESIAN_POINT ( 'NONE',  ( -2.873329055852806402, 7.626065826870668474, 31.96118308163061528 ) ) ;
#8112 = PLANE ( 'NONE',  #2250 ) ;
#8113 = CARTESIAN_POINT ( 'NONE',  ( -53.14475157111026249, 14.17819596930906734, -76.81816462347461538 ) ) ;
#8114 = CARTESIAN_POINT ( 'NONE',  ( -0.8863172752569271617, 7.545240277686256825, -13.19636946549736045 ) ) ;
#8116 = CARTESIAN_POINT ( 'NONE',  ( 174.1251613516844543, 71.84747073139210727, 12.81514609272755045 ) ) ;
#8115 = VECTOR ( 'NONE', #52378, 1000.000000000000000 ) ;
#8117 = AXIS2_PLACEMENT_3D ( 'NONE', #8779, #24950, #35146 ) ;
#8118 = CARTESIAN_POINT ( 'NONE',  ( 110.2429982417149432, 28.88204397445229432, 17.76666361527367499 ) ) ;
#8119 = ORIENTED_EDGE ( 'NONE', *, *, #45679, .F. ) ;
#8120 = CARTESIAN_POINT ( 'NONE',  ( -94.77890319529974761, 30.24118571794804566, -43.01465426540235626 ) ) ;
#8121 = ORIENTED_EDGE ( 'NONE', *, *, #56214, .F. ) ;
#8122 = CARTESIAN_POINT ( 'NONE',  ( 110.2429982417149290, 28.88204397445231209, -77.76698815611739235 ) ) ;
#8123 = ADVANCED_FACE ( 'NONE', ( #38034 ), #43337, .T. ) ;
#8124 = CARTESIAN_POINT ( 'NONE',  ( 200.0000000000000000, 0.000000000000000000, -10.00000000000000000 ) ) ;
#8125 = CARTESIAN_POINT ( 'NONE',  ( 41.09671232177016265, 8.635892912882342287, 56.94825200755940386 ) ) ;
#8126 = DIRECTION ( 'NONE',  ( -0.000000000000000000, 0.000000000000000000, -1.000000000000000000 ) ) ;
#8127 = CARTESIAN_POINT ( 'NONE',  ( -15.32317988097521066, 7.495800589904738409, 90.93220421695207278 ) ) ;
#8128 = VECTOR ( 'NONE', #59536, 1000.000000000000000 ) ;
#8129 = EDGE_CURVE ( 'NONE', #15646, #4543, #15755, .T. ) ;
#8130 = EDGE_CURVE ( 'NONE', #18081, #10959, #45047, .T. ) ;
#8131 = ADVANCED_FACE ( 'NONE', ( #55605 ), #2156, .F. ) ;
#8132 = CARTESIAN_POINT ( 'NONE',  ( 0.1306530452038078272, 5.952467836904149934, -5.690023276062396107 ) ) ;
#8133 = LINE ( 'NONE', #18689, #26336 ) ;
#8134 = CARTESIAN_POINT ( 'NONE',  ( 0.000000000000000000, -36.09918303830819752, 30.00000000000000000 ) ) ;
#8135 = EDGE_LOOP ( 'NONE', ( #60055, #64218, #25337, #33874 ) ) ;
#8136 = ORIENTED_EDGE ( 'NONE', *, *, #40268, .T. ) ;
#8137 = FACE_BOUND ( 'NONE', #65978, .T. ) ;
#8138 = LINE ( 'NONE', #29581, #17587 ) ;
#8139 = CARTESIAN_POINT ( 'NONE',  ( 41.44400078756287797, 8.683588207969460626, -89.58023771676421632 ) ) ;
#8140 = FACE_OUTER_BOUND ( 'NONE', #18034, .T. ) ;
#8141 = CARTESIAN_POINT ( 'NONE',  ( -27.00000000000000355, -30.00000000000000355, 15.00000000000000000 ) ) ;
#8142 = CARTESIAN_POINT ( 'NONE',  ( 62.52762183777210936, 13.59210632617625691, -8.876140241706057310 ) ) ;
#8143 = ORIENTED_EDGE ( 'NONE', *, *, #37114, .F. ) ;
#8144 = CARTESIAN_POINT ( 'NONE',  ( 108.3753929817421522, 29.13179266688723956, -36.14330376477542472 ) ) ;
#8145 = CARTESIAN_POINT ( 'NONE',  ( -9.771516655894554759, 7.025139475821123192, 57.20049567545273561 ) ) ;
#8146 = CARTESIAN_POINT ( 'NONE',  ( -83.52505811737952968, 24.23179517241435121, -21.50563568346970200 ) ) ;
#8147 = CARTESIAN_POINT ( 'NONE',  ( 0.000000000000000000, 0.000000000000000000, 0.000000000000000000 ) ) ;
#8148 = CARTESIAN_POINT ( 'NONE',  ( 13.72076016085272165, 6.443109411582633506, -89.48629928841640435 ) ) ;
#8149 = ORIENTED_EDGE ( 'NONE', *, *, #27974, .T. ) ;
#8150 = ORIENTED_EDGE ( 'NONE', *, *, #52893, .F. ) ;
#8151 = LINE ( 'NONE', #45787, #52516 ) ;
#8152 = LINE ( 'NONE', #7813, #47351 ) ;
#8153 = AXIS2_PLACEMENT_3D ( 'NONE', #28579, #50389, #35242 ) ;
#8154 = DIRECTION ( 'NONE',  ( -0.000000000000000000, -0.000000000000000000, -1.000000000000000000 ) ) ;
#8155 = CARTESIAN_POINT ( 'NONE',  ( -13.24252603915519444, -63.63674649211960599, 170.0000000000000000 ) ) ;
#8156 = CARTESIAN_POINT ( 'NONE',  ( 63.98009977735162579, 12.89803120691696137, 29.85932659275067280 ) ) ;
#8157 = B_SPLINE_CURVE_WITH_KNOTS ( 'NONE', 3,
 ( #1101, #60879, #17983, #44349, #23264, #23609, #34521, #33809, #22552, #66531, #54548, #17628, #27829, #39777, #43995, #18321, #12702, #65474, #6375, #61238, #28886, #38739, #60183, #7776, #34167, #12002, #49618, #44712, #33476, #54898, #7435, #29228, #6722, #66190, #7072, #28167, #1449, #28530, #39427, #55964, #16918, #50338, #50674, #38381, #2497 ),
 .UNSPECIFIED., .F., .F.,
 ( 4, 2, 2, 1, 2, 2, 2, 2, 2, 2, 2, 2, 2, 2, 2, 2, 2, 2, 2, 2, 2, 2, 4 ),
 ( 0.02346464386237015476, 0.02493212228186625704, 0.02566586149161431338, 0.02639960070136236625, 0.02713333991111042259, 0.02786707912085847547, 0.02933455754035457080, 0.03006829675010262715, 0.03080203595985068349, 0.03226951437934681005, 0.03300325358909486639, 0.03373699279884292274, 0.03520447121833903542, 0.03667194963783514117, 0.03740568884758319751, 0.03813942805733125385, 0.03960690647682735960, 0.04107438489632346534, 0.04254186331581957803, 0.04327560252556764131, 0.04400934173531570459, 0.04547682015481182422, 0.04694429857430795078 ),
 .UNSPECIFIED. ) ;
#8158 = CARTESIAN_POINT ( 'NONE',  ( 47.91750333461326505, 19.31887485910233693, 26.66469066592268788 ) ) ;
#8159 = AXIS2_PLACEMENT_3D ( 'NONE', #1440, #2488, #55239 ) ;
#8160 = ORIENTED_EDGE ( 'NONE', *, *, #47994, .F. ) ;
#8161 = DIRECTION ( 'NONE',  ( -0.000000000000000000, -0.000000000000000000, -1.000000000000000000 ) ) ;
#8162 = CARTESIAN_POINT ( 'NONE',  ( 60.58000000000000540, -26.09918303830819397, 10.41169613715280740 ) ) ;
#8163 = VERTEX_POINT ( 'NONE', #1810 ) ;
#8164 = AXIS2_PLACEMENT_3D ( 'NONE', #38494, #11061, #514 ) ;
#8165 = LINE ( 'NONE', #51079, #17116 ) ;
#8166 = VERTEX_POINT ( 'NONE', #17265 ) ;
#8167 = EDGE_CURVE ( 'NONE', #60768, #21955, #8157, .T. ) ;
#8168 = CARTESIAN_POINT ( 'NONE',  ( -81.23297981660239486, 23.31577157498399444, -62.40870875688570862 ) ) ;
#8169 = CARTESIAN_POINT ( 'NONE',  ( -62.15063206372445848, 17.75106610013994413, -18.34472482884989120 ) ) ;
#8170 = CARTESIAN_POINT ( 'NONE',  ( 94.06416612695404922, 23.16920323269610549, -69.14766088501639274 ) ) ;
#8171 = VERTEX_POINT ( 'NONE', #23949 ) ;
#8172 = B_SPLINE_CURVE_WITH_KNOTS ( 'NONE', 3,
 ( #31564, #53000, #68507, #35815, #52663, #4824 ),
 .UNSPECIFIED., .F., .F.,
 ( 4, 2, 4 ),
 ( 1.095770181108053550E-06, 0.03239442681617710901, 0.06478775786217311206 ),
 .UNSPECIFIED. ) ;
#8173 = VECTOR ( 'NONE', #19175, 999.9999999999998863 ) ;
#8174 = EDGE_LOOP ( 'NONE', ( #10388, #33885, #65037, #5269 ) ) ;
#8175 = CARTESIAN_POINT ( 'NONE',  ( 13.84937401517046673, 6.446378549072246500, -35.76972009710845413 ) ) ;
#8176 = CARTESIAN_POINT ( 'NONE',  ( -107.6612349940556328, 36.74343276704001937, -90.96034172286037744 ) ) ;
#8177 = DIRECTION ( 'NONE',  ( -0.000000000000000000, -0.000000000000000000, 1.000000000000000000 ) ) ;
#8178 = EDGE_LOOP ( 'NONE', ( #4658, #42551 ) ) ;
#8179 = EDGE_CURVE ( 'NONE', #5941, #36461, #45398, .T. ) ;
#8180 = ADVANCED_FACE ( 'NONE', ( #14087 ), #35546, .F. ) ;
#8181 = EDGE_CURVE ( 'NONE', #22856, #15204, #57002, .T. ) ;
#8182 = CARTESIAN_POINT ( 'NONE',  ( -31.11269837220801193, 36.11269837220812207, 2.000000000000001776 ) ) ;
#8183 = CARTESIAN_POINT ( 'NONE',  ( 3.000000000000028866, 3.000000000000030198, 0.000000000000000000 ) ) ;
#8184 = CARTESIAN_POINT ( 'NONE',  ( -102.2801239173131194, 32.78103895658057354, 18.67452391595144334 ) ) ;
#8185 = CARTESIAN_POINT ( 'NONE',  ( 0.000000000000000000, 0.000000000000000000, 0.000000000000000000 ) ) ;
#8186 = ADVANCED_FACE ( 'NONE', ( #30616 ), #62628, .F. ) ;
#8187 = CARTESIAN_POINT ( 'NONE',  ( 79.19119222799088220, 18.06817527909835164, -42.32747752434355704 ) ) ;
#8189 = EDGE_LOOP ( 'NONE', ( #19372, #48459, #58598, #25923 ) ) ;
#8188 = CARTESIAN_POINT ( 'NONE',  ( -167.3106824190689110, 82.33819578244379045, -91.13552483532193094 ) ) ;
#8190 = ORIENTED_EDGE ( 'NONE', *, *, #56333, .F. ) ;
#8191 = EDGE_CURVE ( 'NONE', #48198, #41404, #48356, .T. ) ;
#8192 = VERTEX_POINT ( 'NONE', #4227 ) ;
#8193 = CARTESIAN_POINT ( 'NONE',  ( 46.65037935242575884, 9.463293687292228640, 12.51126093126612027 ) ) ;
#8194 = CARTESIAN_POINT ( 'NONE',  ( -31.43908319763710679, -170.0000000000000000, -89.00629854612920155 ) ) ;
#8195 = LINE ( 'NONE', #13473, #43487 ) ;
#8196 = CARTESIAN_POINT ( 'NONE',  ( 102.8111940033034415, 25.59308899183601937, -15.53619449273017494 ) ) ;
#8197 = CARTESIAN_POINT ( 'NONE',  ( 197.9847015768255574, 97.56951352050457160, 13.21957474342690553 ) ) ;
#8198 = CARTESIAN_POINT ( 'NONE',  ( -29.75098818128877198, 9.320063824353118420, -89.18649209667817956 ) ) ;
#8199 = CARTESIAN_POINT ( 'NONE',  ( 210.5761663949224101, 116.5895149528252404, 85.72674437253323276 ) ) ;
#8200 = CARTESIAN_POINT ( 'NONE',  ( 212.1978255065450583, 119.0880569674902461, 37.05661070282843639 ) ) ;
#8201 = CARTESIAN_POINT ( 'NONE',  ( -83.69370847062542396, 25.38703975185373807, 59.19179572676554102 ) ) ;
#8202 = CARTESIAN_POINT ( 'NONE',  ( -12.39701069459753846, 7.231688578592714300, 31.64994337550934489 ) ) ;
#8203 = ORIENTED_EDGE ( 'NONE', *, *, #37152, .T. ) ;
#8204 = VECTOR ( 'NONE', #24155, 1000.000000000000000 ) ;
#8205 = DIRECTION ( 'NONE',  ( 1.000000000000000000, 0.000000000000000000, 0.000000000000000000 ) ) ;
#8206 = ORIENTED_EDGE ( 'NONE', *, *, #23233, .F. ) ;
#8207 = VERTEX_POINT ( 'NONE', #25694 ) ;
#8208 = CARTESIAN_POINT ( 'NONE',  ( -143.2498117110515352, 60.33382252735061257, 7.233766551320602645 ) ) ;
#8209 = AXIS2_PLACEMENT_3D ( 'NONE', #61244, #56654, #3531 ) ;
#8210 = CARTESIAN_POINT ( 'NONE',  ( 259.4165763529819060, -27.00000000000000355, 108.9999999999999858 ) ) ;
#8211 = CARTESIAN_POINT ( 'NONE',  ( -168.0052514572427071, 83.06849406765624622, 43.81149462059376276 ) ) ;
#8212 = CARTESIAN_POINT ( 'NONE',  ( -95.04120270830171080, 29.25306318840326725, -40.48597676605763951 ) ) ;
#8213 = ADVANCED_FACE ( 'NONE', ( #40129 ), #61586, .F. ) ;
#8214 = CARTESIAN_POINT ( 'NONE',  ( -23.95089599695170079, 9.496585844566176604, 10.38338860445121625 ) ) ;
#8215 = VECTOR ( 'NONE', #13644, 1000.000000000000000 ) ;
#8216 = CARTESIAN_POINT ( 'NONE',  ( 4.250000000000000000, 0.000000000000000000, -8.949444346342716017 ) ) ;
#8217 = FACE_OUTER_BOUND ( 'NONE', #67323, .T. ) ;
#8218 = ADVANCED_FACE ( 'NONE', ( #36924 ), #53075, .F. ) ;
#8219 = CARTESIAN_POINT ( 'NONE',  ( 128.3856248084844651, 38.21741401878866640, -48.67688400636009760 ) ) ;
#8220 = EDGE_LOOP ( 'NONE', ( #22699, #19585, #50468, #64923 ) ) ;
#8221 = ORIENTED_EDGE ( 'NONE', *, *, #53653, .T. ) ;
#8222 = CIRCLE ( 'NONE', #47503, 5.000000000000004441 ) ;
#8223 = CARTESIAN_POINT ( 'NONE',  ( 188.4752958934330707, 87.91563303859531686, 91.78575244328496296 ) ) ;
#8224 = DIRECTION ( 'NONE',  ( -0.000000000000000000, -0.000000000000000000, -1.000000000000000000 ) ) ;
#8225 = CARTESIAN_POINT ( 'NONE',  ( 70.34686579112810989, 18.11777090454213379, 43.58025477438756923 ) ) ;
#8226 = AXIS2_PLACEMENT_3D ( 'NONE', #27507, #21882, #63776 ) ;
#8227 = CARTESIAN_POINT ( 'NONE',  ( -24.70354720400821691, 8.582324684301861240, -66.32597363807256841 ) ) ;
#8228 = FACE_OUTER_BOUND ( 'NONE', #21228, .T. ) ;
#8229 = ORIENTED_EDGE ( 'NONE', *, *, #37636, .F. ) ;
#8230 = LINE ( 'NONE', #51495, #27766 ) ;
#8231 = CARTESIAN_POINT ( 'NONE',  ( -62.55320287144887459, 17.87319849854531029, -69.32330422822633409 ) ) ;
#8232 = CARTESIAN_POINT ( 'NONE',  ( 198.2581645178919132, 99.52881771501682806, -66.81519542867474115 ) ) ;
#8233 = SHAPE_REPRESENTATION_RELATIONSHIP ( 'NONE' , 'NONE' ,  #60409, #3860 ) ;
#8234 = CYLINDRICAL_SURFACE ( 'NONE', #53074, 2.999999999999999112 ) ;
#8235 = FACE_OUTER_BOUND ( 'NONE', #56113, .T. ) ;
#8236 = CARTESIAN_POINT ( 'NONE',  ( -24.32776401346968598, 9.546905915310563984, 66.99408005789631204 ) ) ;
#8237 = CARTESIAN_POINT ( 'NONE',  ( -15.55634918610396866, 36.11269837220808654, 0.000000000000000000 ) ) ;
#8238 = CARTESIAN_POINT ( 'NONE',  ( -54.09522495088362604, 14.42642983673692036, 57.20752439395842259 ) ) ;
#8239 = CARTESIAN_POINT ( 'NONE',  ( -101.8637373947396014, 32.56989439519480101, -88.71231002810291955 ) ) ;
#8240 = ORIENTED_EDGE ( 'NONE', *, *, #46920, .T. ) ;
#8241 = DIRECTION ( 'NONE',  ( 0.8584487936018655452, 0.5128992774059070170, -0.000000000000000000 ) ) ;
#8242 = CARTESIAN_POINT ( 'NONE',  ( -126.7989199172159545, 47.09198523267863834, -76.71749280709809682 ) ) ;
#8243 = DIRECTION ( 'NONE',  ( 0.000000000000000000, 0.000000000000000000, -1.000000000000000000 ) ) ;
#8244 = CARTESIAN_POINT ( 'NONE',  ( -78.66644367742109978, 23.39876645725290061, -35.11545063171788428 ) ) ;
#8245 = CYLINDRICAL_SURFACE ( 'NONE', #31109, 7.500000000000013323 ) ;
#8246 = ORIENTED_EDGE ( 'NONE', *, *, #39070, .F. ) ;
#8247 = CARTESIAN_POINT ( 'NONE',  ( 204.6977192012829789, -170.0000000000000000, 36.70772073876943153 ) ) ;
#8248 = EDGE_CURVE ( 'NONE', #26499, #65633, #22009, .T. ) ;
#8249 = DIRECTION ( 'NONE',  ( 1.000000000000000000, 1.001918046209079887E-14, -9.729495617646301779E-15 ) ) ;
#8250 = ORIENTED_EDGE ( 'NONE', *, *, #19133, .F. ) ;
#8251 = ORIENTED_EDGE ( 'NONE', *, *, #19759, .T. ) ;
#8252 = EDGE_CURVE ( 'NONE', #2052, #62563, #42200, .T. ) ;
#8253 =( GEOMETRIC_REPRESENTATION_CONTEXT ( 3 ) GLOBAL_UNCERTAINTY_ASSIGNED_CONTEXT ( ( #56404 ) ) GLOBAL_UNIT_ASSIGNED_CONTEXT ( ( #66641, #61689, #39207 ) ) REPRESENTATION_CONTEXT ( 'NONE', 'WORKASPACE' ) );
#8254 = DIRECTION ( 'NONE',  ( 0.000000000000000000, 0.000000000000000000, -1.000000000000000000 ) ) ;
#8255 = DIRECTION ( 'NONE',  ( 0.000000000000000000, -0.000000000000000000, -1.000000000000000000 ) ) ;
#8256 = CARTESIAN_POINT ( 'NONE',  ( -61.36325649057781817, -43.03793052543183251, 41.38025477438755928 ) ) ;
#8257 = VERTEX_POINT ( 'NONE', #31638 ) ;
#8258 = DIRECTION ( 'NONE',  ( 0.000000000000000000, 0.000000000000000000, -1.000000000000000000 ) ) ;
#8259 = CARTESIAN_POINT ( 'NONE',  ( -179.2262621278717916, 94.19039042964669761, 15.86246328341808365 ) ) ;
#8260 = DIRECTION ( 'NONE',  ( -0.000000000000000000, 1.000000000000000000, -0.000000000000000000 ) ) ;
#8261 = CIRCLE ( 'NONE', #62168, 245.3095347406802205 ) ;
#8262 = CARTESIAN_POINT ( 'NONE',  ( 57.39233401791016576, 12.46575990788837629, -38.23382626024586983 ) ) ;
#8263 = CARTESIAN_POINT ( 'NONE',  ( -83.69370847062540975, 25.38703975185372030, 32.34724513630185783 ) ) ;
#8264 = CARTESIAN_POINT ( 'NONE',  ( 151.2978913959096019, 53.00666906180277493, 86.32333572920605036 ) ) ;
#8265 = VECTOR ( 'NONE', #39964, 1000.000000000000000 ) ;
#8266 = CARTESIAN_POINT ( 'NONE',  ( 134.7697261969508986, 41.97802808873668567, 2.707623648563555196 ) ) ;
#8267 = VECTOR ( 'NONE', #63664, 1000.000000000000114 ) ;
#8268 = EDGE_CURVE ( 'NONE', #8643, #36732, #63662, .T. ) ;
#8269 = ORIENTED_EDGE ( 'NONE', *, *, #40967, .T. ) ;
#8270 = AXIS2_PLACEMENT_3D ( 'NONE', #36099, #30470, #9359 ) ;
#8271 = CARTESIAN_POINT ( 'NONE',  ( -4.164416015345870470, 64.86646004871185767, 40.00000000000003553 ) ) ;
#8272 = AXIS2_PLACEMENT_3D ( 'NONE', #43345, #20865, #32458 ) ;
#8273 = DIRECTION ( 'NONE',  ( 0.000000000000000000, 1.000000000000000000, 0.000000000000000000 ) ) ;
#8274 = EDGE_CURVE ( 'NONE', #38050, #8339, #26588, .T. ) ;
#8275 = CARTESIAN_POINT ( 'NONE',  ( -78.66644367742111399, -170.0000000000000000, -88.80455181264524356 ) ) ;
#8276 = ADVANCED_FACE ( 'NONE', ( #15470 ), #307, .F. ) ;
#8277 = FACE_OUTER_BOUND ( 'NONE', #19680, .T. ) ;
#8279 = EDGE_LOOP ( 'NONE', ( #41736, #58624, #62946, #38975 ) ) ;
#8278 = CARTESIAN_POINT ( 'NONE',  ( -118.6398180864478746, 41.89949912940330279, 93.74388258701110033 ) ) ;
#8280 = CARTESIAN_POINT ( 'NONE',  ( 86.62931800182293784, 20.48449268398422518, 2.867536982015617575 ) ) ;
#8281 = AXIS2_PLACEMENT_3D ( 'NONE', #36421, #55892, #57877 ) ;
#8282 = ORIENTED_EDGE ( 'NONE', *, *, #373, .T. ) ;
#8283 = B_SPLINE_CURVE_WITH_KNOTS ( 'NONE', 3,
 ( #47477, #21117, #6920, #52755, #47829, #69289 ),
 .UNSPECIFIED., .F., .F.,
 ( 4, 2, 4 ),
 ( 0.03218950539619248874, 0.06469844149454670457, 0.09720737759290090652 ),
 .UNSPECIFIED. ) ;
#8284 = PLANE ( 'NONE',  #64935 ) ;
#8285 = CARTESIAN_POINT ( 'NONE',  ( 85.68197636629477643, 20.16141071296262766, 29.75676157746082140 ) ) ;
#8286 = DIRECTION ( 'NONE',  ( -1.000000000000000000, 9.109522253334613014E-16, 1.697894969632810648E-16 ) ) ;
#8287 = LINE ( 'NONE', #61396, #33935 ) ;
#8288 = CARTESIAN_POINT ( 'NONE',  ( -122.3963566076408398, 44.23346594671848209, 58.31322267358287803 ) ) ;
#8289 = CARTESIAN_POINT ( 'NONE',  ( -85.73740570227380431, 26.23277384689411917, -18.28398584103688407 ) ) ;
#8290 = CARTESIAN_POINT ( 'NONE',  ( -173.9526029538035914, 89.57590038685107459, -22.83302484729744464 ) ) ;
#8291 = CARTESIAN_POINT ( 'NONE',  ( -65.20298343242136241, 4.613322252417249913, 43.58025477438756212 ) ) ;
#8292 = ORIENTED_EDGE ( 'NONE', *, *, #46363, .T. ) ;
#8293 = VERTEX_POINT ( 'NONE', #9850 ) ;
#8294 = CARTESIAN_POINT ( 'NONE',  ( -3.000000000000006217, 0.000000000000000000, 0.000000000000000000 ) ) ;
#8295 = CARTESIAN_POINT ( 'NONE',  ( 56.42997683260104225, 32.25922681454269991, 40.00000000000003553 ) ) ;
#8296 = CARTESIAN_POINT ( 'NONE',  ( 157.4703587214989113, 57.65129005721575339, 56.25401806271706562 ) ) ;
#8297 = CARTESIAN_POINT ( 'NONE',  ( -190.6985136298602015, 109.1272424661243434, 69.71826505393651985 ) ) ;
#8298 = CARTESIAN_POINT ( 'NONE',  ( 100.0000000000000284, -5.000000000000000000, 19.36491673103708777 ) ) ;
#8299 = CARTESIAN_POINT ( 'NONE',  ( 3.000000000000002665, 0.000000000000000000, 0.000000000000000000 ) ) ;
#8300 = EDGE_CURVE ( 'NONE', #28657, #37048, #49241, .T. ) ;
#8301 = CARTESIAN_POINT ( 'NONE',  ( -142.0376140313400413, 59.37288070770861736, 92.66934662550120549 ) ) ;
#8302 = EDGE_LOOP ( 'NONE', ( #16523, #9461, #42713, #42175 ) ) ;
#8303 = ORIENTED_EDGE ( 'NONE', *, *, #10070, .T. ) ;
#8304 = VERTEX_POINT ( 'NONE', #47122 ) ;
#8305 = LINE ( 'NONE', #20836, #15087 ) ;
#8306 = CIRCLE ( 'NONE', #16167, 22.00000000000000355 ) ;
#8307 = FACE_OUTER_BOUND ( 'NONE', #58252, .T. ) ;
#8308 = CARTESIAN_POINT ( 'NONE',  ( -46.66904755831210139, 5.000000000000066613, 85.00100000000000477 ) ) ;
#8309 = CARTESIAN_POINT ( 'NONE',  ( 65.62848231372477414, 13.29388722724785232, -50.25499563657418634 ) ) ;
#8310 = CARTESIAN_POINT ( 'NONE',  ( 48.91942932610495376, 19.16407787157945108, 38.91942932610497508 ) ) ;
#8311 = B_SPLINE_CURVE_WITH_KNOTS ( 'NONE', 3,
 ( #58401, #32032, #41892, #10215, #62666, #31681, #53116, #4949, #52449, #30652, #4266, #15846, #14474, #57731, #9542, #31344, #26411, #21139, #47847, #20095, #35929, #41207, #69313, #15162, #42581, #52103, #64037, #52772, #4599, #14805, #3917, #25390, #37291, #46823, #58741, #26753, #68290, #41549, #65790, #5972, #59782, #16190, #32379, #27788, #22860, #11593 ),
 .UNSPECIFIED., .F., .F.,
 ( 4, 2, 2, 2, 2, 2, 2, 2, 2, 2, 2, 2, 2, 2, 2, 2, 2, 2, 2, 2, 2, 2, 4 ),
 ( 0.02989107162308295151, 0.03170280136394039439, 0.03351453110479783726, 0.03532626084565527319, 0.03713799058651271606, 0.03894972032737015893, 0.03985558519779885955, 0.04076145006822755323, 0.04166731493865626079, 0.04257317980908495447, 0.04347904467951365509, 0.04438490954994235571, 0.04529077442037104245, 0.04619663929079972919, 0.04710250416122842287, 0.04800836903165710268, 0.04891423390208579636, 0.04982009877251449004, 0.05163182851337179413, 0.05344355825422911210, 0.05525528799508642314, 0.05706701773594373417, 0.05887874747680104520 ),
 .UNSPECIFIED. ) ;
#8312 = CARTESIAN_POINT ( 'NONE',  ( -59.57462349605616225, 16.98779896904798292, 31.81369624524355544 ) ) ;
#8313 = AXIS2_PLACEMENT_3D ( 'NONE', #32514, #53945, #58889 ) ;
#8314 = B_SPLINE_CURVE_WITH_KNOTS ( 'NONE', 3,
 ( #36284, #68630, #52111, #30317, #25400, #20435, #57390, #4957, #63363, #46481, #40865, #63012, #67957, #51769, #14813, #15170, #41558, #46831, #35938, #9900, #57740, #68302, #62317, #20105, #58083, #19757, #20786, #68963, #47504, #53126, #36636, #4277, #42253, #52457, #9202, #63711, #31354, #9551, #41902, #36976, #31690, #25740, #52784, #4609, #31016, #47169, #26075 ),
 .UNSPECIFIED., .F., .F.,
 ( 4, 2, 2, 2, 2, 2, 2, 2, 2, 2, 2, 2, 1, 2, 2, 2, 2, 2, 2, 2, 2, 2, 2, 4 ),
 ( 1.471961680016038988E-17, 0.001520400357568961946, 0.002280600536353415489, 0.003040800715137868381, 0.004561201072706815365, 0.005321401251491302518, 0.006081601430275788804, 0.007602001787844744896, 0.008362201966629227712, 0.009122402145413712263, 0.01064280250298268136, 0.01140300268176716592, 0.01216320286055165047, 0.01292340303933613502, 0.01368360321812061957, 0.01520400357568959041, 0.01596420375447407322, 0.01672440393325855951, 0.01824480429082752514, 0.01976520464839649077, 0.02052540482718097359, 0.02128560500596545640, 0.02280600536353444979, 0.02432640572110344318 ),
 .UNSPECIFIED. ) ;
#8315 = CARTESIAN_POINT ( 'NONE',  ( -101.3537077702550988, 33.43904726487055257, -8.213091884549116983 ) ) ;
#8316 = VECTOR ( 'NONE', #13758, 1000.000000000000000 ) ;
#8317 = CARTESIAN_POINT ( 'NONE',  ( 36.08729376665095856, 8.001156100723207487, 71.00402338158136217 ) ) ;
#8318 = CARTESIAN_POINT ( 'NONE',  ( 31.93506723555891114, 7.555455508788918806, 91.88129699972643039 ) ) ;
#8319 = DIRECTION ( 'NONE',  ( 1.000000000000000000, 0.000000000000000000, 0.000000000000000000 ) ) ;
#8320 = VERTEX_POINT ( 'NONE', #26711 ) ;
#8321 = CARTESIAN_POINT ( 'NONE',  ( -4.081377963939786468, 6.676029627840588176, -49.42132635526748885 ) ) ;
#8322 = CARTESIAN_POINT ( 'NONE',  ( -84.49322488516129681, 0.000000000000000000, 43.58025477438756212 ) ) ;
#8323 = CARTESIAN_POINT ( 'NONE',  ( -15.13211202216341000, 8.488266782358818929, 9.061675589273599840 ) ) ;
#8324 = CIRCLE ( 'NONE', #17284, 242.4895526022646379 ) ;
#8325 = DIRECTION ( 'NONE',  ( 1.000000000000000000, -0.000000000000000000, -0.000000000000000000 ) ) ;
#8326 = CARTESIAN_POINT ( 'NONE',  ( 19.54326199789021601, 7.657220834818548205, -22.67136140125942134 ) ) ;
#8327 = CARTESIAN_POINT ( 'NONE',  ( -108.1144194775597356, 35.84457139767599898, -74.09833502765862079 ) ) ;
#8328 = AXIS2_PLACEMENT_3D ( 'NONE', #36270, #15512, #20427 ) ;
#8329 = VECTOR ( 'NONE', #54065, 1000.000000000000000 ) ;
#8330 = ORIENTED_EDGE ( 'NONE', *, *, #51938, .F. ) ;
#8332 = TOROIDAL_SURFACE ( 'NONE', #38593, 22.50000000000000000, 1.500000000000000444 ) ;
#8331 =( LENGTH_UNIT ( ) NAMED_UNIT ( * ) SI_UNIT ( .MILLI., .METRE. ) );
#8333 = CARTESIAN_POINT ( 'NONE',  ( 126.7877523219523539, 38.47018873135924366, -40.96342094992535721 ) ) ;
#8334 = FACE_OUTER_BOUND ( 'NONE', #46485, .T. ) ;
#8335 = FACE_OUTER_BOUND ( 'NONE', #67692, .T. ) ;
#8336 = CARTESIAN_POINT ( 'NONE',  ( -166.2727198696243249, 79.81537471512569937, 88.93420674593960484 ) ) ;
#8337 = ORIENTED_EDGE ( 'NONE', *, *, #14857, .T. ) ;
#8338 = CARTESIAN_POINT ( 'NONE',  ( 126.3580464630938707, 38.22944795020836040, 9.865174046250384521 ) ) ;
#8339 = VERTEX_POINT ( 'NONE', #68586 ) ;
#8340 = CARTESIAN_POINT ( 'NONE',  ( -146.1142527948576912, 61.35394402951023096, -8.775903138490287247 ) ) ;
#8341 = EDGE_CURVE ( 'NONE', #61856, #4587, #54589, .T. ) ;
#8342 = DIRECTION ( 'NONE',  ( -0.000000000000000000, -0.000000000000000000, -1.000000000000000000 ) ) ;
#8343 = ORIENTED_EDGE ( 'NONE', *, *, #18653, .F. ) ;
#8344 = ADVANCED_FACE ( 'NONE', ( #41858 ), #47457, .F. ) ;
#8345 = CARTESIAN_POINT ( 'NONE',  ( 149.9615052160180824, 53.28073030175414004, 90.47490059719181943 ) ) ;
#8346 = VERTEX_POINT ( 'NONE', #4905 ) ;
#8347 = CARTESIAN_POINT ( 'NONE',  ( -62.55184817504198946, 17.87278652436697257, 10.45716724043575852 ) ) ;
#8348 = CARTESIAN_POINT ( 'NONE',  ( -2.645453300864630819E-14, -15.55634918610403616, 0.000000000000000000 ) ) ;
#8349 = EDGE_CURVE ( 'NONE', #10821, #58236, #42255, .T. ) ;
#8350 = CARTESIAN_POINT ( 'NONE',  ( -156.4797890011541881, 71.69341087347115149, 35.44366185432402006 ) ) ;
#8351 = DIRECTION ( 'NONE',  ( 1.000000000000000000, 0.000000000000000000, 0.000000000000000000 ) ) ;
#8352 = CARTESIAN_POINT ( 'NONE',  ( 0.000000000000000000, 0.000000000000000000, 20.00000000000000355 ) ) ;
#8354 = ORIENTED_EDGE ( 'NONE', *, *, #64624, .F. ) ;
#8353 = CARTESIAN_POINT ( 'NONE',  ( 15.68296563925497900, 63.09411298019765013, 41.38025477438755928 ) ) ;
#8355 = CARTESIAN_POINT ( 'NONE',  ( 61.10129719786243641, 12.23677173834304988, 44.56861354071796910 ) ) ;
#8356 = ORIENTED_EDGE ( 'NONE', *, *, #68983, .T. ) ;
#8357 = VERTEX_POINT ( 'NONE', #63316 ) ;
#8358 = CARTESIAN_POINT ( 'NONE',  ( -166.0031475600388546, 80.98114714564768235, 13.85762239588704503 ) ) ;
#8359 = ADVANCED_FACE ( 'NONE', ( #59050, #26025, #42538, #37948, #37249, #31988 ), #26369, .T. ) ;
#8360 = CARTESIAN_POINT ( 'NONE',  ( 19.10216788411014122, 6.629360741291162817, -76.59611760968499539 ) ) ;
#8361 = EDGE_CURVE ( 'NONE', #36820, #54048, #51201, .T. ) ;
#8362 = MECHANICAL_DESIGN_GEOMETRIC_PRESENTATION_REPRESENTATION (  '', ( #39786 ), #3725 ) ;
#8364 = ORIENTED_EDGE ( 'NONE', *, *, #2786, .T. ) ;
#8363 = CARTESIAN_POINT ( 'NONE',  ( -130.5904357464318082, 50.88938808445630002, 70.83209939336214234 ) ) ;
#8365 = DIRECTION ( 'NONE',  ( 0.000000000000000000, 0.000000000000000000, 1.000000000000000000 ) ) ;
#8366 = CARTESIAN_POINT ( 'NONE',  ( -71.17846906053298994, 20.67346400882179225, -43.10994888763725186 ) ) ;
#8367 = VECTOR ( 'NONE', #8404, 1000.000000000000114 ) ;
#8368 = EDGE_LOOP ( 'NONE', ( #29024, #5978, #40048, #32895 ) ) ;
#8369 = CARTESIAN_POINT ( 'NONE',  ( 211.3710169359754616, 117.8057917113659983, -74.10472688487821813 ) ) ;
#8370 = VECTOR ( 'NONE', #67571, 1000.000000000000114 ) ;
#8371 = AXIS2_PLACEMENT_3D ( 'NONE', #19317, #18977, #40772 ) ;
#8372 = CARTESIAN_POINT ( 'NONE',  ( 141.2801018238827169, 47.29457739955283557, 38.11267848623182175 ) ) ;
#8373 = DIRECTION ( 'NONE',  ( 0.000000000000000000, 0.000000000000000000, -1.000000000000000000 ) ) ;
#8374 = CIRCLE ( 'NONE', #55557, 8.000000000000001776 ) ;
#8375 = CARTESIAN_POINT ( 'NONE',  ( -132.0870433264403232, 51.94057326482882786, 15.51298448247340644 ) ) ;
#8376 = LINE ( 'NONE', #2746, #10414 ) ;
#8377 = ORIENTED_EDGE ( 'NONE', *, *, #43724, .F. ) ;
#8378 = ORIENTED_EDGE ( 'NONE', *, *, #54533, .T. ) ;
#8379 = CARTESIAN_POINT ( 'NONE',  ( 15.78827728214693416, 7.507518794609596924, -89.20804527961313113 ) ) ;
#8380 = DIRECTION ( 'NONE',  ( 0.000000000000000000, 0.000000000000000000, -1.000000000000000000 ) ) ;
#8381 = CARTESIAN_POINT ( 'NONE',  ( 0.000000000000000000, 190.0000000000000000, 2.000000000000000000 ) ) ;
#8382 = CARTESIAN_POINT ( 'NONE',  ( 0.000000000000000000, 0.000000000000000000, -50.00000000000000711 ) ) ;
#8383 = FACE_OUTER_BOUND ( 'NONE', #40334, .T. ) ;
#8384 = DIRECTION ( 'NONE',  ( -0.000000000000000000, -1.000000000000000000, -0.000000000000000000 ) ) ;
#8385 = CARTESIAN_POINT ( 'NONE',  ( -168.7150276173047416, 82.35404041280327192, -62.96885486901207685 ) ) ;
#8386 = VERTEX_POINT ( 'NONE', #48142 ) ;
#8387 = CARTESIAN_POINT ( 'NONE',  ( -107.2385267828037740, 36.51474259889403129, 32.38677383163555135 ) ) ;
#8388 = VERTEX_POINT ( 'NONE', #32337 ) ;
#8389 = CARTESIAN_POINT ( 'NONE',  ( -38.89042640463648581, 10.93374343663408688, 11.85986522438690471 ) ) ;
#8390 = CARTESIAN_POINT ( 'NONE',  ( 82.95856197793165165, 19.25847567427441120, 57.49813389157625210 ) ) ;
#8391 = ORIENTED_EDGE ( 'NONE', *, *, #66240, .T. ) ;
#8392 = CARTESIAN_POINT ( 'NONE',  ( 188.4389256074244372, 86.37278721358585187, 38.30605937947389350 ) ) ;
#8393 = CARTESIAN_POINT ( 'NONE',  ( -189.3111515777350178, 107.1887855376296983, -67.86724232585632421 ) ) ;
#8394 = CARTESIAN_POINT ( 'NONE',  ( 188.9999999999999432, -0.000000000000000000, 0.000000000000000000 ) ) ;
#8395 = DIRECTION ( 'NONE',  ( 1.000000000000000000, 0.000000000000000000, 0.000000000000000000 ) ) ;
#8396 = CARTESIAN_POINT ( 'NONE',  ( -447.6627218934913799, 367.0710678118653050, -141.4497041420117966 ) ) ;
#8397 = CARTESIAN_POINT ( 'NONE',  ( -14.33060720034884206, 8.412649192293185862, -46.68279329759894125 ) ) ;
#8398 = FACE_BOUND ( 'NONE', #48504, .T. ) ;
#8399 = VERTEX_POINT ( 'NONE', #49529 ) ;
#8400 = CARTESIAN_POINT ( 'NONE',  ( -836.0476379851789943, -568.5227338237882577, 10.00000000000000000 ) ) ;
#8401 = ORIENTED_EDGE ( 'NONE', *, *, #21582, .F. ) ;
#8402 = CARTESIAN_POINT ( 'NONE',  ( -58.96922974609609014, 15.76655591015168056, 31.41653672068953185 ) ) ;
#8403 = CYLINDRICAL_SURFACE ( 'NONE', #44286, 65.00000000000000000 ) ;
#8404 = DIRECTION ( 'NONE',  ( 0.9216045519012663334, 7.132737848110168930E-16, -0.3881301971180111110 ) ) ;
#8405 = ORIENTED_EDGE ( 'NONE', *, *, #38999, .T. ) ;
#8406 = PLANE ( 'NONE',  #22093 ) ;
#8407 = CARTESIAN_POINT ( 'NONE',  ( 149.9883446984744637, 53.30011109831374938, -71.05648309506976545 ) ) ;
#8408 = CARTESIAN_POINT ( 'NONE',  ( -38.84150381976579780, 10.92416363971239157, 36.48547519786994542 ) ) ;
#8409 = CARTESIAN_POINT ( 'NONE',  ( 134.7697261969508702, 41.97802808873665725, -50.98147753236381874 ) ) ;
#8410 = VECTOR ( 'NONE', #8721, 1000.000000000000000 ) ;
#8411 = ORIENTED_EDGE ( 'NONE', *, *, #51326, .F. ) ;
#8412 = DIRECTION ( 'NONE',  ( 9.362537406508114847E-15, -3.837369378729259059E-15, 1.000000000000000000 ) ) ;
#8413 = CARTESIAN_POINT ( 'NONE',  ( -154.0716379918897303, 69.49957566103793738, 59.09515286422640656 ) ) ;
#8414 = CARTESIAN_POINT ( 'NONE',  ( -120.1259246007803370, 42.81147313035990010, 42.94087449994837868 ) ) ;
#8415 = CARTESIAN_POINT ( 'NONE',  ( -58.96922974609608303, 15.76655591015168056, -49.11711505070150707 ) ) ;
#8416 = VERTEX_POINT ( 'NONE', #18238 ) ;
#8417 = CARTESIAN_POINT ( 'NONE',  ( -180.0154536325056824, 96.73346874014742980, -66.08948715273702135 ) ) ;
#8418 = AXIS2_PLACEMENT_3D ( 'NONE', #21280, #53272, #5101 ) ;
#8419 = CARTESIAN_POINT ( 'NONE',  ( 88.28780346671264567, 19.99350429399658324, 56.73837274249751772 ) ) ;
#8420 = VECTOR ( 'NONE', #15399, 1000.000000000000000 ) ;
#8421 = CARTESIAN_POINT ( 'NONE',  ( 113.4493678088378488, 30.39339414805073147, 43.90767737034025231 ) ) ;
#8422 = AXIS2_PLACEMENT_3D ( 'NONE', #51604, #13617, #19942 ) ;
#8423 = ADVANCED_FACE ( 'NONE', ( #66101 ), #17538, .F. ) ;
#8424 = AXIS2_PLACEMENT_3D ( 'NONE', #68725, #57497, #24461 ) ;
#8425 = EDGE_CURVE ( 'NONE', #35305, #28864, #65814, .T. ) ;
#8426 = DIRECTION ( 'NONE',  ( -4.270088556250601699E-16, -0.000000000000000000, -1.000000000000000000 ) ) ;
#8427 = EDGE_LOOP ( 'NONE', ( #22555, #1702, #1669, #39294 ) ) ;
#8428 = FACE_OUTER_BOUND ( 'NONE', #5436, .T. ) ;
#8429 = LINE ( 'NONE', #19664, #35071 ) ;
#8430 = CARTESIAN_POINT ( 'NONE',  ( 70.11438327604402332, 14.43198353181102433, 66.59053383333947806 ) ) ;
#8431 = CARTESIAN_POINT ( 'NONE',  ( 188.1848725084043110, 86.09288252323347024, -95.00000000000133582 ) ) ;
#8432 = ADVANCED_FACE ( 'NONE', ( #11546 ), #33731, .F. ) ;
#8433 = DIRECTION ( 'NONE',  ( -1.000000000000000000, 0.000000000000000000, 0.000000000000000000 ) ) ;
#8434 = ORIENTED_EDGE ( 'NONE', *, *, #19290, .F. ) ;
#8435 = AXIS2_PLACEMENT_3D ( 'NONE', #12625, #55524, #7355 ) ;
#8436 = CARTESIAN_POINT ( 'NONE',  ( 162.7963212667073662, 63.21900188423071398, -11.49336337990347268 ) ) ;
#8437 = ORIENTED_EDGE ( 'NONE', *, *, #55316, .T. ) ;
#8438 = FACE_OUTER_BOUND ( 'NONE', #36799, .T. ) ;
#8439 = CARTESIAN_POINT ( 'NONE',  ( 136.0716339513249409, 42.77788611838532518, 83.52721415416694128 ) ) ;
#8440 = EDGE_CURVE ( 'NONE', #46743, #10004, #50092, .T. ) ;
#8441 = B_SPLINE_CURVE_WITH_KNOTS ( 'NONE', 3,
 ( #35078, #56527, #23838, #3416, #8355, #24875, #12585, #50910, #7310, #29804, #8705, #7666, #29448, #13965, #45977, #56891, #51268, #28768, #55482, #35427, #3078, #66761, #24191, #45636, #40006, #46313, #60762, #67790, #67445, #55845, #24541, #30159, #34402, #34745, #45280, #39319, #44933, #29112, #50562, #66418, #34043, #18904, #50217, #2041 ),
 .UNSPECIFIED., .F., .F.,
 ( 4, 2, 2, 2, 2, 2, 2, 2, 2, 2, 2, 2, 2, 2, 2, 2, 2, 2, 2, 2, 2, 4 ),
 ( 1.430489624538199204E-17, 0.001482469635030031312, 0.002223704452545036993, 0.002964939270060043108, 0.004447408905090028015, 0.005929878540120013357, 0.007412348175149999566, 0.008153582992664998308, 0.008894817810179993581, 0.01037728744520999280, 0.01185975708023999028, 0.01260099189775499770, 0.01334222671527000685, 0.01482469635030002689, 0.01556593116781503257, 0.01630716598533003825, 0.01778963562036003573, 0.01927210525539003322, 0.02001334007290503716, 0.02075457489042003417, 0.02223704452545005941, 0.02371951416048008118 ),
 .UNSPECIFIED. ) ;
#8442 = ORIENTED_EDGE ( 'NONE', *, *, #48484, .F. ) ;
#8443 = CARTESIAN_POINT ( 'NONE',  ( -143.2464978228199470, 59.04559547356110016, -65.01991048928078953 ) ) ;
#8444 = CYLINDRICAL_SURFACE ( 'NONE', #53975, 75.00000000000001421 ) ;
#8445 = CARTESIAN_POINT ( 'NONE',  ( 164.8407099662995563, 63.61629583487395223, -45.03983226934109751 ) ) ;
#8446 = ORIENTED_EDGE ( 'NONE', *, *, #10463, .F. ) ;
#8447 = CARTESIAN_POINT ( 'NONE',  ( -100.4440683050664802, 32.98184228837415333, 18.46101985899770881 ) ) ;
#8448 = DIRECTION ( 'NONE',  ( 1.000000000000000000, 0.000000000000000000, -0.000000000000000000 ) ) ;
#8449 = CARTESIAN_POINT ( 'NONE',  ( 39.40195752203891999, 9.424259417798149130, 44.91383430596327742 ) ) ;
#8450 = AXIS2_PLACEMENT_3D ( 'NONE', #33478, #67813, #23266 ) ;
#8451 = CARTESIAN_POINT ( 'NONE',  ( 79.63513233364427890, 18.20496177163924045, -19.19606465532076101 ) ) ;
#8452 = CARTESIAN_POINT ( 'NONE',  ( -173.5164030641130921, 89.08225398748109569, -88.40105834567732757 ) ) ;
#8453 = CARTESIAN_POINT ( 'NONE',  ( 149.5059104800819796, -64.94516058774519252, -90.98255102680806772 ) ) ;
#8454 = CARTESIAN_POINT ( 'NONE',  ( -34.39004539972345498, 0.000000000000000000, -9.999999999999998224 ) ) ;
#8455 = ORIENTED_EDGE ( 'NONE', *, *, #8735, .T. ) ;
#8456 = CARTESIAN_POINT ( 'NONE',  ( -97.88021438939452423, 31.71889184683104901, 70.95604366137317243 ) ) ;
#8457 = CARTESIAN_POINT ( 'NONE',  ( -13.92109095214680181, 8.375243258322935702, 60.08374128700357630 ) ) ;
#8458 = EDGE_LOOP ( 'NONE', ( #31773, #35346, #60835, #17573, #27613, #66102, #6422, #6758, #46827 ) ) ;
#8459 = AXIS2_PLACEMENT_3D ( 'NONE', #30320, #9554, #52459 ) ;
#8460 = CARTESIAN_POINT ( 'NONE',  ( 153.2208437558771834, 55.67531116261155688, -10.58205773850701092 ) ) ;
#8461 = LINE ( 'NONE', #29913, #12935 ) ;
#8462 = VECTOR ( 'NONE', #33828, 1000.000000000000000 ) ;
#8463 = CARTESIAN_POINT ( 'NONE',  ( -38.54237244144231056, 11.89088379031759857, 40.13604733081889719 ) ) ;
#8464 = CARTESIAN_POINT ( 'NONE',  ( -156.9406434201983700, 70.74968524571474404, -68.00748788645172738 ) ) ;
#8465 = CARTESIAN_POINT ( 'NONE',  ( 10.73115448446747244, -22.57968829347487727, 0.000000000000000000 ) ) ;
#8466 = CARTESIAN_POINT ( 'NONE',  ( -50.51700111023806983, 13.51182830536853707, -63.56779930169986415 ) ) ;
#8467 = CARTESIAN_POINT ( 'NONE',  ( -1.327237339234998759, 7.561837009978233048, -12.32062923382155795 ) ) ;
#8468 = VECTOR ( 'NONE', #11523, 1000.000000000000000 ) ;
#8469 = CARTESIAN_POINT ( 'NONE',  ( 31.11269837220803325, -10.55634918610409656, 85.00100000000000477 ) ) ;
#8470 = CARTESIAN_POINT ( 'NONE',  ( -60.13226458141419783, 16.10241298991027392, 16.49623137758026203 ) ) ;
#8471 = ORIENTED_EDGE ( 'NONE', *, *, #21836, .T. ) ;
#8473 = CIRCLE ( 'NONE', #47765, 5.000000000000060396 ) ;
#8472 = FACE_OUTER_BOUND ( 'NONE', #38130, .T. ) ;
#8474 = ORIENTED_EDGE ( 'NONE', *, *, #37393, .T. ) ;
#8475 = SURFACE_STYLE_FILL_AREA ( #51035 ) ;
#8476 = APPLICATION_CONTEXT ( 'automotive_design' ) ;
#8477 = DIRECTION ( 'NONE',  ( 0.000000000000000000, 0.000000000000000000, -1.000000000000000000 ) ) ;
#8478 = DIRECTION ( 'NONE',  ( -0.9959742939952397345, 0.08963930890342655666, 0.000000000000000000 ) ) ;
#8479 = CARTESIAN_POINT ( 'NONE',  ( 3.673940397442059178E-15, 70.00000000000000000, 30.00000000000000000 ) ) ;
#8480 = CARTESIAN_POINT ( 'NONE',  ( 17.48988570800757714, 7.568061572928497682, 44.82321039106459182 ) ) ;
#8481 = FACE_OUTER_BOUND ( 'NONE', #37348, .T. ) ;
#8482 = ORIENTED_EDGE ( 'NONE', *, *, #24944, .T. ) ;
#8483 = EDGE_CURVE ( 'NONE', #36461, #52626, #670, .T. ) ;
#8484 = CARTESIAN_POINT ( 'NONE',  ( 57.24431143549729484, 12.43480675010534142, -92.04784424611891325 ) ) ;
#8485 = CARTESIAN_POINT ( 'NONE',  ( -165.9111709580270713, 79.44576090485635689, 67.25285630311519469 ) ) ;
#8486 = ORIENTED_EDGE ( 'NONE', *, *, #63356, .T. ) ;
#8487 = VERTEX_POINT ( 'NONE', #6637 ) ;
#8488 = CARTESIAN_POINT ( 'NONE',  ( -102.2801239173131194, -170.0000000000000000, -42.51457726497592660 ) ) ;
#8489 = CARTESIAN_POINT ( 'NONE',  ( -5.767955557622883589E-14, -26.11269837220806522, 0.000000000000000000 ) ) ;
#8490 = CARTESIAN_POINT ( 'NONE',  ( 180.2473887773227830, 77.76029175826235473, -9.380507075415927432 ) ) ;
#8491 = EDGE_CURVE ( 'NONE', #51274, #63292, #38285, .T. ) ;
#8492 = CARTESIAN_POINT ( 'NONE',  ( 0.000000000000000000, 0.000000000000000000, 170.0000000000000000 ) ) ;
#8493 = CARTESIAN_POINT ( 'NONE',  ( 26.11269837220812562, 31.11269837220800483, 0.000000000000000000 ) ) ;
#8494 = CARTESIAN_POINT ( 'NONE',  ( -52.13778968636795241, 39.42540649521991014, 41.38025477438755928 ) ) ;
#8495 = ORIENTED_EDGE ( 'NONE', *, *, #14115, .F. ) ;
#8496 = LINE ( 'NONE', #45780, #36770 ) ;
#8497 = CARTESIAN_POINT ( 'NONE',  ( 208.9781236209185522, 112.4006213943319494, 16.03836552217190103 ) ) ;
#8498 = CARTESIAN_POINT ( 'NONE',  ( 8.480977594057444335, 7.382886909400594000, 62.65247559583071535 ) ) ;
#8499 = CARTESIAN_POINT ( 'NONE',  ( 205.0999694062793708, 106.8955893716604777, 29.20772073876941732 ) ) ;
#8500 = FACE_BOUND ( 'NONE', #39990, .T. ) ;
#8501 = ADVANCED_FACE ( 'NONE', ( #35811 ), #9076, .F. ) ;
#8502 = EDGE_CURVE ( 'NONE', #49177, #18239, #25261, .T. ) ;
#8503 = CONICAL_SURFACE ( 'NONE', #62425, 65.00000000000000000, 0.7853981633974497223 ) ;
#8504 = VERTEX_POINT ( 'NONE', #67475 ) ;
#8505 = ORIENTED_EDGE ( 'NONE', *, *, #60104, .T. ) ;
#8506 = CARTESIAN_POINT ( 'NONE',  ( 0.000000000000000000, 0.000000000000000000, 5.000000000000000000 ) ) ;
#8507 = CARTESIAN_POINT ( 'NONE',  ( -131.7919109508896440, 51.73197705097236820, 87.16560392311338035 ) ) ;
#8508 = CIRCLE ( 'NONE', #25338, 23.50000000000000000 ) ;
#8509 = CARTESIAN_POINT ( 'NONE',  ( 35.66087318222938052, 8.964867769223229033, -76.48343667692702752 ) ) ;
#8510 = CARTESIAN_POINT ( 'NONE',  ( -177.1514380519393228, 93.28180884530866024, 17.81740703023968209 ) ) ;
#8511 = EDGE_CURVE ( 'NONE', #45082, #39183, #10814, .T. ) ;
#8512 = CARTESIAN_POINT ( 'NONE',  ( 10.70182286329413657, 6.391103395496205763, 85.68233535448860039 ) ) ;
#8513 = CARTESIAN_POINT ( 'NONE',  ( 89.99999999999998579, 0.000000000000000000, 10.00000000000000000 ) ) ;
#8514 = VECTOR ( 'NONE', #4420, 1000.000000000000000 ) ;
#8515 = VECTOR ( 'NONE', #8859, 1000.000000000000114 ) ;
#8516 = VERTEX_POINT ( 'NONE', #19270 ) ;
#8517 = CARTESIAN_POINT ( 'NONE',  ( 1.224646799147353256E-15, 200.0000000000000000, 10.00000000000000000 ) ) ;
#8518 = AXIS2_PLACEMENT_3D ( 'NONE', #27196, #47274, #47958 ) ;
#8519 = CARTESIAN_POINT ( 'NONE',  ( 204.3129818922372749, 107.5244029525887726, -51.32593103262158962 ) ) ;
#8520 = VERTEX_POINT ( 'NONE', #36152 ) ;
#8521 = CARTESIAN_POINT ( 'NONE',  ( 15.55634918610409656, 31.11269837220803325, 85.00100000000000477 ) ) ;
#8522 = EDGE_LOOP ( 'NONE', ( #15796, #2759, #58518 ) ) ;
#8523 = CARTESIAN_POINT ( 'NONE',  ( -84.54326985437106146, 24.64760594531648863, -64.77422351691623703 ) ) ;
#8524 = CARTESIAN_POINT ( 'NONE',  ( -58.33157376762797242, 16.63098604184963847, -9.122086124161532084 ) ) ;
#8525 = CARTESIAN_POINT ( 'NONE',  ( 93.72059824125558691, 23.03897520779757357, -67.67350929168541995 ) ) ;
#8527 = VERTEX_POINT ( 'NONE', #29143 ) ;
#8526 = EDGE_CURVE ( 'NONE', #38085, #19443, #14002, .T. ) ;
#8528 = ORIENTED_EDGE ( 'NONE', *, *, #48317, .F. ) ;
#8529 = CARTESIAN_POINT ( 'NONE',  ( 12.03194517566455879, 6.409266703743583982, -36.50893166399959711 ) ) ;
#8530 = EDGE_CURVE ( 'NONE', #53590, #18148, #7473, .T. ) ;
#8532 = ADVANCED_FACE ( 'NONE', ( #26966 ), #4485, .T. ) ;
#8531 = DIRECTION ( 'NONE',  ( 0.000000000000000000, 0.000000000000000000, -1.000000000000000000 ) ) ;
#8533 = ADVANCED_FACE ( 'NONE', ( #52997 ), #15385, .F. ) ;
#8534 = CARTESIAN_POINT ( 'NONE',  ( 103.5589117581614573, 27.00490790413960696, 13.70687759248179383 ) ) ;
#8535 = ORIENTED_EDGE ( 'NONE', *, *, #35179, .T. ) ;
#8536 = CARTESIAN_POINT ( 'NONE',  ( -55.05276343752909440, 15.72344139423348430, -50.21632399845989170 ) ) ;
#8537 = CARTESIAN_POINT ( 'NONE',  ( 177.7886308167536527, 76.74396398590876345, -63.81728127495517100 ) ) ;
#8538 = CARTESIAN_POINT ( 'NONE',  ( -444.2277112916228248, 394.7494927581580555, -127.5188852347322666 ) ) ;
#8539 = FACE_OUTER_BOUND ( 'NONE', #65335, .T. ) ;
#8540 = CARTESIAN_POINT ( 'NONE',  ( 82.14396250120411480, 18.99560174459422868, -49.33747787473168245 ) ) ;
#8541 = CYLINDRICAL_SURFACE ( 'NONE', #14191, 7.500000000000020428 ) ;
#8542 = VERTEX_POINT ( 'NONE', #4819 ) ;
#8543 = VERTEX_POINT ( 'NONE', #25611 ) ;
#8544 = PLANE ( 'NONE',  #22300 ) ;
#8545 = CARTESIAN_POINT ( 'NONE',  ( -8.000000000000000000, -4.618802153517024500, -0.7145311798163346273 ) ) ;
#8546 = DIRECTION ( 'NONE',  ( 1.000000000000000000, 1.850550996349095901E-16, 1.228197773518735191E-20 ) ) ;
#8547 = LINE ( 'NONE', #58106, #60205 ) ;
#8548 = CARTESIAN_POINT ( 'NONE',  ( 132.9485794245231318, 40.87843215479637138, 17.62435611736938768 ) ) ;
#8549 = CARTESIAN_POINT ( 'NONE',  ( -30.37684067568228485, 9.419394800775835463, -89.07888657189737103 ) ) ;
#8550 = CARTESIAN_POINT ( 'NONE',  ( 212.0244789595925852, 118.8177636388541742, 88.78004848219350720 ) ) ;
#8551 = CARTESIAN_POINT ( 'NONE',  ( 210.9631450001600683, 117.1791136960928981, 32.54812793961757933 ) ) ;
#8552 = PLANE ( 'NONE',  #16277 ) ;
#8553 = CARTESIAN_POINT ( 'NONE',  ( -7.825402957745087207, 6.891034867348158954, 45.11558103944722120 ) ) ;
#8554 = EDGE_LOOP ( 'NONE', ( #37579, #50255 ) ) ;
#8555 = CIRCLE ( 'NONE', #48980, 65.36598343705435354 ) ;
#8556 = DIRECTION ( 'NONE',  ( 1.000000000000000000, 1.387778780781443950E-16, 0.000000000000000000 ) ) ;
#8557 = ORIENTED_EDGE ( 'NONE', *, *, #41327, .T. ) ;
#8558 = CARTESIAN_POINT ( 'NONE',  ( 198.4017331595409246, 98.09114638179340773, -21.06574306269706653 ) ) ;
#8559 = EDGE_LOOP ( 'NONE', ( #50087, #52557, #32077, #58326 ) ) ;
#8560 = CARTESIAN_POINT ( 'NONE',  ( 109.9975424824652634, 18.08738615523480675, 402.4289050101931480 ) ) ;
#8561 = VECTOR ( 'NONE', #19278, 1000.000000000000000 ) ;
#8562 = CARTESIAN_POINT ( 'NONE',  ( 188.2086267457325448, 87.61890531228286250, -72.92993270353426283 ) ) ;
#8563 = CARTESIAN_POINT ( 'NONE',  ( -38.74552978434543604, 11.93068052085773445, 93.18845920815178374 ) ) ;
#8564 = CARTESIAN_POINT ( 'NONE',  ( -99.10260179032847816, 31.19580119595417855, -35.71676853837713139 ) ) ;
#8565 = CIRCLE ( 'NONE', #41142, 65.36598343705435354 ) ;
#8566 = VECTOR ( 'NONE', #37739, 1000.000000000000000 ) ;
#8567 = CARTESIAN_POINT ( 'NONE',  ( 38.42020198992003799, 8.283430712587435352, -50.57129177816508303 ) ) ;
#8568 = DIRECTION ( 'NONE',  ( 1.000000000000000000, -0.000000000000000000, -0.000000000000000000 ) ) ;
#8569 = EDGE_CURVE ( 'NONE', #52352, #61540, #36844, .T. ) ;
#8570 = FACE_BOUND ( 'NONE', #68279, .T. ) ;
#8571 = AXIS2_PLACEMENT_3D ( 'NONE', #1654, #7643, #12561 ) ;
#8572 = CARTESIAN_POINT ( 'NONE',  ( 129.1137093889807943, 38.63348691920619871, -49.33819672148214863 ) ) ;
#8573 = VERTEX_POINT ( 'NONE', #21342 ) ;
#8574 = ORIENTED_EDGE ( 'NONE', *, *, #62429, .T. ) ;
#8575 = CONICAL_SURFACE ( 'NONE', #11911, 74.95140232871122521, 0.8777644062502172329 ) ;
#8576 = ADVANCED_FACE ( 'NONE', ( #31911 ), #15041, .F. ) ;
#8577 = DIRECTION ( 'NONE',  ( 0.1342332658176667304, -0.9909497617679331460, 0.000000000000000000 ) ) ;
#8578 = VECTOR ( 'NONE', #229, 1000.000000000000114 ) ;
#8579 = CARTESIAN_POINT ( 'NONE',  ( 188.9999999999999432, -57.00000000000007816, -2.000000000000000888 ) ) ;
#8580 = PLANE ( 'NONE',  #31900 ) ;
#8581 = UNCERTAINTY_MEASURE_WITH_UNIT (LENGTH_MEASURE( 1.000000000000000082E-05 ), #28794, 'distance_accuracy_value', 'NONE');
#8582 = CARTESIAN_POINT ( 'NONE',  ( 12.03317402819681980, 6.409531826169462931, 4.173255377313227044 ) ) ;
#8583 = ORIENTED_EDGE ( 'NONE', *, *, #38351, .T. ) ;
#8584 = CARTESIAN_POINT ( 'NONE',  ( 284.3363611114016862, 21.85800776086857056, -2.510326265702884641 ) ) ;
#8585 = CARTESIAN_POINT ( 'NONE',  ( -58.97243502469714826, 16.81420332340173829, -63.16196468205944115 ) ) ;
#8586 = CARTESIAN_POINT ( 'NONE',  ( -31.11269837220804035, 20.55634918610408945, 85.00100000000000477 ) ) ;
#8587 = CARTESIAN_POINT ( 'NONE',  ( 276.6944765335653074, -21.67660392622677534, -3.765493530430662261 ) ) ;
#8588 = CARTESIAN_POINT ( 'NONE',  ( 181.0840389613909736, 78.60582251573003987, 2.464043515047718458 ) ) ;
#8589 = CARTESIAN_POINT ( 'NONE',  ( -29.74902699556087171, 10.33856194202125600, 71.87213699941901268 ) ) ;
#8590 = CARTESIAN_POINT ( 'NONE',  ( 0.000000000000000000, 19.01593100277521131, 6.196318915105386793 ) ) ;
#8591 = EDGE_CURVE ( 'NONE', #52737, #53508, #16066, .T. ) ;
#8592 = CARTESIAN_POINT ( 'NONE',  ( -53.14475157111026959, 14.17819596930906378, 57.40458832884380058 ) ) ;
#8593 = ADVANCED_FACE ( 'NONE', ( #26633 ), #48067, .F. ) ;
#8594 = CARTESIAN_POINT ( 'NONE',  ( -1.088326810997878091, 6.545818265928950552, 61.12801010162523596 ) ) ;
#8595 = EDGE_CURVE ( 'NONE', #41030, #3067, #14746, .T. ) ;
#8596 = ORIENTED_EDGE ( 'NONE', *, *, #16636, .T. ) ;
#8597 = LINE ( 'NONE', #18102, #65289 ) ;
#8598 = CARTESIAN_POINT ( 'NONE',  ( 154.4617654203036068, 56.60942201271838314, 56.86943609086132057 ) ) ;
#8599 = CARTESIAN_POINT ( 'NONE',  ( -107.0544991134679833, 36.41543129049377114, -75.14825369610649375 ) ) ;
#8600 = CARTESIAN_POINT ( 'NONE',  ( -55.05276343752910151, 14.68156374112636264, -50.21632399845989170 ) ) ;
#8601 = DIRECTION ( 'NONE',  ( 1.000000000000000000, 0.000000000000000000, 0.000000000000000000 ) ) ;
#8602 = FACE_OUTER_BOUND ( 'NONE', #58165, .T. ) ;
#8603 = VERTEX_POINT ( 'NONE', #27306 ) ;
#8604 = DIRECTION ( 'NONE',  ( -1.000000000000000000, 0.000000000000000000, 0.000000000000000000 ) ) ;
#8605 = VERTEX_POINT ( 'NONE', #65305 ) ;
#8606 = VECTOR ( 'NONE', #57939, 1000.000000000000000 ) ;
#8607 = ORIENTED_EDGE ( 'NONE', *, *, #35262, .F. ) ;
#8608 = DIRECTION ( 'NONE',  ( -0.000000000000000000, -0.000000000000000000, -1.000000000000000000 ) ) ;
#8609 = CARTESIAN_POINT ( 'NONE',  ( 151.1827182658834658, 54.16800928478853194, 32.78911015225024528 ) ) ;
#8610 = CYLINDRICAL_SURFACE ( 'NONE', #31391, 4.999999999999997335 ) ;
#8611 = ORIENTED_EDGE ( 'NONE', *, *, #8129, .T. ) ;
#8612 = CARTESIAN_POINT ( 'NONE',  ( -173.1211646369891355, -170.0000000000000000, 45.82169460664104577 ) ) ;
#8613 = VECTOR ( 'NONE', #3544, 1000.000000000000000 ) ;
#8614 = CARTESIAN_POINT ( 'NONE',  ( -179.5178913137216341, 94.54206947403385186, 15.43129202131554756 ) ) ;
#8615 = CARTESIAN_POINT ( 'NONE',  ( -4.955782654901484285, 6.720825733572401539, 3.828862293532663053 ) ) ;
#8616 = DIRECTION ( 'NONE',  ( 1.000000000000000000, 0.000000000000000000, 0.000000000000000000 ) ) ;
#8617 = EDGE_CURVE ( 'NONE', #3858, #54158, #1284, .T. ) ;
#8619 = EDGE_CURVE ( 'NONE', #47553, #69411, #23095, .T. ) ;
#8618 = CARTESIAN_POINT ( 'NONE',  ( -79.14638003838381053, 23.58242782405879723, 45.41820113967313688 ) ) ;
#8620 = VECTOR ( 'NONE', #44395, 1000.000000000000000 ) ;
#8621 = CARTESIAN_POINT ( 'NONE',  ( 151.5037942372329383, 53.15665752640120445, 86.04130639192804608 ) ) ;
#8622 = CARTESIAN_POINT ( 'NONE',  ( 140.4897729434290738, 45.57634363643750675, 13.70496928957165750 ) ) ;
#8623 = PRODUCT_DEFINITION_FORMATION_WITH_SPECIFIED_SOURCE ( 'ANY', '', #58503, .NOT_KNOWN. ) ;
#8624 = EDGE_CURVE ( 'NONE', #11248, #10057, #61672, .T. ) ;
#8625 = ORIENTED_EDGE ( 'NONE', *, *, #32000, .F. ) ;
#8626 = CARTESIAN_POINT ( 'NONE',  ( 117.7411475730015553, 32.50808475802732289, -43.96506892200977035 ) ) ;
#8627 = CARTESIAN_POINT ( 'NONE',  ( 15.78827728214693416, 6.500811158483284835, 56.85925826316891829 ) ) ;
#8628 = DIRECTION ( 'NONE',  ( -0.000000000000000000, 1.000000000000000000, -0.000000000000000000 ) ) ;
#8629 = DIRECTION ( 'NONE',  ( 0.000000000000000000, -0.7071067811865474617, 0.7071067811865474617 ) ) ;
#8631 = VERTEX_POINT ( 'NONE', #60377 ) ;
#8630 = CYLINDRICAL_SURFACE ( 'NONE', #46665, 5.000000000000087930 ) ;
#8632 = CARTESIAN_POINT ( 'NONE',  ( 80.72161230109728081, 17.48902961068030848, -47.96845741328300505 ) ) ;
#8633 = VERTEX_POINT ( 'NONE', #11470 ) ;
#8634 = ORIENTED_EDGE ( 'NONE', *, *, #44852, .F. ) ;
#8635 = FACE_BOUND ( 'NONE', #38514, .T. ) ;
#8636 = CARTESIAN_POINT ( 'NONE',  ( 80.15818551272217007, 18.36718314243334049, 41.03562789125641785 ) ) ;
#8637 = DIRECTION ( 'NONE',  ( 0.000000000000000000, -1.000000000000000000, 0.000000000000000000 ) ) ;
#8638 = CARTESIAN_POINT ( 'NONE',  ( 183.1910712700538113, 80.76073941711165105, -9.669732058764036964 ) ) ;
#8639 = CARTESIAN_POINT ( 'NONE',  ( 0.000000000000000000, 0.000000000000000000, 41.38025477438755928 ) ) ;
#8640 = CARTESIAN_POINT ( 'NONE',  ( -83.53167274806554587, 25.32068190668983831, -10.04220442384894341 ) ) ;
#8641 = FACE_OUTER_BOUND ( 'NONE', #30628, .T. ) ;
#8642 = CARTESIAN_POINT ( 'NONE',  ( -150.3898662070192529, 64.92828409760433317, -34.81283053149196149 ) ) ;
#8643 = VERTEX_POINT ( 'NONE', #67319 ) ;
#8644 = VERTEX_POINT ( 'NONE', #43827 ) ;
#8645 = CARTESIAN_POINT ( 'NONE',  ( -105.8879245385188170, 35.79035667534147791, 17.76733064874386514 ) ) ;
#8646 = CARTESIAN_POINT ( 'NONE',  ( 102.8518012651273921, 25.61025413220827573, 65.25412124308606110 ) ) ;
#8647 = FACE_BOUND ( 'NONE', #61958, .T. ) ;
#8648 = CARTESIAN_POINT ( 'NONE',  ( -189.5325095384513645, 107.4952257375067575, 67.39672208484692817 ) ) ;
#8649 = CARTESIAN_POINT ( 'NONE',  ( 0.000000000000000000, 0.000000000000000000, 0.000000000000000000 ) ) ;
#8650 = CYLINDRICAL_SURFACE ( 'NONE', #60693, 7.500000000000013323 ) ;
#8651 = CARTESIAN_POINT ( 'NONE',  ( -142.7670279077608768, 59.94957184373900816, 88.60369296171910491 ) ) ;
#8652 = VERTEX_POINT ( 'NONE', #16756 ) ;
#8653 = PRODUCT_DEFINITION_SHAPE ( 'NONE', 'NONE',  #69587 ) ;
#8654 = ORIENTED_EDGE ( 'NONE', *, *, #66322, .F. ) ;
#8655 = ORIENTED_EDGE ( 'NONE', *, *, #46300, .T. ) ;
#8656 = AXIS2_PLACEMENT_3D ( 'NONE', #35470, #57275, #9087 ) ;
#8657 = ADVANCED_FACE ( 'NONE', ( #18768 ), #52392, .F. ) ;
#8658 = DIRECTION ( 'NONE',  ( 1.000000000000000000, 0.000000000000000000, 0.000000000000000000 ) ) ;
#8659 = DIRECTION ( 'NONE',  ( 0.2660368455666826670, -0.9639628606958512425, 2.500042656554809847E-16 ) ) ;
#8660 = CARTESIAN_POINT ( 'NONE',  ( 70.11438327604403753, 14.43198353181102433, -40.78766852851526892 ) ) ;
#8661 = CARTESIAN_POINT ( 'NONE',  ( 106.0266963907629645, -21.78888161821124925, 3.052770673153796466 ) ) ;
#8662 = AXIS2_PLACEMENT_3D ( 'NONE', #64980, #28378, #22756 ) ;
#8663 = CARTESIAN_POINT ( 'NONE',  ( -62.54086041493278714, 17.86944394914988976, 38.30844689331261321 ) ) ;
#8664 = CARTESIAN_POINT ( 'NONE',  ( -31.43908319763709969, 10.61114334766716638, -77.16174795566554678 ) ) ;
#8665 = CIRCLE ( 'NONE', #18797, 160.5210298272983209 ) ;
#8666 = CARTESIAN_POINT ( 'NONE',  ( 59.72647370436681769, 12.96353798836696392, 44.05766389829923213 ) ) ;
#8667 = CARTESIAN_POINT ( 'NONE',  ( 44.96493392236942555, 9.198276979102484319, 86.06197627692814933 ) ) ;
#8668 =( NAMED_UNIT ( * ) PLANE_ANGLE_UNIT ( ) SI_UNIT ( $, .RADIAN. ) );
#8669 = VERTEX_POINT ( 'NONE', #49098 ) ;
#8670 = VECTOR ( 'NONE', #66113, 1000.000000000000000 ) ;
#8671 = CARTESIAN_POINT ( 'NONE',  ( -0.3249717932738294679, 6.518578686837486202, -42.42990240311857519 ) ) ;
#8672 = CARTESIAN_POINT ( 'NONE',  ( 58.32618558115825635, 1.250000000000015099, 27.58472369367762411 ) ) ;
#8673 = CARTESIAN_POINT ( 'NONE',  ( -120.1497954511983437, 42.82624472369558788, 6.426331581351773181 ) ) ;
#8674 = CARTESIAN_POINT ( 'NONE',  ( 3.000000000000028866, 6.000000000000000000, -3.000000000000030198 ) ) ;
#8675 = CARTESIAN_POINT ( 'NONE',  ( 130.3019683985925781, 39.31883119822050787, -23.29995166167127252 ) ) ;
#8676 = EDGE_CURVE ( 'NONE', #64051, #24493, #60225, .T. ) ;
#8677 = CARTESIAN_POINT ( 'NONE',  ( -125.8938041572051389, -170.0000000000000000, 11.27539728269340280 ) ) ;
#8678 = CARTESIAN_POINT ( 'NONE',  ( 198.7029050523552485, 98.46895521196215384, 68.08812002989884604 ) ) ;
#8679 = CIRCLE ( 'NONE', #58116, 242.4895526022646379 ) ;
#8680 = EDGE_CURVE ( 'NONE', #59735, #47754, #8909, .T. ) ;
#8681 = EDGE_CURVE ( 'NONE', #7362, #46731, #15214, .T. ) ;
#8682 = ORIENTED_EDGE ( 'NONE', *, *, #41042, .F. ) ;
#8683 = APPLICATION_PROTOCOL_DEFINITION ( 'draft international standard', 'automotive_design', 1998, #11623 ) ;
#8684 = CARTESIAN_POINT ( 'NONE',  ( 126.4219470349615904, 38.26519385429183728, -42.50070869923012395 ) ) ;
#8685 = CYLINDRICAL_SURFACE ( 'NONE', #45508, 7.500000000000013323 ) ;
#8686 = DIRECTION ( 'NONE',  ( 0.000000000000000000, 0.000000000000000000, 1.000000000000000000 ) ) ;
#8687 = CARTESIAN_POINT ( 'NONE',  ( 188.4374648754671568, 87.87346242052443301, -45.22988680152230501 ) ) ;
#8688 = ORIENTED_EDGE ( 'NONE', *, *, #63155, .T. ) ;
#8689 = ORIENTED_EDGE ( 'NONE', *, *, #38093, .T. ) ;
#8690 = CARTESIAN_POINT ( 'NONE',  ( -142.8450945664714880, 58.72815783657285493, -12.01356147524839102 ) ) ;
#8691 = CARTESIAN_POINT ( 'NONE',  ( 0.000000000000000000, 0.000000000000000000, 0.000000000000000000 ) ) ;
#8692 = ORIENTED_EDGE ( 'NONE', *, *, #46795, .F. ) ;
#8693 = B_SPLINE_CURVE_WITH_KNOTS ( 'NONE', 3,
 ( #63374, #53135, #30675, #68973, #31027, #9218, #63722, #26084, #36297, #9567, #4292, #52467, #52122, #68639, #20117, #25410, #20450, #20801, #4965, #3942, #47514, #31703, #46149, #67623, #15532, #15185, #14492, #36646, #67972, #40875, #57066, #36984, #14149, #14828, #3591, #58423, #58091, #9911, #62337, #31367, #10237, #46490, #19418, #52796, #35611, #8879, #30329, #19772, #41230, #35949, #46845, #68313, #41568, #37311, #25 ),
 .UNSPECIFIED., .F., .F.,
 ( 4, 2, 2, 2, 2, 2, 2, 2, 2, 2, 2, 2, 2, 2, 2, 2, 2, 2, 2, 1, 2, 2, 2, 2, 2, 2, 2, 4 ),
 ( 0.000000000000000000, 0.001942359098140214761, 0.002913538647210304252, 0.003884718196280394394, 0.004855897745350484102, 0.005827077294420574677, 0.006798256843490665252, 0.007769436392560754960, 0.009711795490700933509, 0.01068297503977101715, 0.01165415458884109731, 0.01262533413791117921, 0.01359651368698126112, 0.01456769323605134128, 0.01553887278512142318, 0.01748123188326161995, 0.01845241143233171399, 0.01942359098140180457, 0.02039477053047190208, 0.02136595007954199613, 0.02233712962861208670, 0.02330830917768218075, 0.02525066827582240700, 0.02719302737396263325, 0.02816420692303274118, 0.02913538647210285257, 0.03010656602117296396, 0.03107774557024307188 ),
 .UNSPECIFIED. ) ;
#8694 = CARTESIAN_POINT ( 'NONE',  ( 164.6573696294227886, 64.77826598361185972, 92.77428207146242300 ) ) ;
#8695 = ORIENTED_EDGE ( 'NONE', *, *, #69243, .F. ) ;
#8696 = CARTESIAN_POINT ( 'NONE',  ( 126.4318266066172214, 38.27072266789465971, -71.45960955399186787 ) ) ;
#8697 = CARTESIAN_POINT ( 'NONE',  ( 127.4953815656695042, 37.71366486045443622, 41.01473559900087906 ) ) ;
#8698 = CARTESIAN_POINT ( 'NONE',  ( -156.9900125991010498, 72.16580261738673130, 37.63415873823330315 ) ) ;
#8699 = CARTESIAN_POINT ( 'NONE',  ( -102.2801239173131194, -170.0000000000000000, -50.01457726497594081 ) ) ;
#8700 = DIRECTION ( 'NONE',  ( -1.000000000000000000, 0.000000000000000000, 0.000000000000000000 ) ) ;
#8702 = ORIENTED_EDGE ( 'NONE', *, *, #1380, .T. ) ;
#8701 = CARTESIAN_POINT ( 'NONE',  ( 209.3223706822284100, 190.0000000000000000, 277.8007638641562380 ) ) ;
#8703 = VECTOR ( 'NONE', #34561, 1000.000000000000000 ) ;
#8704 = EDGE_CURVE ( 'NONE', #41997, #60761, #46643, .T. ) ;
#8705 = CARTESIAN_POINT ( 'NONE',  ( 58.09436971064711486, 11.58462396079456802, 42.99375819818929045 ) ) ;
#8706 = ORIENTED_EDGE ( 'NONE', *, *, #36936, .T. ) ;
#8707 = ORIENTED_EDGE ( 'NONE', *, *, #13270, .T. ) ;
#8708 = VECTOR ( 'NONE', #37798, 1000.000000000000114 ) ;
#8709 = CARTESIAN_POINT ( 'NONE',  ( -165.7690020878298469, 80.74028011998679233, 9.965654948806628610 ) ) ;
#8710 = CARTESIAN_POINT ( 'NONE',  ( 23.03864809957654103, 6.841061756139155570, -67.92891564569549701 ) ) ;
#8711 = AXIS2_PLACEMENT_3D ( 'NONE', #20766, #5279, #53448 ) ;
#8713 = ORIENTED_EDGE ( 'NONE', *, *, #5490, .F. ) ;
#8712 = CARTESIAN_POINT ( 'NONE',  ( -130.2071229607963119, 50.62285182196877997, 71.11791843384300194 ) ) ;
#8714 = CARTESIAN_POINT ( 'NONE',  ( -149.5074843970971301, -170.0000000000000000, -15.46827994102828541 ) ) ;
#8715 = CARTESIAN_POINT ( 'NONE',  ( -73.09214866197369531, 21.34321757515763451, -47.65756488281920156 ) ) ;
#8716 = VECTOR ( 'NONE', #61722, 1000.000000000000000 ) ;
#8717 = ORIENTED_EDGE ( 'NONE', *, *, #39789, .F. ) ;
#8718 = AXIS2_PLACEMENT_3D ( 'NONE', #29906, #55232, #39077 ) ;
#8719 = CARTESIAN_POINT ( 'NONE',  ( 208.9583973663597760, 114.1615900753670729, -76.85894075021298022 ) ) ;
#8720 = VECTOR ( 'NONE', #64952, 1000.000000000000000 ) ;
#8721 = DIRECTION ( 'NONE',  ( 1.000000000000000000, 0.000000000000000000, -2.220446049250313081E-16 ) ) ;
#8722 = CARTESIAN_POINT ( 'NONE',  ( 116.0822834687217124, 32.80169113915573575, 41.84374816554769438 ) ) ;
#8723 = CARTESIAN_POINT ( 'NONE',  ( -63.89980862959375685, 18.93195709527340043, 34.48241795236666007 ) ) ;
#8724 = DIRECTION ( 'NONE',  ( 0.4738686624729966379, 0.8805955318567391110, 0.000000000000000000 ) ) ;
#8725 = ORIENTED_EDGE ( 'NONE', *, *, #7939, .F. ) ;
#8726 = VERTEX_POINT ( 'NONE', #31060 ) ;
#8727 = DIRECTION ( 'NONE',  ( 1.000000000000000000, 0.000000000000000000, 0.000000000000000000 ) ) ;
#8728 = FACE_OUTER_BOUND ( 'NONE', #54277, .T. ) ;
#8729 = LINE ( 'NONE', #9412, #65502 ) ;
#8730 = PRODUCT_DEFINITION ( 'UNKNOWN', '', #39993, #38055 ) ;
#8731 = CARTESIAN_POINT ( 'NONE',  ( 0.000000000000000000, 0.000000000000000000, 22.50000000000000000 ) ) ;
#8732 = DIRECTION ( 'NONE',  ( -4.314083075427411048E-32, -1.000000000000000000, -6.123233995736763571E-17 ) ) ;
#8733 = DIRECTION ( 'NONE',  ( -0.000000000000000000, 0.000000000000000000, -1.000000000000000000 ) ) ;
#8734 = CARTESIAN_POINT ( 'NONE',  ( 66.30636076182547356, 14.49616748423541779, -36.46357697616834770 ) ) ;
#8735 = EDGE_CURVE ( 'NONE', #26073, #476, #51813, .T. ) ;
#8736 = CARTESIAN_POINT ( 'NONE',  ( -118.8691191306315034, 43.21907118237574252, 40.76062911680295286 ) ) ;
#8737 = CARTESIAN_POINT ( 'NONE',  ( -172.7154982671752634, 86.67743928531946551, -76.55650775521371543 ) ) ;
#8739 = VERTEX_POINT ( 'NONE', #37345 ) ;
#8738 = EDGE_CURVE ( 'NONE', #64426, #55324, #56747, .T. ) ;
#8740 = CARTESIAN_POINT ( 'NONE',  ( -103.8932886509197004, 34.74144483217663293, 30.69090865985877414 ) ) ;
#8741 = ORIENTED_EDGE ( 'NONE', *, *, #49210, .F. ) ;
#8742 = CARTESIAN_POINT ( 'NONE',  ( -179.7494535813537482, 94.82199694967370363, -92.35590895999905570 ) ) ;
#8743 = EDGE_CURVE ( 'NONE', #18334, #16719, #30785, .T. ) ;
#8744 = CARTESIAN_POINT ( 'NONE',  ( 80.16761386260786537, 18.37011649821944559, 60.21652803898918904 ) ) ;
#8745 = VERTEX_POINT ( 'NONE', #42295 ) ;
#8746 = CARTESIAN_POINT ( 'NONE',  ( 44.01696072966020523, -47.84694004974148385, 41.38025477438755928 ) ) ;
#8747 = CARTESIAN_POINT ( 'NONE',  ( -189.7987719395348734, 107.8653664616570467, -66.07470785493005394 ) ) ;
#8748 = DIRECTION ( 'NONE',  ( 0.000000000000000000, 1.000000000000000000, 0.000000000000000000 ) ) ;
#8749 = DIRECTION ( 'NONE',  ( 0.000000000000000000, 0.000000000000000000, -1.000000000000000000 ) ) ;
#8750 = CARTESIAN_POINT ( 'NONE',  ( -64.83840629396348731, 4.580509716059292913, 40.00000000000003553 ) ) ;
#8751 = CARTESIAN_POINT ( 'NONE',  ( -33.12994257348896099, 10.89587983539684934, -23.28366193412811214 ) ) ;
#8752 = EDGE_LOOP ( 'NONE', ( #59293, #45483, #44314, #27129 ) ) ;
#8753 = AXIS2_PLACEMENT_3D ( 'NONE', #56796, #56097, #7913 ) ;
#8754 = DIRECTION ( 'NONE',  ( -0.000000000000000000, -1.000000000000000000, -0.000000000000000000 ) ) ;
#8755 = ORIENTED_EDGE ( 'NONE', *, *, #26991, .F. ) ;
#8756 = EDGE_CURVE ( 'NONE', #9333, #4577, #44511, .T. ) ;
#8757 = CARTESIAN_POINT ( 'NONE',  ( 24.39800339187929268, -60.26242556095670722, 3.061616997868437868E-16 ) ) ;
#8758 = LINE ( 'NONE', #29499, #68982 ) ;
#8759 = PLANE ( 'NONE',  #53313 ) ;
#8760 = EDGE_LOOP ( 'NONE', ( #37980, #44653, #19269, #29519 ) ) ;
#8761 = B_SPLINE_CURVE_WITH_KNOTS ( 'NONE', 3,
 ( #6158, #44504, #50480, #6868, #28317, #65983 ),
 .UNSPECIFIED., .F., .F.,
 ( 4, 2, 4 ),
 ( 0.03218936187311347702, 0.06469833704501401495, 0.09720731221691455981 ),
 .UNSPECIFIED. ) ;
#8762 = CARTESIAN_POINT ( 'NONE',  ( -20.00000000000002842, 3.680555555555560243, 4.000000000000000000 ) ) ;
#8763 = CARTESIAN_POINT ( 'NONE',  ( -57.96611496808679220, 15.48164310774731511, -89.48114299131638916 ) ) ;
#8764 = CARTESIAN_POINT ( 'NONE',  ( 2.699999999999990408, 0.000000000000000000, -20.30000000000000071 ) ) ;
#8765 = VECTOR ( 'NONE', #33584, 1000.000000000000000 ) ;
#8766 = FILL_AREA_STYLE ('',( #37197 ) ) ;
#8767 = EDGE_CURVE ( 'NONE', #66603, #36977, #23182, .T. ) ;
#8768 = EDGE_CURVE ( 'NONE', #9895, #52559, #26535, .T. ) ;
#8769 = VERTEX_POINT ( 'NONE', #29241 ) ;
#8770 =( NAMED_UNIT ( * ) SI_UNIT ( $, .STERADIAN. ) SOLID_ANGLE_UNIT ( ) );
#8771 = CARTESIAN_POINT ( 'NONE',  ( -149.9471644042847061, 65.87751327280741975, 57.57507356156872191 ) ) ;
#8772 = CARTESIAN_POINT ( 'NONE',  ( -190.6985136298602015, 109.1272424661243434, 69.71826505393651985 ) ) ;
#8773 = VECTOR ( 'NONE', #60600, 1000.000000000000000 ) ;
#8774 = CARTESIAN_POINT ( 'NONE',  ( 61.62594073580542897, 21.79346734965000820, 41.38025477438755928 ) ) ;
#8775 = VERTEX_POINT ( 'NONE', #2510 ) ;
#8776 = DIRECTION ( 'NONE',  ( 0.8465179929926601732, 0.5323601107705934199, 0.000000000000000000 ) ) ;
#8777 = CARTESIAN_POINT ( 'NONE',  ( 126.6884460900547253, 38.41453276189364630, 88.46451693205000311 ) ) ;
#8778 = CARTESIAN_POINT ( 'NONE',  ( 202.1047637245956707, 104.5251427319220880, -90.44580026730181999 ) ) ;
#8779 = CARTESIAN_POINT ( 'NONE',  ( 0.000000000000000000, 0.000000000000000000, 170.0000000000000000 ) ) ;
#8780 = VECTOR ( 'NONE', #57937, 1000.000000000000000 ) ;
#8781 = DIRECTION ( 'NONE',  ( 1.807017991507195025E-16, 1.727686100818934983E-16, 1.000000000000000000 ) ) ;
#8782 = VERTEX_POINT ( 'NONE', #45058 ) ;
#8783 = CARTESIAN_POINT ( 'NONE',  ( 133.8566784816069344, -170.0000000000000000, -9.178760341931969435 ) ) ;
#8784 = CARTESIAN_POINT ( 'NONE',  ( 110.2429982417149290, 28.88204397445231209, -77.76698815611739235 ) ) ;
#8785 = CARTESIAN_POINT ( 'NONE',  ( 64.94794467308301478, 13.12874966082104500, 71.42075418314232138 ) ) ;
#8786 = CARTESIAN_POINT ( 'NONE',  ( 134.0849965622592777, 42.73957449886180626, 2.665790248531672457 ) ) ;
#8787 = DIRECTION ( 'NONE',  ( -0.7071067811865405783, -7.105427357601001070E-15, 0.7071067811865545671 ) ) ;
#8788 = ORIENTED_EDGE ( 'NONE', *, *, #1909, .T. ) ;
#8789 = CARTESIAN_POINT ( 'NONE',  ( 164.0105905242218967, 64.23277447906897919, -20.45969130717543294 ) ) ;
#8790 = VERTEX_POINT ( 'NONE', #38753 ) ;
#8791 = DIRECTION ( 'NONE',  ( 0.000000000000000000, 0.000000000000000000, 1.000000000000000000 ) ) ;
#8792 = CARTESIAN_POINT ( 'NONE',  ( 131.4605497067148576, 39.99540099990633735, 83.56475536640037660 ) ) ;
#8794 = ORIENTED_EDGE ( 'NONE', *, *, #38584, .T. ) ;
#8793 = LINE ( 'NONE', #40782, #12943 ) ;
#8795 = CARTESIAN_POINT ( 'NONE',  ( 163.5944155533005642, 63.88379440759436534, -47.96116750131039908 ) ) ;
#8796 = CARTESIAN_POINT ( 'NONE',  ( -142.0747101610765242, 58.12276061064464017, -95.00000000000133582 ) ) ;
#8797 = CARTESIAN_POINT ( 'NONE',  ( 164.0298848570287191, 62.93631132702880393, -39.94902995324983408 ) ) ;
#8798 = ORIENTED_EDGE ( 'NONE', *, *, #54860, .T. ) ;
#8799 = CARTESIAN_POINT ( 'NONE',  ( -101.3537077702551130, 33.43904726487055257, 18.63145870591456088 ) ) ;
#8800 = PLANE ( 'NONE',  #29004 ) ;
#8801 = AXIS2_PLACEMENT_3D ( 'NONE', #53545, #65159, #11682 ) ;
#8802 = CARTESIAN_POINT ( 'NONE',  ( 151.4107046593863970, 54.33532586763775640, -92.88899967025768944 ) ) ;
#8803 = CARTESIAN_POINT ( 'NONE',  ( 84.97658021689284169, 19.92447159015900127, -23.79656231590709226 ) ) ;
#8804 = CARTESIAN_POINT ( 'NONE',  ( -177.4531271036652811, 93.64011491047624247, -89.77488431374720790 ) ) ;
#8805 = CARTESIAN_POINT ( 'NONE',  ( -35.17686701826946205, 10.23452050416468317, -63.14123844676133501 ) ) ;
#8806 = DIRECTION ( 'NONE',  ( 0.000000000000000000, 0.000000000000000000, -1.000000000000000000 ) ) ;
#8807 = ORIENTED_EDGE ( 'NONE', *, *, #38183, .T. ) ;
#8808 = CARTESIAN_POINT ( 'NONE',  ( -100.4347360276018719, 32.97716872911836106, 57.57929195606707395 ) ) ;
#8809 = CARTESIAN_POINT ( 'NONE',  ( -15.32584732649904069, 8.506915958926390076, 64.94853716179643754 ) ) ;
#8810 = ORIENTED_EDGE ( 'NONE', *, *, #54510, .T. ) ;
#8811 = CARTESIAN_POINT ( 'NONE',  ( 150.7770046255793090, 53.87214803240242134, -13.38559856645425938 ) ) ;
#8812 = EDGE_CURVE ( 'NONE', #13372, #64405, #2168, .T. ) ;
#8813 = AXIS2_PLACEMENT_3D ( 'NONE', #50838, #35359, #24117 ) ;
#8814 = CARTESIAN_POINT ( 'NONE',  ( 4.590321433068643486, 24.57496590315240681, 0.000000000000000000 ) ) ;
#8815 = CARTESIAN_POINT ( 'NONE',  ( -16.43619359402630664, 18.99971924381106092, 0.000000000000000000 ) ) ;
#8816 = LINE ( 'NONE', #47118, #43368 ) ;
#8817 = FACE_OUTER_BOUND ( 'NONE', #68179, .T. ) ;
#8818 = CARTESIAN_POINT ( 'NONE',  ( 186.7642514597452816, 86.02880938169741398, 14.86798059005289119 ) ) ;
#8819 = DIRECTION ( 'NONE',  ( 1.000000000000000000, 0.000000000000000000, 0.000000000000000000 ) ) ;
#8820 = ADVANCED_FACE ( 'NONE', ( #1821 ), #33488, .F. ) ;
#8821 = CARTESIAN_POINT ( 'NONE',  ( 181.0840389613909736, 78.60582251573002566, 17.46404351504774510 ) ) ;
#8822 = CARTESIAN_POINT ( 'NONE',  ( -62.30463872474478393, 16.74658165105248031, 8.995110152397721492 ) ) ;
#8823 = ORIENTED_EDGE ( 'NONE', *, *, #5158, .T. ) ;
#8824 = DIRECTION ( 'NONE',  ( 0.000000000000000000, 1.000000000000000000, 0.000000000000000000 ) ) ;
#8826 = ORIENTED_EDGE ( 'NONE', *, *, #44878, .F. ) ;
#8825 = EDGE_CURVE ( 'NONE', #5765, #47170, #55617, .T. ) ;
#8827 = CARTESIAN_POINT ( 'NONE',  ( 103.8093541423579325, 26.01745837747065337, -74.15374262448062836 ) ) ;
#8828 = CARTESIAN_POINT ( 'NONE',  ( 169.9999999999999716, 3.680555555555560243, 4.000000000000000000 ) ) ;
#8829 = CARTESIAN_POINT ( 'NONE',  ( -76.10397364431022993, 21.36211154336730189, 4.020946145479624256 ) ) ;
#8830 = DIRECTION ( 'NONE',  ( -0.1785568947986229116, -0.9839295885986321100, 5.102127870520020458E-18 ) ) ;
#8831 = EDGE_CURVE ( 'NONE', #26680, #67396, #34872, .T. ) ;
#8832 = CARTESIAN_POINT ( 'NONE',  ( -1.041619319073134209, 6.544118473861825436, 88.08972450370782781 ) ) ;
#8833 = CARTESIAN_POINT ( 'NONE',  ( -103.2061297292849673, 34.38496953192505856, -23.12722278067304771 ) ) ;
#8834 = ORIENTED_EDGE ( 'NONE', *, *, #55645, .F. ) ;
#8835 = CARTESIAN_POINT ( 'NONE',  ( -73.09185868250600038, 20.27574131633382848, 69.80405428110501020 ) ) ;
#8836 = CARTESIAN_POINT ( 'NONE',  ( -167.9853834315979668, 81.58767916550898747, 70.65234695604632975 ) ) ;
#8837 = ORIENTED_EDGE ( 'NONE', *, *, #39272, .T. ) ;
#8838 = EDGE_LOOP ( 'NONE', ( #21577, #35325, #6890, #57481 ) ) ;
#8839 = CARTESIAN_POINT ( 'NONE',  ( -156.8764584803562343, 70.69066846313525332, 36.79685793462269316 ) ) ;
#8840 = FACE_OUTER_BOUND ( 'NONE', #4065, .T. ) ;
#8841 = CARTESIAN_POINT ( 'NONE',  ( 173.9288990958750105, 71.66475105971929338, -14.55843106041742629 ) ) ;
#8842 = CARTESIAN_POINT ( 'NONE',  ( 105.4376736768159049, 27.81988511842609668, 58.19221132259757212 ) ) ;
#8843 = CARTESIAN_POINT ( 'NONE',  ( -34.29440389294403246, -17.09499999999999886, 4.000000000000000000 ) ) ;
#8844 = EDGE_CURVE ( 'NONE', #3228, #2336, #27679, .T. ) ;
#8845 = CARTESIAN_POINT ( 'NONE',  ( 56.28782924480459116, 12.23883190161851786, -13.02440547745225707 ) ) ;
#8846 = ORIENTED_EDGE ( 'NONE', *, *, #61382, .T. ) ;
#8847 = PLANE ( 'NONE',  #53612 ) ;
#8848 = ORIENTED_EDGE ( 'NONE', *, *, #7474, .T. ) ;
#8849 = DIRECTION ( 'NONE',  ( 1.000000000000000000, 0.000000000000000000, 0.000000000000000000 ) ) ;
#8850 = CARTESIAN_POINT ( 'NONE',  ( -2.775557561562891351E-14, 3.000000000000030198, -50.00000000000000000 ) ) ;
#8851 = CARTESIAN_POINT ( 'NONE',  ( 206.2980740120524672, 108.5619562183279641, 29.36932263840130375 ) ) ;
#8852 = FACE_BOUND ( 'NONE', #64846, .T. ) ;
#8853 = ORIENTED_EDGE ( 'NONE', *, *, #16274, .T. ) ;
#8854 = CIRCLE ( 'NONE', #68399, 65.36598343705435354 ) ;
#8855 = ORIENTED_EDGE ( 'NONE', *, *, #12862, .F. ) ;
#8856 = DIRECTION ( 'NONE',  ( -1.000000000000000000, -1.387778780781446415E-16, 0.000000000000000000 ) ) ;
#8857 = CARTESIAN_POINT ( 'NONE',  ( -131.1743031487010285, 51.29764465557688879, 86.47423539255719049 ) ) ;
#8858 = CARTESIAN_POINT ( 'NONE',  ( 31.90247004928963648, 8.563336936370813390, -70.46775824028989632 ) ) ;
#8859 = DIRECTION ( 'NONE',  ( 0.7071067811865474617, 0.000000000000000000, -0.7071067811865474617 ) ) ;
#8860 = CARTESIAN_POINT ( 'NONE',  ( 9.319975126229035567, 6.379801983805998944, 94.99999999999866418 ) ) ;
#8861 = CARTESIAN_POINT ( 'NONE',  ( 23.27050824778650551, 7.863710279203344200, 90.59102996714455003 ) ) ;
#8862 = VECTOR ( 'NONE', #2836, 1000.000000000000000 ) ;
#8863 = VERTEX_POINT ( 'NONE', #23623 ) ;
#8864 = PLANE ( 'NONE',  #51684 ) ;
#8865 = CARTESIAN_POINT ( 'NONE',  ( 200.8383807319521281, 102.8517715783673481, -50.27105883604635039 ) ) ;
#8866 = VERTEX_POINT ( 'NONE', #1117 ) ;
#8867 = CYLINDRICAL_SURFACE ( 'NONE', #58691, 7.500000000000013323 ) ;
#8868 = ORIENTED_EDGE ( 'NONE', *, *, #31433, .F. ) ;
#8869 = LINE ( 'NONE', #24002, #26390 ) ;
#8870 = CARTESIAN_POINT ( 'NONE',  ( -94.87734348028330089, 30.28727895192195874, -95.00000000000133582 ) ) ;
#8871 = ORIENTED_EDGE ( 'NONE', *, *, #4195, .T. ) ;
#8872 = VERTEX_POINT ( 'NONE', #6735 ) ;
#8873 = CARTESIAN_POINT ( 'NONE',  ( 46.80475532923156834, 10.50744084852536986, 63.02981851721033024 ) ) ;
#8874 = CARTESIAN_POINT ( 'NONE',  ( -103.1197975032058878, 34.34092642966945874, -88.74784833587132482 ) ) ;
#8875 = DIRECTION ( 'NONE',  ( 1.000000000000000000, 0.000000000000000000, 0.000000000000000000 ) ) ;
#8876 = VERTEX_POINT ( 'NONE', #49991 ) ;
#8877 = EDGE_CURVE ( 'NONE', #54100, #15138, #40142, .T. ) ;
#8878 = B_SPLINE_CURVE_WITH_KNOTS ( 'NONE', 3,
 ( #59101, #56178, #27436, #32728, #64381, #59787, #40003, #721, #48873, #22172, #32387, #29445, #11257, #38345, #37647, #1410, #16545, #10913, #11966, #33078, #43613, #48525, #43257, #34742, #22517, #16883, #50907, #22867, #61460, #17594, #44313, #358, #64740, #65084, #28135, #11602, #7993, #43958, #37999, #54506, #6339, #2722, #27793, #54155, #16196 ),
 .UNSPECIFIED., .F., .F.,
 ( 4, 2, 2, 2, 2, 2, 2, 2, 2, 2, 2, 1, 2, 2, 2, 2, 2, 2, 2, 2, 2, 2, 4 ),
 ( 1.430489624538199204E-17, 0.001502898956853370750, 0.002254348435280047452, 0.003005797913706724153, 0.004508696870560113118, 0.005260146348986827550, 0.006011595827413541114, 0.007514494784267002070, 0.009017393741120462158, 0.01052029269797392398, 0.01127174217640064882, 0.01202319165482737540, 0.01277464113325410371, 0.01352609061168082681, 0.01502898956853427649, 0.01578043904696100133, 0.01653188852538772097, 0.01803478748224116718, 0.01953768643909460992, 0.02028913591752133302, 0.02104058539594805613, 0.02254348435280153704, 0.02404638330965502141 ),
 .UNSPECIFIED. ) ;
#8879 = CARTESIAN_POINT ( 'NONE',  ( -23.95473360498494131, 8.482091576176225445, 90.59507644628696710 ) ) ;
#8880 = CARTESIAN_POINT ( 'NONE',  ( -54.08488990389049889, 15.46443908526321209, 3.519856692167697254 ) ) ;
#8881 = CARTESIAN_POINT ( 'NONE',  ( -125.8938041572051389, 47.69968343338780414, -8.069153307770243089 ) ) ;
#8882 = CARTESIAN_POINT ( 'NONE',  ( 104.3931729003986959, 26.26823401847090267, -38.70273746882388366 ) ) ;
#8883 = CARTESIAN_POINT ( 'NONE',  ( -30.47069031368415537, 9.433993659086574723, 30.26315491089761167 ) ) ;
#8884 = CARTESIAN_POINT ( 'NONE',  ( -167.9527981889698651, 83.01270690821465337, -90.44578552921110770 ) ) ;
#8885 = ORIENTED_EDGE ( 'NONE', *, *, #56327, .F. ) ;
#8886 = ORIENTED_EDGE ( 'NONE', *, *, #51955, .F. ) ;
#8887 = DIRECTION ( 'NONE',  ( -1.850169831522831466E-16, 1.000000000000000000, 1.110223024625156294E-16 ) ) ;
#8888 = DIRECTION ( 'NONE',  ( -0.000000000000000000, -0.000000000000000000, -1.000000000000000000 ) ) ;
#8889 = LINE ( 'NONE', #67635, #35685 ) ;
#8890 = DIRECTION ( 'NONE',  ( -1.110223024625156047E-16, -1.000000000000000000, -1.110223024625155678E-16 ) ) ;
#8891 = CARTESIAN_POINT ( 'NONE',  ( 130.3245512970360664, 39.33195360491887271, 16.79886750242043902 ) ) ;
#8892 = CARTESIAN_POINT ( 'NONE',  ( -59.89379335984659747, -45.06047301136921135, 41.38025477438755928 ) ) ;
#8893 = CARTESIAN_POINT ( 'NONE',  ( 198.3763953778758093, 99.67840569793540340, 86.34231611871854284 ) ) ;
#8894 = EDGE_CURVE ( 'NONE', #35154, #57513, #7446, .T. ) ;
#8895 = CARTESIAN_POINT ( 'NONE',  ( 211.3710169359753479, 117.8057917113659130, 33.27347547697646490 ) ) ;
#8896 = CARTESIAN_POINT ( 'NONE',  ( -83.51110947562233378, 25.31252704029285638, 59.03229609086976382 ) ) ;
#8897 = DIRECTION ( 'NONE',  ( -0.8118923937861950435, -0.5838071093367415143, 0.000000000000000000 ) ) ;
#8898 = ORIENTED_EDGE ( 'NONE', *, *, #15653, .T. ) ;
#8899 = CARTESIAN_POINT ( 'NONE',  ( 437.3372781065086201, 0.000000000000000000, 103.5502958579881749 ) ) ;
#8900 = ORIENTED_EDGE ( 'NONE', *, *, #31356, .F. ) ;
#8901 = CARTESIAN_POINT ( 'NONE',  ( 200.8298320869469933, 101.1869877914232916, -23.42140642344036650 ) ) ;
#8902 = ORIENTED_EDGE ( 'NONE', *, *, #22144, .F. ) ;
#8903 = AXIS2_PLACEMENT_3D ( 'NONE', #51006, #2815, #24279 ) ;
#8904 = DIRECTION ( 'NONE',  ( 1.000000000000000000, 0.000000000000000000, 0.000000000000000000 ) ) ;
#8905 = CARTESIAN_POINT ( 'NONE',  ( 187.0788993276711949, 86.37277723143235164, -75.08339630570569057 ) ) ;
#8906 = CARTESIAN_POINT ( 'NONE',  ( -143.4048679855201271, 60.45763799613828127, 69.43254532525401146 ) ) ;
#8907 = EDGE_CURVE ( 'NONE', #56288, #17657, #66059, .T. ) ;
#8908 = CARTESIAN_POINT ( 'NONE',  ( -125.8938041572051389, -170.0000000000000000, 64.96449846362078517 ) ) ;
#8909 = B_SPLINE_CURVE_WITH_KNOTS ( 'NONE', 3,
 ( #5850, #33655, #6562, #587, #48750, #60010, #938, #38929, #22038, #6205, #51124, #28359, #44174, #49805, #1631, #65663, #49451, #2939, #43484, #56394, #33307, #37875, #8214, #12192, #29664, #17451, #11831, #24402, #64961, #59321, #11133, #32597, #54022, #59655, #27657, #22386, #51476, #68672, #35293, #46527, #30016, #36328, #52503, #30361 ),
 .UNSPECIFIED., .F., .F.,
 ( 4, 2, 2, 2, 2, 2, 2, 2, 2, 2, 2, 2, 2, 2, 2, 2, 2, 2, 2, 2, 2, 4 ),
 ( 7.949501638480626889E-18, 0.001473754749730506707, 0.002210632124595751820, 0.002947509499460997367, 0.004421264249191475017, 0.005895018998921953100, 0.007368773748652430317, 0.008105651123517666756, 0.008842528498382903196, 0.01031628324811337781, 0.01179003799784384895, 0.01252691537270908366, 0.01326379274757431663, 0.01473754749730477737, 0.01547442487217000860, 0.01621130224703523984, 0.01768505699676569884, 0.01915881174649616478, 0.01989568912136139428, 0.02063256649622662725, 0.02210632124595709666, 0.02358007599568756260 ),
 .UNSPECIFIED. ) ;
#8910 = VECTOR ( 'NONE', #60487, 1000.000000000000000 ) ;
#8911 = CARTESIAN_POINT ( 'NONE',  ( 39.40195752203892710, 8.409560354027394879, -50.61981746542779348 ) ) ;
#8912 = CARTESIAN_POINT ( 'NONE',  ( -105.4589068214113894, 34.42476264325675572, 4.365203437741908665 ) ) ;
#8913 = CARTESIAN_POINT ( 'NONE',  ( 12.04188192036245297, 7.416006018508746855, -49.52083859284432776 ) ) ;
#8914 = CARTESIAN_POINT ( 'NONE',  ( 126.3580543567275356, 37.07735301062816546, -43.21940575724328681 ) ) ;
#8915 = ORIENTED_EDGE ( 'NONE', *, *, #39313, .F. ) ;
#8916 = ORIENTED_EDGE ( 'NONE', *, *, #6659, .T. ) ;
#8917 = CARTESIAN_POINT ( 'NONE',  ( 187.1611749077166564, 86.46285392389889068, 86.08845492538941357 ) ) ;
#8918 = CARTESIAN_POINT ( 'NONE',  ( -55.15976438495157197, 34.41253982194030669, 170.0000000000000000 ) ) ;
#8919 = CARTESIAN_POINT ( 'NONE',  ( -23.98903001682803193, 8.486614814224626713, -70.65595771900279942 ) ) ;
#8920 = EDGE_CURVE ( 'NONE', #29802, #46252, #28182, .T. ) ;
#8921 = AXIS2_PLACEMENT_3D ( 'NONE', #60437, #34420, #651 ) ;
#8922 = ADVANCED_FACE ( 'NONE', ( #49633 ), #65845, .T. ) ;
#8923 = CARTESIAN_POINT ( 'NONE',  ( 7.347880794884118356E-15, 70.00000000000000000, 60.00000000000000000 ) ) ;
#8924 = ADVANCED_FACE ( 'NONE', ( #1461 ), #22916, .T. ) ;
#8925 = CARTESIAN_POINT ( 'NONE',  ( 284.8388692023054887, 21.96385131419673442, -1.300671796277831582 ) ) ;
#8926 = CARTESIAN_POINT ( 'NONE',  ( 65.78600657349682024, 10.66798394579848619, 34.48241795236667429 ) ) ;
#8927 = CARTESIAN_POINT ( 'NONE',  ( 173.7227242028391458, 71.47307702680409136, -72.03415706586312695 ) ) ;
#8928 =( NAMED_UNIT ( * ) SI_UNIT ( $, .STERADIAN. ) SOLID_ANGLE_UNIT ( ) );
#8929 = CARTESIAN_POINT ( 'NONE',  ( 276.9483136162804726, -21.63883973695289242, 3.974316929722018443 ) ) ;
#8930 = CARTESIAN_POINT ( 'NONE',  ( 88.98408042523107042, 20.23787745328939636, -23.60181295827505110 ) ) ;
#8931 = CARTESIAN_POINT ( 'NONE',  ( -24.95010104166214049, 9.631487977190598571, 68.32982050694094767 ) ) ;
#8932 = CARTESIAN_POINT ( 'NONE',  ( 107.7789859651022226, 21.53699436807883671, 4.491592093615980552 ) ) ;
#8933 = LINE ( 'NONE', #2612, #15335 ) ;
#8934 = CARTESIAN_POINT ( 'NONE',  ( -101.4457769059400931, 32.35908584109303376, -88.74728229414131420 ) ) ;
#8935 = ORIENTED_EDGE ( 'NONE', *, *, #27892, .T. ) ;
#8936 = DIRECTION ( 'NONE',  ( -1.000000000000000000, 0.000000000000000000, 0.000000000000000000 ) ) ;
#8937 = CARTESIAN_POINT ( 'NONE',  ( 149.9883446984744921, 53.30011109831377070, 63.16626985724861498 ) ) ;
#8938 = FACE_OUTER_BOUND ( 'NONE', #37569, .T. ) ;
#8939 = CARTESIAN_POINT ( 'NONE',  ( -50.51700111023805562, 13.51182830536853352, -36.72324871123618806 ) ) ;
#8940 = FACE_BOUND ( 'NONE', #15808, .T. ) ;
#8941 = DIRECTION ( 'NONE',  ( 1.000000000000000000, -0.000000000000000000, -0.000000000000000000 ) ) ;
#8942 = ORIENTED_EDGE ( 'NONE', *, *, #554, .F. ) ;
#8943 = SURFACE_STYLE_FILL_AREA ( #57135 ) ;
#8944 = CARTESIAN_POINT ( 'NONE',  ( -783.0172411895269988, -622.0000000000060254, 10.00000000000000000 ) ) ;
#8945 = ORIENTED_EDGE ( 'NONE', *, *, #65993, .T. ) ;
#8946 = ORIENTED_EDGE ( 'NONE', *, *, #40571, .F. ) ;
#8947 = CARTESIAN_POINT ( 'NONE',  ( 60.40479419793796012, -24.00543350795314979, 170.0000000000000000 ) ) ;
#8948 = LINE ( 'NONE', #25823, #51250 ) ;
#8949 = DIRECTION ( 'NONE',  ( 0.000000000000000000, 0.000000000000000000, 1.000000000000000000 ) ) ;
#8950 = B_SPLINE_CURVE_WITH_KNOTS ( 'NONE', 3,
 ( #52359, #25642, #47073, #68537, #15069, #57982, #9799, #68862, #20686, #32628, #38598, #26659, #258, #28039, #31942, #53370, #60040, #5205, #27338, #17122, #16451, #54762, #11858, #37204, #22418, #21375, #33337, #48426, #48096, #59685, #6592, #37552, #32287, #49479, #48776, #58651, #11497, #10472, #1312, #64991, #63946, #65334, #22764, #615, #11162, #53721, #43512, #54054 ),
 .UNSPECIFIED., .F., .F.,
 ( 4, 2, 2, 2, 2, 2, 2, 2, 2, 2, 2, 2, 2, 2, 2, 2, 2, 2, 2, 2, 2, 2, 2, 4 ),
 ( 0.02554216173022672010, 0.02715505844859240903, 0.02796150680777522574, 0.02876795516695804245, 0.03038085188532362729, 0.03199374860368921214, 0.03360664532205479699, 0.03441309368123757900, 0.03521954204042036102, 0.03602599039960314303, 0.03683243875878592505, 0.03844533547715150990, 0.03925178383633430579, 0.04005823219551710862, 0.04086468055469991145, 0.04167112891388270735, 0.04247757727306551712, 0.04328402563224831301, 0.04489692235061395337, 0.04650981906897959373, 0.04731626742816241737, 0.04812271578734524102, 0.04973561250571082587, 0.05134850922407641072 ),
 .UNSPECIFIED. ) ;
#8951 = ORIENTED_EDGE ( 'NONE', *, *, #3648, .F. ) ;
#8952 = PLANE ( 'NONE',  #21090 ) ;
#8953 = VECTOR ( 'NONE', #7588, 1000.000000000000000 ) ;
#8954 = DIRECTION ( 'NONE',  ( 1.000000000000000000, 0.000000000000000000, 0.000000000000000000 ) ) ;
#8955 = LINE ( 'NONE', #2297, #1634 ) ;
#8956 = CARTESIAN_POINT ( 'NONE',  ( 62.53356220515463093, 13.59349015304564823, -50.72069083216976537 ) ) ;
#8957 = FACE_OUTER_BOUND ( 'NONE', #20268, .T. ) ;
#8958 = CIRCLE ( 'NONE', #24679, 246.3582898394606957 ) ;
#8959 = CARTESIAN_POINT ( 'NONE',  ( -28.35957743809534648, 10.12373109553627692, -22.81564308554694165 ) ) ;
#8960 = CARTESIAN_POINT ( 'NONE',  ( 138.6020257460769187, 44.36414356192209851, 15.99390124636234845 ) ) ;
#8961 = EDGE_CURVE ( 'NONE', #25778, #4257, #37775, .T. ) ;
#8962 = ORIENTED_EDGE ( 'NONE', *, *, #15500, .F. ) ;
#8963 = EDGE_CURVE ( 'NONE', #52465, #37055, #66205, .T. ) ;
#8964 = CARTESIAN_POINT ( 'NONE',  ( -7.825402957745083654, 6.891034867348166948, -77.26262132240753999 ) ) ;
#8965 = DIRECTION ( 'NONE',  ( -1.000000000000000000, -0.000000000000000000, -0.000000000000000000 ) ) ;
#8966 = CARTESIAN_POINT ( 'NONE',  ( 50.98853755884157124, 395.0000000000065938, -133.9497041420122798 ) ) ;
#8968 = VERTEX_POINT ( 'NONE', #60893 ) ;
#8967 = DIRECTION ( 'NONE',  ( 0.000000000000000000, 1.000000000000000000, -0.000000000000000000 ) ) ;
#8970 = CARTESIAN_POINT ( 'NONE',  ( 417.3372781065085633, 395.0000000000000568, -146.4497041420118535 ) ) ;
#8969 = B_SPLINE_CURVE_WITH_KNOTS ( 'NONE', 3,
 ( #30483, #62846, #52617, #62502, #19226, #24531, #4104, #45969, #40681, #35771, #67434, #68464, #41730, #41392, #62140, #36452, #13957, #56883, #8696, #3407, #57566, #25221, #14648, #25566, #36111, #9376, #42068, #32214, #26925, #10060, #69483, #59609, #5121, #15684, #58925, #37132, #21302, #59271 ),
 .UNSPECIFIED., .F., .F.,
 ( 4, 2, 2, 2, 2, 2, 2, 2, 2, 2, 2, 2, 2, 2, 2, 2, 2, 2, 4 ),
 ( 0.02546424207107601118, 0.02703543426729225485, 0.02782103036540034199, 0.02860662646350842914, 0.03017781865972465893, 0.03174901085594088873, 0.03332020305215711159, 0.03489139524837334139, 0.03646258744458957118, 0.03724818354269765486, 0.03803377964080574547, 0.03881937573891382914, 0.03960497183702191282, 0.04117616403323804547, 0.04274735622945417812, 0.04431854842567031078, 0.04588974062188644343, 0.04746093281810256914, 0.05060331721053484832 ),
 .UNSPECIFIED. ) ;
#8971 = ORIENTED_EDGE ( 'NONE', *, *, #29550, .F. ) ;
#8972 = AXIS2_PLACEMENT_3D ( 'NONE', #69350, #749, #59475 ) ;
#8973 = VERTEX_POINT ( 'NONE', #9512 ) ;
#8974 = DIRECTION ( 'NONE',  ( 0.000000000000000000, 1.000000000000000000, -0.000000000000000000 ) ) ;
#8975 = CARTESIAN_POINT ( 'NONE',  ( -4.999999999999922728, 51.66904755831208718, 2.000000000000001776 ) ) ;
#8976 = CARTESIAN_POINT ( 'NONE',  ( 200.4600337307566349, 100.7087439352121265, -64.46507461282644158 ) ) ;
#8977 = EDGE_CURVE ( 'NONE', #13387, #65364, #57015, .T. ) ;
#8978 = DIRECTION ( 'NONE',  ( -0.8805955318567322276, -0.4738686624730095165, 5.102127870520022769E-18 ) ) ;
#8979 = EDGE_CURVE ( 'NONE', #36166, #52636, #64744, .T. ) ;
#8980 = CARTESIAN_POINT ( 'NONE',  ( 11.98601804829806561, 14.28438006995821219, -38.01398195170192906 ) ) ;
#8981 = LINE ( 'NONE', #30429, #43221 ) ;
#8982 = DIRECTION ( 'NONE',  ( 0.000000000000000000, 0.000000000000000000, -1.000000000000000000 ) ) ;
#8983 = CARTESIAN_POINT ( 'NONE',  ( -155.1302201283145905, 69.09929365814134883, -37.34342092834704374 ) ) ;
#8984 = VERTEX_POINT ( 'NONE', #30283 ) ;
#8985 =( REPRESENTATION_RELATIONSHIP ('NONE','NONE', #40274, #60409 ) REPRESENTATION_RELATIONSHIP_WITH_TRANSFORMATION ( #58118 )SHAPE_REPRESENTATION_RELATIONSHIP( ) );
#8986 = ORIENTED_EDGE ( 'NONE', *, *, #28519, .F. ) ;
#8987 = ADVANCED_FACE ( 'NONE', ( #56661 ), #46441, .F. ) ;
#8988 = CARTESIAN_POINT ( 'NONE',  ( -108.5248383251030049, 37.21456094989613916, 7.013330406097838754 ) ) ;
#8989 = CARTESIAN_POINT ( 'NONE',  ( 102.7425154123292685, 25.56407025871218863, 63.71405795841012321 ) ) ;
#8990 = CARTESIAN_POINT ( 'NONE',  ( 110.9409838438198932, 29.20603643730970944, 83.32602672627702134 ) ) ;
#8991 = ADVANCED_FACE ( 'NONE', ( #8481 ), #3537, .T. ) ;
#8992 = AXIS2_PLACEMENT_3D ( 'NONE', #40810, #34519, #67555 ) ;
#8993 = DIRECTION ( 'NONE',  ( 0.000000000000000000, 0.000000000000000000, 1.000000000000000000 ) ) ;
#8994 = DIRECTION ( 'NONE',  ( 0.000000000000000000, -1.000000000000000000, 0.000000000000000000 ) ) ;
#8995 = DIRECTION ( 'NONE',  ( 0.000000000000000000, 0.000000000000000000, -1.000000000000000000 ) ) ;
#8996 = CARTESIAN_POINT ( 'NONE',  ( -143.4445817893553112, 60.48932258267372220, 87.48363363319201369 ) ) ;
#8997 = VERTEX_POINT ( 'NONE', #19721 ) ;
#8998 = ORIENTED_EDGE ( 'NONE', *, *, #12701, .T. ) ;
#8999 = EDGE_LOOP ( 'NONE', ( #25995, #54804, #2071, #22165 ) ) ;
#9000 = B_SPLINE_CURVE_WITH_KNOTS ( 'NONE', 3,
 ( #64060, #68980, #26089, #15872 ),
 .UNSPECIFIED., .F., .F.,
 ( 4, 4 ),
 ( 9.900409499073836656E-07, 0.05658314289920116785 ),
 .UNSPECIFIED. ) ;
#9001 = DIRECTION ( 'NONE',  ( 0.000000000000000000, -1.000000000000000000, 0.000000000000000000 ) ) ;
#9002 = CARTESIAN_POINT ( 'NONE',  ( -81.90020664963797969, 23.57971581008655804, 57.99140405555259292 ) ) ;
#9003 = CARTESIAN_POINT ( 'NONE',  ( 70.50372867914784081, 14.53505678900967446, -42.73019894926635232 ) ) ;
#9004 = CARTESIAN_POINT ( 'NONE',  ( 105.5292268913834448, 26.76134294421019177, -91.26444993491544722 ) ) ;
#9005 = EDGE_CURVE ( 'NONE', #41100, #30857, #37489, .T. ) ;
#9006 = CARTESIAN_POINT ( 'NONE',  ( -59.58556642339447507, 16.99097764963621771, 43.81259177720935583 ) ) ;
#9007 = CARTESIAN_POINT ( 'NONE',  ( -34.74023699876256899, 11.17830703027883388, -76.41366003997089251 ) ) ;
#9008 = EDGE_CURVE ( 'NONE', #51470, #61262, #35530, .T. ) ;
#9009 = EDGE_CURVE ( 'NONE', #33511, #39615, #42211, .T. ) ;
#9010 = VECTOR ( 'NONE', #54598, 1000.000000000000000 ) ;
#9011 = ADVANCED_FACE ( 'NONE', ( #37261 ), #26724, .F. ) ;
#9012 = CARTESIAN_POINT ( 'NONE',  ( 38.91493890549799062, 8.346224043800608783, 56.75838489642698192 ) ) ;
#9013 = CARTESIAN_POINT ( 'NONE',  ( 13.84120792123768773, 6.445822122644895735, -23.43379455737267136 ) ) ;
#9014 = VERTEX_POINT ( 'NONE', #36937 ) ;
#9015 = CARTESIAN_POINT ( 'NONE',  ( -4.070918861171934466, 6.675509947362631813, -36.42082469883077067 ) ) ;
#9016 = CARTESIAN_POINT ( 'NONE',  ( 56.48035995027075273, 49.34540444547854321, 0.000000000000000000 ) ) ;
#9017 = CARTESIAN_POINT ( 'NONE',  ( -118.7011677090246735, 41.93687969120206560, 9.134074366734774131 ) ) ;
#9018 = CARTESIAN_POINT ( 'NONE',  ( 429.8372781065087906, 395.0000000000066507, -128.9497041420121093 ) ) ;
#9019 = DIRECTION ( 'NONE',  ( 1.000000000000000000, 0.000000000000000000, 0.000000000000000000 ) ) ;
#9020 = CARTESIAN_POINT ( 'NONE',  ( 22.28700331106867694, 7.803633676228380445, -12.42248016224392693 ) ) ;
#9021 = CARTESIAN_POINT ( 'NONE',  ( 12.04188192036245120, 7.416006018508747744, 4.168262588083034181 ) ) ;
#9022 = EDGE_LOOP ( 'NONE', ( #61019, #60838, #58387, #58725 ) ) ;
#9023 = PRODUCT_CONTEXT ( 'NONE', #45341, 'mechanical' ) ;
#9024 = VECTOR ( 'NONE', #36147, 1000.000000000000114 ) ;
#9025 = CARTESIAN_POINT ( 'NONE',  ( -36.11269837220809364, -15.55634918610397754, 2.000000000000000000 ) ) ;
#9026 = DIRECTION ( 'NONE',  ( -0.000000000000000000, -0.000000000000000000, 1.000000000000000000 ) ) ;
#9027 = CARTESIAN_POINT ( 'NONE',  ( -40.27405704175634327, 63.28161525591265502, 43.58025477438756212 ) ) ;
#9028 = DIRECTION ( 'NONE',  ( 0.000000000000000000, 0.000000000000000000, 1.000000000000000000 ) ) ;
#9029 = VERTEX_POINT ( 'NONE', #10880 ) ;
#9030 = ORIENTED_EDGE ( 'NONE', *, *, #32388, .F. ) ;
#9031 = CARTESIAN_POINT ( 'NONE',  ( -148.6409722988649946, 63.44808865916660778, -8.015346559020745332 ) ) ;
#9032 = DIRECTION ( 'NONE',  ( 1.000000000000000000, 0.000000000000000000, -0.000000000000000000 ) ) ;
#9033 = VERTEX_POINT ( 'NONE', #58713 ) ;
#9034 = CARTESIAN_POINT ( 'NONE',  ( 153.4899842167529869, 55.87722776145639614, 84.23368635199832966 ) ) ;
#9035 = VERTEX_POINT ( 'NONE', #5598 ) ;
#9036 = CARTESIAN_POINT ( 'NONE',  ( -56.73868929054668797, 16.18382781951277138, 18.28487575996624415 ) ) ;
#9037 = CARTESIAN_POINT ( 'NONE',  ( 0.000000000000000000, -31.50328976398030534, 5.000000000000000000 ) ) ;
#9038 = CARTESIAN_POINT ( 'NONE',  ( -155.7457403566965297, 71.01814553754118720, 34.02709316248113680 ) ) ;
#9039 = VECTOR ( 'NONE', #68090, 1000.000000000000000 ) ;
#9040 = CARTESIAN_POINT ( 'NONE',  ( -96.02415295709703003, 29.71480036090584775, 33.87477838304790367 ) ) ;
#9041 = LINE ( 'NONE', #35424, #38372 ) ;
#9043 = ORIENTED_EDGE ( 'NONE', *, *, #56787, .F. ) ;
#9042 = CARTESIAN_POINT ( 'NONE',  ( 26.11269837220812562, 36.11269837220800838, 0.000000000000000000 ) ) ;
#9044 = CARTESIAN_POINT ( 'NONE',  ( 5.694488383565878387, -51.35054909896783215, 26.66469104408690427 ) ) ;
#9045 = EDGE_LOOP ( 'NONE', ( #5242, #53942, #39507, #50271 ) ) ;
#9046 = ORIENTED_EDGE ( 'NONE', *, *, #49061, .F. ) ;
#9048 = ADVANCED_FACE ( 'NONE', ( #9864 ), #27052, .F. ) ;
#9047 = CARTESIAN_POINT ( 'NONE',  ( 174.6307688320643194, 73.70327352127000609, 32.97779385060549373 ) ) ;
#9049 = CARTESIAN_POINT ( 'NONE',  ( 17.74393407086869701, 6.570779001277776921, -62.60608148900111303 ) ) ;
#9051 = ORIENTED_EDGE ( 'NONE', *, *, #61156, .T. ) ;
#9050 = CARTESIAN_POINT ( 'NONE',  ( -126.3495878770405909, 48.00153794568855403, 72.46449846362078517 ) ) ;
#9052 = PLANE ( 'NONE',  #27410 ) ;
#9053 = FACE_BOUND ( 'NONE', #5303, .T. ) ;
#9054 = ORIENTED_EDGE ( 'NONE', *, *, #40444, .T. ) ;
#9055 = CARTESIAN_POINT ( 'NONE',  ( 48.39383208188445451, -43.94028683479019293, 6.377659838150144402E-18 ) ) ;
#9056 = EDGE_CURVE ( 'NONE', #28933, #68971, #64345, .T. ) ;
#9057 = CARTESIAN_POINT ( 'NONE',  ( 136.1215428813736708, 43.99260314811116501, 29.84553875828433078 ) ) ;
#9058 = CARTESIAN_POINT ( 'NONE',  ( 10.01137213834874196, 64.59476928204604462, 41.38025477438755928 ) ) ;
#9059 = CARTESIAN_POINT ( 'NONE',  ( -129.4036885357273547, 50.06837984316182855, 17.90749390567040678 ) ) ;
#9060 = CARTESIAN_POINT ( 'NONE',  ( 68.94309019697858787, 15.16533147648752156, -65.44371665737369881 ) ) ;
#9061 = ORIENTED_EDGE ( 'NONE', *, *, #49882, .T. ) ;
#9062 = EDGE_CURVE ( 'NONE', #45314, #39145, #32351, .T. ) ;
#9063 = ORIENTED_EDGE ( 'NONE', *, *, #50367, .F. ) ;
#9064 = VECTOR ( 'NONE', #16328, 1000.000000000000227 ) ;
#9065 = CARTESIAN_POINT ( 'NONE',  ( -142.9756886485677398, 60.11539876121631920, -19.16347302773874262 ) ) ;
#9066 = CARTESIAN_POINT ( 'NONE',  ( 121.4242852856285566, 6.000000000000000000, -20.00000000000000000 ) ) ;
#9067 = DIRECTION ( 'NONE',  ( -0.8160245890732938934, -0.5780171883497599028, 0.000000000000000000 ) ) ;
#9068 = CARTESIAN_POINT ( 'NONE',  ( -54.84008385043469502, 14.62454595683343150, -88.90542517938720835 ) ) ;
#9069 = CARTESIAN_POINT ( 'NONE',  ( -52.73319225379935205, 53.34578647582052469, 170.0000000000000000 ) ) ;
#9070 = CARTESIAN_POINT ( 'NONE',  ( -49.77357484059193382, 41.82599373102802787, 170.0000000000000000 ) ) ;
#9071 = CARTESIAN_POINT ( 'NONE',  ( 70.12389542974193546, 15.47520081968151651, -45.66377706524675517 ) ) ;
#9072 = DIRECTION ( 'NONE',  ( 4.691548276051942630E-18, 2.005263967813518922E-18, -1.000000000000000000 ) ) ;
#9073 = CARTESIAN_POINT ( 'NONE',  ( -166.7049310409072405, 80.25944422923579680, -65.16385208324180667 ) ) ;
#9074 = PRODUCT_DEFINITION_SHAPE ( 'NONE', 'NONE',  #55565 ) ;
#9075 = ORIENTED_EDGE ( 'NONE', *, *, #10851, .F. ) ;
#9076 = CYLINDRICAL_SURFACE ( 'NONE', #5198, 7.500000000000020428 ) ;
#9077 = ORIENTED_EDGE ( 'NONE', *, *, #25580, .F. ) ;
#9078 = VECTOR ( 'NONE', #44320, 1000.000000000000000 ) ;
#9079 = CARTESIAN_POINT ( 'NONE',  ( 81.49482595366482940, 18.78720120198666166, -91.48285567191722123 ) ) ;
#9080 = CARTESIAN_POINT ( 'NONE',  ( 82.12277968641508608, 18.98848723477814460, 70.07157773562504133 ) ) ;
#9081 = VERTEX_POINT ( 'NONE', #5940 ) ;
#9082 = DIRECTION ( 'NONE',  ( 0.4887922226926450509, 0.000000000000000000, -0.8724002309921654597 ) ) ;
#9083 = LINE ( 'NONE', #68181, #56913 ) ;
#9084 = CARTESIAN_POINT ( 'NONE',  ( 39.40195752203892710, 9.424259417798131366, 3.069283715499574239 ) ) ;
#9085 = DIRECTION ( 'NONE',  ( 0.000000000000000000, 0.000000000000000000, -1.000000000000000000 ) ) ;
#9086 = CARTESIAN_POINT ( 'NONE',  ( 32.29989959354728768, 7.591763852038297067, 12.99235193929992072 ) ) ;
#9087 = DIRECTION ( 'NONE',  ( 0.000000000000000000, 0.000000000000000000, 1.000000000000000000 ) ) ;
#9088 = AXIS2_PLACEMENT_3D ( 'NONE', #64615, #16427, #5182 ) ;
#9089 = DIRECTION ( 'NONE',  ( 1.000000000000000000, -0.000000000000000000, 0.000000000000000000 ) ) ;
#9090 = ADVANCED_FACE ( 'NONE', ( #32004 ), #53776, .F. ) ;
#9091 = ORIENTED_EDGE ( 'NONE', *, *, #1996, .T. ) ;
#9092 = CARTESIAN_POINT ( 'NONE',  ( -119.1961424429667034, 43.42002938933726597, -92.69538835324019033 ) ) ;
#9093 = ORIENTED_EDGE ( 'NONE', *, *, #15435, .F. ) ;
#9094 = PLANE ( 'NONE',  #68854 ) ;
#9095 = CARTESIAN_POINT ( 'NONE',  ( -59.95412189755932530, 17.09836075175410031, 58.96417071872249238 ) ) ;
#9097 = EDGE_CURVE ( 'NONE', #27270, #54323, #13093, .T. ) ;
#9096 = CARTESIAN_POINT ( 'NONE',  ( -26.50364027666003963, 8.832969329054176200, 5.203539351318217321 ) ) ;
#9098 = DIRECTION ( 'NONE',  ( 0.000000000000000000, 0.000000000000000000, 1.000000000000000000 ) ) ;
#9099 = CARTESIAN_POINT ( 'NONE',  ( -13.47680110791658414, 7.324966777230640602, -74.71809665986256732 ) ) ;
#9100 = CARTESIAN_POINT ( 'NONE',  ( 12.93264331410902379, 21.39501663729252456, 0.000000000000000000 ) ) ;
#9101 = CARTESIAN_POINT ( 'NONE',  ( 153.8224167330182013, 56.12711234192238408, -37.06696685681204428 ) ) ;
#9102 = ORIENTED_EDGE ( 'NONE', *, *, #7493, .T. ) ;
#9103 = CARTESIAN_POINT ( 'NONE',  ( 403.0071894358293321, 1011.991584617513809, 794.0068267248735765 ) ) ;
#9104 = CARTESIAN_POINT ( 'NONE',  ( -24.51966494718099909, -5.470267094204724678, 0.000000000000000000 ) ) ;
#9105 = CARTESIAN_POINT ( 'NONE',  ( 177.7886308167536242, 76.74396398590877766, -10.12818009402780461 ) ) ;
#9106 = CARTESIAN_POINT ( 'NONE',  ( 0.000000000000000000, 0.000000000000000000, -9.500000000000000000 ) ) ;
#9107 = CARTESIAN_POINT ( 'NONE',  ( 39.40195752203892710, 8.409560354027394879, -50.61981746542779348 ) ) ;
#9108 = VERTEX_POINT ( 'NONE', #64008 ) ;
#9109 = DIRECTION ( 'NONE',  ( -0.000000000000000000, -0.000000000000000000, -1.000000000000000000 ) ) ;
#9110 = CARTESIAN_POINT ( 'NONE',  ( 126.3484241331027675, 38.22406654827073424, 90.61007899326968129 ) ) ;
#9111 = CARTESIAN_POINT ( 'NONE',  ( 204.3129818922373602, 107.5244029525888720, -24.48138044215792419 ) ) ;
#9112 = CARTESIAN_POINT ( 'NONE',  ( -122.3745688183166465, 44.21964839958061333, -62.61830058063351601 ) ) ;
#9113 = ORIENTED_EDGE ( 'NONE', *, *, #12074, .F. ) ;
#9114 = LINE ( 'NONE', #30572, #3077 ) ;
#9115 = CARTESIAN_POINT ( 'NONE',  ( 117.4696399285658686, 32.37118663718648293, -72.33972432310571321 ) ) ;
#9116 = CARTESIAN_POINT ( 'NONE',  ( 188.2962140587029864, 87.71627202537840162, 34.72967280661650591 ) ) ;
#9117 = CARTESIAN_POINT ( 'NONE',  ( 136.1215428813736992, 43.99260314811115791, 3.000988167820665353 ) ) ;
#9118 = LINE ( 'NONE', #14731, #6035 ) ;
#9119 = AXIS2_PLACEMENT_3D ( 'NONE', #29665, #68005, #56749 ) ;
#9120 = CIRCLE ( 'NONE', #67522, 200.0000000000000000 ) ;
#9121 = ORIENTED_EDGE ( 'NONE', *, *, #21343, .F. ) ;
#9122 = EDGE_CURVE ( 'NONE', #65219, #2040, #28198, .T. ) ;
#9123 = CARTESIAN_POINT ( 'NONE',  ( 181.0840389613909736, 80.03940679743416808, 56.15314469597509373 ) ) ;
#9124 = AXIS2_PLACEMENT_3D ( 'NONE', #12076, #1515, #28240 ) ;
#9125 = AXIS2_PLACEMENT_3D ( 'NONE', #27577, #1201, #49369 ) ;
#9126 = VERTEX_POINT ( 'NONE', #28099 ) ;
#9128 = ADVANCED_FACE ( 'NONE', ( #59746 ), #38661, .T. ) ;
#9127 = CARTESIAN_POINT ( 'NONE',  ( 69.35866309798979046, 15.27376159675660716, 68.16710321307755294 ) ) ;
#9129 = CARTESIAN_POINT ( 'NONE',  ( 141.1600430683898537, 46.01273571695310949, 92.44402370497088839 ) ) ;
#9131 = EDGE_LOOP ( 'NONE', ( #33787, #14223, #56092, #40351 ) ) ;
#9130 = CARTESIAN_POINT ( 'NONE',  ( 15.55634918610406103, 15.55634918610400241, 0.000000000000000000 ) ) ;
#9132 = DIRECTION ( 'NONE',  ( 0.000000000000000000, 0.000000000000000000, 1.000000000000000000 ) ) ;
#9133 = VECTOR ( 'NONE', #2916, 1000.000000000000000 ) ;
#9134 = DIRECTION ( 'NONE',  ( -0.000000000000000000, -1.000000000000000000, 0.000000000000000000 ) ) ;
#9135 = CARTESIAN_POINT ( 'NONE',  ( 113.8626313173125766, 31.71036178495293001, -36.83649234522183491 ) ) ;
#9136 = ORIENTED_EDGE ( 'NONE', *, *, #1352, .F. ) ;
#9137 = CARTESIAN_POINT ( 'NONE',  ( 12.99074365121454910, -21.50298515537749822, 3.061616997868437868E-16 ) ) ;
#9138 = EDGE_CURVE ( 'NONE', #33323, #38900, #1031, .T. ) ;
#9139 = DIRECTION ( 'NONE',  ( -0.9959742939952382912, -0.08963930890344089242, 0.000000000000000000 ) ) ;
#9140 = CARTESIAN_POINT ( 'NONE',  ( 79.91920957766410538, 18.29292522273511068, -13.08905856853260019 ) ) ;
#9141 = CARTESIAN_POINT ( 'NONE',  ( -166.2028193222419077, 79.74385139484274987, 35.41135073535578215 ) ) ;
#9142 = CARTESIAN_POINT ( 'NONE',  ( 151.3309484205705076, 53.03078371058069962, 68.06927186267586194 ) ) ;
#9143 = EDGE_CURVE ( 'NONE', #8163, #57196, #39709, .T. ) ;
#9144 = CARTESIAN_POINT ( 'NONE',  ( 266.9165763529819628, 192.0000000000000000, 108.9999999999999858 ) ) ;
#9145 = ORIENTED_EDGE ( 'NONE', *, *, #44739, .F. ) ;
#9146 = PLANE ( 'NONE',  #57921 ) ;
#9148 = EDGE_CURVE ( 'NONE', #11003, #56134, #41202, .T. ) ;
#9147 = CARTESIAN_POINT ( 'NONE',  ( -7.825402957745085430, 7.899365992529246761, 71.96013162991091860 ) ) ;
#9149 = VERTEX_POINT ( 'NONE', #44978 ) ;
#9150 = CARTESIAN_POINT ( 'NONE',  ( 150.0278556977734468, 53.32860603304212077, -15.70126343080858611 ) ) ;
#9151 = CARTESIAN_POINT ( 'NONE',  ( -62.02002361825626053, 16.66092005917081664, 88.71144110712529596 ) ) ;
#9152 = CARTESIAN_POINT ( 'NONE',  ( 108.3942953861066343, 29.14039925067522674, 29.82753592392950992 ) ) ;
#9153 = CARTESIAN_POINT ( 'NONE',  ( -84.49322488516129681, 0.000000000000000000, 43.58025477438756212 ) ) ;
#9154 = CARTESIAN_POINT ( 'NONE',  ( 56.64858667248266499, 11.28546282538443357, 87.02427806644405450 ) ) ;
#9155 = CARTESIAN_POINT ( 'NONE',  ( 187.5246323291927126, 86.86207184872516507, 13.84593183401972460 ) ) ;
#9156 = CARTESIAN_POINT ( 'NONE',  ( -442.6627218934913230, 399.9999999999997726, 103.5502958579881891 ) ) ;
#9157 = CARTESIAN_POINT ( 'NONE',  ( -173.1211646369891355, -170.0000000000000000, -15.36740657428631351 ) ) ;
#9158 = ORIENTED_EDGE ( 'NONE', *, *, #46685, .F. ) ;
#9159 = CARTESIAN_POINT ( 'NONE',  ( 6.375108774214766072E-14, 36.11269837220805812, 2.000000000000001776 ) ) ;
#9160 = VERTEX_POINT ( 'NONE', #61164 ) ;
#9161 = CARTESIAN_POINT ( 'NONE',  ( 107.0471828278920725, 27.43080724084231647, -63.46514271234853055 ) ) ;
#9162 = CARTESIAN_POINT ( 'NONE',  ( 56.66438910147189034, 11.28870326331392526, -74.06174710983880516 ) ) ;
#9163 = DIRECTION ( 'NONE',  ( 0.000000000000000000, 0.000000000000000000, -1.000000000000000000 ) ) ;
#9164 = CARTESIAN_POINT ( 'NONE',  ( -0.4198266561544487518, 6.521779739161982725, 89.94873814021600822 ) ) ;
#9165 = VECTOR ( 'NONE', #61009, 1000.000000000000114 ) ;
#9166 = CARTESIAN_POINT ( 'NONE',  ( -109.4995148930278646, 37.75156937139181679, -17.76878308378839932 ) ) ;
#9167 = ORIENTED_EDGE ( 'NONE', *, *, #64153, .T. ) ;
#9168 = VECTOR ( 'NONE', #59971, 1000.000000000000000 ) ;
#9169 = DIRECTION ( 'NONE',  ( -0.000000000000000000, -0.000000000000000000, -1.000000000000000000 ) ) ;
#9170 = CARTESIAN_POINT ( 'NONE',  ( -166.9969673948021978, 80.56076768517787912, 69.50387472010612555 ) ) ;
#9171 = VERTEX_POINT ( 'NONE', #60804 ) ;
#9172 = EDGE_CURVE ( 'NONE', #15171, #33294, #65400, .T. ) ;
#9173 = ORIENTED_EDGE ( 'NONE', *, *, #26128, .T. ) ;
#9174 = CARTESIAN_POINT ( 'NONE',  ( -8.000000000000000000, -4.618802153517024500, -0.7145311798163346273 ) ) ;
#9175 = CARTESIAN_POINT ( 'NONE',  ( -118.4753258120605324, 41.79945864152914936, -95.00000000000133582 ) ) ;
#9177 = CARTESIAN_POINT ( 'NONE',  ( 177.0075766083213011, 74.58167636505953624, -23.18021568563761292 ) ) ;
#9176 = AXIS2_PLACEMENT_3D ( 'NONE', #37315, #10933, #65458 ) ;
#9178 = VECTOR ( 'NONE', #30636, 1000.000000000000000 ) ;
#9179 = DIRECTION ( 'NONE',  ( 0.000000000000000000, 0.000000000000000000, 1.000000000000000000 ) ) ;
#9180 = CARTESIAN_POINT ( 'NONE',  ( -20.55634918610411077, -46.66904755831208718, 2.000000000000000000 ) ) ;
#9181 = VERTEX_POINT ( 'NONE', #28814 ) ;
#9182 = CARTESIAN_POINT ( 'NONE',  ( 39.40195752203892710, -170.0000000000000000, 29.91383430596324899 ) ) ;
#9183 = ORIENTED_EDGE ( 'NONE', *, *, #41454, .T. ) ;
#9184 = CARTESIAN_POINT ( 'NONE',  ( 212.0739503583953933, 117.0412199804969759, 8.464582291069975284 ) ) ;
#9185 = CARTESIAN_POINT ( 'NONE',  ( 15.78827728214693771, 7.507518794609574719, 71.85925826316895382 ) ) ;
#9186 = CARTESIAN_POINT ( 'NONE',  ( 210.5178985598940073, 114.6803933586780886, 41.44437144286931840 ) ) ;
#9187 = FACE_BOUND ( 'NONE', #17403, .T. ) ;
#9188 = VERTEX_POINT ( 'NONE', #17189 ) ;
#9189 = ORIENTED_EDGE ( 'NONE', *, *, #18185, .T. ) ;
#9190 = LINE ( 'NONE', #30649, #5313 ) ;
#9191 = CARTESIAN_POINT ( 'NONE',  ( -118.6212148433689464, 43.06705977238695482, 93.76419461760292506 ) ) ;
#9192 = CARTESIAN_POINT ( 'NONE',  ( 36.98541457540710553, 9.120571655722411464, -62.84764358573202969 ) ) ;
#9193 = LINE ( 'NONE', #30653, #69140 ) ;
#9194 = CARTESIAN_POINT ( 'NONE',  ( 204.6977192012829505, 108.0580384837234931, 56.05227132923312183 ) ) ;
#9195 = DIRECTION ( 'NONE',  ( 1.000000000000000000, 1.110223024625118675E-14, -1.110223024625118675E-14 ) ) ;
#9196 = EDGE_CURVE ( 'NONE', #33759, #48517, #23237, .T. ) ;
#9197 = ORIENTED_EDGE ( 'NONE', *, *, #7793, .F. ) ;
#9198 = CARTESIAN_POINT ( 'NONE',  ( -25.99999999999998934, 0.000000000000000000, -50.00000000000000000 ) ) ;
#9199 = CARTESIAN_POINT ( 'NONE',  ( -40.99999999999994316, 0.000000000000000000, -104.9999999999999858 ) ) ;
#9200 = EDGE_CURVE ( 'NONE', #30237, #57581, #39022, .T. ) ;
#9201 = VERTEX_POINT ( 'NONE', #6299 ) ;
#9202 = CARTESIAN_POINT ( 'NONE',  ( -84.55373779407986490, 24.65190748253136377, 6.400853874559598644 ) ) ;
#9203 = EDGE_LOOP ( 'NONE', ( #17271, #26273 ) ) ;
#9204 = B_SPLINE_CURVE_WITH_KNOTS ( 'NONE', 3,
 ( #54483, #33755, #54125, #49912, #39032, #34105, #1040, #12290, #49204, #60476, #28109, #54838, #27761, #65409, #64708, #22491, #17918, #48847, #11937, #331, #692, #17199, #55189, #66131, #43587, #16516, #38671, #33409, #60117, #7373, #6660, #65058, #49552, #7013, #1742, #23202, #16857, #60816, #12642, #55540, #37974, #21784, #43233, #59418 ),
 .UNSPECIFIED., .F., .F.,
 ( 4, 2, 2, 2, 2, 2, 2, 2, 2, 2, 2, 2, 2, 2, 2, 2, 2, 2, 2, 2, 2, 4 ),
 ( 0.000000000000000000, 0.001472974678681649233, 0.002209462018022473849, 0.002945949357363298465, 0.004418924036044928616, 0.005891898714726559634, 0.007364873393408188050, 0.008101360732749002258, 0.008837848072089817333, 0.01031082275077144575, 0.01178379742945307763, 0.01252028476879390138, 0.01325677210813472687, 0.01472974678681635528, 0.01546623412615717209, 0.01620272146549798370, 0.01767569614417961732, 0.01914867082286124747, 0.01988515816220205734, 0.02062164550154286374, 0.02209462018022448695, 0.02356759485890610670 ),
 .UNSPECIFIED. ) ;
#9205 = DIRECTION ( 'NONE',  ( 1.000000000000000000, -0.000000000000000000, -0.000000000000000000 ) ) ;
#9206 = EDGE_CURVE ( 'NONE', #31187, #31627, #22349, .T. ) ;
#9207 = ORIENTED_EDGE ( 'NONE', *, *, #13430, .F. ) ;
#9208 = ADVANCED_FACE ( 'NONE', ( #54827 ), #12279, .F. ) ;
#9209 = AXIS2_PLACEMENT_3D ( 'NONE', #58153, #69031, #20862 ) ;
#9210 = ORIENTED_EDGE ( 'NONE', *, *, #25346, .T. ) ;
#9211 = CARTESIAN_POINT ( 'NONE',  ( 45.89232972083999584, 10.36128169546909561, 60.49194103217620011 ) ) ;
#9212 = CARTESIAN_POINT ( 'NONE',  ( 21.96921518829188358, 71.65937688154191676, 41.38025477438755928 ) ) ;
#9213 = CARTESIAN_POINT ( 'NONE',  ( 15.78827728214693416, 6.500811158483284835, 3.170157082241545687 ) ) ;
#9214 = ORIENTED_EDGE ( 'NONE', *, *, #23752, .T. ) ;
#9215 = PRODUCT_DEFINITION_SHAPE ( 'NONE', 'NONE',  #69623 ) ;
#9216 = AXIS2_PLACEMENT_3D ( 'NONE', #56295, #56647, #55248 ) ;
#9217 = VECTOR ( 'NONE', #1651, 1000.000000000000000 ) ;
#9218 = CARTESIAN_POINT ( 'NONE',  ( -38.92952675655186567, 10.94143817563081100, 91.90481984702363150 ) ) ;
#9219 = CARTESIAN_POINT ( 'NONE',  ( 175.0696098417092230, 74.11936424544846602, -75.05761745562652720 ) ) ;
#9220 = CARTESIAN_POINT ( 'NONE',  ( -444.4229916354184979, 394.6798985497181889, -128.5895624939293498 ) ) ;
#9221 = EDGE_CURVE ( 'NONE', #29497, #12427, #56627, .T. ) ;
#9222 = DIRECTION ( 'NONE',  ( 0.000000000000000000, 1.000000000000000000, 0.000000000000000000 ) ) ;
#9223 = AXIS2_PLACEMENT_3D ( 'NONE', #43882, #27361, #33710 ) ;
#9224 = CARTESIAN_POINT ( 'NONE',  ( 79.92842440418706929, 18.29578799637232933, -46.72678255005806136 ) ) ;
#9225 = DIRECTION ( 'NONE',  ( -0.8118923937861950435, -0.5838071093367415143, 0.000000000000000000 ) ) ;
#9226 = ORIENTED_EDGE ( 'NONE', *, *, #66169, .T. ) ;
#9227 = VERTEX_POINT ( 'NONE', #62609 ) ;
#9228 = LINE ( 'NONE', #42610, #30904 ) ;
#9229 = CARTESIAN_POINT ( 'NONE',  ( -84.55783695959765112, 25.74181993349143482, -64.79229219887942293 ) ) ;
#9230 = CARTESIAN_POINT ( 'NONE',  ( 181.0840389613909736, 80.03940679743415387, 17.46404351504774866 ) ) ;
#9231 = DIRECTION ( 'NONE',  ( 1.000000000000000000, 1.387778780781445676E-16, 0.000000000000000000 ) ) ;
#9232 = CARTESIAN_POINT ( 'NONE',  ( 0.000000000000000000, 0.000000000000000000, 0.000000000000000000 ) ) ;
#9233 = DIRECTION ( 'NONE',  ( -0.000000000000000000, 1.000000000000000000, -0.000000000000000000 ) ) ;
#9234 = CARTESIAN_POINT ( 'NONE',  ( -156.0171627975467459, 69.90368824761763733, 15.11010338763517069 ) ) ;
#9235 = CARTESIAN_POINT ( 'NONE',  ( -119.2949674747224833, 43.48097822533566870, -65.65536687615315259 ) ) ;
#9236 = CARTESIAN_POINT ( 'NONE',  ( 7.347880794884118356E-15, 0.000000000000000000, 60.00000000000000000 ) ) ;
#9237 = CARTESIAN_POINT ( 'NONE',  ( -73.79615177260653525, 20.52570924097572203, -63.73540638605312836 ) ) ;
#9238 = CARTESIAN_POINT ( 'NONE',  ( -108.1144194775597214, 35.84457139767598477, 33.27986733419606225 ) ) ;
#9239 = ORIENTED_EDGE ( 'NONE', *, *, #46997, .F. ) ;
#9240 = ITEM_DEFINED_TRANSFORMATION ( 'NONE', 'NONE', #32107,  #66832 ) ;
#9241 = CARTESIAN_POINT ( 'NONE',  ( -62.55959671100190178, 17.87514270266995808, 91.55944001517654840 ) ) ;
#9242 = ORIENTED_EDGE ( 'NONE', *, *, #623, .F. ) ;
#9243 = CARTESIAN_POINT ( 'NONE',  ( 198.3926538463959162, 98.07933330386025261, -12.88060239399294638 ) ) ;
#9244 = VERTEX_POINT ( 'NONE', #2819 ) ;
#9245 = CARTESIAN_POINT ( 'NONE',  ( -144.2038301586456726, 61.09856042007388055, 6.051060875653559989 ) ) ;
#9246 = CARTESIAN_POINT ( 'NONE',  ( -449.7337897053571965, 364.9999999999955662, 110.6213636698579705 ) ) ;
#9247 = CARTESIAN_POINT ( 'NONE',  ( 9.962235950565768050, -64.23203137738408941, 170.0000000000000000 ) ) ;
#9248 = LINE ( 'NONE', #3619, #40081 ) ;
#9249 = CARTESIAN_POINT ( 'NONE',  ( 141.3400002717723112, 47.33399859146518196, -42.95563374243955934 ) ) ;
#9250 = CARTESIAN_POINT ( 'NONE',  ( 37.00112095025829717, 8.109340230899354296, -36.01023555749208072 ) ) ;
#9251 = DIRECTION ( 'NONE',  ( 0.7071067811865405783, 7.105427357601001070E-15, -0.7071067811865545671 ) ) ;
#9252 = CARTESIAN_POINT ( 'NONE',  ( 9.050324533885213185, 7.384616180193962265, -46.34927038791500564 ) ) ;
#9253 = CARTESIAN_POINT ( 'NONE',  ( 132.9485794245231318, 40.87843215479637138, -36.06474506355797160 ) ) ;
#9254 = ORIENTED_EDGE ( 'NONE', *, *, #31048, .F. ) ;
#9255 = ORIENTED_EDGE ( 'NONE', *, *, #36424, .T. ) ;
#9256 = CARTESIAN_POINT ( 'NONE',  ( 176.7865369010601739, 75.76733092971367967, 84.34302050498311587 ) ) ;
#9257 = CARTESIAN_POINT ( 'NONE',  ( -190.6985136298601731, 109.1272424661242582, -95.00000000000133582 ) ) ;
#9258 = UNCERTAINTY_MEASURE_WITH_UNIT (LENGTH_MEASURE( 1.000000000000000082E-05 ), #38027, 'distance_accuracy_value', 'NONE');
#9259 = AXIS2_PLACEMENT_3D ( 'NONE', #66754, #11872, #65345 ) ;
#9260 = PLANE ( 'NONE',  #31759 ) ;
#9261 = CARTESIAN_POINT ( 'NONE',  ( -417.6627218934913230, 219.4906275429376308, -144.4497041420118819 ) ) ;
#9262 = ORIENTED_EDGE ( 'NONE', *, *, #30490, .F. ) ;
#9263 = CARTESIAN_POINT ( 'NONE',  ( 73.95984195137785377, 12.15131637179898583, 41.38025477438755928 ) ) ;
#9264 = CARTESIAN_POINT ( 'NONE',  ( -36.11269837220804391, 15.55634918610408945, 0.000000000000000000 ) ) ;
#9265 = VECTOR ( 'NONE', #66787, 1000.000000000000000 ) ;
#9266 = CARTESIAN_POINT ( 'NONE',  ( -175.1920326508032986, 89.46239303019291356, -49.43298755416176249 ) ) ;
#9267 = CARTESIAN_POINT ( 'NONE',  ( 93.61951000632932107, 21.92572933971852223, -19.20632885156578240 ) ) ;
#9268 = CARTESIAN_POINT ( 'NONE',  ( -27.49195330402088544, 9.993776132065303131, 58.17902382732258104 ) ) ;
#9269 = DIRECTION ( 'NONE',  ( -0.000000000000000000, -0.000000000000000000, -1.000000000000000000 ) ) ;
#9270 = CARTESIAN_POINT ( 'NONE',  ( 51.39999999999999858, 0.000000000000000000, 0.000000000000000000 ) ) ;
#9271 = ORIENTED_EDGE ( 'NONE', *, *, #49208, .T. ) ;
#9272 = DIRECTION ( 'NONE',  ( -0.000000000000000000, -1.000000000000000000, -0.000000000000000000 ) ) ;
#9273 = AXIS2_PLACEMENT_3D ( 'NONE', #41737, #38090, #32823 ) ;
#9274 = CARTESIAN_POINT ( 'NONE',  ( 15.55634918610403261, 0.000000000000000000, 0.000000000000000000 ) ) ;
#9275 = CARTESIAN_POINT ( 'NONE',  ( -105.4642082819536455, 35.56541171990219397, -62.55240665351630014 ) ) ;
#9276 = CARTESIAN_POINT ( 'NONE',  ( -51.34325167237333432, 13.71819364263222418, -36.19337418838312459 ) ) ;
#9277 = DIRECTION ( 'NONE',  ( -1.000000000000000000, 0.000000000000000000, 0.000000000000000000 ) ) ;
#9278 = LINE ( 'NONE', #4354, #27716 ) ;
#9279 = ORIENTED_EDGE ( 'NONE', *, *, #56136, .T. ) ;
#9280 = PRESENTATION_STYLE_ASSIGNMENT (( #7905 ) ) ;
#9281 = CARTESIAN_POINT ( 'NONE',  ( -2.999999999999990674, 21.50000000000000000, 0.000000000000000000 ) ) ;
#9282 = EDGE_CURVE ( 'NONE', #18239, #35316, #46068, .T. ) ;
#9283 = ORIENTED_EDGE ( 'NONE', *, *, #20333, .F. ) ;
#9284 = ORIENTED_EDGE ( 'NONE', *, *, #57336, .F. ) ;
#9285 = LINE ( 'NONE', #30748, #60009 ) ;
#9286 = FACE_OUTER_BOUND ( 'NONE', #58448, .T. ) ;
#9287 = DIRECTION ( 'NONE',  ( 0.000000000000000000, 0.000000000000000000, 1.000000000000000000 ) ) ;
#9288 = VERTEX_POINT ( 'NONE', #45729 ) ;
#9289 = CARTESIAN_POINT ( 'NONE',  ( 427.4999999999999432, -18.06806526123148160, -2.000000000000000000 ) ) ;
#9290 = LINE ( 'NONE', #57144, #63732 ) ;
#9291 = CARTESIAN_POINT ( 'NONE',  ( 78.57571471437145760, 0.000000000000000000, -20.00000000000000000 ) ) ;
#9292 = ADVANCED_FACE ( 'NONE', ( #67539 ), #61893, .T. ) ;
#9293 = CARTESIAN_POINT ( 'NONE',  ( 59.30258796551118650, 12.87111270082601422, -49.75570897052192976 ) ) ;
#9294 = CARTESIAN_POINT ( 'NONE',  ( -81.89510452344293867, 24.66033552777454929, 31.13203741669646263 ) ) ;
#9295 = CARTESIAN_POINT ( 'NONE',  ( -23.95089599695169014, 9.496585844566173051, -16.46116198601244918 ) ) ;
#9296 = DIRECTION ( 'NONE',  ( -0.000000000000000000, -0.000000000000000000, 1.000000000000000000 ) ) ;
#9297 = ORIENTED_EDGE ( 'NONE', *, *, #59308, .T. ) ;
#9298 = CARTESIAN_POINT ( 'NONE',  ( 133.8566784816069344, -170.0000000000000000, 29.51034083899533300 ) ) ;
#9299 = CARTESIAN_POINT ( 'NONE',  ( -60.00000000000000000, 7.347880794884118356E-15, 5.000000000000000000 ) ) ;
#9301 = EDGE_CURVE ( 'NONE', #61321, #61115, #4149, .T. ) ;
#9300 = CARTESIAN_POINT ( 'NONE',  ( -24.95010104166215470, 9.631487977190602123, 41.48526991647725737 ) ) ;
#9302 = CARTESIAN_POINT ( 'NONE',  ( 200.8303160266298732, 102.8412051751308667, 43.14791935769463294 ) ) ;
#9303 = B_SPLINE_CURVE_WITH_KNOTS ( 'NONE', 3,
 ( #9123, #25314, #64305, #15773, #25658, #4869, #58671, #47091, #31276, #52702, #46745, #57658, #68554, #20356, #9470, #47773, #42163, #4531, #20706, #26337, #63626, #15440, #68218, #41481, #31958, #36892, #69230, #58328, #63960, #21062, #53386, #26679, #32642, #277, #49147, #28404, #987, #21730, #5893, #22783, #22435, #66070, #16799, #12238 ),
 .UNSPECIFIED., .F., .F.,
 ( 4, 2, 2, 2, 2, 2, 2, 2, 2, 2, 2, 2, 2, 2, 2, 2, 2, 2, 2, 2, 2, 4 ),
 ( 0.02895403260893137515, 0.03071603688922225697, 0.03247804116951313880, 0.03424004544980401715, 0.03600204973009489551, 0.03776405401038578080, 0.03864505615053121651, 0.03952605829067665222, 0.04040706043082208793, 0.04128806257096752363, 0.04216906471111296628, 0.04305006685125840199, 0.04393106899140383770, 0.04481207113154928035, 0.04569307327169470911, 0.04657407541184015176, 0.04745507755198558747, 0.04833607969213102318, 0.05009808397242189459, 0.05186008825271277295, 0.05362209253300365130, 0.05714610109358542189 ),
 .UNSPECIFIED. ) ;
#9304 = FACE_OUTER_BOUND ( 'NONE', #4348, .T. ) ;
#9306 = ORIENTED_EDGE ( 'NONE', *, *, #28463, .F. ) ;
#9305 = LINE ( 'NONE', #30079, #63541 ) ;
#9307 = PLANE ( 'NONE',  #59991 ) ;
#9308 = ORIENTED_EDGE ( 'NONE', *, *, #56633, .T. ) ;
#9309 = VECTOR ( 'NONE', #39059, 1000.000000000000000 ) ;
#9310 = ORIENTED_EDGE ( 'NONE', *, *, #68306, .F. ) ;
#9311 = CIRCLE ( 'NONE', #48589, 65.00000000000000000 ) ;
#9312 = CARTESIAN_POINT ( 'NONE',  ( 115.0485321076020853, 32.28990710985444679, -64.48787662897211703 ) ) ;
#9313 = CARTESIAN_POINT ( 'NONE',  ( 8.000000000000007105, 249.8719672152120381, 94.99999999999866418 ) ) ;
#9314 = FACE_OUTER_BOUND ( 'NONE', #66410, .T. ) ;
#9315 = DIRECTION ( 'NONE',  ( 0.7071067811865476838, -6.441404958702661839E-16, 0.7071067811865474617 ) ) ;
#9316 = AXIS2_PLACEMENT_3D ( 'NONE', #41620, #9962, #53538 ) ;
#9317 = FACE_OUTER_BOUND ( 'NONE', #39668, .T. ) ;
#9318 = DIRECTION ( 'NONE',  ( 0.000000000000000000, -0.000000000000000000, 1.000000000000000000 ) ) ;
#9319 = DIRECTION ( 'NONE',  ( -0.5773502691896258421, -0.5773502691896258421, -0.5773502691896258421 ) ) ;
#9320 = VECTOR ( 'NONE', #36694, 1000.000000000000000 ) ;
#9321 = CARTESIAN_POINT ( 'NONE',  ( -51.13576748034040520, 14.70354244225167406, 31.41683688099750071 ) ) ;
#9322 = ORIENTED_EDGE ( 'NONE', *, *, #36064, .F. ) ;
#9323 = ORIENTED_EDGE ( 'NONE', *, *, #67194, .F. ) ;
#9324 = CARTESIAN_POINT ( 'NONE',  ( 10.55634918610406281, 15.55634918610400241, 85.00100000000000477 ) ) ;
#9325 = CARTESIAN_POINT ( 'NONE',  ( -86.15466590221103615, 26.40813842494317498, -42.12330144728298364 ) ) ;
#9326 = AXIS2_PLACEMENT_3D ( 'NONE', #59218, #21252, #42363 ) ;
#9327 = CARTESIAN_POINT ( 'NONE',  ( 103.3371571523556014, 25.81603694048630615, 93.80874747008428471 ) ) ;
#9328 = CARTESIAN_POINT ( 'NONE',  ( 8.000000000000000000, 3.115336682267014101, -9.180606868608490956 ) ) ;
#9329 = CARTESIAN_POINT ( 'NONE',  ( 188.0081045302011091, 85.89855126821616693, -46.62130388048676366 ) ) ;
#9330 = CARTESIAN_POINT ( 'NONE',  ( -59.09450113343241640, 27.07101652673493319, 170.0000000000000000 ) ) ;
#9331 = CARTESIAN_POINT ( 'NONE',  ( -5.000000000000073719, -46.66904755831211560, 85.00100000000000477 ) ) ;
#9332 = ORIENTED_EDGE ( 'NONE', *, *, #20722, .F. ) ;
#9333 = VERTEX_POINT ( 'NONE', #19335 ) ;
#9334 = ORIENTED_EDGE ( 'NONE', *, *, #16653, .T. ) ;
#9335 = DIRECTION ( 'NONE',  ( -0.000000000000000000, -2.500042656554809847E-16, 1.000000000000000000 ) ) ;
#9336 = CARTESIAN_POINT ( 'NONE',  ( 179.7182127114821810, 77.23376928426336008, -90.00569010101817469 ) ) ;
#9337 = CARTESIAN_POINT ( 'NONE',  ( 70.46452034227871764, 14.52462608639673647, -44.22581347596196366 ) ) ;
#9338 = CARTESIAN_POINT ( 'NONE',  ( 107.2180420114370492, 27.50716259871310143, -90.23723215542567289 ) ) ;
#9339 = DIRECTION ( 'NONE',  ( 0.7071067811865473507, -6.441404958702665783E-16, -0.7071067811865477948 ) ) ;
#9340 = DIRECTION ( 'NONE',  ( 0.000000000000000000, 0.000000000000000000, 1.000000000000000000 ) ) ;
#9341 = FACE_BOUND ( 'NONE', #3126, .T. ) ;
#9342 = CARTESIAN_POINT ( 'NONE',  ( 8.951900209438536038, 6.378066731449592908, -19.26863345807493388 ) ) ;
#9344 = ORIENTED_EDGE ( 'NONE', *, *, #14136, .T. ) ;
#9343 = EDGE_CURVE ( 'NONE', #36820, #23240, #46407, .T. ) ;
#9345 = CARTESIAN_POINT ( 'NONE',  ( 15.78827728214693416, 7.507518794609588042, 3.170157082241545687 ) ) ;
#9346 = CARTESIAN_POINT ( 'NONE',  ( 181.0840389613909736, 78.60582251573006829, 71.15314469597512925 ) ) ;
#9347 = CARTESIAN_POINT ( 'NONE',  ( -125.8938041572051105, 46.49392987655492959, 3.775397282693376599 ) ) ;
#9348 = CARTESIAN_POINT ( 'NONE',  ( -17.89459634713042391, -72.78390022947110083, 41.38025477438755928 ) ) ;
#9349 = DIRECTION ( 'NONE',  ( -1.000000000000000000, 0.000000000000000000, 0.000000000000000000 ) ) ;
#9350 = B_SPLINE_CURVE_WITH_KNOTS ( 'NONE', 3,
 ( #58036, #36930, #20746, #40911, #15477, #4911, #61327, #66971, #61670, #51123, #37603, #54460, #58706, #16839, #37955, #53427, #10523, #312, #32343, #22122, #27045, #31062, #21427, #38299, #43569, #59739, #60096, #43911, #42869, #65394, #11213, #6642, #64693, #31995, #676, #53770, #1024, #6293, #5591, #17182, #65040, #27389, #11553, #37254, #33392, #48478, #10873, #42544, #59402, #38655 ),
 .UNSPECIFIED., .F., .F.,
 ( 4, 2, 2, 2, 2, 2, 2, 2, 2, 2, 2, 2, 2, 2, 2, 2, 2, 2, 2, 2, 2, 2, 2, 2, 4 ),
 ( 0.03126542424884326543, 0.03330676804260261636, 0.03534811183636196730, 0.03738945563012131823, 0.03943079942388067610, 0.04045147132076034463, 0.04147214321764001316, 0.04249281511451968862, 0.04351348701139935715, 0.04555483080515874972, 0.04657550270203845988, 0.04759617459891818392, 0.04810651054735805981, 0.04861684649579793571, 0.04963751839267768751, 0.05065819028955745318, 0.05167886218643720497, 0.05269953408331695677, 0.05372020598019670856, 0.05474087787707647423, 0.05576154977395622603, 0.05780289356771575737, 0.05984423736147530259, 0.06188558115523483394, 0.06392692494899437916 ),
 .UNSPECIFIED. ) ;
#9351 = CARTESIAN_POINT ( 'NONE',  ( 19.75315861330098244, 7.667327050329332927, -22.54537247460588034 ) ) ;
#9352 = CARTESIAN_POINT ( 'NONE',  ( 10.13563904803030979, 7.391572367417560407, 15.62368066821783685 ) ) ;
#9353 = ADVANCED_FACE ( 'NONE', ( #51360 ), #35525, .T. ) ;
#9354 = AXIS2_PLACEMENT_3D ( 'NONE', #45077, #60911, #12734 ) ;
#9355 = VERTEX_POINT ( 'NONE', #40448 ) ;
#9357 = CARTESIAN_POINT ( 'NONE',  ( -125.8938041572051105, 46.49392987655493670, -88.60280507916129977 ) ) ;
#9356 = CONICAL_SURFACE ( 'NONE', #62123, 74.95140232871122521, 0.8777644062502172329 ) ;
#9358 = APPLICATION_PROTOCOL_DEFINITION ( 'draft international standard', 'automotive_design', 1998, #45758 ) ;
#9359 = DIRECTION ( 'NONE',  ( -0.3090169943749446757, -0.9510565162951544194, 0.000000000000000000 ) ) ;
#9360 = CARTESIAN_POINT ( 'NONE',  ( -129.6001310305488516, 48.98284622040320357, -35.88933794309529901 ) ) ;
#9361 = CARTESIAN_POINT ( 'NONE',  ( -109.5157885508426432, 37.76058765671429995, -40.47346829093316956 ) ) ;
#9362 = CARTESIAN_POINT ( 'NONE',  ( 183.9887307715836755, 83.05100282186906213, -36.80690435289106688 ) ) ;
#9363 = ORIENTED_EDGE ( 'NONE', *, *, #29015, .F. ) ;
#9364 = VECTOR ( 'NONE', #50767, 1000.000000000000000 ) ;
#9365 = EDGE_LOOP ( 'NONE', ( #28126, #1997, #15700, #68418 ) ) ;
#9367 = EDGE_CURVE ( 'NONE', #59065, #64204, #49184, .T. ) ;
#9366 = VECTOR ( 'NONE', #7323, 1000.000000000000000 ) ;
#9368 = CARTESIAN_POINT ( 'NONE',  ( -29.75049355503752579, 9.320234381800311496, -23.28418078306753003 ) ) ;
#9369 = VECTOR ( 'NONE', #31257, 999.9999999999998863 ) ;
#9370 = PLANE ( 'NONE',  #40593 ) ;
#9371 = ADVANCED_FACE ( 'NONE', ( #9485 ), #63644, .F. ) ;
#9372 = ORIENTED_EDGE ( 'NONE', *, *, #27484, .T. ) ;
#9373 = AXIS2_PLACEMENT_3D ( 'NONE', #52520, #9269, #4346 ) ;
#9374 = FACE_OUTER_BOUND ( 'NONE', #3949, .T. ) ;
#9375 = EDGE_LOOP ( 'NONE', ( #40008, #23303, #63264, #43200 ) ) ;
#9376 = CARTESIAN_POINT ( 'NONE',  ( 126.6266894765173987, 38.37986986668740741, -68.30481562020717945 ) ) ;
#9377 = CARTESIAN_POINT ( 'NONE',  ( 10.01137213834873840, 64.59476928204603041, 6.377659838150142862E-18 ) ) ;
#9378 = CARTESIAN_POINT ( 'NONE',  ( -65.99999999999997158, 29.79383981485517197, -2.367957528293540247E-14 ) ) ;
#9379 = CIRCLE ( 'NONE', #62143, 5.000000000000000888 ) ;
#9380 = ADVANCED_FACE ( 'NONE', ( #36213 ), #31622, .F. ) ;
#9381 = CARTESIAN_POINT ( 'NONE',  ( -94.85061234775062644, 29.16417548023186157, 36.96106783413039665 ) ) ;
#9382 = DIRECTION ( 'NONE',  ( 0.000000000000000000, 0.000000000000000000, 1.000000000000000000 ) ) ;
#9384 = ORIENTED_EDGE ( 'NONE', *, *, #37296, .F. ) ;
#9383 = CARTESIAN_POINT ( 'NONE',  ( -67.03031041878421092, -33.66749151869542089, 170.0000000000000000 ) ) ;
#9385 = DIRECTION ( 'NONE',  ( 0.8090169943749506709, -0.5877852522924686962, 0.000000000000000000 ) ) ;
#9386 = EDGE_LOOP ( 'NONE', ( #23868, #37434, #5468, #46800 ) ) ;
#9387 = ORIENTED_EDGE ( 'NONE', *, *, #41155, .F. ) ;
#9388 = CARTESIAN_POINT ( 'NONE',  ( -172.7173255566597447, 88.18461381371098184, 3.977144016177347030 ) ) ;
#9389 = LINE ( 'NONE', #68804, #60559 ) ;
#9390 = APPLICATION_CONTEXT ( 'automotive_design' ) ;
#9391 = ADVANCED_FACE ( 'NONE', ( #10501 ), #15452, .T. ) ;
#9392 = CARTESIAN_POINT ( 'NONE',  ( -178.0633751203918678, 92.80295726428050784, -9.721336043951847472 ) ) ;
#9394 = ORIENTED_EDGE ( 'NONE', *, *, #56443, .F. ) ;
#9393 = CARTESIAN_POINT ( 'NONE',  ( -126.7944042662569046, 48.29830493043732531, 57.50493334633024745 ) ) ;
#9395 = CARTESIAN_POINT ( 'NONE',  ( -109.1372336806175554, 37.55118937703328186, 88.60118964784474827 ) ) ;
#9396 = EDGE_CURVE ( 'NONE', #20231, #41387, #26009, .T. ) ;
#9397 = EDGE_CURVE ( 'NONE', #6351, #49086, #37826, .T. ) ;
#9398 = DIRECTION ( 'NONE',  ( 0.000000000000000000, 0.000000000000000000, 1.000000000000000000 ) ) ;
#9399 = EDGE_CURVE ( 'NONE', #17356, #57474, #31288, .T. ) ;
#9400 = ORIENTED_EDGE ( 'NONE', *, *, #44188, .T. ) ;
#9401 = CARTESIAN_POINT ( 'NONE',  ( -58.76006735892197952, 15.70681061434692971, -22.39598332331549102 ) ) ;
#9402 = LINE ( 'NONE', #10084, #56701 ) ;
#9404 = DIRECTION ( 'NONE',  ( 0.000000000000000000, 1.000000000000000000, -0.000000000000000000 ) ) ;
#9403 = VECTOR ( 'NONE', #36955, 1000.000000000000000 ) ;
#9405 = CARTESIAN_POINT ( 'NONE',  ( -126.8016613879753578, 48.30316697011513583, 18.73391331175302810 ) ) ;
#9406 = CARTESIAN_POINT ( 'NONE',  ( 70.12389542974193546, 15.47520081968152006, -72.50832765571044547 ) ) ;
#9407 = ORIENTED_EDGE ( 'NONE', *, *, #34558, .T. ) ;
#9408 = VERTEX_POINT ( 'NONE', #47436 ) ;
#9409 = COLOUR_RGB ( '',0.7921568627450980005, 0.8196078431372548767, 0.9333333333333333481 ) ;
#9410 = CARTESIAN_POINT ( 'NONE',  ( 10.46559741370271723, 7.394044226375385165, -91.35694110006950552 ) ) ;
#9411 = CARTESIAN_POINT ( 'NONE',  ( -167.1540252468941787, 80.72321878831098729, -46.76267734215787186 ) ) ;
#9412 = CARTESIAN_POINT ( 'NONE',  ( 442.3372781065085633, 400.0000000000000568, -136.4497041420118251 ) ) ;
#9413 = VECTOR ( 'NONE', #11666, 1000.000000000000000 ) ;
#9414 = DIRECTION ( 'NONE',  ( 0.000000000000000000, -1.000000000000000000, 0.000000000000000000 ) ) ;
#9415 = CARTESIAN_POINT ( 'NONE',  ( -77.02112161466367013, 22.77583432622785509, 45.23932557689580847 ) ) ;
#9416 = CARTESIAN_POINT ( 'NONE',  ( -52.73319225379935205, 53.34578647582052469, 170.0000000000000000 ) ) ;
#9417 = CARTESIAN_POINT ( 'NONE',  ( -143.3925773749112977, 59.16144459815141943, 42.57086191493854699 ) ) ;
#9418 = AXIS2_PLACEMENT_3D ( 'NONE', #36587, #15474, #68257 ) ;
#9419 = CARTESIAN_POINT ( 'NONE',  ( 93.85477471612979627, 23.08982334209078147, -95.00000000000133582 ) ) ;
#9420 = CARTESIAN_POINT ( 'NONE',  ( -166.2028657618940599, 79.74389853943286255, -66.14595115942351811 ) ) ;
#9421 = ORIENTED_EDGE ( 'NONE', *, *, #64314, .T. ) ;
#9423 = DIRECTION ( 'NONE',  ( 0.9362348706397418674, -0.3513748240813305279, 0.000000000000000000 ) ) ;
#9422 = CIRCLE ( 'NONE', #17287, 65.36598343705435354 ) ;
#9424 = ORIENTED_EDGE ( 'NONE', *, *, #67510, .F. ) ;
#9425 = CARTESIAN_POINT ( 'NONE',  ( -33.83558513595455253, 9.996963989836510578, 17.98292301535087034 ) ) ;
#9426 = AXIS2_PLACEMENT_3D ( 'NONE', #64039, #26413, #64375 ) ;
#9427 = DIRECTION ( 'NONE',  ( -1.000000000000000000, 0.000000000000000000, 0.000000000000000000 ) ) ;
#9428 = DIRECTION ( 'NONE',  ( -1.000000000000000000, 0.000000000000000000, 0.000000000000000000 ) ) ;
#9429 = DIRECTION ( 'NONE',  ( -3.356887510711391189E-18, -3.842266915190438346E-18, -1.000000000000000000 ) ) ;
#9430 = DIRECTION ( 'NONE',  ( -0.000000000000000000, 0.000000000000000000, -1.000000000000000000 ) ) ;
#9431 = CARTESIAN_POINT ( 'NONE',  ( 8.000000000000007105, 249.8719672152120381, -95.00000000000133582 ) ) ;
#9432 = CARTESIAN_POINT ( 'NONE',  ( 50.98853755884142203, 395.0000000000065938, -123.9497041420120382 ) ) ;
#9433 = CIRCLE ( 'NONE', #28502, 242.4895526022646379 ) ;
#9434 = CARTESIAN_POINT ( 'NONE',  ( -37.93379515072632557, 11.77251734620211465, -19.75563545715445457 ) ) ;
#9435 = EDGE_LOOP ( 'NONE', ( #37837, #56480, #17568, #28156 ) ) ;
#9436 = CARTESIAN_POINT ( 'NONE',  ( -118.4753258120605466, 42.97785158603420541, -95.00000000000133582 ) ) ;
#9437 = EDGE_LOOP ( 'NONE', ( #3244, #21939, #10507, #34679 ) ) ;
#9438 = DIRECTION ( 'NONE',  ( 1.000000000000000000, -0.000000000000000000, -0.000000000000000000 ) ) ;
#9439 = DIRECTION ( 'NONE',  ( -1.000000000000000000, 0.000000000000000000, 0.000000000000000000 ) ) ;
#9440 = FACE_OUTER_BOUND ( 'NONE', #1072, .T. ) ;
#9441 = CARTESIAN_POINT ( 'NONE',  ( -10.91976120871578004, 7.112268444252505262, -76.59894436445749477 ) ) ;
#9442 = CARTESIAN_POINT ( 'NONE',  ( -95.21430597939263407, 29.33390900154316583, -18.23546955400044212 ) ) ;
#9443 = CARTESIAN_POINT ( 'NONE',  ( 150.2193536046551685, 53.46717047532151668, -45.55991080038433694 ) ) ;
#9444 = ADVANCED_FACE ( 'NONE', ( #4206 ), #64318, .F. ) ;
#9445 = VERTEX_POINT ( 'NONE', #63974 ) ;
#9446 = CARTESIAN_POINT ( 'NONE',  ( 403.0071894358272289, 992.0915846175145134, 569.0068267248735765 ) ) ;
#9447 = CARTESIAN_POINT ( 'NONE',  ( -156.3734885497380844, 71.59531449004281001, 62.03543042666215968 ) ) ;
#9448 = CARTESIAN_POINT ( 'NONE',  ( 180.2494929075578227, 79.18888319146952881, -9.380507075415932761 ) ) ;
#9449 = CARTESIAN_POINT ( 'NONE',  ( -103.8932886509197004, 34.74144483217664003, 57.53545925032246799 ) ) ;
#9450 = DIRECTION ( 'NONE',  ( 0.000000000000000000, -1.000000000000000000, 0.000000000000000000 ) ) ;
#9451 = ORIENTED_EDGE ( 'NONE', *, *, #44658, .F. ) ;
#9452 = CARTESIAN_POINT ( 'NONE',  ( -180.0094637318087223, 96.72611451757710199, -72.03732202628357584 ) ) ;
#9453 = CARTESIAN_POINT ( 'NONE',  ( 93.61951000632933528, 21.92572933971851157, 61.32732291982528494 ) ) ;
#9454 = EDGE_CURVE ( 'NONE', #32748, #26944, #30593, .T. ) ;
#9456 = ADVANCED_FACE ( 'NONE', ( #20039 ), #10160, .F. ) ;
#9455 = CARTESIAN_POINT ( 'NONE',  ( 116.1021807117072058, 31.68810634233425816, 41.81952508025639048 ) ) ;
#9457 = ADVANCED_FACE ( 'NONE', ( #20369 ), #4544, .F. ) ;
#9458 = AXIS2_PLACEMENT_3D ( 'NONE', #56331, #17664, #34554 ) ;
#9459 = CARTESIAN_POINT ( 'NONE',  ( -118.8504142000306132, 42.02789424825281372, -66.66768671471533025 ) ) ;
#9460 = ADVANCED_FACE ( 'NONE', ( #41493 ), #52389, .F. ) ;
#9461 = ORIENTED_EDGE ( 'NONE', *, *, #9148, .F. ) ;
#9462 = CARTESIAN_POINT ( 'NONE',  ( 199.3671895066314335, 99.30947926630329903, 31.40750943429757669 ) ) ;
#9463 = CARTESIAN_POINT ( 'NONE',  ( 116.8937673311173029, 32.08228998570056234, -73.74270732603237377 ) ) ;
#9464 = CARTESIAN_POINT ( 'NONE',  ( 183.9887307715835902, 83.05100282186904792, 43.72674741849996849 ) ) ;
#9465 = CARTESIAN_POINT ( 'NONE',  ( -13.32397999417977630, -63.99361958670536410, 41.38025477438755928 ) ) ;
#9466 = CARTESIAN_POINT ( 'NONE',  ( -440.1146514826279486, 388.0000000000019895, 101.0022254471289074 ) ) ;
#9467 = CONICAL_SURFACE ( 'NONE', #13979, 4.999999999999997335, 0.7853981633974482790 ) ;
#9468 = ORIENTED_EDGE ( 'NONE', *, *, #45418, .F. ) ;
#9469 = VECTOR ( 'NONE', #5942, 1000.000000000000000 ) ;
#9470 = CARTESIAN_POINT ( 'NONE',  ( 174.4978817191264682, 73.57770570413208588, 60.05495216553277515 ) ) ;
#9471 = VERTEX_POINT ( 'NONE', #58683 ) ;
#9472 = CARTESIAN_POINT ( 'NONE',  ( -102.7502407665687798, 33.01985383847078026, -35.01457726497592660 ) ) ;
#9473 = CARTESIAN_POINT ( 'NONE',  ( 141.3536823173203913, 46.13936215296858734, 90.27715462940014390 ) ) ;
#9474 = AXIS2_PLACEMENT_3D ( 'NONE', #35507, #30576, #20026 ) ;
#9475 = CARTESIAN_POINT ( 'NONE',  ( -62.15324028806256962, 16.70091357159899914, 40.28273643365055534 ) ) ;
#9477 = ORIENTED_EDGE ( 'NONE', *, *, #4191, .T. ) ;
#9476 = DIRECTION ( 'NONE',  ( 1.000000000000000000, 0.000000000000000000, 0.000000000000000000 ) ) ;
#9478 = CARTESIAN_POINT ( 'NONE',  ( -178.7458319892713519, 93.61502008198021940, 43.28923195309091199 ) ) ;
#9479 = DIRECTION ( 'NONE',  ( -1.000000000000000000, 0.000000000000000000, 0.000000000000000000 ) ) ;
#9480 = EDGE_CURVE ( 'NONE', #41324, #25791, #48125, .T. ) ;
#9481 = ADVANCED_FACE ( 'NONE', ( #55813 ), #57673, .F. ) ;
#9482 = CARTESIAN_POINT ( 'NONE',  ( 115.7612476187723729, 32.64200929566222698, -38.31947670043274456 ) ) ;
#9483 = ORIENTED_EDGE ( 'NONE', *, *, #29794, .T. ) ;
#9484 = EDGE_CURVE ( 'NONE', #33479, #66025, #52573, .T. ) ;
#9485 = FACE_OUTER_BOUND ( 'NONE', #40553, .T. ) ;
#9486 = CARTESIAN_POINT ( 'NONE',  ( 444.9999999999999432, 225.0000000000000000, -2.000000000000000000 ) ) ;
#9487 = ORIENTED_EDGE ( 'NONE', *, *, #40703, .T. ) ;
#9488 = CARTESIAN_POINT ( 'NONE',  ( 138.1919700334460117, 44.10401742531045954, 57.71697704383397820 ) ) ;
#9489 = CARTESIAN_POINT ( 'NONE',  ( -175.0670687835823003, 90.85007209570210307, -88.64706874488653909 ) ) ;
#9490 = CYLINDRICAL_SURFACE ( 'NONE', #43700, 7.500000000000020428 ) ;
#9491 = CARTESIAN_POINT ( 'NONE',  ( 87.58754341703159696, 20.81465688423119786, 44.66585312417346643 ) ) ;
#9492 = EDGE_LOOP ( 'NONE', ( #68981, #35356 ) ) ;
#9493 = CARTESIAN_POINT ( 'NONE',  ( 41.09759788073309750, 9.651672055033847286, 17.87914307703790229 ) ) ;
#9494 = ORIENTED_EDGE ( 'NONE', *, *, #63914, .F. ) ;
#9495 = CARTESIAN_POINT ( 'NONE',  ( 155.2992895652387801, 57.24699634758577815, -23.97237736446589196 ) ) ;
#9496 = CARTESIAN_POINT ( 'NONE',  ( 208.5936709733499015, 113.6229123546138453, -23.40417240335101923 ) ) ;
#9497 = LINE ( 'NONE', #36918, #5430 ) ;
#9498 = CARTESIAN_POINT ( 'NONE',  ( -153.7005182577088931, 67.81869626254724892, -62.92235873534134072 ) ) ;
#9499 = CARTESIAN_POINT ( 'NONE',  ( 55.65828023224232624, 11.08571960351219765, 89.50825515078493311 ) ) ;
#9500 = CARTESIAN_POINT ( 'NONE',  ( 188.0103583326377077, 87.39896620268119420, 12.85485524293919468 ) ) ;
#9501 = CARTESIAN_POINT ( 'NONE',  ( 211.5175447467296692, 116.1901475271414057, -40.69079531326852361 ) ) ;
#9502 = CARTESIAN_POINT ( 'NONE',  ( 173.9413349464226997, 71.67637800842356910, 7.659110634810657459 ) ) ;
#9503 = ORIENTED_EDGE ( 'NONE', *, *, #22947, .F. ) ;
#9504 = VECTOR ( 'NONE', #6347, 1000.000000000000000 ) ;
#9505 = DIRECTION ( 'NONE',  ( -0.000000000000000000, 1.000000000000000000, -0.000000000000000000 ) ) ;
#9506 = ORIENTED_EDGE ( 'NONE', *, *, #24050, .F. ) ;
#9507 = CARTESIAN_POINT ( 'NONE',  ( -71.86568654225716557, 20.91200104397924164, 61.59056581666523300 ) ) ;
#9508 = CARTESIAN_POINT ( 'NONE',  ( 58.09607305250593612, 11.58497620657515803, -75.74799500400911256 ) ) ;
#9509 = LINE ( 'NONE', #14445, #27139 ) ;
#9510 = DIRECTION ( 'NONE',  ( 0.000000000000000000, 0.000000000000000000, 1.000000000000000000 ) ) ;
#9511 = CARTESIAN_POINT ( 'NONE',  ( -1.298947065946362001, 6.553849421084473548, 94.99999999999866418 ) ) ;
#9512 = CARTESIAN_POINT ( 'NONE',  ( 442.3372781065086201, 0.000000000000000000, 83.55029585798817493 ) ) ;
#9513 = CIRCLE ( 'NONE', #54419, 21.99999999999998579 ) ;
#9514 = ORIENTED_EDGE ( 'NONE', *, *, #18668, .F. ) ;
#9515 = CARTESIAN_POINT ( 'NONE',  ( -77.71448999903259391, 21.96089801565739208, 72.21751608881839957 ) ) ;
#9516 = CARTESIAN_POINT ( 'NONE',  ( 65.13282190615461786, 1.839221433318906476E-12, -5.000000000000000000 ) ) ;
#9517 = EDGE_LOOP ( 'NONE', ( #61861, #65426, #23642, #69064 ) ) ;
#9518 = VECTOR ( 'NONE', #48761, 1000.000000000000000 ) ;
#9519 = ORIENTED_EDGE ( 'NONE', *, *, #51386, .F. ) ;
#9520 = CIRCLE ( 'NONE', #61190, 25.12245591505646303 ) ;
#9521 = CARTESIAN_POINT ( 'NONE',  ( -152.5067928559255677, 66.76529500553621688, 31.33228448026122237 ) ) ;
#9522 = DIRECTION ( 'NONE',  ( -0.000000000000000000, -1.000000000000000000, -0.000000000000000000 ) ) ;
#9523 = CARTESIAN_POINT ( 'NONE',  ( 174.2469308602415481, 71.96142024047682639, -19.97548777397644670 ) ) ;
#9524 = CARTESIAN_POINT ( 'NONE',  ( -14.79841479960619921, -20.14961338137257840, 0.000000000000000000 ) ) ;
#9525 = EDGE_CURVE ( 'NONE', #13412, #51562, #55950, .T. ) ;
#9526 = VECTOR ( 'NONE', #10062, 1000.000000000000000 ) ;
#9527 = CARTESIAN_POINT ( 'NONE',  ( -142.0081215801270105, 58.07066293384866640, 11.07645372095419489 ) ) ;
#9528 = EDGE_LOOP ( 'NONE', ( #58115, #10190, #40668, #65343, #31297, #32731 ) ) ;
#9529 = CARTESIAN_POINT ( 'NONE',  ( -4.610955605662443446, -74.80943656680585718, 41.38025477438755928 ) ) ;
#9530 = ORIENTED_EDGE ( 'NONE', *, *, #36855, .F. ) ;
#9531 = CARTESIAN_POINT ( 'NONE',  ( 210.6741002223296562, 114.9147155784837793, 14.40197977070410751 ) ) ;
#9532 = CARTESIAN_POINT ( 'NONE',  ( 12.46490660984525789, 7.423426948220649635, 71.08722924195309645 ) ) ;
#9533 = CARTESIAN_POINT ( 'NONE',  ( 212.1535111375854683, 117.1635556319084657, 37.53863579503308046 ) ) ;
#9534 = FACE_BOUND ( 'NONE', #47207, .T. ) ;
#9535 = ADVANCED_FACE ( 'NONE', ( #11190 ), #34491, .T. ) ;
#9536 = EDGE_CURVE ( 'NONE', #36166, #989, #60072, .T. ) ;
#9537 = ORIENTED_EDGE ( 'NONE', *, *, #30277, .T. ) ;
#9538 = EDGE_CURVE ( 'NONE', #15521, #63292, #16478, .T. ) ;
#9539 = ORIENTED_EDGE ( 'NONE', *, *, #37765, .T. ) ;
#9540 = LINE ( 'NONE', #36267, #46898 ) ;
#9541 = CARTESIAN_POINT ( 'NONE',  ( -118.3971226877368537, 42.93006216270222808, 91.40225232301679625 ) ) ;
#9542 = CARTESIAN_POINT ( 'NONE',  ( -166.5704851812740799, 80.12110537694668722, -19.03004029801454422 ) ) ;
#9543 = CARTESIAN_POINT ( 'NONE',  ( 36.64089410029665572, -65.45232906116368099, 43.58025477438756923 ) ) ;
#9544 = CARTESIAN_POINT ( 'NONE',  ( 20.87035195714981484, 6.716493875830939153, 85.67848478272195223 ) ) ;
#9545 = CARTESIAN_POINT ( 'NONE',  ( 22.95772980082745462, 7.844166310250415108, 88.97759199307637346 ) ) ;
#9546 = ADVANCED_FACE ( 'NONE', ( #48454 ), #33714, .T. ) ;
#9547 = VERTEX_POINT ( 'NONE', #49508 ) ;
#9548 = DIRECTION ( 'NONE',  ( 0.000000000000000000, -1.000000000000000000, 0.000000000000000000 ) ) ;
#9549 = FACE_OUTER_BOUND ( 'NONE', #68436, .T. ) ;
#9550 = ORIENTED_EDGE ( 'NONE', *, *, #39019, .F. ) ;
#9551 = CARTESIAN_POINT ( 'NONE',  ( -83.14462298835726983, 24.07775853418027623, 5.038079082316872181 ) ) ;
#9552 = ORIENTED_EDGE ( 'NONE', *, *, #47627, .F. ) ;
#9553 = CIRCLE ( 'NONE', #33092, 74.95140232871122521 ) ;
#9554 = DIRECTION ( 'NONE',  ( 0.000000000000000000, 0.000000000000000000, -1.000000000000000000 ) ) ;
#9555 = ORIENTED_EDGE ( 'NONE', *, *, #12386, .T. ) ;
#9556 = CIRCLE ( 'NONE', #17419, 85.31295361348101380 ) ;
#9557 = ORIENTED_EDGE ( 'NONE', *, *, #21995, .F. ) ;
#9558 = CARTESIAN_POINT ( 'NONE',  ( 9.823983574062872037, 6.382904402091121199, -47.59236116552792595 ) ) ;
#9559 = CARTESIAN_POINT ( 'NONE',  ( -178.0633751203918962, 92.80295726428049363, 70.81231572743919855 ) ) ;
#9560 = CARTESIAN_POINT ( 'NONE',  ( 132.7179291807800610, 40.74118679001687582, 56.43832664394951593 ) ) ;
#9561 = VECTOR ( 'NONE', #10952, 1000.000000000000000 ) ;
#9562 = CIRCLE ( 'NONE', #38787, 65.36598343705435354 ) ;
#9563 = ORIENTED_EDGE ( 'NONE', *, *, #3366, .F. ) ;
#9564 = AXIS2_PLACEMENT_3D ( 'NONE', #1213, #22666, #1928 ) ;
#9565 = ADVANCED_FACE ( 'NONE', ( #10850 ), #27364, .F. ) ;
#9566 = AXIS2_PLACEMENT_3D ( 'NONE', #5129, #21307, #48708 ) ;
#9567 = CARTESIAN_POINT ( 'NONE',  ( -38.80623589257147898, 10.91725262622218828, 89.96254966543166631 ) ) ;
#9568 = CARTESIAN_POINT ( 'NONE',  ( 173.5844030397475990, 72.71952271766126330, -70.87456350105938441 ) ) ;
#9569 = VECTOR ( 'NONE', #16116, 1000.000000000000000 ) ;
#9570 = CARTESIAN_POINT ( 'NONE',  ( -443.6229740799757906, 394.9118408295729523, -126.2130497528550990 ) ) ;
#9571 = CARTESIAN_POINT ( 'NONE',  ( 107.9301116202191935, 27.82606182274594886, -50.57270492925939465 ) ) ;
#9572 = CARTESIAN_POINT ( 'NONE',  ( 79.33384730094452664, 18.11203072455029073, -45.07922390903824805 ) ) ;
#9573 = CARTESIAN_POINT ( 'NONE',  ( 31.89651141207536256, 56.63578868294628421, 40.00000000000003553 ) ) ;
#9574 = ORIENTED_EDGE ( 'NONE', *, *, #68829, .F. ) ;
#9575 = CARTESIAN_POINT ( 'NONE',  ( -51.66904755831210139, 6.635317295611287136E-14, 85.00100000000000477 ) ) ;
#9576 = CARTESIAN_POINT ( 'NONE',  ( -82.93126516400698733, 25.07709093823495294, -75.63414270348664559 ) ) ;
#9577 = CARTESIAN_POINT ( 'NONE',  ( 180.2494929075577659, 79.18888319146950039, 17.46404351504774866 ) ) ;
#9578 = DIRECTION ( 'NONE',  ( -0.000000000000000000, -0.000000000000000000, -1.000000000000000000 ) ) ;
#9579 = FACE_OUTER_BOUND ( 'NONE', #33902, .T. ) ;
#9580 = CARTESIAN_POINT ( 'NONE',  ( 126.8237978310704221, 37.33705012421152247, 12.78451399988137105 ) ) ;
#9581 = CARTESIAN_POINT ( 'NONE',  ( -155.7433525314458791, 69.65452735858370659, 15.55135967904255168 ) ) ;
#9582 = FACE_OUTER_BOUND ( 'NONE', #17935, .T. ) ;
#9583 = CARTESIAN_POINT ( 'NONE',  ( 205.5130322755755685, 109.1888880665735826, 44.20772073876945285 ) ) ;
#9584 = CARTESIAN_POINT ( 'NONE',  ( -81.01931326044685022, 24.31309346877658584, 71.88812866901480447 ) ) ;
#9585 = CARTESIAN_POINT ( 'NONE',  ( -102.7456062648101778, 33.01749955571778372, 30.51907450641510877 ) ) ;
#9586 = EDGE_LOOP ( 'NONE', ( #6122, #39532 ) ) ;
#9587 = CONTEXT_DEPENDENT_SHAPE_REPRESENTATION ( #66934, #60250 ) ;
#9588 = CARTESIAN_POINT ( 'NONE',  ( -48.08829070713510134, 13.95819972868300418, 88.70444353358108458 ) ) ;
#9589 = ORIENTED_EDGE ( 'NONE', *, *, #36903, .F. ) ;
#9590 = CARTESIAN_POINT ( 'NONE',  ( 7.533997733928853968, 64.93035244659016314, 3.125053320693570118E-16 ) ) ;
#9591 = EDGE_LOOP ( 'NONE', ( #62598, #61913, #37505, #11408, #50798, #48930, #15590, #30937 ) ) ;
#9592 = CARTESIAN_POINT ( 'NONE',  ( 33.18066491647863359, 39.60239344302862463, 26.66469104408689006 ) ) ;
#9593 = FACE_OUTER_BOUND ( 'NONE', #41307, .T. ) ;
#9594 = DIRECTION ( 'NONE',  ( 1.000000000000000000, 0.000000000000000000, 0.000000000000000000 ) ) ;
#9595 = DIRECTION ( 'NONE',  ( 0.000000000000000000, 0.000000000000000000, 1.000000000000000000 ) ) ;
#9596 = CARTESIAN_POINT ( 'NONE',  ( 136.1215428813736708, 43.99260314811117212, -50.68811301310670103 ) ) ;
#9597 = EDGE_CURVE ( 'NONE', #41430, #19049, #287, .T. ) ;
#9598 = CARTESIAN_POINT ( 'NONE',  ( 32.67604596315972287, 7.629767358313822356, -46.44744588816674735 ) ) ;
#9599 = CARTESIAN_POINT ( 'NONE',  ( 427.4999999999999432, 207.5000000000000284, 380.0000000000000000 ) ) ;
#9600 = CARTESIAN_POINT ( 'NONE',  ( 86.62931800182293784, 20.48449268398423229, 44.71208757247933363 ) ) ;
#9601 = LINE ( 'NONE', #31064, #27333 ) ;
#9602 = ORIENTED_EDGE ( 'NONE', *, *, #17786, .T. ) ;
#9603 = ADVANCED_FACE ( 'NONE', ( #6968 ), #21745, .T. ) ;
#9604 = ORIENTED_EDGE ( 'NONE', *, *, #23572, .T. ) ;
#9605 = EDGE_CURVE ( 'NONE', #11859, #49581, #63695, .T. ) ;
#9606 = AXIS2_PLACEMENT_3D ( 'NONE', #25752, #20451, #56362 ) ;
#9607 = DIRECTION ( 'NONE',  ( -0.000000000000000000, -0.000000000000000000, -1.000000000000000000 ) ) ;
#9608 = FACE_OUTER_BOUND ( 'NONE', #62403, .T. ) ;
#9609 = B_SPLINE_CURVE_WITH_KNOTS ( 'NONE', 3,
 ( #55826, #23120, #7646, #35403, #62126, #18881, #61777, #2363, #61445, #23815, #13946, #29097, #28384, #23476, #45257, #2706, #13600, #40330, #55464, #13263, #24167, #7288, #50195, #35058, #34724, #45609, #18534, #44571, #6933, #49831, #66047, #56162, #60743, #67093, #56503, #17841, #39298, #28743, #44915, #66398, #61098, #26228, #9712 ),
 .UNSPECIFIED., .F., .F.,
 ( 4, 2, 2, 2, 2, 2, 2, 2, 2, 2, 2, 2, 1, 2, 2, 2, 2, 2, 2, 2, 2, 4 ),
 ( 0.02358007599568756954, 0.02505677178601666000, 0.02579511968118118961, 0.02653346757634572270, 0.02801016336667479581, 0.02948685915700387239, 0.03022520705216839507, 0.03096355494733291774, 0.03244025073766196310, 0.03391694652799101539, 0.03539364231832005381, 0.03613199021348457995, 0.03687033810864910610, 0.03760868600381363225, 0.03834703389897815146, 0.03982372968930719681, 0.04130042547963624910, 0.04277712126996529446, 0.04351546916512981367, 0.04425381706029432594, 0.04573051285062335047, 0.04720720864095236113 ),
 .UNSPECIFIED. ) ;
#9610 = EDGE_CURVE ( 'NONE', #64530, #23937, #1367, .T. ) ;
#9611 = CARTESIAN_POINT ( 'NONE',  ( 66.50000000000000000, 0.000000000000000000, -0.002000000000002000178 ) ) ;
#9612 = VECTOR ( 'NONE', #27215, 1000.000000000000000 ) ;
#9613 = CARTESIAN_POINT ( 'NONE',  ( 15.29899606819416569, 6.485153354884286792, 3.170157082241544799 ) ) ;
#9614 = CARTESIAN_POINT ( 'NONE',  ( 41.80869235728138023, 9.750404582811610155, -77.08460388544597208 ) ) ;
#9615 = VECTOR ( 'NONE', #7900, 1000.000000000000000 ) ;
#9616 = DIRECTION ( 'NONE',  ( -0.000000000000000000, 0.000000000000000000, -1.000000000000000000 ) ) ;
#9617 = CARTESIAN_POINT ( 'NONE',  ( 210.6592759200688079, 116.7161312026394171, 14.42140922515896584 ) ) ;
#9618 = PLANE ( 'NONE',  #306 ) ;
#9619 = CARTESIAN_POINT ( 'NONE',  ( 93.92910382125423041, 22.04227458821882379, -14.73737663557316857 ) ) ;
#9620 = CARTESIAN_POINT ( 'NONE',  ( -30.46002654261638298, 10.45132580906816067, 57.10924613618367118 ) ) ;
#9621 = CARTESIAN_POINT ( 'NONE',  ( 424.8372781065089043, 400.0000000000000568, -123.9497041420121235 ) ) ;
#9622 = CARTESIAN_POINT ( 'NONE',  ( -49.14234466229833487, 13.17605306081208205, 60.03827907641571215 ) ) ;
#9623 = AXIS2_PLACEMENT_3D ( 'NONE', #40283, #24462, #20205 ) ;
#9624 = AXIS2_PLACEMENT_3D ( 'NONE', #23338, #28241, #65189 ) ;
#9625 = ADVANCED_FACE ( 'NONE', ( #27720 ), #17598, .T. ) ;
#9626 = EDGE_LOOP ( 'NONE', ( #30057, #38468, #49736, #30287 ) ) ;
#9627 = EDGE_CURVE ( 'NONE', #2888, #52414, #27391, .T. ) ;
#9628 = CARTESIAN_POINT ( 'NONE',  ( 131.3924949472282435, 41.12442122814098155, 3.078401348124321757 ) ) ;
#9629 = LINE ( 'NONE', #52527, #42875 ) ;
#9630 = CARTESIAN_POINT ( 'NONE',  ( -55.05276343752908730, 15.72344139423348430, 72.16187836339486239 ) ) ;
#9631 = CARTESIAN_POINT ( 'NONE',  ( -107.7886332494339996, 36.81249801143972178, -64.24604545677848932 ) ) ;
#9632 = CARTESIAN_POINT ( 'NONE',  ( -53.38256734720888375, 14.24001356352780867, -50.03199302348036781 ) ) ;
#9633 = LINE ( 'NONE', #68037, #53713 ) ;
#9634 = CARTESIAN_POINT ( 'NONE',  ( -28.32746765835526048, 69.45586423092609607, 73.58025477438756923 ) ) ;
#9635 = ORIENTED_EDGE ( 'NONE', *, *, #65097, .F. ) ;
#9636 = CARTESIAN_POINT ( 'NONE',  ( -31.43908319763710679, -170.0000000000000000, 30.21645440618916112 ) ) ;
#9637 = CARTESIAN_POINT ( 'NONE',  ( 0.01688885742776671806, 7.321065037175427115, 3.319543390096037605 ) ) ;
#9638 = VERTEX_POINT ( 'NONE', #66433 ) ;
#9639 = ORIENTED_EDGE ( 'NONE', *, *, #18014, .T. ) ;
#9640 = CARTESIAN_POINT ( 'NONE',  ( 34.55626349558410482, 8.840813453039558567, 85.36898312980444814 ) ) ;
#9641 = CARTESIAN_POINT ( 'NONE',  ( 0.000000000000000000, 0.000000000000000000, 0.000000000000000000 ) ) ;
#9642 = CARTESIAN_POINT ( 'NONE',  ( 10.55634918610411432, 51.66904755831205875, 2.000000000000001776 ) ) ;
#9643 = ORIENTED_EDGE ( 'NONE', *, *, #37934, .F. ) ;
#9644 = CARTESIAN_POINT ( 'NONE',  ( 0.000000000000000000, -6.928203230275503444, 4.000000000000010658 ) ) ;
#9645 = LINE ( 'NONE', #15263, #25245 ) ;
#9646 = CARTESIAN_POINT ( 'NONE',  ( 31.99894129856764025, 7.561773404408291377, -17.50242361378957412 ) ) ;
#9647 = CARTESIAN_POINT ( 'NONE',  ( -80.56139928459657540, 24.13290941644246956, 45.17878892873373076 ) ) ;
#9648 = CARTESIAN_POINT ( 'NONE',  ( 161.3124398469970231, 60.70116285586392024, 84.15009968631400739 ) ) ;
#9649 = CARTESIAN_POINT ( 'NONE',  ( 92.51858280840789917, 21.51505926344916020, 32.54138647035420462 ) ) ;
#9650 = ORIENTED_EDGE ( 'NONE', *, *, #43482, .T. ) ;
#9651 = CARTESIAN_POINT ( 'NONE',  ( 104.7227067006896704, 27.50728936118536438, -21.67830293406160891 ) ) ;
#9652 = AXIS2_PLACEMENT_3D ( 'NONE', #15105, #11446, #36563 ) ;
#9653 = CARTESIAN_POINT ( 'NONE',  ( 12.46277766093406569, 6.416700641561363661, 71.09963920718769259 ) ) ;
#9654 = CARTESIAN_POINT ( 'NONE',  ( -190.6985136298601731, 109.1272424661242582, 94.99999999999866418 ) ) ;
#9655 = CARTESIAN_POINT ( 'NONE',  ( 197.5344630110112689, 98.61758706718750034, 34.46336747874654094 ) ) ;
#9656 = DIRECTION ( 'NONE',  ( -0.000000000000000000, -0.000000000000000000, 1.000000000000000000 ) ) ;
#9657 = VECTOR ( 'NONE', #33393, 1000.000000000000000 ) ;
#9659 = ORIENTED_EDGE ( 'NONE', *, *, #26286, .F. ) ;
#9658 = CARTESIAN_POINT ( 'NONE',  ( 157.4703587214989398, -170.0000000000000000, 10.06491688178970456 ) ) ;
#9660 = CARTESIAN_POINT ( 'NONE',  ( -36.61438981621041933, -5.226566692248928447, -54.38561018378954515 ) ) ;
#9661 = ORIENTED_EDGE ( 'NONE', *, *, #8181, .T. ) ;
#9662 = CIRCLE ( 'NONE', #62435, 25.00000000000000000 ) ;
#9663 = VECTOR ( 'NONE', #10297, 1000.000000000000114 ) ;
#9664 = ORIENTED_EDGE ( 'NONE', *, *, #18763, .F. ) ;
#9665 = CARTESIAN_POINT ( 'NONE',  ( 112.1009898303695564, 30.86414810229298311, -62.98576819390486037 ) ) ;
#9666 = DIRECTION ( 'NONE',  ( 1.000000000000000000, 1.131929979755206441E-16, -1.697894969632809662E-16 ) ) ;
#9667 = CARTESIAN_POINT ( 'NONE',  ( 201.5903370237274999, 102.1785392640257726, -77.50997439458886618 ) ) ;
#9668 = AXIS2_PLACEMENT_3D ( 'NONE', #54049, #6227, #49124 ) ;
#9669 = CARTESIAN_POINT ( 'NONE',  ( -36.37229078872272936, 11.47648211215765102, 58.89076057092043470 ) ) ;
#9670 =( BOUNDED_CURVE ( )  B_SPLINE_CURVE ( 3, ( #66116, #44977, #39359, #66459 ),
 .UNSPECIFIED., .F., .F. ) 
 B_SPLINE_CURVE_WITH_KNOTS ( ( 4, 4 ),
 ( 1.570796326794908326, 3.141592653589805106 ),
 .UNSPECIFIED. ) 
 CURVE ( )  GEOMETRIC_REPRESENTATION_ITEM ( )  RATIONAL_B_SPLINE_CURVE ( ( 1.000000000000000000, 0.8047378541243649375, 0.8047378541243649375, 1.000000000000000000 ) ) 
 REPRESENTATION_ITEM ( '' )  );
#9671 = CARTESIAN_POINT ( 'NONE',  ( -118.5043919384111462, 41.81711884544881030, 66.27494688493422359 ) ) ;
#9672 = CARTESIAN_POINT ( 'NONE',  ( -86.16504208171679124, 26.41251233979377133, -16.30058366687843829 ) ) ;
#9673 = CARTESIAN_POINT ( 'NONE',  ( 17.72992212664810197, 6.570588738776103277, -23.42286153992951725 ) ) ;
#9674 = VECTOR ( 'NONE', #6097, 1000.000000000000114 ) ;
#9675 = CARTESIAN_POINT ( 'NONE',  ( -1.224646799147352468E-15, 16.00000000000000000, -5.803681084894614095 ) ) ;
#9676 = ORIENTED_EDGE ( 'NONE', *, *, #21898, .F. ) ;
#9677 = VERTEX_POINT ( 'NONE', #40367 ) ;
#9678 = CARTESIAN_POINT ( 'NONE',  ( -26.83517958587657404, 59.60356471962912650, 43.58025477438756212 ) ) ;
#9679 = CARTESIAN_POINT ( 'NONE',  ( -79.62207341875657107, 23.76621716825512465, -35.16117203328388285 ) ) ;
#9680 = CARTESIAN_POINT ( 'NONE',  ( 163.7607557204680120, 62.71181783708026813, 67.86960462155784057 ) ) ;
#9681 = CARTESIAN_POINT ( 'NONE',  ( 113.8626313173126334, 31.71036178495293711, -9.991941754758171257 ) ) ;
#9682 = CARTESIAN_POINT ( 'NONE',  ( 186.2722199822850655, 84.01218714714251234, -38.28895599514326875 ) ) ;
#9683 = FACE_OUTER_BOUND ( 'NONE', #56398, .T. ) ;
#9684 = CARTESIAN_POINT ( 'NONE',  ( -153.7013249156687777, 69.16788179302882611, 85.68575647905826997 ) ) ;
#9685 = ORIENTED_EDGE ( 'NONE', *, *, #17023, .T. ) ;
#9686 = ORIENTED_EDGE ( 'NONE', *, *, #34175, .T. ) ;
#9687 = EDGE_CURVE ( 'NONE', #24552, #31912, #61812, .T. ) ;
#9688 = ORIENTED_EDGE ( 'NONE', *, *, #60121, .F. ) ;
#9689 = DIRECTION ( 'NONE',  ( 0.000000000000000000, 0.000000000000000000, 1.000000000000000000 ) ) ;
#9690 = EDGE_CURVE ( 'NONE', #17040, #51087, #4727, .T. ) ;
#9691 = DIRECTION ( 'NONE',  ( -0.000000000000000000, -0.000000000000000000, -1.000000000000000000 ) ) ;
#9692 = CARTESIAN_POINT ( 'NONE',  ( 108.7042516502346814, 28.17621584866460438, -89.76095026914288155 ) ) ;
#9693 = EDGE_CURVE ( 'NONE', #14491, #37440, #37155, .T. ) ;
#9694 = CARTESIAN_POINT ( 'NONE',  ( -34.06637338149494099, 11.05895377318623574, -76.69071157721195675 ) ) ;
#9695 = DIRECTION ( 'NONE',  ( 0.000000000000000000, 1.000000000000000000, -0.000000000000000000 ) ) ;
#9696 = CARTESIAN_POINT ( 'NONE',  ( 185.1710994180822638, 84.30654632312740659, 69.95762266168335941 ) ) ;
#9697 = CARTESIAN_POINT ( 'NONE',  ( 46.13705514479446634, 9.381301642376868699, 94.41946954417569771 ) ) ;
#9698 =( LENGTH_UNIT ( ) NAMED_UNIT ( * ) SI_UNIT ( .MILLI., .METRE. ) );
#9699 = LINE ( 'NONE', #15316, #18300 ) ;
#9700 = CARTESIAN_POINT ( 'NONE',  ( 187.2465631085774476, 85.06582225041687195, 67.95777364192932168 ) ) ;
#9701 = CARTESIAN_POINT ( 'NONE',  ( -119.1795380580999932, 42.22910606512927956, 7.923488756519734721 ) ) ;
#9702 = CARTESIAN_POINT ( 'NONE',  ( 0.000000000000000000, 0.000000000000000000, 41.38025477438755928 ) ) ;
#9703 = CARTESIAN_POINT ( 'NONE',  ( 127.4750938923429828, 37.70245908594343121, -20.62732788491080527 ) ) ;
#9704 = CARTESIAN_POINT ( 'NONE',  ( 16.77104078056616743, 7.540619757007628543, -8.723023917128227112 ) ) ;
#9705 = CARTESIAN_POINT ( 'NONE',  ( 12.46490660984525611, 7.423426948220646970, 17.39812806102571230 ) ) ;
#9706 = VECTOR ( 'NONE', #65918, 999.9999999999998863 ) ;
#9707 = ADVANCED_FACE ( 'NONE', ( #42092 ), #3769, .T. ) ;
#9708 = ORIENTED_EDGE ( 'NONE', *, *, #43789, .F. ) ;
#9709 = CARTESIAN_POINT ( 'NONE',  ( 188.0081045302010807, 85.89855126821616693, 7.067797300440569863 ) ) ;
#9710 = APPLICATION_PROTOCOL_DEFINITION ( 'draft international standard', 'automotive_design', 1998, #48477 ) ;
#9711 = CARTESIAN_POINT ( 'NONE',  ( -132.6811329440527061, 51.12842468617797920, 94.99999999999866418 ) ) ;
#9712 = CARTESIAN_POINT ( 'NONE',  ( -31.43908319763710679, 10.61114334766715928, -35.31719736520183517 ) ) ;
#9713 = CARTESIAN_POINT ( 'NONE',  ( -109.7156874346698316, 37.87149323084328500, -41.49882581585664099 ) ) ;
#9714 = CONTEXT_DEPENDENT_SHAPE_REPRESENTATION ( #44513, #10733 ) ;
#9715 = CARTESIAN_POINT ( 'NONE',  ( 185.1660960081724170, 84.30194217633010112, -50.02099752507488262 ) ) ;
#9716 = VERTEX_POINT ( 'NONE', #57241 ) ;
#9717 = AXIS2_PLACEMENT_3D ( 'NONE', #36878, #25295, #57642 ) ;
#9718 = AXIS2_PLACEMENT_3D ( 'NONE', #5384, #63791, #26840 ) ;
#9719 = VERTEX_POINT ( 'NONE', #42437 ) ;
#9720 = DIRECTION ( 'NONE',  ( 1.000000000000000000, 0.000000000000000000, 0.000000000000000000 ) ) ;
#9721 = CARTESIAN_POINT ( 'NONE',  ( 197.6341357773624452, 98.74251867088341328, 12.40192937851051624 ) ) ;
#9722 = ORIENTED_EDGE ( 'NONE', *, *, #37384, .T. ) ;
#9723 = VECTOR ( 'NONE', #7085, 1000.000000000000000 ) ;
#9724 = CARTESIAN_POINT ( 'NONE',  ( 115.0454575488273719, 31.16784721673997893, 58.18990905230850785 ) ) ;
#9725 = B_SPLINE_CURVE_WITH_KNOTS ( 'NONE', 3,
 ( #59985, #5493, #6880, #1258 ),
 .UNSPECIFIED., .F., .F.,
 ( 4, 4 ),
 ( 9.900409499046083621E-07, 0.05658314289920115397 ),
 .UNSPECIFIED. ) ;
#9726 = ORIENTED_EDGE ( 'NONE', *, *, #33020, .T. ) ;
#9727 = CARTESIAN_POINT ( 'NONE',  ( -57.89360549284268131, 16.50663738101750511, 17.92646098985595771 ) ) ;
#9728 = CARTESIAN_POINT ( 'NONE',  ( 133.3990214534117342, 41.14886683286417934, 29.52083177294308669 ) ) ;
#9729 = CARTESIAN_POINT ( 'NONE',  ( -2.609024107869115977E-14, 3.000000000000030198, -46.99999999999997158 ) ) ;
#9730 = CARTESIAN_POINT ( 'NONE',  ( -100.4466073551322722, 31.85873123265079698, 30.73181422168544685 ) ) ;
#9731 = FACE_OUTER_BOUND ( 'NONE', #41243, .T. ) ;
#9733 = ORIENTED_EDGE ( 'NONE', *, *, #53016, .F. ) ;
#9732 = CARTESIAN_POINT ( 'NONE',  ( 209.3223706822284100, -1.426547569622074412E-15, 31.44247402469554942 ) ) ;
#9734 = PLANE ( 'NONE',  #26091 ) ;
#9735 = ORIENTED_EDGE ( 'NONE', *, *, #43488, .F. ) ;
#9736 = ORIENTED_EDGE ( 'NONE', *, *, #9605, .T. ) ;
#9737 = CARTESIAN_POINT ( 'NONE',  ( -120.1497954511983721, 42.82624472369560209, -20.41821900911190113 ) ) ;
#9738 = LINE ( 'NONE', #67202, #34763 ) ;
#9739 = CARTESIAN_POINT ( 'NONE',  ( -174.7869898116916545, 88.99756909636809610, -8.005991368106910144 ) ) ;
#9741 = ORIENTED_EDGE ( 'NONE', *, *, #56244, .T. ) ;
#9740 = CARTESIAN_POINT ( 'NONE',  ( -128.3448054685827628, 49.34430406923178225, 57.87263026190729676 ) ) ;
#9742 = CARTESIAN_POINT ( 'NONE',  ( -109.6883992247426818, 37.85633120528618178, 90.49244489616368980 ) ) ;
#9743 = DIRECTION ( 'NONE',  ( 0.000000000000000000, 0.000000000000000000, 1.000000000000000000 ) ) ;
#9744 = ORIENTED_EDGE ( 'NONE', *, *, #46447, .T. ) ;
#9745 = ADVANCED_FACE ( 'NONE', ( #20987 ), #38953, .T. ) ;
#9746 = CARTESIAN_POINT ( 'NONE',  ( 73.51344971438123821, 14.61114034329559352, 41.38025477438755928 ) ) ;
#9747 = B_SPLINE_CURVE_WITH_KNOTS ( 'NONE', 3,
 ( #29168, #18960, #8409, #35484, #56946, #18615, #39373, #23204, #28468, #60818, #56238, #45694, #12644, #34106, #34463, #61176, #55541, #40069, #46032, #7721, #50617, #7374, #28826, #67173, #50278, #13343, #2100, #23552, #2435, #61525, #44990, #67498, #66471, #8054, #29506, #19295, #50970, #2782, #40406, #56588, #61854, #13677, #29860 ),
 .UNSPECIFIED., .F., .F.,
 ( 4, 2, 2, 2, 2, 2, 2, 2, 2, 2, 2, 1, 2, 2, 2, 2, 2, 2, 2, 2, 2, 4 ),
 ( 0.02515559250233023042, 0.02674001423437968178, 0.02753222510040440746, 0.02832443596642913314, 0.02990885769847851511, 0.03149327943052789708, 0.03307770116257727905, 0.03386991202860197003, 0.03466212289462666796, 0.03624654462667600829, 0.03703875549270066458, 0.03783096635872532781, 0.03862317722474998410, 0.03941538809077464733, 0.04099980982282398767, 0.04258423155487332801, 0.04337644242089799818, 0.04416865328692266834, 0.04575307501897196011, 0.04733749675102125187, 0.04892191848307054364, 0.05050634021511983540 ),
 .UNSPECIFIED. ) ;
#9748 = VECTOR ( 'NONE', #47211, 1000.000000000000000 ) ;
#9749 = CARTESIAN_POINT ( 'NONE',  ( -127.6894679065405143, 48.89973668460848444, -61.96241609914127935 ) ) ;
#9750 = FACE_OUTER_BOUND ( 'NONE', #64777, .T. ) ;
#9751 = CARTESIAN_POINT ( 'NONE',  ( -132.2286325684322605, 52.04087929935081291, 15.29861258695694914 ) ) ;
#9752 = LINE ( 'NONE', #36482, #19412 ) ;
#9753 = ORIENTED_EDGE ( 'NONE', *, *, #48332, .T. ) ;
#9754 = VERTEX_POINT ( 'NONE', #9746 ) ;
#9755 = AXIS2_PLACEMENT_3D ( 'NONE', #25964, #15745, #21029 ) ;
#9756 = DIRECTION ( 'NONE',  ( 0.000000000000000000, 0.000000000000000000, 1.000000000000000000 ) ) ;
#9757 = DIRECTION ( 'NONE',  ( 0.000000000000000000, 0.000000000000000000, -1.000000000000000000 ) ) ;
#9758 = LINE ( 'NONE', #15026, #4834 ) ;
#9759 = AXIS2_PLACEMENT_3D ( 'NONE', #52665, #61834, #13660 ) ;
#9760 = CARTESIAN_POINT ( 'NONE',  ( -9.119248870808011276, 70.00000000000000000, 4.103571619000548232 ) ) ;
#9761 = CARTESIAN_POINT ( 'NONE',  ( -72.78270026377323632, 21.23376443558121451, 42.59545495974758467 ) ) ;
#9762 = CARTESIAN_POINT ( 'NONE',  ( 83.60262962804348774, 18.41036205028015615, 30.34569721731013558 ) ) ;
#9763 = CARTESIAN_POINT ( 'NONE',  ( -148.6409722988650230, 63.44808865916660778, 45.67375462190659618 ) ) ;
#9764 = LINE ( 'NONE', #40721, #40692 ) ;
#9765 = CARTESIAN_POINT ( 'NONE',  ( -166.3175803736862122, 79.86140754556168986, -65.88834115860622376 ) ) ;
#9766 = ORIENTED_EDGE ( 'NONE', *, *, #67198, .F. ) ;
#9767 = CARTESIAN_POINT ( 'NONE',  ( -109.7816385129979153, 36.75776661907243437, -16.17071436857322908 ) ) ;
#9768 = ADVANCED_FACE ( 'NONE', ( #25924 ), #5147, .F. ) ;
#9769 = ORIENTED_EDGE ( 'NONE', *, *, #11261, .T. ) ;
#9771 = AXIS2_PLACEMENT_3D ( 'NONE', #27025, #28067, #33370 ) ;
#9770 = CARTESIAN_POINT ( 'NONE',  ( 433.3728120124414431, 400.0000000000110276, 99.58582976391696207 ) ) ;
#9772 = LINE ( 'NONE', #8746, #66676 ) ;
#9773 = CARTESIAN_POINT ( 'NONE',  ( 62.82395662043622764, -22.24309023158800613, 34.48241823985147647 ) ) ;
#9774 = DIRECTION ( 'NONE',  ( -1.000000000000000000, 0.000000000000000000, 0.000000000000000000 ) ) ;
#9775 = PLANE ( 'NONE',  #21503 ) ;
#9776 = CARTESIAN_POINT ( 'NONE',  ( 36.31593203568479566, 8.028139509847026289, 3.729209276822607944 ) ) ;
#9777 = CARTESIAN_POINT ( 'NONE',  ( -101.8140949286062664, 33.67224128592401655, -61.85912785543960268 ) ) ;
#9778 = EDGE_CURVE ( 'NONE', #42183, #52004, #57564, .T. ) ;
#9779 = CARTESIAN_POINT ( 'NONE',  ( -38.17232309348611352, 11.81874355808867882, -12.63221164914891226 ) ) ;
#9780 = ORIENTED_EDGE ( 'NONE', *, *, #63242, .F. ) ;
#9781 = PLANE ( 'NONE',  #51094 ) ;
#9782 = VERTEX_POINT ( 'NONE', #33284 ) ;
#9783 = CYLINDRICAL_SURFACE ( 'NONE', #49717, 7.500000000000013323 ) ;
#9784 = CARTESIAN_POINT ( 'NONE',  ( -22.17966026246265798, -25.00691441576276475, 6.893342939543525283 ) ) ;
#9785 = CARTESIAN_POINT ( 'NONE',  ( -189.5329886872042948, 107.4958891766010538, 9.446604222255606587 ) ) ;
#9786 = DIRECTION ( 'NONE',  ( 0.000000000000000000, 0.000000000000000000, 1.000000000000000000 ) ) ;
#9787 = CARTESIAN_POINT ( 'NONE',  ( -15.08468253268400616, 7.472949889606721463, -71.71047699793288643 ) ) ;
#9788 = DIRECTION ( 'NONE',  ( -0.000000000000000000, 0.000000000000000000, -1.000000000000000000 ) ) ;
#9789 = CARTESIAN_POINT ( 'NONE',  ( 150.5744176759382640, 53.72473166688030233, -46.58491299805970698 ) ) ;
#9790 = ADVANCED_FACE ( 'NONE', ( #11111 ), #54713, .T. ) ;
#9791 = ORIENTED_EDGE ( 'NONE', *, *, #40759, .T. ) ;
#9792 = B_SPLINE_CURVE_WITH_KNOTS ( 'NONE', 3,
 ( #47738, #15058, #20673, #58637, #37536, #69202, #58987, #21027, #42471, #46717, #3811, #63932, #31928, #15743, #10454, #5191, #64273, #53356, #19996, #10807, #21359, #42806, #25279, #31246, #36168, #52676, #41792, #68191, #52343, #25962, #25628, #42130, #47062, #28023, #17109, #38948, #65678, #49821, #5529, #54040, #54751, #49467, #26981, #17467, #59336 ),
 .UNSPECIFIED., .F., .F.,
 ( 4, 2, 2, 1, 2, 2, 2, 2, 2, 2, 2, 2, 2, 2, 2, 2, 2, 2, 2, 2, 2, 2, 4 ),
 ( 0.02346057189573570734, 0.02492590417315489540, 0.02565857031186449116, 0.02639123645057409040, 0.02712390258928368963, 0.02785656872799328540, 0.02932190100541250469, 0.03005456714412212821, 0.03078723328283175520, 0.03225256556025103694, 0.03298523169896067087, 0.03371789783767031173, 0.03518323011508959347, 0.03664856239250887521, 0.03738122853121851608, 0.03811389466992815694, 0.03957922694734743174, 0.04104455922476671348, 0.04250989150218599522, 0.04324255764089562221, 0.04397522377960524920, 0.04544055605702451706, 0.04690588833444379185 ),
 .UNSPECIFIED. ) ;
#9793 = CARTESIAN_POINT ( 'NONE',  ( -339.7485839210589802, 237.7268033019657878, 598.9431028211000694 ) ) ;
#9794 = DIRECTION ( 'NONE',  ( -1.000000000000000000, 0.000000000000000000, 0.000000000000000000 ) ) ;
#9796 = ADVANCED_FACE ( 'NONE', ( #58949 ), #44154, .F. ) ;
#9795 = CARTESIAN_POINT ( 'NONE',  ( 173.6007744016332310, 72.73482010729016167, -16.29864277669430450 ) ) ;
#9797 = EDGE_CURVE ( 'NONE', #59256, #31208, #60349, .T. ) ;
#9798 = CARTESIAN_POINT ( 'NONE',  ( -108.6622665321722963, 37.28993738537004532, 60.91613424318486381 ) ) ;
#9799 = CARTESIAN_POINT ( 'NONE',  ( -128.3448054685827913, 49.34430406923178225, -49.50557209994745733 ) ) ;
#9800 = ORIENTED_EDGE ( 'NONE', *, *, #50666, .T. ) ;
#9801 = CARTESIAN_POINT ( 'NONE',  ( -180.6021503146988891, 97.45669259943414886, -68.43622221639195402 ) ) ;
#9802 = CARTESIAN_POINT ( 'NONE',  ( -0.3734056954813043117, 6.520221844775925923, -15.09543421113058592 ) ) ;
#9803 = VECTOR ( 'NONE', #1853, 1000.000000000000000 ) ;
#9804 = CARTESIAN_POINT ( 'NONE',  ( 203.1423857108908351, 105.9238244286949708, -24.32896508841773908 ) ) ;
#9805 = CARTESIAN_POINT ( 'NONE',  ( 93.62778197569794258, 21.92873160988601811, -94.18428683514613908 ) ) ;
#9806 = CIRCLE ( 'NONE', #1935, 10.00000000000000000 ) ;
#9807 = CARTESIAN_POINT ( 'NONE',  ( 141.0645618855930650, 45.95036951196544095, 34.87073521758011907 ) ) ;
#9808 = VERTEX_POINT ( 'NONE', #22364 ) ;
#9809 = CARTESIAN_POINT ( 'NONE',  ( 198.3926538463959162, 98.07933330386030946, 40.80849878693443600 ) ) ;
#9810 = CARTESIAN_POINT ( 'NONE',  ( 117.3110050642448527, 32.29133253383015756, -72.82576982094163043 ) ) ;
#9811 = CIRCLE ( 'NONE', #12060, 2.999999999999999112 ) ;
#9812 = CARTESIAN_POINT ( 'NONE',  ( 188.2950976467627129, 87.71503060978554345, 38.89136225366228672 ) ) ;
#9813 = CARTESIAN_POINT ( 'NONE',  ( -26.69131247781301752, 59.26697088776972322, 40.00000000000003553 ) ) ;
#9814 = CARTESIAN_POINT ( 'NONE',  ( 46.68054346512387554, -170.0000000000000000, -95.00000000000133582 ) ) ;
#9815 = AXIS2_PLACEMENT_3D ( 'NONE', #62416, #68714, #42338 ) ;
#9816 = ORIENTED_EDGE ( 'NONE', *, *, #50367, .T. ) ;
#9817 = AXIS2_PLACEMENT_3D ( 'NONE', #20749, #62637, #41866 ) ;
#9818 = CARTESIAN_POINT ( 'NONE',  ( 8.000000000000007105, 249.8719672152120381, 94.99999999999866418 ) ) ;
#9819 = ORIENTED_EDGE ( 'NONE', *, *, #48014, .F. ) ;
#9820 = CIRCLE ( 'NONE', #38991, 74.95140232871122521 ) ;
#9821 = CARTESIAN_POINT ( 'NONE',  ( -77.02372450489325217, 21.70271995013164457, -23.09265542052123976 ) ) ;
#9822 = CARTESIAN_POINT ( 'NONE',  ( 70.38121440378671423, 14.50253793787157619, -68.58809608872070385 ) ) ;
#9823 = CARTESIAN_POINT ( 'NONE',  ( -62.15799747763097827, 16.70234469631019181, 35.36517553705993322 ) ) ;
#9825 = VERTEX_POINT ( 'NONE', #16730 ) ;
#9824 = CARTESIAN_POINT ( 'NONE',  ( 153.4509883044095773, 55.84811350575042610, 3.728611983228252491 ) ) ;
#9826 = CARTESIAN_POINT ( 'NONE',  ( -180.3158531669106708, 95.51092859788505507, 36.18186780709032746 ) ) ;
#9827 = CARTESIAN_POINT ( 'NONE',  ( -55.05276343752909440, 14.68156374112638751, 30.31732777293113301 ) ) ;
#9828 = CARTESIAN_POINT ( 'NONE',  ( 110.2429982417149574, 29.99119854320846201, -50.92243756565370916 ) ) ;
#9829 = VERTEX_POINT ( 'NONE', #26946 ) ;
#9830 = EDGE_CURVE ( 'NONE', #10821, #26782, #9725, .T. ) ;
#9831 = DIRECTION ( 'NONE',  ( -0.8118923937861950435, -0.5838071093367415143, 0.000000000000000000 ) ) ;
#9832 = ADVANCED_FACE ( 'NONE', ( #10766 ), #11445, .F. ) ;
#9833 = CARTESIAN_POINT ( 'NONE',  ( -20.55634918610400419, 15.55634918610405748, 0.000000000000000000 ) ) ;
#9834 = CARTESIAN_POINT ( 'NONE',  ( 138.2204650371258765, 44.12203217345471984, 69.97322756756503281 ) ) ;
#9835 = FACE_OUTER_BOUND ( 'NONE', #136, .T. ) ;
#9836 = CARTESIAN_POINT ( 'NONE',  ( 149.9838583332408177, 52.05699766415860097, 63.22552044860083242 ) ) ;
#9837 = CARTESIAN_POINT ( 'NONE',  ( 94.06416612695406343, 23.16920323269611970, 38.23054147683830450 ) ) ;
#9838 = VERTEX_POINT ( 'NONE', #32576 ) ;
#9839 = CARTESIAN_POINT ( 'NONE',  ( 46.85361596800669304, 10.51535167202353982, 11.55398794432161047 ) ) ;
#9840 = ORIENTED_EDGE ( 'NONE', *, *, #30834, .F. ) ;
#9841 = CARTESIAN_POINT ( 'NONE',  ( 150.2805372522807374, 53.51147386362153924, -14.62797420608141685 ) ) ;
#9842 = CARTESIAN_POINT ( 'NONE',  ( -60.68849253689218415, 16.26481095007954636, 86.51621802059693778 ) ) ;
#9843 = CARTESIAN_POINT ( 'NONE',  ( 105.2529848321548513, 27.73895015262024089, 31.50682025230513972 ) ) ;
#9844 = CARTESIAN_POINT ( 'NONE',  ( 15.55634918610406103, 20.55634918610400064, 85.00100000000000477 ) ) ;
#9845 = CARTESIAN_POINT ( 'NONE',  ( 55.55684455929184651, 11.06550510321506309, 91.85626868916205012 ) ) ;
#9846 = CARTESIAN_POINT ( 'NONE',  ( 181.9411407973024950, 80.91291802046384873, 17.46404351504775221 ) ) ;
#9847 = EDGE_CURVE ( 'NONE', #54476, #45879, #32233, .T. ) ;
#9848 = CARTESIAN_POINT ( 'NONE',  ( 210.4897348480409107, 114.6382060222044856, -48.59704500875022148 ) ) ;
#9849 = B_SPLINE_CURVE_WITH_KNOTS ( 'NONE', 3,
 ( #46714, #52673, #47735, #41789, #53009, #46357, #4498, #19636, #14704, #31243, #51992, #63245, #36165, #25276, #62558, #35826, #57625, #9092, #3808, #68188, #15055, #9436 ),
 .UNSPECIFIED., .F., .F.,
 ( 4, 2, 2, 2, 2, 2, 2, 2, 2, 2, 4 ),
 ( 0.01188903298721832522, 0.01335733661179801766, 0.01409148842408784741, 0.01482564023637767715, 0.01629394386095731409, 0.01702809567324713863, 0.01776224748553696664, 0.01923055111011659490, 0.02069885473469623011, 0.02216715835927585837, 0.02363546198385549010 ),
 .UNSPECIFIED. ) ;
#9850 = CARTESIAN_POINT ( 'NONE',  ( 46.66904755831210139, 4.999999999999909406, 0.000000000000000000 ) ) ;
#9851 = EDGE_CURVE ( 'NONE', #42925, #42894, #53670, .T. ) ;
#9852 = ORIENTED_EDGE ( 'NONE', *, *, #40876, .T. ) ;
#9853 = VECTOR ( 'NONE', #9873, 1000.000000000000227 ) ;
#9854 = LINE ( 'NONE', #31311, #54269 ) ;
#9855 = ORIENTED_EDGE ( 'NONE', *, *, #34557, .T. ) ;
#9856 = CARTESIAN_POINT ( 'NONE',  ( 0.000000000000000000, 0.000000000000000000, 8.000000000000000000 ) ) ;
#9857 = ADVANCED_FACE ( 'NONE', ( #21322 ), #65637, .T. ) ;
#9858 = CARTESIAN_POINT ( 'NONE',  ( 55.52750043885183828, 11.05966813607792609, -70.55512089573974777 ) ) ;
#9859 = VECTOR ( 'NONE', #53368, 1000.000000000000000 ) ;
#9860 = DIRECTION ( 'NONE',  ( 0.000000000000000000, 0.000000000000000000, -1.000000000000000000 ) ) ;
#9861 = FACE_OUTER_BOUND ( 'NONE', #53704, .T. ) ;
#9862 = CARTESIAN_POINT ( 'NONE',  ( -5.276390875695798677, 6.738249428566100541, 84.24366927175032060 ) ) ;
#9863 = ADVANCED_FACE ( 'NONE', ( #21667 ), #42768, .F. ) ;
#9864 = FACE_OUTER_BOUND ( 'NONE', #28830, .T. ) ;
#9865 = ORIENTED_EDGE ( 'NONE', *, *, #29593, .T. ) ;
#9866 = CARTESIAN_POINT ( 'NONE',  ( -440.1146514826279486, 388.0000000000064233, 101.0022254471246441 ) ) ;
#9867 = CARTESIAN_POINT ( 'NONE',  ( 204.6977192012829789, 106.3443248447423315, -90.01503221354893469 ) ) ;
#9868 = ORIENTED_EDGE ( 'NONE', *, *, #57601, .T. ) ;
#9869 = VERTEX_POINT ( 'NONE', #16396 ) ;
#9870 = DIRECTION ( 'NONE',  ( 0.5111246509603011301, 0.000000000000000000, 0.8595065975201763298 ) ) ;
#9871 = CARTESIAN_POINT ( 'NONE',  ( 60.63507185982732040, 12.13307030573224310, -36.10436450079728843 ) ) ;
#9872 = B_SPLINE_CURVE_WITH_KNOTS ( 'NONE', 3,
 ( #24424, #19830, #68366, #36349, #19126, #8932, #30379, #57801, #45866, #62035, #41283, #62742, #35312, #14546, #57457, #433, #42654, #64111, #53189, #64455, #53541, #59509, #58475, #10633, #64808, #48945, #53880, #42314, #37365, #36701, #16608, #5703, #21207, #9965, #31418, #27160 ),
 .UNSPECIFIED., .F., .F.,
 ( 4, 2, 2, 2, 2, 2, 2, 2, 2, 2, 2, 2, 2, 2, 2, 2, 2, 4 ),
 ( 0.000000000000000000, 0.0009802228717936162412, 0.001960445743587232482, 0.002940668615380848724, 0.003920891487174464965, 0.004901114358968081640, 0.005881337230761697447, 0.006371448666658505351, 0.006861560102555313255, 0.007841782974348921256, 0.008822005846142528390, 0.009802228717936137259, 0.01078245158972974439, 0.01176267446152335153, 0.01274289733331695866, 0.01372312020511056579, 0.01470334307690417466, 0.01568356594869778006 ),
 .UNSPECIFIED. ) ;
#9873 = DIRECTION ( 'NONE',  ( -0.9578262852211514300, 1.172998894335282758E-16, 0.2873478855663451625 ) ) ;
#9874 = CARTESIAN_POINT ( 'NONE',  ( -53.17301597236439648, 40.17754241810537508, 34.48241795236665297 ) ) ;
#9875 = VECTOR ( 'NONE', #30686, 1000.000000000000000 ) ;
#9876 = CARTESIAN_POINT ( 'NONE',  ( -142.6264002846224059, 58.55577336362197371, 8.380890507460796002 ) ) ;
#9877 = EDGE_LOOP ( 'NONE', ( #22982, #24362, #53064, #14384 ) ) ;
#9878 = ADVANCED_FACE ( 'NONE', ( #27283 ), #37849, .F. ) ;
#9879 = EDGE_CURVE ( 'NONE', #44841, #47929, #65278, .T. ) ;
#9880 = CARTESIAN_POINT ( 'NONE',  ( -132.2286325684321753, 52.04087929935079160, 42.14316317742062523 ) ) ;
#9881 = ORIENTED_EDGE ( 'NONE', *, *, #7578, .T. ) ;
#9882 = CARTESIAN_POINT ( 'NONE',  ( 17.73567516211396011, 7.577454475141603751, -50.27825812027533914 ) ) ;
#9883 = CARTESIAN_POINT ( 'NONE',  ( -145.3233446620410518, 62.00659513626053609, 44.46214151374382340 ) ) ;
#9884 = CARTESIAN_POINT ( 'NONE',  ( 207.8484262634767958, 110.7633525054914685, 29.88871051959747049 ) ) ;
#9885 = CARTESIAN_POINT ( 'NONE',  ( -5.417282889646090283, 7.753782747238992634, 71.56727370822876821 ) ) ;
#9886 = ADVANCED_FACE ( 'NONE', ( #5827 ), #43459, .F. ) ;
#9887 = EDGE_LOOP ( 'NONE', ( #40031, #63016, #43313 ) ) ;
#9888 = ORIENTED_EDGE ( 'NONE', *, *, #67535, .T. ) ;
#9889 = CARTESIAN_POINT ( 'NONE',  ( 412.3372781065086770, 0.000000000000000000, -146.4497041420118251 ) ) ;
#9890 = CARTESIAN_POINT ( 'NONE',  ( -132.9421279255324180, 52.54859020878311782, 94.39416510571184915 ) ) ;
#9891 = CARTESIAN_POINT ( 'NONE',  ( 33.44035656425387515, 8.720466003183664938, -65.38726348901131757 ) ) ;
#9892 = CARTESIAN_POINT ( 'NONE',  ( -9.964117946888929822, -64.24592483216726180, 170.0000000000000000 ) ) ;
#9893 = CARTESIAN_POINT ( 'NONE',  ( -67.03031041878421092, -33.66749151869542089, 170.0000000000000000 ) ) ;
#9894 = CARTESIAN_POINT ( 'NONE',  ( 8.312979081382955826, 7.382612536522051627, 91.89463208679092077 ) ) ;
#9895 = VERTEX_POINT ( 'NONE', #49076 ) ;
#9896 = FACE_OUTER_BOUND ( 'NONE', #1961, .T. ) ;
#9897 = CYLINDRICAL_SURFACE ( 'NONE', #31651, 21.99999999999998579 ) ;
#9898 = EDGE_LOOP ( 'NONE', ( #63134, #43456, #20793, #28046 ) ) ;
#9900 = CARTESIAN_POINT ( 'NONE',  ( -85.75222301046100881, 25.14826148333819233, 13.58240162667133433 ) ) ;
#9899 = AXIS2_PLACEMENT_3D ( 'NONE', #1840, #23637, #61610 ) ;
#9901 = ORIENTED_EDGE ( 'NONE', *, *, #50361, .F. ) ;
#9902 =( REPRESENTATION_RELATIONSHIP ('NONE','NONE', #40274, #64096 ) REPRESENTATION_RELATIONSHIP_WITH_TRANSFORMATION ( #14975 )SHAPE_REPRESENTATION_RELATIONSHIP( ) );
#9903 = ORIENTED_EDGE ( 'NONE', *, *, #60097, .T. ) ;
#9904 = AXIS2_PLACEMENT_3D ( 'NONE', #1, #63088, #57129 ) ;
#9905 = EDGE_LOOP ( 'NONE', ( #64861, #51171, #32704, #4194 ) ) ;
#9906 = CARTESIAN_POINT ( 'NONE',  ( 11.21387192505586583, 6.397095920409658909, -48.98246565900599592 ) ) ;
#9907 = CARTESIAN_POINT ( 'NONE',  ( -173.1211646369891355, 87.12891641440857882, 72.66624519710475738 ) ) ;
#9908 = CIRCLE ( 'NONE', #8813, 125.0000000000000000 ) ;
#9909 = CARTESIAN_POINT ( 'NONE',  ( 129.4987365823222376, 38.85470922756775991, 57.74612764648421859 ) ) ;
#9910 = ORIENTED_EDGE ( 'NONE', *, *, #43805, .F. ) ;
#9911 = CARTESIAN_POINT ( 'NONE',  ( -26.69041786375498759, 8.859891017920633161, 85.59129543098580939 ) ) ;
#9912 = VECTOR ( 'NONE', #23444, 1000.000000000000000 ) ;
#9913 = ADVANCED_FACE ( 'NONE', ( #38905 ), #12170, .F. ) ;
#9914 = FACE_OUTER_BOUND ( 'NONE', #45544, .T. ) ;
#9915 = CARTESIAN_POINT ( 'NONE',  ( 69.77839676787897361, -27.52340539439948586, 43.58025477438756212 ) ) ;
#9916 = DIRECTION ( 'NONE',  ( -0.000000000000000000, 1.000000000000000000, -0.000000000000000000 ) ) ;
#9917 = DIRECTION ( 'NONE',  ( 1.000000000000000000, 0.000000000000000000, 0.000000000000000000 ) ) ;
#9918 = CARTESIAN_POINT ( 'NONE',  ( -142.0729208125266325, 59.40063722436773475, -68.01976547901179515 ) ) ;
#9919 = ORIENTED_EDGE ( 'NONE', *, *, #8341, .T. ) ;
#9920 = CARTESIAN_POINT ( 'NONE',  ( 100.0000000000000284, 5.000000000000000000, 18.50000000000000000 ) ) ;
#9921 = CARTESIAN_POINT ( 'NONE',  ( -86.10360257264201778, 26.38663017581291115, -68.45782834547087248 ) ) ;
#9922 = CARTESIAN_POINT ( 'NONE',  ( -3.000000000000002665, 0.000000000000000000, 0.000000000000000000 ) ) ;
#9923 = LINE ( 'NONE', #31378, #51446 ) ;
#9924 = CARTESIAN_POINT ( 'NONE',  ( 31.11269837220803325, -15.55634918610409656, 0.000000000000000000 ) ) ;
#9925 = CARTESIAN_POINT ( 'NONE',  ( 126.3541873520043737, 37.07520218256171063, 9.666275146592695933 ) ) ;
#9926 = CARTESIAN_POINT ( 'NONE',  ( 49.76301652092167416, 41.81676920493115546, 40.00000000000003553 ) ) ;
#9927 = EDGE_CURVE ( 'NONE', #41004, #68538, #45854, .T. ) ;
#9928 = CARTESIAN_POINT ( 'NONE',  ( -84.49322488516129681, 0.000000000000000000, 43.58025477438756212 ) ) ;
#9929 = DIRECTION ( 'NONE',  ( -0.000000000000000000, -0.000000000000000000, 1.000000000000000000 ) ) ;
#9930 = CARTESIAN_POINT ( 'NONE',  ( 164.4615316623334991, 63.29763980349835606, 7.335938463145385668 ) ) ;
#9931 = DIRECTION ( 'NONE',  ( -0.2225209339563042066, -0.9749279121818259508, 0.000000000000000000 ) ) ;
#9932 = ORIENTED_EDGE ( 'NONE', *, *, #24558, .T. ) ;
#9933 = CARTESIAN_POINT ( 'NONE',  ( -53.82112958582657569, 15.39502561506177436, 84.10151456793303737 ) ) ;
#9934 = VERTEX_POINT ( 'NONE', #29730 ) ;
#9935 = EDGE_CURVE ( 'NONE', #1535, #22014, #40153, .T. ) ;
#9936 = CARTESIAN_POINT ( 'NONE',  ( -442.6627218934912662, 394.9999999999998295, 92.24186470396634263 ) ) ;
#9937 = VERTEX_POINT ( 'NONE', #28698 ) ;
#9938 = ADVANCED_FACE ( 'NONE', ( #23430 ), #29384, .F. ) ;
#9939 = CARTESIAN_POINT ( 'NONE',  ( 18.19858669090299585, 7.596860100017450712, -62.75709018195347966 ) ) ;
#9940 = DIRECTION ( 'NONE',  ( 1.000000000000000000, 0.000000000000000000, 0.000000000000000000 ) ) ;
#9941 = CARTESIAN_POINT ( 'NONE',  ( -167.6524579626394882, 82.69702609844095775, 33.18325406944033062 ) ) ;
#9942 = CARTESIAN_POINT ( 'NONE',  ( -305.1627218934913230, 399.9999999999997726, 1.050295857988214898 ) ) ;
#9943 = CARTESIAN_POINT ( 'NONE',  ( 136.7507824285648894, 44.38599729999916121, -36.60034384241509997 ) ) ;
#9944 = CARTESIAN_POINT ( 'NONE',  ( 38.42384008295178432, 8.283891555743467805, -35.66795922405820818 ) ) ;
#9945 = CARTESIAN_POINT ( 'NONE',  ( 154.0401952541423327, 55.03227529428315279, -36.95059798010156271 ) ) ;
#9946 = LINE ( 'NONE', #56481, #54324 ) ;
#9947 = PLANE ( 'NONE',  #20610 ) ;
#9948 = ORIENTED_EDGE ( 'NONE', *, *, #20809, .F. ) ;
#9949 = VERTEX_POINT ( 'NONE', #51195 ) ;
#9950 = AXIS2_PLACEMENT_3D ( 'NONE', #28749, #6938, #12221 ) ;
#9951 = CARTESIAN_POINT ( 'NONE',  ( 174.4872540107491830, 73.56684916581080813, 86.85688443472005815 ) ) ;
#9952 = DIRECTION ( 'NONE',  ( -1.000000000000000000, 0.000000000000000000, 0.000000000000000000 ) ) ;
#9953 = CARTESIAN_POINT ( 'NONE',  ( -7.329206686002009974E-14, -46.66904755831211560, 2.000000000000001776 ) ) ;
#9954 = AXIS2_PLACEMENT_3D ( 'NONE', #6517, #12491, #64560 ) ;
#9955 = PRODUCT_DEFINITION_CONTEXT ( 'detailed design', #26937, 'design' ) ;
#9956 = CARTESIAN_POINT ( 'NONE',  ( 417.3372781065086201, 399.9999999999998863, 108.5502958579881891 ) ) ;
#9957 = EDGE_CURVE ( 'NONE', #67298, #12758, #18832, .T. ) ;
#9958 = CIRCLE ( 'NONE', #63879, 74.95140232871122521 ) ;
#9959 = CARTESIAN_POINT ( 'NONE',  ( 284.8405205227987835, 21.96421596965998901, 1.294720749503649015 ) ) ;
#9960 = CARTESIAN_POINT ( 'NONE',  ( 15.55634918610397399, -31.11269837220809364, 2.000000000000001776 ) ) ;
#9961 = CARTESIAN_POINT ( 'NONE',  ( 175.5406524085946671, 73.17873692326780599, -75.64701513590247828 ) ) ;
#9962 = DIRECTION ( 'NONE',  ( 0.000000000000000000, 0.000000000000000000, 1.000000000000000000 ) ) ;
#9963 = CARTESIAN_POINT ( 'NONE',  ( 91.49345572560146422, 21.13836538408680354, -22.19096141595985827 ) ) ;
#9964 = FACE_OUTER_BOUND ( 'NONE', #66239, .T. ) ;
#9965 = CARTESIAN_POINT ( 'NONE',  ( 109.3411025683418529, 21.43200632497275038, -4.967238636669211616 ) ) ;
#9966 = EDGE_CURVE ( 'NONE', #52761, #36484, #3008, .T. ) ;
#9967 = CARTESIAN_POINT ( 'NONE',  ( 158.3636111008086402, 59.62671916656142912, 71.25401806271710825 ) ) ;
#9968 = VERTEX_POINT ( 'NONE', #19169 ) ;
#9969 = CARTESIAN_POINT ( 'NONE',  ( 127.2107679985236501, 38.70844091144999055, 13.68070527223361665 ) ) ;
#9970 = CARTESIAN_POINT ( 'NONE',  ( 0.000000000000000000, 0.000000000000000000, -33.00000000000000000 ) ) ;
#9971 = B_SPLINE_CURVE_WITH_KNOTS ( 'NONE', 3,
 ( #1297, #39285, #18521, #18175, #60727, #61761, #29419, #39625, #62110, #50179, #13249, #34007, #29762, #23462, #45242, #12547, #29082, #3380, #61081, #67077, #51573, #50528, #56849, #13928, #50868, #12908, #40315, #45939, #23800, #35390, #61429, #34364, #51224, #45592, #56146, #34709, #8666, #18867, #28728, #7964, #55446, #66723, #56488 ),
 .UNSPECIFIED., .F., .F.,
 ( 4, 2, 2, 2, 2, 2, 2, 2, 2, 2, 2, 2, 1, 2, 2, 2, 2, 2, 2, 2, 2, 4 ),
 ( 0.02379577142314828753, 0.02527778373276530488, 0.02601878988757380315, 0.02675979604238230489, 0.02824180835199932571, 0.02972382066161635347, 0.03046482681642485868, 0.03120583297123336736, 0.03268784528085037777, 0.03416985759046738125, 0.03565186990008439166, 0.03639287605489288646, 0.03713388220970138126, 0.03787488836450987606, 0.03861589451931837086, 0.04009790682893536046, 0.04157991913855234312, 0.04306193144816933271, 0.04380293760297783445, 0.04454394375778632231, 0.04602595606740331191, 0.04750796837702030151 ),
 .UNSPECIFIED. ) ;
#9972 = CARTESIAN_POINT ( 'NONE',  ( 144.4165763529819344, -26.99999999999998224, 138.9999999999999716 ) ) ;
#9973 = CARTESIAN_POINT ( 'NONE',  ( -106.6711220790662935, 36.20923238211248929, -75.44417277361526430 ) ) ;
#9974 = CARTESIAN_POINT ( 'NONE',  ( -47.80193682758674356, 12.85650137125658077, -44.69689073443416305 ) ) ;
#9975 = CARTESIAN_POINT ( 'NONE',  ( -7.504072346567051355, 7.878344583761114350, 83.80449388539848599 ) ) ;
#9976 = B_SPLINE_CURVE_WITH_KNOTS ( 'NONE', 3,
 ( #30837, #25222, #13958, #30484, #25567, #41731, #50901, #35417, #46655, #24867, #56884, #8697, #52281, #63189, #51600, #3408, #36453, #57906, #41038, #35772, #24180, #68133, #62847, #36112, #47005, #40345, #68465, #67104, #61792, #35069, #10393, #21303, #25905, #16022, #10744, #63529, #53296, #69135, #37133, #20964, #36803, #5122, #63876, #9728, #4443, #47677 ),
 .UNSPECIFIED., .F., .F.,
 ( 4, 2, 2, 2, 2, 2, 2, 2, 2, 2, 2, 2, 2, 2, 2, 2, 2, 2, 2, 2, 2, 2, 4 ),
 ( 3.179800655392250756E-17, 0.001572224531395685155, 0.003144449062791338217, 0.004716673594186991496, 0.006288898125582645209, 0.007861122656978298054, 0.009433347188373950032, 0.01021945945407176301, 0.01100557171976957599, 0.01179168398546738897, 0.01257779625116520195, 0.01415002078256084699, 0.01493613304825866690, 0.01572224531395648855, 0.01650835757965430847, 0.01729446984535213186, 0.01886669437674773700, 0.01965280664244555345, 0.02043891890814336990, 0.02201114343953899585, 0.02358336797093462528, 0.02436948023663244867, 0.02515559250233026511 ),
 .UNSPECIFIED. ) ;
#9977 = ORIENTED_EDGE ( 'NONE', *, *, #39148, .T. ) ;
#9978 = CARTESIAN_POINT ( 'NONE',  ( 0.000000000000000000, 0.000000000000000000, -33.00000000000000000 ) ) ;
#9979 = CARTESIAN_POINT ( 'NONE',  ( -60.13226458141419073, 16.10241298991027037, 70.18533255850762487 ) ) ;
#9980 = ORIENTED_EDGE ( 'NONE', *, *, #39856, .F. ) ;
#9981 = ORIENTED_EDGE ( 'NONE', *, *, #936, .F. ) ;
#9982 = CARTESIAN_POINT ( 'NONE',  ( 46.23891277379962617, 10.41636740230860525, 88.00200862900838672 ) ) ;
#9983 = CARTESIAN_POINT ( 'NONE',  ( -174.7800083645696532, 88.99302808536934606, -76.38271240644930060 ) ) ;
#9984 = DIRECTION ( 'NONE',  ( 0.8660254037844433705, 0.000000000000000000, -0.4999999999999918954 ) ) ;
#9985 = EDGE_LOOP ( 'NONE', ( #38162, #68083 ) ) ;
#9986 = FACE_OUTER_BOUND ( 'NONE', #45980, .T. ) ;
#9987 = CARTESIAN_POINT ( 'NONE',  ( 0.000000000000000000, 0.000000000000000000, 41.38025477438755928 ) ) ;
#9988 = CARTESIAN_POINT ( 'NONE',  ( 33.76124497394584978, 7.742545529019359662, -11.30815924838790743 ) ) ;
#9989 = CARTESIAN_POINT ( 'NONE',  ( 175.0634607207819329, 74.11351956991634893, -39.24529874372897353 ) ) ;
#9990 = CARTESIAN_POINT ( 'NONE',  ( 55.00000000000000000, 16.00000000000000000, -5.803681084894614095 ) ) ;
#9991 = PRODUCT_DEFINITION ( 'UNKNOWN', '', #23172, #27497 ) ;
#9992 = CARTESIAN_POINT ( 'NONE',  ( 204.6977192012829789, 106.3443248447423599, -24.48138044215792419 ) ) ;
#9993 = EDGE_CURVE ( 'NONE', #26796, #35022, #9820, .T. ) ;
#9994 = ORIENTED_EDGE ( 'NONE', *, *, #48174, .F. ) ;
#9995 = CARTESIAN_POINT ( 'NONE',  ( 109.3154830994003390, 29.56170298203817381, -24.03505716380648138 ) ) ;
#9996 = EDGE_CURVE ( 'NONE', #19095, #33531, #42012, .T. ) ;
#9997 = CYLINDRICAL_SURFACE ( 'NONE', #58334, 74.99999999999998579 ) ;
#9998 = CARTESIAN_POINT ( 'NONE',  ( 8.540564391411908929, 7.383006541823029067, 35.57011664530912753 ) ) ;
#9999 = CARTESIAN_POINT ( 'NONE',  ( 200.4574930424075205, 102.3536505870638251, 42.91127342808825063 ) ) ;
#10000 = VECTOR ( 'NONE', #66938, 1000.000000000000000 ) ;
#10001 = VECTOR ( 'NONE', #51518, 1000.000000000000000 ) ;
#10002 = DIRECTION ( 'NONE',  ( -0.000000000000000000, -0.000000000000000000, 1.000000000000000000 ) ) ;
#10004 = VERTEX_POINT ( 'NONE', #47278 ) ;
#10003 = DIRECTION ( 'NONE',  ( 1.000000000000000000, 0.000000000000000000, 1.337618101958020291E-16 ) ) ;
#10005 = ORIENTED_EDGE ( 'NONE', *, *, #45518, .T. ) ;
#10006 =( GEOMETRIC_REPRESENTATION_CONTEXT ( 3 ) GLOBAL_UNCERTAINTY_ASSIGNED_CONTEXT ( ( #7182 ) ) GLOBAL_UNIT_ASSIGNED_CONTEXT ( ( #26664, #21379, #264 ) ) REPRESENTATION_CONTEXT ( 'NONE', 'WORKASPACE' ) );
#10007 = ORIENTED_EDGE ( 'NONE', *, *, #56079, .F. ) ;
#10008 = LINE ( 'NONE', #20903, #62599 ) ;
#10009 = DIRECTION ( 'NONE',  ( -1.000000000000000000, 0.000000000000000000, 0.000000000000000000 ) ) ;
#10010 = EDGE_CURVE ( 'NONE', #964, #21211, #8679, .T. ) ;
#10011 = LINE ( 'NONE', #53586, #17031 ) ;
#10012 = DIRECTION ( 'NONE',  ( 1.000000000000000000, 0.000000000000000000, 0.000000000000000000 ) ) ;
#10013 = CARTESIAN_POINT ( 'NONE',  ( 151.6192474229130198, 53.24103268919213860, -75.16762133081471120 ) ) ;
#10014 = CARTESIAN_POINT ( 'NONE',  ( 0.000000000000000000, 0.000000000000000000, -2.000000000000000000 ) ) ;
#10015 = CARTESIAN_POINT ( 'NONE',  ( -153.5002794404625490, 67.64160439471096709, -48.66572705198576188 ) ) ;
#10016 = EDGE_LOOP ( 'NONE', ( #950, #60613 ) ) ;
#10017 = ADVANCED_FACE ( 'NONE', ( #15627 ), #14253, .F. ) ;
#10018 = EDGE_LOOP ( 'NONE', ( #13039, #38080, #26577, #24138 ) ) ;
#10019 = ADVANCED_FACE ( 'NONE', ( #30776 ), #69069, .F. ) ;
#10020 = CARTESIAN_POINT ( 'NONE',  ( 410.0000000000000000, 0.000000000000000000, 2.000000000000000000 ) ) ;
#10021 = CARTESIAN_POINT ( 'NONE',  ( -81.24432217070638274, 24.40203426192924852, -35.56837079089353182 ) ) ;
#10022 = CARTESIAN_POINT ( 'NONE',  ( 163.1495034066983862, 62.20479872133083887, 68.67890006866612396 ) ) ;
#10023 = CARTESIAN_POINT ( 'NONE',  ( -156.7435307435794130, 71.93726016406968427, 9.383933217110650205 ) ) ;
#10024 = PLANE ( 'NONE',  #29251 ) ;
#10025 = FACE_OUTER_BOUND ( 'NONE', #69535, .T. ) ;
#10026 = CARTESIAN_POINT ( 'NONE',  ( 57.30278335769610010, -48.40406511297319980, 170.0000000000000000 ) ) ;
#10027 = VERTEX_POINT ( 'NONE', #25162 ) ;
#10028 = ORIENTED_EDGE ( 'NONE', *, *, #60738, .T. ) ;
#10029 = VERTEX_POINT ( 'NONE', #68730 ) ;
#10030 = CARTESIAN_POINT ( 'NONE',  ( 32.90051628396145134, 8.664124555952449569, -46.89117901519352927 ) ) ;
#10031 = PLANE ( 'NONE',  #33315 ) ;
#10032 = CARTESIAN_POINT ( 'NONE',  ( -33.83721310978700814, 11.01869210665939569, -76.77220433069990690 ) ) ;
#10033 = CARTESIAN_POINT ( 'NONE',  ( 197.5344630110112973, 98.61758706718748613, 61.30791806921028808 ) ) ;
#10034 = ORIENTED_EDGE ( 'NONE', *, *, #14314, .T. ) ;
#10035 = CARTESIAN_POINT ( 'NONE',  ( 35.65775178405256440, 7.951994368745589625, 57.75521004793950652 ) ) ;
#10036 = CARTESIAN_POINT ( 'NONE',  ( -173.1211646369891355, -170.0000000000000000, -69.05650775521368701 ) ) ;
#10037 = CARTESIAN_POINT ( 'NONE',  ( -6.840981040171508099, 6.828436339979229608, -35.46654583414340323 ) ) ;
#10038 = CARTESIAN_POINT ( 'NONE',  ( 0.000000000000000000, 5.000000000000000000, 85.00100000000000477 ) ) ;
#10039 = CARTESIAN_POINT ( 'NONE',  ( 6.689127551062003185, 5.375634714784618851, -0.3173508448886520061 ) ) ;
#10040 = CARTESIAN_POINT ( 'NONE',  ( 0.000000000000000000, 0.000000000000000000, 40.00000000000003553 ) ) ;
#10041 = CARTESIAN_POINT ( 'NONE',  ( -23.85457283326439182, 7.880174245944055578, 0.000000000000000000 ) ) ;
#10042 = DIRECTION ( 'NONE',  ( 0.000000000000000000, 0.000000000000000000, 1.000000000000000000 ) ) ;
#10043 = CARTESIAN_POINT ( 'NONE',  ( 10.83521140779424385, 7.398743030771590234, 5.017172746912176962 ) ) ;
#10044 = VECTOR ( 'NONE', #69152, 1000.000000000000000 ) ;
#10045 = ORIENTED_EDGE ( 'NONE', *, *, #23759, .T. ) ;
#10046 = CARTESIAN_POINT ( 'NONE',  ( 181.5127080940606845, 79.03904173130086974, 17.46404351504774510 ) ) ;
#10047 = PRODUCT_CONTEXT ( 'NONE', #32296, 'mechanical' ) ;
#10048 = CARTESIAN_POINT ( 'NONE',  ( 175.8855729601531834, 73.50624012737691260, 31.38118644907393673 ) ) ;
#10049 = DIRECTION ( 'NONE',  ( -0.000000000000000000, -0.000000000000000000, 1.000000000000000000 ) ) ;
#10050 = DIRECTION ( 'NONE',  ( 0.000000000000000000, 0.000000000000000000, 1.000000000000000000 ) ) ;
#10051 = VECTOR ( 'NONE', #40595, 1000.000000000000000 ) ;
#10052 = CARTESIAN_POINT ( 'NONE',  ( 188.2950976467627129, 87.71503060978560029, -41.64228951772874154 ) ) ;
#10053 = ORIENTED_EDGE ( 'NONE', *, *, #15518, .T. ) ;
#10054 = ORIENTED_EDGE ( 'NONE', *, *, #46476, .F. ) ;
#10055 = CYLINDRICAL_SURFACE ( 'NONE', #17941, 200.0000000000000000 ) ;
#10056 = CARTESIAN_POINT ( 'NONE',  ( 173.6797811602132811, 71.43321480276107138, 89.28613363591487939 ) ) ;
#10057 = VERTEX_POINT ( 'NONE', #36395 ) ;
#10058 = CARTESIAN_POINT ( 'NONE',  ( 112.7784411285249035, 30.07270878825233140, 56.89340532513772786 ) ) ;
#10059 = ORIENTED_EDGE ( 'NONE', *, *, #9879, .F. ) ;
#10060 = CARTESIAN_POINT ( 'NONE',  ( 128.0540543950622521, 39.18660671946769014, -65.58941647092106564 ) ) ;
#10061 = CARTESIAN_POINT ( 'NONE',  ( 8.000000000000007105, 249.8719672152120381, 94.99999999999866418 ) ) ;
#10062 = DIRECTION ( 'NONE',  ( 1.000000000000000000, -0.000000000000000000, 0.000000000000000000 ) ) ;
#10063 = AXIS2_PLACEMENT_3D ( 'NONE', #42440, #21325, #58605 ) ;
#10065 = EDGE_CURVE ( 'NONE', #16002, #47540, #27781, .T. ) ;
#10064 = CARTESIAN_POINT ( 'NONE',  ( 160.3358006062388199, 59.91363101085903509, -90.37214895256691705 ) ) ;
#10066 = CARTESIAN_POINT ( 'NONE',  ( 94.12811352634518869, 22.11743943276050217, -43.84554527026892146 ) ) ;
#10068 = EDGE_LOOP ( 'NONE', ( #22843, #39530, #33720, #46263 ) ) ;
#10067 = LINE ( 'NONE', #47681, #47701 ) ;
#10069 = CARTESIAN_POINT ( 'NONE',  ( 7.484861546145933353, -64.56761454192826477, 40.00000000000003553 ) ) ;
#10070 = EDGE_CURVE ( 'NONE', #11364, #8050, #65973, .T. ) ;
#10071 = ORIENTED_EDGE ( 'NONE', *, *, #19714, .T. ) ;
#10072 = ORIENTED_EDGE ( 'NONE', *, *, #55049, .T. ) ;
#10073 = CARTESIAN_POINT ( 'NONE',  ( -119.5576859660651365, 42.46117483543969939, -19.59024322217818792 ) ) ;
#10074 = ADVANCED_FACE ( 'NONE', ( #46590 ), #52220, .F. ) ;
#10075 = DIRECTION ( 'NONE',  ( -0.4738686624729966379, -0.8805955318567391110, 0.000000000000000000 ) ) ;
#10076 = CARTESIAN_POINT ( 'NONE',  ( -180.5230320745700681, 95.76406004447549947, -16.61624996634525786 ) ) ;
#10078 = ORIENTED_EDGE ( 'NONE', *, *, #33445, .F. ) ;
#10077 = DIRECTION ( 'NONE',  ( -0.000000000000000000, -0.000000000000000000, -1.000000000000000000 ) ) ;
#10079 = CARTESIAN_POINT ( 'NONE',  ( -109.2878468539942816, 37.63446276172139449, 94.40069165669748941 ) ) ;
#10080 = EDGE_CURVE ( 'NONE', #29635, #60780, #19519, .T. ) ;
#10081 = AXIS2_PLACEMENT_3D ( 'NONE', #28798, #33727, #49888 ) ;
#10082 = ORIENTED_EDGE ( 'NONE', *, *, #1936, .F. ) ;
#10083 = CARTESIAN_POINT ( 'NONE',  ( -60.97727891098333686, 16.35024395194893287, -20.49696293675446412 ) ) ;
#10084 = CARTESIAN_POINT ( 'NONE',  ( 64.08056813503712590, -12.89932471814424630, 6.377659838150142091E-18 ) ) ;
#10085 = DIRECTION ( 'NONE',  ( -0.000000000000000000, -0.000000000000000000, -1.000000000000000000 ) ) ;
#10086 = CARTESIAN_POINT ( 'NONE',  ( -94.85061234775062644, 29.16417548023187223, 10.11651724366670457 ) ) ;
#10087 = CARTESIAN_POINT ( 'NONE',  ( -98.69283175933883001, 30.99524616306738523, -75.96291905404460465 ) ) ;
#10088 = ORIENTED_EDGE ( 'NONE', *, *, #2190, .F. ) ;
#10089 = EDGE_CURVE ( 'NONE', #61561, #24336, #57847, .T. ) ;
#10090 = ORIENTED_EDGE ( 'NONE', *, *, #39111, .T. ) ;
#10091 = AXIS2_PLACEMENT_3D ( 'NONE', #19078, #25063, #20119 ) ;
#10092 = CARTESIAN_POINT ( 'NONE',  ( 47.99999999999997158, 19.99999999999996447, 4.000000000000000000 ) ) ;
#10093 = CARTESIAN_POINT ( 'NONE',  ( -166.3188283541502699, 79.86268666707378827, -45.38284161879311540 ) ) ;
#10094 = CARTESIAN_POINT ( 'NONE',  ( 50.98853755884132255, 395.0000000000004547, 91.05029585798797598 ) ) ;
#10095 = CIRCLE ( 'NONE', #43771, 4.999999999999997335 ) ;
#10096 = B_SPLINE_CURVE_WITH_KNOTS ( 'NONE', 3,
 ( #33418, #17209, #1751, #28832, #23212, #60483 ),
 .UNSPECIFIED., .F., .F.,
 ( 4, 2, 4 ),
 ( 1.095770181117027441E-06, 0.03239442681617711595, 0.06478775786217311206 ),
 .UNSPECIFIED. ) ;
#10097 = DIRECTION ( 'NONE',  ( 0.8345732537212999791, 0.5508969814521065267, 5.102127870520020458E-18 ) ) ;
#10098 = CARTESIAN_POINT ( 'NONE',  ( -71.27103490383372275, 20.70545763375144332, 39.19188336387009741 ) ) ;
#10099 = CARTESIAN_POINT ( 'NONE',  ( 84.05098130332766004, 18.55728792516086756, 44.25912196898673301 ) ) ;
#10100 = FACE_OUTER_BOUND ( 'NONE', #44750, .T. ) ;
#10101 = CARTESIAN_POINT ( 'NONE',  ( -119.2949674747224833, 43.48097822533565449, 41.72283548570154466 ) ) ;
#10102 = FACE_OUTER_BOUND ( 'NONE', #57610, .T. ) ;
#10103 = ORIENTED_EDGE ( 'NONE', *, *, #20727, .F. ) ;
#10104 = DIRECTION ( 'NONE',  ( 0.000000000000000000, 0.000000000000000000, -1.000000000000000000 ) ) ;
#10105 = ORIENTED_EDGE ( 'NONE', *, *, #59946, .F. ) ;
#10106 = CARTESIAN_POINT ( 'NONE',  ( -14.55425570676092129, 7.423011834016145727, -39.59648726401223229 ) ) ;
#10107 = CARTESIAN_POINT ( 'NONE',  ( 86.14890207173843351, 20.31981596387580424, 71.55663816294304524 ) ) ;
#10108 = CARTESIAN_POINT ( 'NONE',  ( -80.34986779050261418, 22.96961150679207719, -88.98360521546140944 ) ) ;
#10109 = CARTESIAN_POINT ( 'NONE',  ( 57.30278335769610010, -48.40406511297319980, 170.0000000000000000 ) ) ;
#10110 = CARTESIAN_POINT ( 'NONE',  ( 32.66883187925819243, 8.640402022338113497, 7.229089490855268529 ) ) ;
#10111 = CARTESIAN_POINT ( 'NONE',  ( -45.81425895439360829, -46.10914959592906115, 40.00000000000003553 ) ) ;
#10112 = CARTESIAN_POINT ( 'NONE',  ( 33.03621582719334526, 7.666716336587111158, -73.93768929495423947 ) ) ;
#10113 = CARTESIAN_POINT ( 'NONE',  ( -96.43817545481738307, 31.02509717589733640, -74.08903276496864976 ) ) ;
#10114 = DIRECTION ( 'NONE',  ( -0.000000000000000000, 1.000000000000000000, -0.000000000000000000 ) ) ;
#10115 = VERTEX_POINT ( 'NONE', #35712 ) ;
#10116 = CYLINDRICAL_SURFACE ( 'NONE', #40999, 7.500000000000020428 ) ;
#10117 = ORIENTED_EDGE ( 'NONE', *, *, #25425, .T. ) ;
#10118 = LINE ( 'NONE', #4837, #34031 ) ;
#10119 =( NAMED_UNIT ( * ) SI_UNIT ( $, .STERADIAN. ) SOLID_ANGLE_UNIT ( ) );
#10120 = CARTESIAN_POINT ( 'NONE',  ( -189.3111515777349894, 107.1887855376296699, 12.66640944553473069 ) ) ;
#10121 = DIRECTION ( 'NONE',  ( -0.000000000000000000, -0.000000000000000000, 1.000000000000000000 ) ) ;
#10122 = CARTESIAN_POINT ( 'NONE',  ( -15.07200981767290493, 7.471751903425211339, -67.81403541448362660 ) ) ;
#10123 = CARTESIAN_POINT ( 'NONE',  ( 31.89651141207536256, 56.63578868294628421, 40.00000000000003553 ) ) ;
#10124 = CARTESIAN_POINT ( 'NONE',  ( 150.0278556977734468, 53.32860603304212788, -42.54581402127228529 ) ) ;
#10125 = ORIENTED_EDGE ( 'NONE', *, *, #16907, .T. ) ;
#10126 = CARTESIAN_POINT ( 'NONE',  ( 848.0071894358328564, 629.9915846175180150, 794.5748919860992601 ) ) ;
#10127 = VECTOR ( 'NONE', #6816, 1000.000000000000000 ) ;
#10128 = DIRECTION ( 'NONE',  ( -1.261617073437677999E-16, -0.000000000000000000, -1.000000000000000000 ) ) ;
#10129 = CARTESIAN_POINT ( 'NONE',  ( 173.9457771591584390, 73.05793967547533896, -19.19921062527386368 ) ) ;
#10130 = DIRECTION ( 'NONE',  ( 0.7530714660036196273, -0.6579387259397027066, 0.000000000000000000 ) ) ;
#10131 = DIRECTION ( 'NONE',  ( -0.000000000000000000, 1.000000000000000000, -0.000000000000000000 ) ) ;
#10132 = ORIENTED_EDGE ( 'NONE', *, *, #35579, .T. ) ;
#10133 = DIRECTION ( 'NONE',  ( -0.000000000000000000, 1.000000000000000000, -0.000000000000000000 ) ) ;
#10134 = EDGE_CURVE ( 'NONE', #26715, #7387, #10008, .T. ) ;
#10135 = CARTESIAN_POINT ( 'NONE',  ( -1.857619870843141952, 6.575690665396231260, -11.50454659054918949 ) ) ;
#10136 = CARTESIAN_POINT ( 'NONE',  ( 197.2847860006354779, 98.30530166401517533, -18.13261055250281473 ) ) ;
#10137 = CARTESIAN_POINT ( 'NONE',  ( -152.2442544045799480, 66.53514540059047988, 84.90555898563886217 ) ) ;
#10138 = CARTESIAN_POINT ( 'NONE',  ( 139.2921620648436942, 44.80435067172504660, 31.81952079417536083 ) ) ;
#10139 = ORIENTED_EDGE ( 'NONE', *, *, #18850, .F. ) ;
#10140 = CARTESIAN_POINT ( 'NONE',  ( 31.11269837220803325, -10.55634918610409656, 2.000000000000001776 ) ) ;
#10141 = FACE_OUTER_BOUND ( 'NONE', #59352, .T. ) ;
#10142 = CARTESIAN_POINT ( 'NONE',  ( 153.4509883044095773, 55.84811350575044031, 30.57316257369191703 ) ) ;
#10143 = LINE ( 'NONE', #59362, #36435 ) ;
#10144 = VECTOR ( 'NONE', #29624, 1000.000000000000000 ) ;
#10145 = ORIENTED_EDGE ( 'NONE', *, *, #28172, .F. ) ;
#10146 = DIRECTION ( 'NONE',  ( -0.000000000000000000, -0.000000000000000000, -1.000000000000000000 ) ) ;
#10147 = ADVANCED_FACE ( 'NONE', ( #26180 ), #31461, .F. ) ;
#10148 = ORIENTED_EDGE ( 'NONE', *, *, #12558, .F. ) ;
#10149 = CARTESIAN_POINT ( 'NONE',  ( -109.7647482398635361, 36.74843029291201191, -41.96704509549551432 ) ) ;
#10150 = CARTESIAN_POINT ( 'NONE',  ( 69.49862690228275142, 14.27023134440512386, -73.86852559465907575 ) ) ;
#10151 = LINE ( 'NONE', #53739, #48537 ) ;
#10153 = ORIENTED_EDGE ( 'NONE', *, *, #15775, .T. ) ;
#10152 = CARTESIAN_POINT ( 'NONE',  ( -1.666933348991701536, -64.97862212458815634, 40.00000000000003553 ) ) ;
#10154 = CARTESIAN_POINT ( 'NONE',  ( -179.2262621278718200, 94.19039042964671182, 42.70701387388177750 ) ) ;
#10155 = EDGE_CURVE ( 'NONE', #36914, #55296, #19875, .T. ) ;
#10156 = VECTOR ( 'NONE', #2409, 1000.000000000000000 ) ;
#10157 = CARTESIAN_POINT ( 'NONE',  ( 422.4999999999999432, 207.5000000000000284, 0.000000000000000000 ) ) ;
#10158 = CARTESIAN_POINT ( 'NONE',  ( 113.4402889550712530, 31.50582881646776912, -36.62137660074326106 ) ) ;
#10159 = ORIENTED_EDGE ( 'NONE', *, *, #48623, .F. ) ;
#10160 = CYLINDRICAL_SURFACE ( 'NONE', #45720, 7.500000000000020428 ) ;
#10161 = CARTESIAN_POINT ( 'NONE',  ( 137.3958226571046453, 43.60243650158411555, 57.22592436439141039 ) ) ;
#10162 = CARTESIAN_POINT ( 'NONE',  ( 63.01563776193091826, 13.70579113808095073, 2.968410348757589468 ) ) ;
#10163 = CARTESIAN_POINT ( 'NONE',  ( 0.000000000000000000, 0.000000000000000000, 0.000000000000000000 ) ) ;
#10164 = CARTESIAN_POINT ( 'NONE',  ( 186.6054783416232112, 84.37128553200975034, -21.98102405639298595 ) ) ;
#10165 = EDGE_CURVE ( 'NONE', #45811, #48517, #60916, .T. ) ;
#10166 = ORIENTED_EDGE ( 'NONE', *, *, #45081, .T. ) ;
#10167 = CARTESIAN_POINT ( 'NONE',  ( 46.23304607317101045, 10.41544405387737982, 7.463327010731485522 ) ) ;
#10168 = VERTEX_POINT ( 'NONE', #8975 ) ;
#10169 = AXIS2_PLACEMENT_3D ( 'NONE', #18519, #39968, #29417 ) ;
#10170 = EDGE_CURVE ( 'NONE', #54229, #41559, #67130, .T. ) ;
#10171 = CARTESIAN_POINT ( 'NONE',  ( -30.60309003827877916, -68.41902945196855512, 41.38025477438755928 ) ) ;
#10172 = CARTESIAN_POINT ( 'NONE',  ( -62.41607942644581897, 16.78015853244291478, 89.94130366719888059 ) ) ;
#10173 = FACE_OUTER_BOUND ( 'NONE', #18433, .T. ) ;
#10174 = LINE ( 'NONE', #15801, #50169 ) ;
#10175 = CARTESIAN_POINT ( 'NONE',  ( 70.37328515878277813, 14.50043699572714040, 89.50955696056523436 ) ) ;
#10176 = CARTESIAN_POINT ( 'NONE',  ( -7.329206686002009974E-14, -46.66904755831211560, 2.000000000000001776 ) ) ;
#10177 = CARTESIAN_POINT ( 'NONE',  ( 212.1707951106655514, 117.1901534358505899, -43.16799237652320187 ) ) ;
#10178 = CARTESIAN_POINT ( 'NONE',  ( 0.000000000000000000, 0.000000000000000000, 5.000000000000000000 ) ) ;
#10179 = VERTEX_POINT ( 'NONE', #14589 ) ;
#10180 = LINE ( 'NONE', #35549, #65555 ) ;
#10181 = ORIENTED_EDGE ( 'NONE', *, *, #13431, .T. ) ;
#10182 = CARTESIAN_POINT ( 'NONE',  ( 181.0840389613909736, -170.0000000000000000, 29.30859410551139277 ) ) ;
#10183 = CARTESIAN_POINT ( 'NONE',  ( 60.40277045393652600, 12.08176563382370183, -63.03086484206352225 ) ) ;
#10184 = CARTESIAN_POINT ( 'NONE',  ( -122.3994536713185255, 45.42826354555015911, 71.60485157671216427 ) ) ;
#10185 = DIRECTION ( 'NONE',  ( 0.000000000000000000, 0.000000000000000000, -1.000000000000000000 ) ) ;
#10186 = CARTESIAN_POINT ( 'NONE',  ( 164.0073343966822392, 64.23003864582459244, -66.78297849933632335 ) ) ;
#10187 = ORIENTED_EDGE ( 'NONE', *, *, #56064, .T. ) ;
#10188 = CARTESIAN_POINT ( 'NONE',  ( -72.20490592113146988, 19.96451062593607872, 68.60262606855620504 ) ) ;
#10189 = CARTESIAN_POINT ( 'NONE',  ( 199.3110346421775603, 99.23841336744848718, -92.27908572396052023 ) ) ;
#10190 = ORIENTED_EDGE ( 'NONE', *, *, #8569, .T. ) ;
#10191 = ORIENTED_EDGE ( 'NONE', *, *, #4290, .F. ) ;
#10192 = CARTESIAN_POINT ( 'NONE',  ( -156.9252506979473196, 70.73559306219777909, 37.07661470075439070 ) ) ;
#10193 = DIRECTION ( 'NONE',  ( 0.000000000000000000, 0.000000000000000000, -1.000000000000000000 ) ) ;
#10194 = CARTESIAN_POINT ( 'NONE',  ( 424.8372781065089612, 400.0000000000001705, 91.05029585798857283 ) ) ;
#10195 = DIRECTION ( 'NONE',  ( -0.000000000000000000, 1.000000000000000000, -0.000000000000000000 ) ) ;
#10196 = DIRECTION ( 'NONE',  ( 0.000000000000000000, -0.000000000000000000, -1.000000000000000000 ) ) ;
#10197 = AXIS2_PLACEMENT_3D ( 'NONE', #17463, #33320, #22050 ) ;
#10198 = VERTEX_POINT ( 'NONE', #36049 ) ;
#10199 = CARTESIAN_POINT ( 'NONE',  ( -132.8150886319752146, 52.45790550853838852, 35.21935937789461235 ) ) ;
#10200 = VERTEX_POINT ( 'NONE', #1177 ) ;
#10201 = CARTESIAN_POINT ( 'NONE',  ( 206.3125232506202735, 108.5822159704961933, 17.19853195675947788 ) ) ;
#10202 = CARTESIAN_POINT ( 'NONE',  ( -143.2498117110515068, 60.33382252735059126, 34.07831714178427518 ) ) ;
#10203 = CIRCLE ( 'NONE', #29298, 0.4000000000000001887 ) ;
#10204 = CARTESIAN_POINT ( 'NONE',  ( 208.6132326550593916, 111.8685719053116543, 43.11846758867611129 ) ) ;
#10205 = ADVANCED_FACE ( 'NONE', ( #37412 ), #124, .F. ) ;
#10206 = CARTESIAN_POINT ( 'NONE',  ( -1.455067768715155196, 7.566780179921179794, 68.42619738054045797 ) ) ;
#10207 = DIRECTION ( 'NONE',  ( 1.000000000000000000, 1.110223024625118675E-14, -1.110223024625118675E-14 ) ) ;
#10208 = AXIS2_PLACEMENT_3D ( 'NONE', #196, #555, #65630 ) ;
#10209 = LINE ( 'NONE', #53455, #45008 ) ;
#10210 = ADVANCED_FACE ( 'NONE', ( #58866 ), #54267, .T. ) ;
#10211 = ORIENTED_EDGE ( 'NONE', *, *, #25898, .T. ) ;
#10212 = ORIENTED_EDGE ( 'NONE', *, *, #43336, .T. ) ;
#10213 = LINE ( 'NONE', #31679, #44638 ) ;
#10214 = CARTESIAN_POINT ( 'NONE',  ( -190.6985136298601731, 109.1272424661242582, -95.00000000000133582 ) ) ;
#10215 = CARTESIAN_POINT ( 'NONE',  ( -171.4867114763003997, 85.32693843184996751, -22.69890371670287266 ) ) ;
#10216 = DIRECTION ( 'NONE',  ( -0.7071067811865474617, 0.7071067811865474617, 0.000000000000000000 ) ) ;
#10217 = DIRECTION ( 'NONE',  ( 0.9561276726666709802, 1.170918693907447064E-16, -0.2929502919626733037 ) ) ;
#10218 = AXIS2_PLACEMENT_3D ( 'NONE', #33581, #66300, #34271 ) ;
#10219 = CARTESIAN_POINT ( 'NONE',  ( 8.747314885369917192, 7.383532170996436328, 93.80849556495012109 ) ) ;
#10220 = B_SPLINE_CURVE_WITH_KNOTS ( 'NONE', 3,
 ( #16061, #27301, #58966, #54017, #48743, #11128, #582, #58278, #10780, #64602, #47717, #16410, #25938, #32253, #5507, #21004, #15722, #59650, #44537, #50162, #28001, #66018, #22735, #54731, #17089, #60713, #38923, #44169, #50511, #17814, #54373, #1625, #38212, #11465, #12529, #7259, #39610, #44885, #23447, #18157, #49445, #1990, #39269, #33301, #23090 ),
 .UNSPECIFIED., .F., .F.,
 ( 4, 2, 2, 2, 2, 2, 2, 2, 2, 2, 2, 1, 2, 2, 2, 2, 2, 2, 2, 2, 2, 2, 4 ),
 ( 0.000000000000000000, 0.001512548138464782236, 0.002268822207697173462, 0.003025096276929564471, 0.004537644415394318301, 0.005293918484626675483, 0.006050192553859033533, 0.007562740692323722744, 0.009075288830788411087, 0.01058783696925309943, 0.01134411103848542365, 0.01210038510771774788, 0.01285665917695007210, 0.01361293324618239459, 0.01512548138464699446, 0.01588175545387929613, 0.01663802952311159433, 0.01815057766157616645, 0.01966312580004073510, 0.02041939986927301942, 0.02117567393850530028, 0.02268822207696985158, 0.02420077021543439941 ),
 .UNSPECIFIED. ) ;
#10221 = VERTEX_POINT ( 'NONE', #37764 ) ;
#10223 = EDGE_CURVE ( 'NONE', #38457, #366, #26527, .T. ) ;
#10222 = DIRECTION ( 'NONE',  ( 1.000000000000000000, 0.000000000000000000, 0.000000000000000000 ) ) ;
#10224 = CARTESIAN_POINT ( 'NONE',  ( 99.99999999999997158, 6.000000000000000000, -25.00000000000000000 ) ) ;
#10225 = ORIENTED_EDGE ( 'NONE', *, *, #65595, .T. ) ;
#10226 = ADVANCED_FACE ( 'NONE', ( #11029 ), #47964, .F. ) ;
#10227 = CARTESIAN_POINT ( 'NONE',  ( 0.000000000000000000, 0.000000000000000000, 0.000000000000000000 ) ) ;
#10228 = ORIENTED_EDGE ( 'NONE', *, *, #54067, .F. ) ;
#10229 = ORIENTED_EDGE ( 'NONE', *, *, #32472, .T. ) ;
#10230 = EDGE_CURVE ( 'NONE', #30657, #34238, #59209, .T. ) ;
#10231 = ORIENTED_EDGE ( 'NONE', *, *, #2486, .T. ) ;
#10232 = CARTESIAN_POINT ( 'NONE',  ( -119.2804658695888094, 43.47213805166352785, 7.728477835248403593 ) ) ;
#10233 = ADVANCED_FACE ( 'NONE', ( #44071 ), #59899, .F. ) ;
#10234 = CARTESIAN_POINT ( 'NONE',  ( -175.9852529046322331, 90.37283472601130541, 72.11072863597617300 ) ) ;
#10235 = CARTESIAN_POINT ( 'NONE',  ( 126.8237978310705358, 37.33705012421154379, 66.47361518080877829 ) ) ;
#10236 = EDGE_LOOP ( 'NONE', ( #13576, #37625, #11876, #47673 ) ) ;
#10237 = CARTESIAN_POINT ( 'NONE',  ( -25.36310660490340396, 8.672627506263530961, 86.99672183978204032 ) ) ;
#10238 = CARTESIAN_POINT ( 'NONE',  ( 16.78635691501517613, 6.000000000000000000, -36.68900338898716740 ) ) ;
#10239 = CARTESIAN_POINT ( 'NONE',  ( 412.3372781065085064, 397.0710678118653618, 78.55029585798826020 ) ) ;
#10240 = CARTESIAN_POINT ( 'NONE',  ( 109.7724924842965919, 28.66436020578543520, -35.92243756565368784 ) ) ;
#10241 = ADVANCED_FACE ( 'NONE', ( #69429 ), #42694, .T. ) ;
#10242 = CARTESIAN_POINT ( 'NONE',  ( -24.41864932425148993, 8.543938959778817122, 40.36687269096346853 ) ) ;
#10243 = CARTESIAN_POINT ( 'NONE',  ( 109.9975424824652777, 296.0000000000000000, 418.0000000000000000 ) ) ;
#10244 = ORIENTED_EDGE ( 'NONE', *, *, #49853, .F. ) ;
#10245 = AXIS2_PLACEMENT_3D ( 'NONE', #21288, #41713, #63174 ) ;
#10246 = EDGE_CURVE ( 'NONE', #28008, #44519, #64280, .T. ) ;
#10247 = ADVANCED_FACE ( 'NONE', ( #27202 ), #53584, .F. ) ;
#10248 = EDGE_CURVE ( 'NONE', #36451, #3230, #48637, .T. ) ;
#10249 = CARTESIAN_POINT ( 'NONE',  ( 262.2516123306975260, 190.0000000000000000, -91.28179539054376335 ) ) ;
#10250 = CARTESIAN_POINT ( 'NONE',  ( -79.61235761536667610, 23.76245710489569518, -76.91537820575416617 ) ) ;
#10251 = CARTESIAN_POINT ( 'NONE',  ( 173.9457771591584105, 73.05793967547531054, 7.645339965189813292 ) ) ;
#10252 = DIRECTION ( 'NONE',  ( -0.000000000000000000, -0.000000000000000000, -1.000000000000000000 ) ) ;
#10253 = CARTESIAN_POINT ( 'NONE',  ( 8.000000000000007105, 249.8719672152120381, -95.00000000000133582 ) ) ;
#10254 = CARTESIAN_POINT ( 'NONE',  ( 447.3372781065082791, 400.0000000000044338, 78.55029585798382641 ) ) ;
#10255 = CARTESIAN_POINT ( 'NONE',  ( 36.77263075747509902, 8.082075437684869357, -89.78184162056548701 ) ) ;
#10256 = CARTESIAN_POINT ( 'NONE',  ( 197.2450958997033865, 98.25574850261155291, 91.26861472641076034 ) ) ;
#10258 = CARTESIAN_POINT ( 'NONE',  ( 70.51484748609223630, 14.53801151001411363, 9.956432264353654915 ) ) ;
#10257 = AXIS2_PLACEMENT_3D ( 'NONE', #8454, #17612, #17965 ) ;
#10259 = AXIS2_PLACEMENT_3D ( 'NONE', #19459, #40566, #30024 ) ;
#10260 = CARTESIAN_POINT ( 'NONE',  ( 157.4703587214989113, 57.65129005721576760, 2.564916881789689018 ) ) ;
#10261 = CARTESIAN_POINT ( 'NONE',  ( 26.99999999999999645, 26.99999999999999645, 12.00000000000000000 ) ) ;
#10262 = ORIENTED_EDGE ( 'NONE', *, *, #44657, .F. ) ;
#10263 = CARTESIAN_POINT ( 'NONE',  ( -49.42889165003705187, 14.28050133789322018, 86.50253100448308885 ) ) ;
#10264 = VERTEX_POINT ( 'NONE', #26869 ) ;
#10265 = FACE_OUTER_BOUND ( 'NONE', #29897, .T. ) ;
#10266 = VERTEX_POINT ( 'NONE', #11721 ) ;
#10267 = CARTESIAN_POINT ( 'NONE',  ( 22.15943197741200521, 7.796127622097903220, -73.82810297161255164 ) ) ;
#10268 = CARTESIAN_POINT ( 'NONE',  ( -149.5074843970971017, 65.50121172469319220, 72.56537183036277838 ) ) ;
#10269 = DIRECTION ( 'NONE',  ( -0.000000000000000000, 1.000000000000000000, -0.000000000000000000 ) ) ;
#10270 = AXIS2_PLACEMENT_3D ( 'NONE', #36324, #20830, #58124 ) ;
#10271 = CARTESIAN_POINT ( 'NONE',  ( 139.3041645503688528, 46.00819478311334620, -48.68433813850839442 ) ) ;
#10272 = CARTESIAN_POINT ( 'NONE',  ( 207.3574376820450595, 111.8208281420536707, -90.49371098840704519 ) ) ;
#10273 = CARTESIAN_POINT ( 'NONE',  ( 15.55634918610406103, 20.55634918610400064, 0.000000000000000000 ) ) ;
#10274 = CARTESIAN_POINT ( 'NONE',  ( -84.49322488516129681, 0.000000000000000000, 43.58025477438756212 ) ) ;
#10275 = ORIENTED_EDGE ( 'NONE', *, *, #10170, .F. ) ;
#10276 = ORIENTED_EDGE ( 'NONE', *, *, #39806, .T. ) ;
#10277 = FILL_AREA_STYLE ('',( #48241 ) ) ;
#10278 = CARTESIAN_POINT ( 'NONE',  ( -422.6627218934914367, 0.000000000000000000, -141.4497041420118535 ) ) ;
#10279 = CARTESIAN_POINT ( 'NONE',  ( 128.3483068049043538, 39.35455865146280274, -92.10653312658361358 ) ) ;
#10280 = CARTESIAN_POINT ( 'NONE',  ( 66.89344749234535925, 14.64254390099354985, -90.47725094589908679 ) ) ;
#10281 = CARTESIAN_POINT ( 'NONE',  ( 92.52113039222221857, 22.58921125235803018, 15.03444035171357740 ) ) ;
#10282 = CARTESIAN_POINT ( 'NONE',  ( 185.5457097283154724, 84.70846743303873438, -10.83386876099697282 ) ) ;
#10283 = CARTESIAN_POINT ( 'NONE',  ( -86.06016868996614733, 25.27707703029502539, -14.48738519166817440 ) ) ;
#10284 =( LENGTH_UNIT ( ) NAMED_UNIT ( * ) SI_UNIT ( .MILLI., .METRE. ) );
#10285 = CARTESIAN_POINT ( 'NONE',  ( -179.5082312244189495, 94.53075638132058600, -46.15200650400738169 ) ) ;
#10286 = CARTESIAN_POINT ( 'NONE',  ( 92.53566308513171634, 21.52138666710686721, -11.82835652178502706 ) ) ;
#10287 = CARTESIAN_POINT ( 'NONE',  ( 14.72760828316778259, -30.00634389893561504, 6.893343212288930211 ) ) ;
#10288 = DIRECTION ( 'NONE',  ( 1.000000000000000000, 0.000000000000000000, 0.000000000000000000 ) ) ;
#10289 = CARTESIAN_POINT ( 'NONE',  ( 0.000000000000000000, 0.000000000000000000, 41.38025477438755928 ) ) ;
#10290 = EDGE_CURVE ( 'NONE', #33258, #57934, #48293, .T. ) ;
#10291 =( REPRESENTATION_RELATIONSHIP ('NONE','NONE', #40274, #19523 ) REPRESENTATION_RELATIONSHIP_WITH_TRANSFORMATION ( #5792 )SHAPE_REPRESENTATION_RELATIONSHIP( ) );
#10292 = ORIENTED_EDGE ( 'NONE', *, *, #10080, .T. ) ;
#10293 = DIRECTION ( 'NONE',  ( -0.000000000000000000, 1.000000000000000000, -0.000000000000000000 ) ) ;
#10294 = CYLINDRICAL_SURFACE ( 'NONE', #60867, 5.000000000000060396 ) ;
#10295 = AXIS2_PLACEMENT_3D ( 'NONE', #15592, #52853, #58479 ) ;
#10296 = CARTESIAN_POINT ( 'NONE',  ( 151.3136733342017237, 54.26417151662144533, 68.04466391889920374 ) ) ;
#10297 = DIRECTION ( 'NONE',  ( 0.9839295885986321100, -0.1785568947986229116, 0.000000000000000000 ) ) ;
#10298 = CARTESIAN_POINT ( 'NONE',  ( 0.000000000000000000, 0.000000000000000000, 133.5802547743875550 ) ) ;
#10299 = CARTESIAN_POINT ( 'NONE',  ( -6.210370628187416919, 7.798947244808402957, 83.97346081649014593 ) ) ;
#10300 = VECTOR ( 'NONE', #67787, 1000.000000000000000 ) ;
#10301 = ORIENTED_EDGE ( 'NONE', *, *, #45433, .T. ) ;
#10303 = ADVANCED_FACE ( 'NONE', ( #64503 ), #10337, .F. ) ;
#10302 = CARTESIAN_POINT ( 'NONE',  ( 0.000000000000000000, 0.000000000000000000, 8.000000000000000000 ) ) ;
#10304 = EDGE_CURVE ( 'NONE', #56564, #55579, #27908, .T. ) ;
#10305 = DIRECTION ( 'NONE',  ( 1.000000000000000000, 0.000000000000000000, 0.000000000000000000 ) ) ;
#10306 = ORIENTED_EDGE ( 'NONE', *, *, #17243, .T. ) ;
#10307 = VECTOR ( 'NONE', #68733, 1000.000000000000000 ) ;
#10308 = VECTOR ( 'NONE', #32015, 1000.000000000000114 ) ;
#10309 = EDGE_CURVE ( 'NONE', #52004, #42183, #31519, .T. ) ;
#10310 = VERTEX_POINT ( 'NONE', #40206 ) ;
#10311 = CARTESIAN_POINT ( 'NONE',  ( 32.57244506765509584, 8.630607406489110289, 87.98557846726629350 ) ) ;
#10312 = DIRECTION ( 'NONE',  ( 1.000000000000000000, 0.000000000000000000, 0.000000000000000000 ) ) ;
#10313 = CARTESIAN_POINT ( 'NONE',  ( 39.40195752203892710, 9.424259417798133143, -77.46436805589148378 ) ) ;
#10314 = ORIENTED_EDGE ( 'NONE', *, *, #42088, .F. ) ;
#10315 = ADVANCED_FACE ( 'NONE', ( #39512 ), #17714, .F. ) ;
#10316 = PLANE ( 'NONE',  #35620 ) ;
#10317 = DIRECTION ( 'NONE',  ( -0.000000000000000000, -0.000000000000000000, 1.000000000000000000 ) ) ;
#10318 = CLOSED_SHELL ( 'NONE', ( #44388, #64080, #1409, #13631, #52648, #31992 ) ) ;
#10319 = CARTESIAN_POINT ( 'NONE',  ( -3.253130881186330647, 7.643323950922364496, 4.805877217267385149 ) ) ;
#10320 = CARTESIAN_POINT ( 'NONE',  ( 173.8623159076319951, 72.97967239795019623, -45.76964742264968322 ) ) ;
#10321 = CARTESIAN_POINT ( 'NONE',  ( 160.5022159022404367, 60.04643339566187876, 83.71124699655744905 ) ) ;
#10322 = CARTESIAN_POINT ( 'NONE',  ( 50.98853755884157124, 400.0000000000065938, -128.9497041420121946 ) ) ;
#10323 = ORIENTED_EDGE ( 'NONE', *, *, #53799, .F. ) ;
#10324 = CARTESIAN_POINT ( 'NONE',  ( -3.469446951953614189E-15, 0.000000000000000000, -17.00000000000000355 ) ) ;
#10325 = B_SPLINE_CURVE_WITH_KNOTS ( 'NONE', 3,
 ( #69314, #27086, #43610, #43253, #21140, #42582, #64733, #32724, #64038, #37996, #54148, #15847, #58742, #65080, #10565, #5973, #48869, #52773, #58074, #49228, #55214, #44310, #23226, #45005, #39392, #65791, #50298, #28847, #55925, #12663, #55563, #66843, #33775, #7738, #22513, #2456, #23910, #44675, #34125, #54502, #50632, #60143, #29190 ),
 .UNSPECIFIED., .F., .F.,
 ( 4, 2, 2, 2, 2, 2, 2, 2, 2, 2, 2, 1, 2, 2, 2, 2, 2, 2, 2, 2, 2, 4 ),
 ( 0.02515559250233022348, 0.02674001423437951525, 0.02753222510040416460, 0.02832443596642881742, 0.02990885769847818204, 0.03149327943052755013, 0.03307770116257691129, 0.03386991202860161615, 0.03466212289462632101, 0.03624654462667572380, 0.03703875549270041478, 0.03783096635872511271, 0.03862317722474981063, 0.03941538809077450162, 0.04099980982282387665, 0.04258423155487325168, 0.04337644242089793573, 0.04416865328692261977, 0.04575307501897192541, 0.04733749675102122412, 0.04892191848307052976, 0.05050634021511983540 ),
 .UNSPECIFIED. ) ;
#10326 = LINE ( 'NONE', #20890, #66259 ) ;
#10327 = CARTESIAN_POINT ( 'NONE',  ( 109.9975424824652634, 22.00669820036271673, 401.6295345748408181 ) ) ;
#10328 = CARTESIAN_POINT ( 'NONE',  ( 197.1979149960397990, 98.19687999752002838, 36.37236663005180759 ) ) ;
#10329 = LINE ( 'NONE', #53577, #15241 ) ;
#10331 = ORIENTED_EDGE ( 'NONE', *, *, #138, .T. ) ;
#10330 = LINE ( 'NONE', #37071, #38845 ) ;
#10332 = ORIENTED_EDGE ( 'NONE', *, *, #27544, .F. ) ;
#10333 = EDGE_CURVE ( 'NONE', #3562, #45063, #42398, .T. ) ;
#10334 = ADVANCED_FACE ( 'NONE', ( #66953 ), #19087, .T. ) ;
#10335 = ORIENTED_EDGE ( 'NONE', *, *, #43559, .T. ) ;
#10336 = DIRECTION ( 'NONE',  ( -0.000000000000000000, 0.000000000000000000, 1.000000000000000000 ) ) ;
#10337 = PLANE ( 'NONE',  #3094 ) ;
#10338 = CARTESIAN_POINT ( 'NONE',  ( 107.3013380801406385, 400.0000000000076739, 96.05029585798752123 ) ) ;
#10339 = EDGE_CURVE ( 'NONE', #56789, #54495, #34243, .T. ) ;
#10340 = CARTESIAN_POINT ( 'NONE',  ( -32.40928421737412179, 10.77259363352673205, 57.10791823073882512 ) ) ;
#10341 = FACE_OUTER_BOUND ( 'NONE', #30220, .T. ) ;
#10342 = CARTESIAN_POINT ( 'NONE',  ( 152.1190604254710479, 53.60705199010334354, -75.72949298238010840 ) ) ;
#10343 = LINE ( 'NONE', #20910, #58937 ) ;
#10344 = DIRECTION ( 'NONE',  ( -1.000000000000000000, -0.000000000000000000, -0.000000000000000000 ) ) ;
#10345 = EDGE_LOOP ( 'NONE', ( #24574, #33856, #6403 ) ) ;
#10346 = ORIENTED_EDGE ( 'NONE', *, *, #9196, .T. ) ;
#10347 = DIRECTION ( 'NONE',  ( -1.000000000000000000, -0.000000000000000000, -0.000000000000000000 ) ) ;
#10348 = VECTOR ( 'NONE', #67867, 1000.000000000000000 ) ;
#10349 = CARTESIAN_POINT ( 'NONE',  ( -81.00768240531208164, 24.30850321514433432, -49.74466447296814664 ) ) ;
#10350 = CARTESIAN_POINT ( 'NONE',  ( 159.6725804802005371, 59.38339663535509771, 70.93746766617782384 ) ) ;
#10351 = CARTESIAN_POINT ( 'NONE',  ( -150.3850953947692517, 66.25368649589887582, 18.83771815676428574 ) ) ;
#10352 = AXIS2_PLACEMENT_3D ( 'NONE', #57064, #8177, #8875 ) ;
#10353 = CARTESIAN_POINT ( 'NONE',  ( 38.07387128079424343, 34.92400860923387995, 26.66469066592269144 ) ) ;
#10354 = CARTESIAN_POINT ( 'NONE',  ( 15.78827728214693416, 6.500811158483329244, 45.01470767270524931 ) ) ;
#10355 = CARTESIAN_POINT ( 'NONE',  ( -156.9757241921502953, 72.15252929097994183, 92.68305819821679847 ) ) ;
#10356 = ORIENTED_EDGE ( 'NONE', *, *, #817, .F. ) ;
#10357 = EDGE_LOOP ( 'NONE', ( #38129, #68885, #33719, #14622 ) ) ;
#10358 = ORIENTED_EDGE ( 'NONE', *, *, #48041, .F. ) ;
#10359 = AXIS2_PLACEMENT_3D ( 'NONE', #14524, #47900, #4323 ) ;
#10360 = CARTESIAN_POINT ( 'NONE',  ( 35.65622260226239604, 8.964590916200315007, -36.61753697201972813 ) ) ;
#10361 = CARTESIAN_POINT ( 'NONE',  ( -17.89459634713042391, -72.78390022947110083, 41.38025477438755928 ) ) ;
#10362 = CIRCLE ( 'NONE', #49673, 24.99999999999985434 ) ;
#10363 = CARTESIAN_POINT ( 'NONE',  ( -37.92542950990691963, 10.74638084523342130, 60.78760712818166212 ) ) ;
#10364 = DIRECTION ( 'NONE',  ( 1.000000000000000000, 1.110223024625155594E-14, -1.110223024625155594E-14 ) ) ;
#10365 = ORIENTED_EDGE ( 'NONE', *, *, #38334, .F. ) ;
#10366 = CARTESIAN_POINT ( 'NONE',  ( 186.0827296088607170, 85.28826835108064586, 69.24936458491407620 ) ) ;
#10367 = CARTESIAN_POINT ( 'NONE',  ( 8.336031647119270360, 6.376437040857336314, -15.19577221354909824 ) ) ;
#10368 = CARTESIAN_POINT ( 'NONE',  ( 8.171862787985018528, 51.01496593442378469, 26.66469104408689716 ) ) ;
#10369 = CARTESIAN_POINT ( 'NONE',  ( 28.73969565797881387, 50.76944201751176422, 27.58472315868180402 ) ) ;
#10370 = FACE_OUTER_BOUND ( 'NONE', #17033, .T. ) ;
#10371 = CARTESIAN_POINT ( 'NONE',  ( -83.12901536265221125, 24.07178615860086168, -36.58265565400330388 ) ) ;
#10372 = CARTESIAN_POINT ( 'NONE',  ( 15.78827728214693060, 6.500811158483329244, 71.85925826316895382 ) ) ;
#10373 = DIRECTION ( 'NONE',  ( -3.081487911019579554E-32, -1.000000000000000000, -3.469446951953612956E-17 ) ) ;
#10374 = CARTESIAN_POINT ( 'NONE',  ( 8.540564391411908929, 7.383006541823030844, 8.725566054845465658 ) ) ;
#10375 = EDGE_CURVE ( 'NONE', #2402, #43402, #8195, .T. ) ;
#10376 = VERTEX_POINT ( 'NONE', #50413 ) ;
#10377 = DIRECTION ( 'NONE',  ( -1.000000000000000000, 0.000000000000000000, 0.000000000000000000 ) ) ;
#10378 = PRODUCT_CONTEXT ( 'NONE', #41742, 'mechanical' ) ;
#10379 = DIRECTION ( 'NONE',  ( -0.000000000000000000, -0.000000000000000000, 1.000000000000000000 ) ) ;
#10380 = LINE ( 'NONE', #48338, #10695 ) ;
#10381 = CARTESIAN_POINT ( 'NONE',  ( -108.9444157621018547, 37.44493815491211564, -39.03547156667866602 ) ) ;
#10382 = DIRECTION ( 'NONE',  ( 0.000000000000000000, 0.000000000000000000, 1.000000000000000000 ) ) ;
#10383 = ORIENTED_EDGE ( 'NONE', *, *, #18660, .F. ) ;
#10384 = EDGE_LOOP ( 'NONE', ( #9394, #48068, #53579, #47165, #31204, #1851 ) ) ;
#10386 = EDGE_CURVE ( 'NONE', #62269, #16032, #69255, .T. ) ;
#10385 = CARTESIAN_POINT ( 'NONE',  ( -26.49516976694650339, 8.831756547364850718, -10.31156455694099883 ) ) ;
#10387 = CARTESIAN_POINT ( 'NONE',  ( 197.3064269725219333, 98.33232022113057269, 11.17706977006253766 ) ) ;
#10388 = ORIENTED_EDGE ( 'NONE', *, *, #12502, .F. ) ;
#10389 = EDGE_CURVE ( 'NONE', #41408, #31811, #31037, .T. ) ;
#10390 = CARTESIAN_POINT ( 'NONE',  ( 112.5554747942046134, 29.96654954475022237, 56.81725345967257113 ) ) ;
#10391 = ORIENTED_EDGE ( 'NONE', *, *, #22790, .T. ) ;
#10392 = CARTESIAN_POINT ( 'NONE',  ( 86.62931800182293784, 19.42108912189600645, -8.977013608448025650 ) ) ;
#10393 = CARTESIAN_POINT ( 'NONE',  ( 127.6144785300460143, 37.78099129859914740, 32.84513397848537153 ) ) ;
#10394 = ADVANCED_FACE ( 'NONE', ( #20462 ), #3267, .F. ) ;
#10395 = LINE ( 'NONE', #42752, #37523 ) ;
#10396 = CIRCLE ( 'NONE', #36269, 4.999999999999996447 ) ;
#10397 = EDGE_CURVE ( 'NONE', #17506, #32477, #35624, .T. ) ;
#10398 = DIRECTION ( 'NONE',  ( -0.000000000000000000, -1.000000000000000000, 0.000000000000000000 ) ) ;
#10399 = PLANE ( 'NONE',  #11397 ) ;
#10400 = VECTOR ( 'NONE', #16824, 1000.000000000000000 ) ;
#10402 = ORIENTED_EDGE ( 'NONE', *, *, #21208, .T. ) ;
#10401 = DIRECTION ( 'NONE',  ( 0.000000000000000000, -1.000000000000000000, 0.000000000000000000 ) ) ;
#10403 = VERTEX_POINT ( 'NONE', #56729 ) ;
#10404 = VECTOR ( 'NONE', #35125, 1000.000000000000000 ) ;
#10405 = EDGE_LOOP ( 'NONE', ( #57561, #43931, #57378, #57229, #9254, #57778, #38972, #63901, #23057, #68473, #58540, #23737, #49244 ) ) ;
#10406 = CARTESIAN_POINT ( 'NONE',  ( -125.4481990864046423, 46.20056605584957055, -23.06915330777029993 ) ) ;
#10407 = AXIS2_PLACEMENT_3D ( 'NONE', #35304, #56760, #35656 ) ;
#10408 = FACE_BOUND ( 'NONE', #13332, .T. ) ;
#10409 = CARTESIAN_POINT ( 'NONE',  ( -180.4643341113398378, 95.69224917234933514, -13.81201931865484589 ) ) ;
#10410 = CARTESIAN_POINT ( 'NONE',  ( 0.000000000000000000, -0.2591992991291388049, -2.646296226153046938 ) ) ;
#10412 = VERTEX_POINT ( 'NONE', #57416 ) ;
#10411 = CARTESIAN_POINT ( 'NONE',  ( -142.4991775570125299, 58.45550857435406300, -39.58818248682278096 ) ) ;
#10413 = CYLINDRICAL_SURFACE ( 'NONE', #25232, 7.500000000000013323 ) ;
#10414 = VECTOR ( 'NONE', #18922, 1000.000000000000114 ) ;
#10415 = ORIENTED_EDGE ( 'NONE', *, *, #48308, .T. ) ;
#10416 = CARTESIAN_POINT ( 'NONE',  ( -133.3149301983942507, 51.57857650535022032, 39.23854680323682231 ) ) ;
#10417 = CARTESIAN_POINT ( 'NONE',  ( -62.45356936877016807, 16.79156452995241366, -17.11305785722446160 ) ) ;
#10418 = ADVANCED_FACE ( 'NONE', ( #14842 ), #24727, .T. ) ;
#10419 = CARTESIAN_POINT ( 'NONE',  ( 79.23200707685333555, 17.02828389812517074, -15.21462584625181691 ) ) ;
#10420 = CARTESIAN_POINT ( 'NONE',  ( -125.8938041572051389, 47.69968343338778283, -76.75825448869764500 ) ) ;
#10421 = DIRECTION ( 'NONE',  ( -0.000000000000000000, -0.000000000000000000, -1.000000000000000000 ) ) ;
#10422 = PLANE ( 'NONE',  #35855 ) ;
#10423 = CARTESIAN_POINT ( 'NONE',  ( -99.10260179032844974, 31.19580119595417855, -62.56131912884078616 ) ) ;
#10424 = ORIENTED_EDGE ( 'NONE', *, *, #57887, .F. ) ;
#10425 = ORIENTED_EDGE ( 'NONE', *, *, #26829, .T. ) ;
#10426 = B_SPLINE_CURVE_WITH_KNOTS ( 'NONE', 3,
 ( #69353, #31382, #35966, #4308, #51798, #15548, #31041, #31718, #57420, #4982, #20466, #52486, #46865, #3607, #9235, #68331, #30690, #36660, #26450, #47887, #21172, #64073, #58782, #52141, #3958, #20131, #25075, #54897, #44347, #6721, #21500, #27828, #6010, #38033, #32758, #43643, #28165, #22206, #53504, #43993, #37681, #42947, #49266, #64417, #33112, #6374 ),
 .UNSPECIFIED., .F., .F.,
 ( 4, 2, 2, 2, 2, 2, 2, 2, 2, 2, 2, 2, 2, 2, 2, 2, 2, 2, 2, 2, 2, 2, 4 ),
 ( 6.938893903907228378E-18, 0.003192770216278258480, 0.003990962770347825268, 0.004789155324417392924, 0.006385540432556518695, 0.007183732986626099361, 0.007981925540695681762, 0.009578310648834874319, 0.01037650320290446106, 0.01117469575697404606, 0.01197288831104363106, 0.01277108086511321607, 0.01436746597325242771, 0.01596385108139163761, 0.01676204363546123649, 0.01756023618953083190, 0.01835842874360043078, 0.01915662129767002619, 0.02075300640580920661, 0.02234939151394838355, 0.02394577662208756397, 0.02474396917615715244, 0.02554216173022674438 ),
 .UNSPECIFIED. ) ;
#10427 = CARTESIAN_POINT ( 'NONE',  ( 188.4359598230020651, 86.36951380984525883, -72.08147103809925227 ) ) ;
#10428 = CARTESIAN_POINT ( 'NONE',  ( 14.80205238535217127, 6.470775952815775334, 30.06371155530308670 ) ) ;
#10429 = DIRECTION ( 'NONE',  ( -0.8118923937861950435, -0.5838071093367415143, 0.000000000000000000 ) ) ;
#10430 = CARTESIAN_POINT ( 'NONE',  ( 141.9165763529819344, 242.0000000000000000, 108.9999999999999858 ) ) ;
#10431 = FACE_OUTER_BOUND ( 'NONE', #61194, .T. ) ;
#10432 = CARTESIAN_POINT ( 'NONE',  ( -74.79539698934961223, 21.95498232236883851, 31.48986615712328430 ) ) ;
#10433 = CARTESIAN_POINT ( 'NONE',  ( 84.97343609940688225, 18.86260005312943377, 44.53087885251839140 ) ) ;
#10434 = CARTESIAN_POINT ( 'NONE',  ( 68.94948716683070700, 15.16699441119057923, -47.83381367184613708 ) ) ;
#10435 = CARTESIAN_POINT ( 'NONE',  ( -118.6727642982647239, 43.09863379477474865, 36.02294872542282889 ) ) ;
#10436 = CARTESIAN_POINT ( 'NONE',  ( 212.0739503583954217, 117.0412199804969617, 62.15368347199733279 ) ) ;
#10437 = ORIENTED_EDGE ( 'NONE', *, *, #35607, .T. ) ;
#10438 = CARTESIAN_POINT ( 'NONE',  ( -108.5289085648060734, 36.07014995015116909, -11.51505029103895517 ) ) ;
#10439 = ORIENTED_EDGE ( 'NONE', *, *, #58459, .T. ) ;
#10440 = CARTESIAN_POINT ( 'NONE',  ( -15.07200981767291204, 7.471751903425211339, -40.96948482401995761 ) ) ;
#10441 = COLOUR_RGB ( '',0.7921568627450980005, 0.8196078431372548767, 0.9333333333333333481 ) ;
#10442 = CARTESIAN_POINT ( 'NONE',  ( -20.55634918610403261, 5.000000000000028422, 0.000000000000000000 ) ) ;
#10443 = CARTESIAN_POINT ( 'NONE',  ( 87.11239765416380010, 20.65008247340817960, 71.55663816294303103 ) ) ;
#10444 = CARTESIAN_POINT ( 'NONE',  ( 151.7956716830626647, 53.36999433148314154, -11.86948592691346605 ) ) ;
#10445 = CARTESIAN_POINT ( 'NONE',  ( 26.99999999999999645, 26.99999999999999645, 12.00000000000000000 ) ) ;
#10446 = CARTESIAN_POINT ( 'NONE',  ( 31.99894129856762603, 7.561773404408291377, -71.19152479471692629 ) ) ;
#10447 = CARTESIAN_POINT ( 'NONE',  ( 13.24564585880038514, 63.65041531508843065, 41.38025477438755928 ) ) ;
#10448 = VECTOR ( 'NONE', #21509, 1000.000000000000000 ) ;
#10449 = LINE ( 'NONE', #22398, #6813 ) ;
#10450 = ORIENTED_EDGE ( 'NONE', *, *, #809, .T. ) ;
#10451 = CARTESIAN_POINT ( 'NONE',  ( 19.84876894326305319, 26.89441334579538534, 6.893342937333461151 ) ) ;
#10452 = ORIENTED_EDGE ( 'NONE', *, *, #18428, .F. ) ;
#10453 = CARTESIAN_POINT ( 'NONE',  ( 60.40531521312254171, 13.11276739283242421, 57.12225848735855038 ) ) ;
#10454 = CARTESIAN_POINT ( 'NONE',  ( 9.837735240994025077, 7.389327806910503504, -74.43536120031389203 ) ) ;
#10455 = CARTESIAN_POINT ( 'NONE',  ( 5.799999999999999822, 1.502314598737159031E-15, -8.000000000000000000 ) ) ;
#10456 = EDGE_CURVE ( 'NONE', #59826, #43402, #47525, .T. ) ;
#10457 = DIRECTION ( 'NONE',  ( 0.9510565162951544194, -0.3090169943749446757, -2.199760087730564624E-16 ) ) ;
#10459 = ADVANCED_FACE ( 'NONE', ( #47195 ), #63035, .T. ) ;
#10458 = CARTESIAN_POINT ( 'NONE',  ( 280.3272854519634052, -21.42428528562853529, 4.999999999999992895 ) ) ;
#10460 = CARTESIAN_POINT ( 'NONE',  ( -99.10260179032840711, 31.19580119595418211, -8.872217947913421554 ) ) ;
#10461 = VECTOR ( 'NONE', #23119, 1000.000000000000000 ) ;
#10462 = CARTESIAN_POINT ( 'NONE',  ( 79.94135235523673089, 18.29982848521581928, 87.49016971473862725 ) ) ;
#10463 = EDGE_CURVE ( 'NONE', #22089, #47869, #8889, .T. ) ;
#10464 = CIRCLE ( 'NONE', #28444, 65.36598343705435354 ) ;
#10465 = ORIENTED_EDGE ( 'NONE', *, *, #41864, .F. ) ;
#10466 = EDGE_CURVE ( 'NONE', #61415, #55296, #4632, .T. ) ;
#10468 = AXIS2_PLACEMENT_3D ( 'NONE', #39958, #11829, #34698 ) ;
#10467 = DIRECTION ( 'NONE',  ( 9.989315170677463157E-15, -1.000000000000000000, -4.052314039881817428E-15 ) ) ;
#10469 = CARTESIAN_POINT ( 'NONE',  ( 6.933333333333328241, 0.000000000000000000, -11.86666666666666536 ) ) ;
#10470 = CARTESIAN_POINT ( 'NONE',  ( 442.3372781065085633, 392.9289321881346382, -141.4497041420117966 ) ) ;
#10471 = CARTESIAN_POINT ( 'NONE',  ( -109.7811201291769834, 37.90784085457603680, 65.09395327358092231 ) ) ;
#10472 = CARTESIAN_POINT ( 'NONE',  ( -130.5904357464318366, 50.88938808445631423, -36.54610296849261886 ) ) ;
#10473 = VERTEX_POINT ( 'NONE', #19429 ) ;
#10474 = LINE ( 'NONE', #59353, #4177 ) ;
#10475 = CARTESIAN_POINT ( 'NONE',  ( -5.416136198635864041, 6.745992685878658079, -23.18025356100167045 ) ) ;
#10476 = CARTESIAN_POINT ( 'NONE',  ( 197.1975259970232059, 98.19639476549650681, -16.65484193907906629 ) ) ;
#10477 = LINE ( 'NONE', #47764, #48342 ) ;
#10478 = ADVANCED_FACE ( 'NONE', ( #14503 ), #52136, .T. ) ;
#10479 = CARTESIAN_POINT ( 'NONE',  ( 140.2332932573541484, 45.41010019581507606, 40.99038388568915536 ) ) ;
#10480 = EDGE_LOOP ( 'NONE', ( #46112, #53786, #23789, #45716 ) ) ;
#10481 = CARTESIAN_POINT ( 'NONE',  ( 0.3157512944565323831, -3.097794232830194172, -8.000000000000000000 ) ) ;
#10482 = CARTESIAN_POINT ( 'NONE',  ( 112.3013380801408658, 400.0000000000065938, 91.05029585798857283 ) ) ;
#10483 = EDGE_CURVE ( 'NONE', #10617, #24043, #9923, .T. ) ;
#10484 = CARTESIAN_POINT ( 'NONE',  ( 160.5018603162734792, 61.33906090758087259, 3.190259315126446449 ) ) ;
#10485 = CARTESIAN_POINT ( 'NONE',  ( 73.57152302639893549, 14.62167909564606916, 43.58025477438756923 ) ) ;
#10486 = ORIENTED_EDGE ( 'NONE', *, *, #11040, .F. ) ;
#10487 = LINE ( 'NONE', #48111, #65366 ) ;
#10488 = VERTEX_POINT ( 'NONE', #26095 ) ;
#10489 = CARTESIAN_POINT ( 'NONE',  ( -108.5289085648060308, 36.07014995015116199, -38.35960088150262237 ) ) ;
#10490 = LINE ( 'NONE', #47427, #26395 ) ;
#10491 = AXIS2_PLACEMENT_3D ( 'NONE', #7891, #24068, #2272 ) ;
#10492 = CARTESIAN_POINT ( 'NONE',  ( -60.97011009284708649, 16.34812508431679490, 42.45179124754056943 ) ) ;
#10493 = AXIS2_PLACEMENT_3D ( 'NONE', #42460, #63917, #41777 ) ;
#10495 = VERTEX_POINT ( 'NONE', #57076 ) ;
#10494 = CARTESIAN_POINT ( 'NONE',  ( 156.5890478960376981, 58.24007662587946754, 17.52612138860288837 ) ) ;
#10496 = CARTESIAN_POINT ( 'NONE',  ( -180.4654253355437277, 95.69358270527506249, 36.77113452514563363 ) ) ;
#10497 = CARTESIAN_POINT ( 'NONE',  ( 0.000000000000000000, 0.000000000000000000, 40.00000000000003553 ) ) ;
#10498 = LINE ( 'NONE', #42518, #62031 ) ;
#10499 = AXIS2_PLACEMENT_3D ( 'NONE', #23362, #11736, #49709 ) ;
#10500 = ORIENTED_EDGE ( 'NONE', *, *, #33854, .F. ) ;
#10501 = FACE_OUTER_BOUND ( 'NONE', #5614, .T. ) ;
#10502 = VECTOR ( 'NONE', #59714, 1000.000000000000000 ) ;
#10503 = FACE_OUTER_BOUND ( 'NONE', #21510, .T. ) ;
#10504 = CARTESIAN_POINT ( 'NONE',  ( -169.8791831685529985, 83.59058982490282119, 45.09941841846899990 ) ) ;
#10505 = AXIS2_PLACEMENT_3D ( 'NONE', #28042, #11863, #7293 ) ;
#10506 = CARTESIAN_POINT ( 'NONE',  ( -31.92580063159128301, 9.671320706097199960, -77.16174795566554678 ) ) ;
#10507 = ORIENTED_EDGE ( 'NONE', *, *, #36534, .F. ) ;
#10508 = LINE ( 'NONE', #52399, #5028 ) ;
#10509 = ORIENTED_EDGE ( 'NONE', *, *, #29144, .T. ) ;
#10510 = EDGE_LOOP ( 'NONE', ( #62783, #688, #10606, #21869, #28775, #32569, #337, #23067, #54642 ) ) ;
#10511 = CARTESIAN_POINT ( 'NONE',  ( 0.000000000000000000, 0.000000000000000000, 0.000000000000000000 ) ) ;
#10512 = CARTESIAN_POINT ( 'NONE',  ( 212.0803491126037557, 118.9047894217573571, -15.61684406194017960 ) ) ;
#10513 = DIRECTION ( 'NONE',  ( 1.000000000000000000, 0.000000000000000000, 0.000000000000000000 ) ) ;
#10514 = CARTESIAN_POINT ( 'NONE',  ( -156.3790798118594410, 70.23422112803311279, -72.17447922398677917 ) ) ;
#10515 = CARTESIAN_POINT ( 'NONE',  ( -108.6669825835168268, 36.14542924967227577, 87.76374826371203142 ) ) ;
#10516 = FACE_BOUND ( 'NONE', #1797, .T. ) ;
#10517 = LINE ( 'NONE', #37248, #2496 ) ;
#10518 = DIRECTION ( 'NONE',  ( 2.312964634635743450E-16, -0.000000000000000000, 1.000000000000000000 ) ) ;
#10519 = ORIENTED_EDGE ( 'NONE', *, *, #68285, .F. ) ;
#10520 = CARTESIAN_POINT ( 'NONE',  ( -102.2801239173131052, 33.91021738430208643, -88.70367844590326456 ) ) ;
#10521 = ORIENTED_EDGE ( 'NONE', *, *, #13717, .F. ) ;
#10522 = CARTESIAN_POINT ( 'NONE',  ( -71.42546113164833343, 20.75891408601220078, 66.78154372501096248 ) ) ;
#10523 = CARTESIAN_POINT ( 'NONE',  ( 211.0967808702091588, 115.5516932918877018, -74.59216173768591318 ) ) ;
#10524 = FACE_OUTER_BOUND ( 'NONE', #8302, .T. ) ;
#10525 = CARTESIAN_POINT ( 'NONE',  ( -71.56718866013694935, 19.74312628447964002, 13.54490632388451843 ) ) ;
#10526 = CARTESIAN_POINT ( 'NONE',  ( -120.5002574492099114, 44.22930148497322023, 70.18197274062502800 ) ) ;
#10527 = CARTESIAN_POINT ( 'NONE',  ( 15.78827728214693416, 7.507518794609589818, 30.01470767270522089 ) ) ;
#10528 = CARTESIAN_POINT ( 'NONE',  ( 197.3953739035038950, 96.83737926879658175, 92.16504039591205810 ) ) ;
#10529 = CARTESIAN_POINT ( 'NONE',  ( -45.81425895439424067, 46.10914959592843587, 170.0000000000000000 ) ) ;
#10530 = ORIENTED_EDGE ( 'NONE', *, *, #63696, .T. ) ;
#10531 = DIRECTION ( 'NONE',  ( 1.334402673828311860E-15, -1.000000000000000000, 0.000000000000000000 ) ) ;
#10532 = DIRECTION ( 'NONE',  ( 0.000000000000000000, 0.000000000000000000, 1.000000000000000000 ) ) ;
#10533 = ORIENTED_EDGE ( 'NONE', *, *, #41476, .T. ) ;
#10534 = ORIENTED_EDGE ( 'NONE', *, *, #55997, .F. ) ;
#10536 = ADVANCED_FACE ( 'NONE', ( #68988 ), #13807, .T. ) ;
#10535 = CARTESIAN_POINT ( 'NONE',  ( -24.32471770265757982, 9.546495606312149107, -72.08645900122067474 ) ) ;
#10537 = CARTESIAN_POINT ( 'NONE',  ( 0.000000000000000000, 35.00000000000000000, 0.000000000000000000 ) ) ;
#10538 = LINE ( 'NONE', #10194, #67172 ) ;
#10539 = CARTESIAN_POINT ( 'NONE',  ( -59.89379335984725117, 45.06047301136835870, 41.38025477438755928 ) ) ;
#10540 = VECTOR ( 'NONE', #7495, 1000.000000000000114 ) ;
#10541 = CARTESIAN_POINT ( 'NONE',  ( -148.6426981422628444, 63.44891673852537650, 3.913616068001397164 ) ) ;
#10542 = ADVANCED_FACE ( 'NONE', ( #51456 ), #40889, .F. ) ;
#10543 = EDGE_LOOP ( 'NONE', ( #41686, #46294, #63996, #41184, #25059 ) ) ;
#10544 = ADVANCED_FACE ( 'NONE', ( #3603 ), #25071, .F. ) ;
#10545 = ORIENTED_EDGE ( 'NONE', *, *, #941, .F. ) ;
#10546 = CARTESIAN_POINT ( 'NONE',  ( -128.1267916618074878, 49.19573276651589566, 45.29461237954313191 ) ) ;
#10547 = ORIENTED_EDGE ( 'NONE', *, *, #39694, .F. ) ;
#10548 = CYLINDRICAL_SURFACE ( 'NONE', #59281, 5.000000000000004441 ) ;
#10549 = CARTESIAN_POINT ( 'NONE',  ( -147.7925265216585444, 64.04960911618974251, 30.91620572533726374 ) ) ;
#10550 = VECTOR ( 'NONE', #46109, 1000.000000000000000 ) ;
#10551 = CARTESIAN_POINT ( 'NONE',  ( 181.0840389613909736, -170.0000000000000000, 71.15314469597512925 ) ) ;
#10552 = FACE_OUTER_BOUND ( 'NONE', #4431, .T. ) ;
#10553 = VECTOR ( 'NONE', #17179, 1000.000000000000114 ) ;
#10554 = FILL_AREA_STYLE_COLOUR ( '', #23478 ) ;
#10555 = VECTOR ( 'NONE', #48967, 1000.000000000000227 ) ;
#10556 = DIRECTION ( 'NONE',  ( 0.000000000000000000, 0.000000000000000000, 1.000000000000000000 ) ) ;
#10557 = VECTOR ( 'NONE', #20965, 1000.000000000000227 ) ;
#10558 = EDGE_CURVE ( 'NONE', #4675, #15602, #15496, .T. ) ;
#10559 = ORIENTED_EDGE ( 'NONE', *, *, #15348, .T. ) ;
#10560 = ORIENTED_EDGE ( 'NONE', *, *, #21984, .T. ) ;
#10561 = FACE_OUTER_BOUND ( 'NONE', #20899, .T. ) ;
#10562 = DIRECTION ( 'NONE',  ( 0.000000000000000000, -0.5000000000000008882, 0.8660254037844381525 ) ) ;
#10563 = AXIS2_PLACEMENT_3D ( 'NONE', #2956, #45504, #66989 ) ;
#10564 = CARTESIAN_POINT ( 'NONE',  ( 32.89501968360929851, 8.663558833820815153, -66.20267533015858419 ) ) ;
#10565 = CARTESIAN_POINT ( 'NONE',  ( 140.1999945597798671, 45.38880890490931108, -74.37758294665758285 ) ) ;
#10566 = CARTESIAN_POINT ( 'NONE',  ( 70.50372867914784081, 14.53505678900967268, 37.80345282212471858 ) ) ;
#10567 = CARTESIAN_POINT ( 'NONE',  ( 8.289642123990038414, 7.382587591294829998, 91.56333915467209295 ) ) ;
#10568 = ORIENTED_EDGE ( 'NONE', *, *, #63330, .F. ) ;
#10569 = ADVANCED_BREP_SHAPE_REPRESENTATION ( '', ( #41060, #66832 ), #12941 ) ;
#10570 = DIRECTION ( 'NONE',  ( -0.000000000000000000, -0.000000000000000000, 1.000000000000000000 ) ) ;
#10571 = ORIENTED_EDGE ( 'NONE', *, *, #60873, .F. ) ;
#10572 = CARTESIAN_POINT ( 'NONE',  ( -73.10694748374054086, 20.28107308417882848, 32.86053516446196454 ) ) ;
#10573 = EDGE_LOOP ( 'NONE', ( #40343, #21052, #8898, #1185 ) ) ;
#10574 = ORIENTED_EDGE ( 'NONE', *, *, #58374, .F. ) ;
#10575 = CARTESIAN_POINT ( 'NONE',  ( 100.0000000000000284, -5.000000000000000000, 18.50000000000000000 ) ) ;
#10576 = CARTESIAN_POINT ( 'NONE',  ( -180.4643341113398094, 95.69224917234933514, 66.72163245273618770 ) ) ;
#10577 = CARTESIAN_POINT ( 'NONE',  ( 127.2202105166096118, 37.55913282978153944, 60.35159291791857328 ) ) ;
#10578 = ORIENTED_EDGE ( 'NONE', *, *, #5300, .T. ) ;
#10579 = CARTESIAN_POINT ( 'NONE',  ( 150.2809931605061990, 52.27058242113233888, 34.75635080141699262 ) ) ;
#10580 = AXIS2_PLACEMENT_3D ( 'NONE', #59794, #33783, #32733 ) ;
#10581 = DIRECTION ( 'NONE',  ( 0.3090169943749447312, 0.9510565162951544194, -7.147453794906795954E-17 ) ) ;
#10582 = DIRECTION ( 'NONE',  ( 0.000000000000000000, 0.000000000000000000, 1.000000000000000000 ) ) ;
#10583 = CARTESIAN_POINT ( 'NONE',  ( -190.6985136298601731, 109.1272424661242582, -95.00000000000133582 ) ) ;
#10584 = CARTESIAN_POINT ( 'NONE',  ( 137.5911612413395630, 44.91497189902067078, -63.85950958629689467 ) ) ;
#10585 = CARTESIAN_POINT ( 'NONE',  ( -148.6426892915312408, 64.76241938621078020, -61.65738112195565890 ) ) ;
#10586 = VERTEX_POINT ( 'NONE', #46860 ) ;
#10587 = VECTOR ( 'NONE', #12206, 1000.000000000000114 ) ;
#10588 = CARTESIAN_POINT ( 'NONE',  ( 8.000000000000007105, 249.8719672152120381, 0.000000000000000000 ) ) ;
#10589 = CARTESIAN_POINT ( 'NONE',  ( 311.9975424824652350, 0.000000000000000000, 255.6641978984094408 ) ) ;
#10590 = CARTESIAN_POINT ( 'NONE',  ( -180.5801285865471755, 97.42945596116099694, 64.36713565232477663 ) ) ;
#10591 = CARTESIAN_POINT ( 'NONE',  ( 114.9635499210459670, 31.12758084072142140, -91.26968024238497890 ) ) ;
#10592 = LINE ( 'NONE', #64764, #41302 ) ;
#10593 = ADVANCED_FACE ( 'NONE', ( #68327 ), #41579, .T. ) ;
#10594 = CARTESIAN_POINT ( 'NONE',  ( -84.21836162213170951, 25.60181819557224259, 6.007885502826089130 ) ) ;
#10595 = CARTESIAN_POINT ( 'NONE',  ( 0.000000000000000000, 0.000000000000000000, 0.000000000000000000 ) ) ;
#10596 = VECTOR ( 'NONE', #3211, 1000.000000000000000 ) ;
#10597 = CARTESIAN_POINT ( 'NONE',  ( 447.3372781065085633, 365.0000000000001137, -146.4497041420118251 ) ) ;
#10598 = CARTESIAN_POINT ( 'NONE',  ( 197.1966017667921278, 98.19524189129653280, 90.58426338797916344 ) ) ;
#10599 = VECTOR ( 'NONE', #44406, 1000.000000000000000 ) ;
#10600 = LINE ( 'NONE', #5338, #11868 ) ;
#10601 = CARTESIAN_POINT ( 'NONE',  ( -80.56139928459658961, 24.13290941644245535, 72.02333951919742105 ) ) ;
#10602 = CARTESIAN_POINT ( 'NONE',  ( 43.33582519206056816, 9.970536411945046140, -90.41014636795507897 ) ) ;
#10603 = VERTEX_POINT ( 'NONE', #39 ) ;
#10605 = VECTOR ( 'NONE', #31106, 1000.000000000000000 ) ;
#10604 = CARTESIAN_POINT ( 'NONE',  ( -37.37206033059240440, 11.66494618096612612, 6.277285149997919866 ) ) ;
#10606 = ORIENTED_EDGE ( 'NONE', *, *, #41471, .F. ) ;
#10607 = DIRECTION ( 'NONE',  ( 0.7071067811865475727, -0.7071067811865475727, 0.000000000000000000 ) ) ;
#10608 = ORIENTED_EDGE ( 'NONE', *, *, #53288, .T. ) ;
#10609 = CARTESIAN_POINT ( 'NONE',  ( 24.86543818044729193, 29.17542891737278765, 13.32819397642334103 ) ) ;
#10610 = PRESENTATION_STYLE_ASSIGNMENT (( #4649 ) ) ;
#10611 = CARTESIAN_POINT ( 'NONE',  ( -144.2038301586456157, 61.09856042007388055, 59.74016205658093526 ) ) ;
#10612 = DIRECTION ( 'NONE',  ( -0.8160245890732938934, -0.5780171883497599028, 0.000000000000000000 ) ) ;
#10613 = CARTESIAN_POINT ( 'NONE',  ( 138.2136629441928619, 45.30947856186674727, -49.64627368863411050 ) ) ;
#10614 = CARTESIAN_POINT ( 'NONE',  ( 211.6758053788387883, 118.2764674294293457, -94.75375889897657089 ) ) ;
#10615 = CARTESIAN_POINT ( 'NONE',  ( -26.69131247781301752, 59.26697088776972322, 170.0000000000000000 ) ) ;
#10616 = FACE_OUTER_BOUND ( 'NONE', #7524, .T. ) ;
#10617 = VERTEX_POINT ( 'NONE', #33107 ) ;
#10618 = EDGE_CURVE ( 'NONE', #59496, #39183, #18860, .T. ) ;
#10619 = EDGE_LOOP ( 'NONE', ( #31894, #45676, #45909, #49439 ) ) ;
#10621 = EDGE_CURVE ( 'NONE', #16495, #58982, #10592, .T. ) ;
#10620 = CARTESIAN_POINT ( 'NONE',  ( 444.9999999999999432, -35.00000000000000000, 378.0000000000000000 ) ) ;
#10622 = CARTESIAN_POINT ( 'NONE',  ( 0.000000000000000000, 0.000000000000000000, 0.000000000000000000 ) ) ;
#10623 = CARTESIAN_POINT ( 'NONE',  ( -169.1116812882276292, 84.24296059722695418, -9.013269524975111580 ) ) ;
#10624 = ADVANCED_FACE ( 'NONE', ( #54543 ), #48214, .F. ) ;
#10625 = LINE ( 'NONE', #64444, #31922 ) ;
#10626 = ORIENTED_EDGE ( 'NONE', *, *, #27889, .F. ) ;
#10627 = CARTESIAN_POINT ( 'NONE',  ( 284.4933711091047712, 21.89007574053286120, 2.217281872662929754 ) ) ;
#10628 = CARTESIAN_POINT ( 'NONE',  ( -12.78015296493257225, 7.264294661536299991, 70.11165917322330188 ) ) ;
#10629 = PLANE ( 'NONE',  #40535 ) ;
#10630 = FACE_OUTER_BOUND ( 'NONE', #20860, .T. ) ;
#10631 = CARTESIAN_POINT ( 'NONE',  ( 43.14356474118745410, 8.925336319666904217, -22.79396403428114937 ) ) ;
#10632 = DIRECTION ( 'NONE',  ( -1.000000000000000000, 0.000000000000000000, 0.000000000000000000 ) ) ;
#10633 = CARTESIAN_POINT ( 'NONE',  ( 105.5073993722360655, 21.88991381840459383, -2.219103374846306931 ) ) ;
#10634 = CARTESIAN_POINT ( 'NONE',  ( 164.8433205901839074, 64.93586312665797777, 65.15668412550157029 ) ) ;
#10635 = AXIS2_PLACEMENT_3D ( 'NONE', #54358, #22721, #27642 ) ;
#10636 = EDGE_CURVE ( 'NONE', #24965, #59809, #27824, .T. ) ;
#10637 = ORIENTED_EDGE ( 'NONE', *, *, #64391, .T. ) ;
#10638 = CARTESIAN_POINT ( 'NONE',  ( 129.4887940973039804, 40.01039828304094215, 16.28148538411281976 ) ) ;
#10639 = CARTESIAN_POINT ( 'NONE',  ( 74.62299871641508275, -5.461138973197948943, 41.38025477438755928 ) ) ;
#10640 = VECTOR ( 'NONE', #51083, 1000.000000000000000 ) ;
#10641 = CARTESIAN_POINT ( 'NONE',  ( 152.2924710224605462, 54.98503313872889464, 69.18529703667503838 ) ) ;
#10642 = CYLINDRICAL_SURFACE ( 'NONE', #28750, 7.500000000000020428 ) ;
#10643 = FACE_OUTER_BOUND ( 'NONE', #42422, .T. ) ;
#10644 = EDGE_CURVE ( 'NONE', #44856, #33368, #38374, .T. ) ;
#10645 = EDGE_CURVE ( 'NONE', #44574, #10732, #747, .T. ) ;
#10646 = CARTESIAN_POINT ( 'NONE',  ( -14.35185884954381308, 8.414771159230838293, 94.99999999999866418 ) ) ;
#10647 = VECTOR ( 'NONE', #52928, 1000.000000000000000 ) ;
#10648 = ORIENTED_EDGE ( 'NONE', *, *, #61789, .T. ) ;
#10649 = AXIS2_PLACEMENT_3D ( 'NONE', #42127, #58299, #63588 ) ;
#10650 =( NAMED_UNIT ( * ) PLANE_ANGLE_UNIT ( ) SI_UNIT ( $, .RADIAN. ) );
#10651 = VECTOR ( 'NONE', #35516, 1000.000000000000000 ) ;
#10652 = CARTESIAN_POINT ( 'NONE',  ( 109.9975424824652634, 18.08738615523480675, 402.4289050101931480 ) ) ;
#10653 = VERTEX_POINT ( 'NONE', #37676 ) ;
#10654 = ORIENTED_EDGE ( 'NONE', *, *, #32356, .F. ) ;
#10655 = CARTESIAN_POINT ( 'NONE',  ( 46.81205265836391050, 10.50862573052651072, 89.89773165160593749 ) ) ;
#10656 = DIRECTION ( 'NONE',  ( 1.000000000000000000, 0.000000000000000000, 0.000000000000000000 ) ) ;
#10657 = CARTESIAN_POINT ( 'NONE',  ( 141.0229350107040887, 47.12561858623062960, -95.00000000000133582 ) ) ;
#10658 = VERTEX_POINT ( 'NONE', #49261 ) ;
#10659 = CARTESIAN_POINT ( 'NONE',  ( -56.97107423601133291, 15.20373812575555306, -76.82745312835619700 ) ) ;
#10660 = CARTESIAN_POINT ( 'NONE',  ( 31.90217595456442012, 7.552213897210509508, -15.78119844062844734 ) ) ;
#10661 = CARTESIAN_POINT ( 'NONE',  ( 173.7263186949343776, 72.85225335320951956, -45.20748257772405765 ) ) ;
#10662 = CARTESIAN_POINT ( 'NONE',  ( -4.681481898397003683, 6.534749472788141667, -9.500000000000005329 ) ) ;
#10663 = CARTESIAN_POINT ( 'NONE',  ( 87.58098510096635891, 19.74745174099416900, 29.75724612964751259 ) ) ;
#10664 = VERTEX_POINT ( 'NONE', #16569 ) ;
#10665 = CARTESIAN_POINT ( 'NONE',  ( -54.56685407443680447, 15.59259313022788085, -35.21632399845987038 ) ) ;
#10666 = DIRECTION ( 'NONE',  ( 0.9195277725514489076, 0.3930250316539278810, 5.102127870520022769E-18 ) ) ;
#10667 = CARTESIAN_POINT ( 'NONE',  ( 12.91653430408660697, 7.431946598423015971, 30.57340478084518764 ) ) ;
#10668 = CARTESIAN_POINT ( 'NONE',  ( 68.78485849535977081, 14.08475838183477080, -92.04534818299838150 ) ) ;
#10669 = B_SPLINE_CURVE_WITH_KNOTS ( 'NONE', 3,
 ( #61756, #3035, #40311, #30115, #52248, #46622, #8309, #56484, #29758, #35042, #30449, #24498, #18863, #45935, #47908, #57533, #42639, #4069, #2680, #9337, #51220, #64095, #9003, #19191, #40650, #62106, #8660, #69372, #67068, #15910, #13580, #30800, #13922, #29413, #35386, #56844, #26470, #37350, #35738, #46270, #51566, #41008, #58808 ),
 .UNSPECIFIED., .F., .F.,
 ( 4, 2, 2, 2, 2, 2, 2, 2, 2, 2, 2, 2, 1, 2, 2, 2, 2, 2, 2, 2, 2, 4 ),
 ( 0.02371951416048008465, 0.02520633211177543062, 0.02594974108742308105, 0.02669315006307073496, 0.02817996801436603582, 0.02966678596566133322, 0.03041019494130899059, 0.03115360391695664796, 0.03264042186825195924, 0.03412723981954727398, 0.03561405777084258872, 0.03635746674649023569, 0.03710087572213788265, 0.03784428469778552961, 0.03858769367343317658, 0.04007451162472847050, 0.04156132957602376443, 0.04304814752731905836, 0.04379155650296670532, 0.04453496547861433841, 0.04602178342990957682, 0.04750860138120482218 ),
 .UNSPECIFIED. ) ;
#10670 = CARTESIAN_POINT ( 'NONE',  ( -85.97950457423550574, 26.33440868064809237, 89.91133426644037741 ) ) ;
#10672 = ORIENTED_EDGE ( 'NONE', *, *, #45101, .F. ) ;
#10671 = FACE_OUTER_BOUND ( 'NONE', #1307, .T. ) ;
#10673 = ORIENTED_EDGE ( 'NONE', *, *, #22732, .F. ) ;
#10674 = ORIENTED_EDGE ( 'NONE', *, *, #39970, .T. ) ;
#10675 = SURFACE_SIDE_STYLE ('',( #4039 ) ) ;
#10676 = CARTESIAN_POINT ( 'NONE',  ( 28.03046753626767895, -26.14935100755965891, 13.32819397642332682 ) ) ;
#10677 = EDGE_CURVE ( 'NONE', #31197, #19164, #49944, .T. ) ;
#10678 = DIRECTION ( 'NONE',  ( -0.000000000000000000, -0.000000000000000000, -1.000000000000000000 ) ) ;
#10679 = CARTESIAN_POINT ( 'NONE',  ( 188.9999999999999432, -57.00000000000007816, 72.99999999999998579 ) ) ;
#10680 = CARTESIAN_POINT ( 'NONE',  ( -13.29455179262033226, 8.319166883236663423, -21.21143003818049166 ) ) ;
#10681 = DIRECTION ( 'NONE',  ( -0.9009688679024155933, -0.4338837391175656699, 0.000000000000000000 ) ) ;
#10682 = DIRECTION ( 'NONE',  ( -0.000000000000000000, -0.000000000000000000, -1.000000000000000000 ) ) ;
#10684 = ORIENTED_EDGE ( 'NONE', *, *, #33364, .T. ) ;
#10683 = EDGE_CURVE ( 'NONE', #47961, #46223, #10955, .T. ) ;
#10685 = AXIS2_PLACEMENT_3D ( 'NONE', #68390, #57146, #13874 ) ;
#10686 = CARTESIAN_POINT ( 'NONE',  ( -156.8764584803561206, 70.69066846313522490, -43.73679383676832799 ) ) ;
#10687 = ORIENTED_EDGE ( 'NONE', *, *, #11964, .T. ) ;
#10688 = ORIENTED_EDGE ( 'NONE', *, *, #6269, .T. ) ;
#10689 = DIRECTION ( 'NONE',  ( -1.000000000000000000, 0.000000000000000000, 0.000000000000000000 ) ) ;
#10690 = VECTOR ( 'NONE', #41576, 1000.000000000000000 ) ;
#10691 = CARTESIAN_POINT ( 'NONE',  ( -85.73740570227384694, 26.23277384689413694, -45.12853643150059924 ) ) ;
#10692 = CARTESIAN_POINT ( 'NONE',  ( 117.6855018526752161, 32.47998843907879518, 91.79128257728453377 ) ) ;
#10693 = CARTESIAN_POINT ( 'NONE',  ( -156.3734885497381413, 71.59531449004289527, 8.346329245734816382 ) ) ;
#10694 = AXIS2_PLACEMENT_3D ( 'NONE', #41357, #62809, #14614 ) ;
#10695 = VECTOR ( 'NONE', #21629, 1000.000000000000000 ) ;
#10696 = DIRECTION ( 'NONE',  ( 0.5508969814521065267, -0.8345732537212999791, 0.000000000000000000 ) ) ;
#10697 = CARTESIAN_POINT ( 'NONE',  ( 22.81270948571149404, 6.827178363529885274, 40.15439324559184087 ) ) ;
#10698 = LINE ( 'NONE', #4402, #50956 ) ;
#10699 = ORIENTED_EDGE ( 'NONE', *, *, #32324, .F. ) ;
#10700 = ADVANCED_FACE ( 'NONE', ( #6716 ), #19613, .T. ) ;
#10701 = ORIENTED_EDGE ( 'NONE', *, *, #47877, .F. ) ;
#10702 = AXIS2_PLACEMENT_3D ( 'NONE', #66076, #29117, #44594 ) ;
#10703 = ORIENTED_EDGE ( 'NONE', *, *, #56157, .T. ) ;
#10704 = EDGE_CURVE ( 'NONE', #43978, #16942, #54922, .T. ) ;
#10705 = PLANE ( 'NONE',  #20640 ) ;
#10706 = CARTESIAN_POINT ( 'NONE',  ( 36.08914434112044489, 9.014684630517859176, -36.38665694955406593 ) ) ;
#10707 = APPLICATION_CONTEXT ( 'automotive_design' ) ;
#10708 = ADVANCED_FACE ( 'NONE', ( #45042 ), #57251, .F. ) ;
#10709 = DIRECTION ( 'NONE',  ( 1.000000000000000000, -0.000000000000000000, 0.000000000000000000 ) ) ;
#10710 = CARTESIAN_POINT ( 'NONE',  ( 198.2588776805010866, 99.52972231602377917, 59.69594739211307655 ) ) ;
#10711 = ORIENTED_EDGE ( 'NONE', *, *, #31931, .F. ) ;
#10712 = LINE ( 'NONE', #53950, #37950 ) ;
#10713 = CARTESIAN_POINT ( 'NONE',  ( -149.5074843970971017, 64.17983161892348676, 57.56537183036274996 ) ) ;
#10714 = CARTESIAN_POINT ( 'NONE',  ( 23.09590709048885060, 7.852755081912512480, 12.37589148572721953 ) ) ;
#10715 = CARTESIAN_POINT ( 'NONE',  ( -84.49322488516129681, 0.000000000000000000, 43.58025477438756212 ) ) ;
#10716 = CARTESIAN_POINT ( 'NONE',  ( 6.375108774214766072E-14, 36.11269837220805812, 2.000000000000001776 ) ) ;
#10717 = CARTESIAN_POINT ( 'NONE',  ( -82.93267503967652488, 23.99263498936122474, -36.44237337058958559 ) ) ;
#10718 = CARTESIAN_POINT ( 'NONE',  ( 23.24028701062093560, 6.853614888934260740, 65.33720227182544704 ) ) ;
#10719 = DIRECTION ( 'NONE',  ( -1.000000000000000000, -0.000000000000000000, -0.000000000000000000 ) ) ;
#10720 = CARTESIAN_POINT ( 'NONE',  ( 10.13405324523498585, 6.385324379632245417, -74.81575908290277255 ) ) ;
#10721 = B_SPLINE_CURVE_WITH_KNOTS ( 'NONE', 3,
 ( #61167, #31160, #40059, #46974, #23543, #60807, #4411, #55531, #56229, #8045, #12634, #29496, #12991, #61515, #7364, #44981, #25874, #41361, #29158, #39712, #50608, #23883, #13334, #2772, #45685, #67162, #62815, #14618, #52252, #25537, #37105, #5776, #16683, #63848, #11393, #43407, #5440, #53264, #26555, #59240, #15991, #154, #59577, #32868 ),
 .UNSPECIFIED., .F., .F.,
 ( 4, 2, 2, 2, 2, 2, 2, 2, 2, 2, 2, 2, 2, 2, 2, 2, 2, 2, 2, 2, 2, 4 ),
 ( 1.398578778534940505E-17, 0.003433139681083792211, 0.004291424601354686813, 0.005149709521625580981, 0.006866279362167290387, 0.007724564282438155065, 0.008582849202709021477, 0.009441134122979885288, 0.01029941904325075083, 0.01201598888379252529, 0.01373255872433429801, 0.01459084364460517917, 0.01544912856487606553, 0.01630741348514694669, 0.01716569840541783132, 0.01888226824595960751, 0.02059883808650138370, 0.02145712300677229956, 0.02231540792704321888, 0.02403197776758502283, 0.02574854760812682677, 0.02746511744866863072 ),
 .UNSPECIFIED. ) ;
#10722 = B_SPLINE_CURVE_WITH_KNOTS ( 'NONE', 3,
 ( #36738, #20897, #42352, #26862, #48287, #14918 ),
 .UNSPECIFIED., .F., .F.,
 ( 4, 2, 4 ),
 ( 1.095770181106172926E-06, 0.03239442681617710901, 0.06478775786217311206 ),
 .UNSPECIFIED. ) ;
#10723 = EDGE_LOOP ( 'NONE', ( #13621, #18710, #52372, #18212 ) ) ;
#10724 = DIRECTION ( 'NONE',  ( 0.000000000000000000, 0.000000000000000000, 1.000000000000000000 ) ) ;
#10725 = APPLICATION_PROTOCOL_DEFINITION ( 'draft international standard', 'automotive_design', 1998, #31878 ) ;
#10726 = CARTESIAN_POINT ( 'NONE',  ( 175.8963338753314360, 73.51705463274397800, 42.23070144013426130 ) ) ;
#10727 = CARTESIAN_POINT ( 'NONE',  ( -130.2196570250629293, 49.40815211106347959, -48.55858868297418240 ) ) ;
#10728 = EDGE_CURVE ( 'NONE', #11517, #64911, #17260, .T. ) ;
#10729 = CARTESIAN_POINT ( 'NONE',  ( -104.5916564445180796, 35.10571011602409186, -35.36428607247657396 ) ) ;
#10730 = ADVANCED_FACE ( 'NONE', ( #60176 ), #22897, .F. ) ;
#10731 = CARTESIAN_POINT ( 'NONE',  ( 55.52751777340356654, 12.08567914268658683, -69.57556231829563842 ) ) ;
#10732 = VERTEX_POINT ( 'NONE', #43989 ) ;
#10733 = PRODUCT_DEFINITION_SHAPE ( 'NONE', 'NONE',  #69632 ) ;
#10734 = ORIENTED_EDGE ( 'NONE', *, *, #22542, .F. ) ;
#10735 = EDGE_CURVE ( 'NONE', #56044, #67138, #60533, .T. ) ;
#10736 = CARTESIAN_POINT ( 'NONE',  ( -24.19091603582231897, 8.513464105188678133, -14.02971085878847823 ) ) ;
#10737 = CARTESIAN_POINT ( 'NONE',  ( 175.0836463967652605, 72.74684624755143147, 85.98398430601433517 ) ) ;
#10738 = ORIENTED_EDGE ( 'NONE', *, *, #6259, .T. ) ;
#10739 = VECTOR ( 'NONE', #20213, 1000.000000000000000 ) ;
#10740 = ORIENTED_EDGE ( 'NONE', *, *, #14837, .T. ) ;
#10741 = CARTESIAN_POINT ( 'NONE',  ( 110.7114632166111790, 29.09878355652112703, 56.45576479620100940 ) ) ;
#10742 = VERTEX_POINT ( 'NONE', #35449 ) ;
#10743 = FACE_OUTER_BOUND ( 'NONE', #34044, .T. ) ;
#10744 = CARTESIAN_POINT ( 'NONE',  ( 129.1137093889808511, 38.63348691920622713, 31.19545504990886897 ) ) ;
#10745 = AXIS2_PLACEMENT_3D ( 'NONE', #21102, #62970, #52070 ) ;
#10746 = CARTESIAN_POINT ( 'NONE',  ( 140.0820590176526537, 46.51134312115247837, 59.66472826312686095 ) ) ;
#10747 = LINE ( 'NONE', #4444, #22976 ) ;
#10748 = CARTESIAN_POINT ( 'NONE',  ( 81.52811112547603045, 17.74308114851538676, -91.50889126552081621 ) ) ;
#10749 = CIRCLE ( 'NONE', #52337, 4.999999999999997335 ) ;
#10750 = LINE ( 'NONE', #21306, #5780 ) ;
#10751 = CARTESIAN_POINT ( 'NONE',  ( 0.000000000000000000, 0.000000000000000000, -5.000000000000000000 ) ) ;
#10752 =( GEOMETRIC_REPRESENTATION_CONTEXT ( 3 ) GLOBAL_UNCERTAINTY_ASSIGNED_CONTEXT ( ( #2262 ) ) GLOBAL_UNIT_ASSIGNED_CONTEXT ( ( #25461, #51498, #13512 ) ) REPRESENTATION_CONTEXT ( 'NONE', 'WORKASPACE' ) );
#10753 = VECTOR ( 'NONE', #44699, 1000.000000000000000 ) ;
#10754 = EDGE_LOOP ( 'NONE', ( #16020, #40102, #33403, #23452 ) ) ;
#10755 = ORIENTED_EDGE ( 'NONE', *, *, #61855, .F. ) ;
#10756 = CARTESIAN_POINT ( 'NONE',  ( -166.3205068063722081, 81.30869308872871670, 8.302501522647505183 ) ) ;
#10757 = VECTOR ( 'NONE', #66610, 1000.000000000000000 ) ;
#10758 = DIRECTION ( 'NONE',  ( -0.000000000000000000, -0.000000000000000000, -1.000000000000000000 ) ) ;
#10759 = CARTESIAN_POINT ( 'NONE',  ( -174.7800083645696532, 88.99302808536933185, -22.69361122552189869 ) ) ;
#10760 = CARTESIAN_POINT ( 'NONE',  ( -190.6985136298601731, 109.1272424661242582, 94.99999999999866418 ) ) ;
#10762 = ORIENTED_EDGE ( 'NONE', *, *, #45896, .F. ) ;
#10761 = CARTESIAN_POINT ( 'NONE',  ( -149.5074843970971301, 64.17983161892345834, -49.81283053149198992 ) ) ;
#10763 = CARTESIAN_POINT ( 'NONE',  ( 39.77028211725815510, -51.87520073220884598, 6.377659838150125143E-18 ) ) ;
#10764 = ORIENTED_EDGE ( 'NONE', *, *, #62967, .T. ) ;
#10765 = CARTESIAN_POINT ( 'NONE',  ( -126.3508039230933377, 46.79479538767116509, 45.61994787315712330 ) ) ;
#10766 = FACE_OUTER_BOUND ( 'NONE', #35088, .T. ) ;
#10767 = CARTESIAN_POINT ( 'NONE',  ( 86.14852828165528820, 19.25704475759651402, -8.977013608448029203 ) ) ;
#10768 = DIRECTION ( 'NONE',  ( -0.9959742939952397345, 0.08963930890342655666, 0.000000000000000000 ) ) ;
#10769 = EDGE_CURVE ( 'NONE', #48528, #2304, #13993, .T. ) ;
#10770 = DIRECTION ( 'NONE',  ( -1.000000000000000000, 0.000000000000000000, 0.000000000000000000 ) ) ;
#10771 = CARTESIAN_POINT ( 'NONE',  ( -95.19652294162975181, 29.32558722310178823, 13.69184615439291619 ) ) ;
#10772 = CARTESIAN_POINT ( 'NONE',  ( -152.6866856590304735, 66.92104572559831865, -89.15920658215685535 ) ) ;
#10773 = ORIENTED_EDGE ( 'NONE', *, *, #29862, .T. ) ;
#10774 = VERTEX_POINT ( 'NONE', #9066 ) ;
#10775 = CARTESIAN_POINT ( 'NONE',  ( 186.6054783416232112, 84.37128553200975034, -75.67012523732033458 ) ) ;
#10776 = FACE_OUTER_BOUND ( 'NONE', #60970, .T. ) ;
#10777 = CARTESIAN_POINT ( 'NONE',  ( -165.9986675144416211, 79.53506019208359135, -39.84463087508462564 ) ) ;
#10778 = PLANE ( 'NONE',  #59853 ) ;
#10779 = CARTESIAN_POINT ( 'NONE',  ( 106.4072861358878299, 28.24787347451998798, -63.81749795290593852 ) ) ;
#10780 = CARTESIAN_POINT ( 'NONE',  ( -75.00636493611888511, 22.03142602679957207, -62.89598738381337029 ) ) ;
#10781 = CARTESIAN_POINT ( 'NONE',  ( 429.8372781065087338, 388.0000000000066507, -123.9497041420121235 ) ) ;
#10782 = CARTESIAN_POINT ( 'NONE',  ( 46.65860211212413589, 10.48377752989034128, -41.16074490250159812 ) ) ;
#10783 = CARTESIAN_POINT ( 'NONE',  ( 211.7451286015360949, 116.5372661580811666, 66.13550906399829898 ) ) ;
#10784 = ADVANCED_FACE ( 'NONE', ( #8728 ), #33803, .T. ) ;
#10785 = ORIENTED_EDGE ( 'NONE', *, *, #11877, .F. ) ;
#10786 = CARTESIAN_POINT ( 'NONE',  ( -108.9136445001390001, 36.28030794288192595, -12.16150055407688058 ) ) ;
#10787 = EDGE_LOOP ( 'NONE', ( #50395, #54175, #55009, #26614 ) ) ;
#10788 = DIRECTION ( 'NONE',  ( 1.000000000000000000, 0.000000000000000000, -0.000000000000000000 ) ) ;
#10789 = CARTESIAN_POINT ( 'NONE',  ( -45.99287130332146489, 23.53639479597885398, 26.66469104408688295 ) ) ;
#10790 = EDGE_CURVE ( 'NONE', #56693, #989, #30178, .T. ) ;
#10791 = CARTESIAN_POINT ( 'NONE',  ( -85.00384554948603011, 24.83757696374530965, -92.28742627645222285 ) ) ;
#10792 = B_SPLINE_CURVE_WITH_KNOTS ( 'NONE', 3,
 ( #8664, #63159, #41697, #67751, #36078, #10032, #9694, #9007, #14955, #52251, #68431, #47645, #19195, #36420, #31159, #35389, #31487, #3713, #30453, #40656, #57537, #46625, #4409, #56847, #24833, #41011, #52590, #62109, #4073, #30120, #62465, #68100, #19904, #14281, #58216, #25873, #47301, #35741, #41360, #15311, #13926, #62813, #57192 ),
 .UNSPECIFIED., .F., .F.,
 ( 4, 2, 2, 2, 2, 2, 2, 2, 2, 2, 2, 2, 1, 2, 2, 2, 2, 2, 2, 2, 2, 4 ),
 ( 0.02358007599568757648, 0.02505677178601659061, 0.02579511968118109247, 0.02653346757634559433, 0.02801016336667459805, 0.02948685915700360524, 0.03022520705216810710, 0.03096355494733261243, 0.03244025073766165779, 0.03391694652799069620, 0.03539364231831973462, 0.03613199021348427464, 0.03687033810864881467, 0.03760868600381335469, 0.03834703389897789472, 0.03982372968930697477, 0.04130042547963604788, 0.04277712126996512099, 0.04351546916512966101, 0.04425381706029420104, 0.04573051285062328802, 0.04720720864095238195 ),
 .UNSPECIFIED. ) ;
#10793 = CARTESIAN_POINT ( 'NONE',  ( 112.1100957124161539, 30.86846953551571104, 2.987587920464681357 ) ) ;
#10794 = CARTESIAN_POINT ( 'NONE',  ( -78.66644367742109978, 23.39876645725288640, -23.27090004125422595 ) ) ;
#10795 = EDGE_CURVE ( 'NONE', #68783, #31812, #35640, .T. ) ;
#10796 = AXIS2_PLACEMENT_3D ( 'NONE', #44896, #56485, #29414 ) ;
#10797 = CARTESIAN_POINT ( 'NONE',  ( -101.3537077702550562, 33.43904726487055967, -61.90219306547648159 ) ) ;
#10798 = CARTESIAN_POINT ( 'NONE',  ( -101.8140949286062238, 33.67224128592401655, -8.170026674512227416 ) ) ;
#10799 = AXIS2_PLACEMENT_3D ( 'NONE', #2708, #31508, #9028 ) ;
#10800 = AXIS2_PLACEMENT_3D ( 'NONE', #4015, #20185, #57825 ) ;
#10801 = VERTEX_POINT ( 'NONE', #14676 ) ;
#10802 = CARTESIAN_POINT ( 'NONE',  ( 211.9471657255442949, 116.8466227750260344, 92.33050231943069264 ) ) ;
#10803 = CARTESIAN_POINT ( 'NONE',  ( 141.9165763529819344, 192.0000000000000000, 129.0000000000000284 ) ) ;
#10804 = EDGE_LOOP ( 'NONE', ( #48687, #23451, #50641, #18575 ) ) ;
#10805 = PRODUCT_DEFINITION_FORMATION_WITH_SPECIFIED_SOURCE ( 'ANY', '', #45703, .NOT_KNOWN. ) ;
#10806 = CARTESIAN_POINT ( 'NONE',  ( 70.65683382808195745, 25.18281821780106355, 43.58025477438756212 ) ) ;
#10807 = CARTESIAN_POINT ( 'NONE',  ( 8.683910719548892487, 7.383368463746304400, -72.27984568902408569 ) ) ;
#10808 = DIRECTION ( 'NONE',  ( 0.000000000000000000, -1.000000000000000000, 0.000000000000000000 ) ) ;
#10809 = CARTESIAN_POINT ( 'NONE',  ( 46.85361596800670725, 10.51535167202354515, -68.97966382706947286 ) ) ;
#10810 = VECTOR ( 'NONE', #46773, 1000.000000000000000 ) ;
#10811 = CARTESIAN_POINT ( 'NONE',  ( 281.6139602183311013, -21.48286796535249721, 4.743729604094155228 ) ) ;
#10812 = LINE ( 'NONE', #33676, #42337 ) ;
#10813 = CARTESIAN_POINT ( 'NONE',  ( 79.97476514061575870, 18.30994623469640104, 94.42742991237855676 ) ) ;
#10814 = CIRCLE ( 'NONE', #11971, 8.000000000000000000 ) ;
#10815 = ORIENTED_EDGE ( 'NONE', *, *, #62148, .F. ) ;
#10816 = CARTESIAN_POINT ( 'NONE',  ( 620.5071894358655982, 928.5915846175170145, 486.5068267241127842 ) ) ;
#10817 = CARTESIAN_POINT ( 'NONE',  ( -58.00979178563853367, 29.32343869649098878, 40.00000000000003553 ) ) ;
#10818 = CARTESIAN_POINT ( 'NONE',  ( -131.7724154034330297, 50.48821165954358037, 15.93959937002138716 ) ) ;
#10819 = CARTESIAN_POINT ( 'NONE',  ( -107.7886332494339570, 36.81249801143972888, 69.97670749553998348 ) ) ;
#10820 = CARTESIAN_POINT ( 'NONE',  ( -180.6010819689385301, 95.85959870121170923, 91.43127333083813824 ) ) ;
#10821 = VERTEX_POINT ( 'NONE', #52988 ) ;
#10822 = DIRECTION ( 'NONE',  ( -0.9839295885986295565, -0.1785568947986370392, 0.000000000000000000 ) ) ;
#10823 = CARTESIAN_POINT ( 'NONE',  ( -6.126800896373028493, 6.786243985899684361, -23.38278218708607525 ) ) ;
#10824 = EDGE_CURVE ( 'NONE', #21633, #31241, #36827, .T. ) ;
#10825 = B_SPLINE_CURVE_WITH_KNOTS ( 'NONE', 3,
 ( #48413, #601, #22056, #245, #64977, #43153, #16437, #32957, #38231, #49114, #59673, #22406, #54752, #43845, #1302, #22754, #34714, #12914, #44192, #61087, #12207, #8323, #34370, #50534, #7969, #23806, #13255, #2013, #28734, #61436, #17468, #50874, #7281, #23108, #66040, #28375, #55100, #66729, #17833, #39290, #66390, #38949, #6926, #49822, #55816 ),
 .UNSPECIFIED., .F., .F.,
 ( 4, 2, 2, 1, 2, 2, 2, 2, 2, 2, 2, 2, 2, 2, 2, 2, 2, 2, 2, 2, 2, 2, 4 ),
 ( 0.02346464386237014782, 0.02493212228186625704, 0.02566586149161431685, 0.02639960070136237319, 0.02713333991111042953, 0.02786707912085848587, 0.02933455754035460203, 0.03006829675010265837, 0.03080203595985071124, 0.03226951437934682393, 0.03300325358909487333, 0.03373699279884292968, 0.03520447121833904236, 0.03667194963783515504, 0.03740568884758320445, 0.03813942805733125385, 0.03960690647682736654, 0.04107438489632347228, 0.04254186331581957803, 0.04327560252556764131, 0.04400934173531569071, 0.04547682015481180340, 0.04694429857430792302 ),
 .UNSPECIFIED. ) ;
#10826 = CARTESIAN_POINT ( 'NONE',  ( 197.5344433744249386, 98.61756151884681287, -14.73665922601220757 ) ) ;
#10827 = CARTESIAN_POINT ( 'NONE',  ( -155.6121305361943143, 69.53530207094544835, 87.54207503471559448 ) ) ;
#10828 = CARTESIAN_POINT ( 'NONE',  ( 141.3707934840545022, 46.15056991286790122, 36.98067333115320565 ) ) ;
#10829 = EDGE_LOOP ( 'NONE', ( #67970, #52613, #98, #33206 ) ) ;
#10830 = DIRECTION ( 'NONE',  ( 0.000000000000000000, 0.000000000000000000, -1.000000000000000000 ) ) ;
#10831 = CARTESIAN_POINT ( 'NONE',  ( 79.19119222799092483, 18.06817527909834098, 11.36162365658382356 ) ) ;
#10832 = CARTESIAN_POINT ( 'NONE',  ( 161.7006237583813402, 62.31514460450498660, 3.854726898469810425 ) ) ;
#10833 = DIRECTION ( 'NONE',  ( -1.000000000000000000, -0.000000000000000000, -0.000000000000000000 ) ) ;
#10834 = ORIENTED_EDGE ( 'NONE', *, *, #63454, .T. ) ;
#10835 = CARTESIAN_POINT ( 'NONE',  ( -0.2727178028659107412, 0.000000000000000000, 0.000000000000000000 ) ) ;
#10836 = ORIENTED_EDGE ( 'NONE', *, *, #49373, .T. ) ;
#10837 = AXIS2_PLACEMENT_3D ( 'NONE', #5248, #302, #48818 ) ;
#10838 = CARTESIAN_POINT ( 'NONE',  ( -75.43953471071002070, 21.11829282998124668, -22.55799270516261146 ) ) ;
#10839 = CARTESIAN_POINT ( 'NONE',  ( 69.73342236697681074, 14.33173522011653311, -73.43652197196315967 ) ) ;
#10840 = CARTESIAN_POINT ( 'NONE',  ( -61.86403937395564157, 16.61416349803656090, 40.96657735976691583 ) ) ;
#10841 = CIRCLE ( 'NONE', #53516, 245.3095347406802489 ) ;
#10843 = VERTEX_POINT ( 'NONE', #47712 ) ;
#10842 = CARTESIAN_POINT ( 'NONE',  ( 149.9683128897950155, 53.28564708287390772, 10.59517325904875662 ) ) ;
#10844 = CARTESIAN_POINT ( 'NONE',  ( 159.6593397521790791, 59.37286298965128850, 29.72214504742798624 ) ) ;
#10845 = LINE ( 'NONE', #4203, #21559 ) ;
#10846 = DIRECTION ( 'NONE',  ( 0.000000000000000000, 0.000000000000000000, -1.000000000000000000 ) ) ;
#10847 = AXIS2_PLACEMENT_3D ( 'NONE', #32459, #53550, #32117 ) ;
#10848 = ORIENTED_EDGE ( 'NONE', *, *, #20333, .T. ) ;
#10849 = ORIENTED_EDGE ( 'NONE', *, *, #56442, .F. ) ;
#10850 = FACE_OUTER_BOUND ( 'NONE', #63710, .T. ) ;
#10851 = EDGE_CURVE ( 'NONE', #22589, #20231, #41764, .T. ) ;
#10852 = AXIS2_PLACEMENT_3D ( 'NONE', #30942, #36562, #68567 ) ;
#10853 = CARTESIAN_POINT ( 'NONE',  ( 7.484861546145933353, -64.56761454192826477, 170.0000000000000000 ) ) ;
#10854 = EDGE_CURVE ( 'NONE', #9719, #21528, #61537, .T. ) ;
#10855 = CARTESIAN_POINT ( 'NONE',  ( -180.0094637318086370, 96.72611451757710199, 35.34088033557112851 ) ) ;
#10856 = CARTESIAN_POINT ( 'NONE',  ( 126.6266894765173419, 38.37986986668738609, 65.91793733211123651 ) ) ;
#10857 = ORIENTED_EDGE ( 'NONE', *, *, #13025, .T. ) ;
#10858 = ORIENTED_EDGE ( 'NONE', *, *, #7947, .F. ) ;
#10859 = EDGE_LOOP ( 'NONE', ( #40307, #14428, #62803, #55921 ) ) ;
#10860 = DIRECTION ( 'NONE',  ( 0.000000000000000000, 1.000000000000000000, 0.000000000000000000 ) ) ;
#10861 = CARTESIAN_POINT ( 'NONE',  ( -102.7447593990059289, 34.14748189312170723, 3.674523915951409148 ) ) ;
#10862 = PLANE ( 'NONE',  #54875 ) ;
#10863 = DIRECTION ( 'NONE',  ( 1.000000000000000000, 0.000000000000000000, 0.000000000000000000 ) ) ;
#10864 = CARTESIAN_POINT ( 'NONE',  ( -26.00000000000000000, 0.000000000000000000, -2.818925648462311923E-15 ) ) ;
#10865 = DIRECTION ( 'NONE',  ( -1.000000000000000000, 0.000000000000000000, -0.000000000000000000 ) ) ;
#10866 = CARTESIAN_POINT ( 'NONE',  ( -132.9109786433856186, 51.29129389542018203, 67.62515982255897029 ) ) ;
#10867 = DIRECTION ( 'NONE',  ( -1.000000000000000000, 0.000000000000000000, 2.135044278125301096E-16 ) ) ;
#10868 = ORIENTED_EDGE ( 'NONE', *, *, #51245, .F. ) ;
#10869 = DIRECTION ( 'NONE',  ( 0.3930250316539278255, -0.9195277725514487965, -9.090529987421286498E-17 ) ) ;
#10870 = EDGE_LOOP ( 'NONE', ( #24126, #32764, #62167, #10916, #13445, #62557, #68941, #47675, #25896 ) ) ;
#10871 = DIRECTION ( 'NONE',  ( -1.792759282944425749E-18, -4.776790026843733425E-18, -1.000000000000000000 ) ) ;
#10872 = EDGE_CURVE ( 'NONE', #38069, #32692, #41422, .T. ) ;
#10873 = CARTESIAN_POINT ( 'NONE',  ( 206.3125232506203872, 108.5822159704962075, -63.33511981463161078 ) ) ;
#10874 = DIRECTION ( 'NONE',  ( 0.000000000000000000, 0.000000000000000000, 1.000000000000000000 ) ) ;
#10875 = EDGE_CURVE ( 'NONE', #27866, #57040, #6500, .T. ) ;
#10876 = CARTESIAN_POINT ( 'NONE',  ( 412.3372781065085633, 400.0000000000000568, -111.4497041420117682 ) ) ;
#10877 = CARTESIAN_POINT ( 'NONE',  ( -37.36232632813460697, 10.63891575123902200, -91.90072181533541595 ) ) ;
#10878 = CARTESIAN_POINT ( 'NONE',  ( 22.90619343622340054, 7.840927939412484449, 35.10082476785152039 ) ) ;
#10879 = CARTESIAN_POINT ( 'NONE',  ( 198.3689982626052313, 98.05019997562733636, 86.36795352984687213 ) ) ;
#10880 = CARTESIAN_POINT ( 'NONE',  ( -125.8938041572051105, 46.49392987655492959, -76.75825448869764500 ) ) ;
#10881 = B_SPLINE_CURVE_WITH_KNOTS ( 'NONE', 3,
 ( #3888, #30974, #26035, #8480, #14780, #3208, #24662, #36244, #52420, #47130, #68594, #21106, #63670, #33034, #53432, #65045, #42548, #36935, #54109, #32348, #64004, #32001, #59743, #31647, #16505, #10878, #318, #37608, #11557, #59062, #5261, #16155, #68926, #27747, #15815, #37258, #16843, #22127, #53774, #26381, #48483, #58372, #10527 ),
 .UNSPECIFIED., .F., .F.,
 ( 4, 2, 2, 2, 2, 2, 2, 2, 1, 2, 2, 2, 2, 2, 2, 2, 2, 2, 2, 2, 2, 4 ),
 ( 0.000000000000000000, 0.001466285743483475203, 0.002199428615225213022, 0.002932571486966950407, 0.004398857230450435585, 0.005865142973933920763, 0.007331428717417405073, 0.008064571589159148096, 0.008797714460900890251, 0.009530857332642634142, 0.01026400020438437630, 0.01173028594786783806, 0.01319657169135130155, 0.01466285743483476331, 0.01539600030657650546, 0.01612914317831825109, 0.01759542892180173193, 0.01906171466528521971, 0.01979485753702697054, 0.02052800040876871790, 0.02199428615225220915, 0.02346057189573570387 ),
 .UNSPECIFIED. ) ;
#10882 = ORIENTED_EDGE ( 'NONE', *, *, #14912, .T. ) ;
#10883 = DIRECTION ( 'NONE',  ( 0.000000000000000000, 0.000000000000000000, -1.000000000000000000 ) ) ;
#10884 = DIRECTION ( 'NONE',  ( 0.1342332658176522420, 0.9909497617679351444, 0.000000000000000000 ) ) ;
#10885 = VERTEX_POINT ( 'NONE', #46687 ) ;
#10886 = ORIENTED_EDGE ( 'NONE', *, *, #65532, .F. ) ;
#10887 = CARTESIAN_POINT ( 'NONE',  ( -26.88234027341226096, 9.904106450608207268, -75.63871759701287090 ) ) ;
#10888 = CARTESIAN_POINT ( 'NONE',  ( 55.57657751403269941, 11.06944050856661832, -44.20687798256333423 ) ) ;
#10889 = CIRCLE ( 'NONE', #3081, 2.999999999999999112 ) ;
#10890 = DIRECTION ( 'NONE',  ( 1.000000000000000000, 0.000000000000000000, 0.000000000000000000 ) ) ;
#10891 = VECTOR ( 'NONE', #15405, 1000.000000000000000 ) ;
#10892 = ORIENTED_EDGE ( 'NONE', *, *, #33419, .T. ) ;
#10893 = ORIENTED_EDGE ( 'NONE', *, *, #37724, .T. ) ;
#10894 = CARTESIAN_POINT ( 'NONE',  ( -130.5904357464317798, 50.88938808445630713, 43.98754880289844493 ) ) ;
#10895 = VECTOR ( 'NONE', #8954, 1000.000000000000000 ) ;
#10896 = ORIENTED_EDGE ( 'NONE', *, *, #63842, .F. ) ;
#10897 = CARTESIAN_POINT ( 'NONE',  ( -20.55634918610408945, -26.11269837220804035, 0.000000000000000000 ) ) ;
#10898 = FACE_OUTER_BOUND ( 'NONE', #29450, .T. ) ;
#10899 = CARTESIAN_POINT ( 'NONE',  ( 62.04326772936976653, 12.44884401098615534, 56.70505522888109340 ) ) ;
#10900 = CARTESIAN_POINT ( 'NONE',  ( -57.97933172774389732, 6.473286776202990644, 27.58472315868180047 ) ) ;
#10901 = AXIS2_PLACEMENT_3D ( 'NONE', #35899, #8830, #51392 ) ;
#10902 = LINE ( 'NONE', #48513, #42587 ) ;
#10903 = LINE ( 'NONE', #64367, #49186 ) ;
#10904 = ORIENTED_EDGE ( 'NONE', *, *, #42697, .F. ) ;
#10905 = EDGE_LOOP ( 'NONE', ( #65462, #4726, #57157, #8855 ) ) ;
#10906 = PLANE ( 'NONE',  #62624 ) ;
#10907 = PLANE ( 'NONE',  #36177 ) ;
#10908 = DIRECTION ( 'NONE',  ( 1.000000000000000000, 1.387778780781445922E-16, 0.000000000000000000 ) ) ;
#10909 = CARTESIAN_POINT ( 'NONE',  ( 181.0840389613909736, -170.0000000000000000, 36.80859410551140343 ) ) ;
#10910 = CARTESIAN_POINT ( 'NONE',  ( 70.02892116572940040, 14.40944430928137088, 39.98237600456136676 ) ) ;
#10911 = CARTESIAN_POINT ( 'NONE',  ( 9.628853386404982118, 7.387802178417762100, 86.91185589324661009 ) ) ;
#10912 = VERTEX_POINT ( 'NONE', #31898 ) ;
#10913 = CARTESIAN_POINT ( 'NONE',  ( 79.53408731553408018, 17.12082763744059832, 12.84865754040789732 ) ) ;
#10914 = EDGE_LOOP ( 'NONE', ( #57946, #30950 ) ) ;
#10915 = DIRECTION ( 'NONE',  ( -0.000000000000000000, 1.000000000000000000, -0.000000000000000000 ) ) ;
#10916 = ORIENTED_EDGE ( 'NONE', *, *, #22390, .T. ) ;
#10917 = B_SPLINE_CURVE_WITH_KNOTS ( 'NONE', 3,
 ( #49541, #60103, #33397, #11925, #1373, #20484, #54468, #52832 ),
 .UNSPECIFIED., .F., .F.,
 ( 4, 2, 2, 4 ),
 ( 0.02285338877108900393, 0.02519297479642216772, 0.02636276780908874962, 0.02753256082175533151 ),
 .UNSPECIFIED. ) ;
#10918 = ORIENTED_EDGE ( 'NONE', *, *, #63068, .T. ) ;
#10919 = CARTESIAN_POINT ( 'NONE',  ( -118.3948752128398496, 42.92869324237092599, 11.57276413738803456 ) ) ;
#10920 = PLANE ( 'NONE',  #14833 ) ;
#10921 = EDGE_CURVE ( 'NONE', #15873, #38606, #31220, .T. ) ;
#10922 = CARTESIAN_POINT ( 'NONE',  ( 131.6189313563687620, 40.08924984825279125, 71.02825006529253926 ) ) ;
#10923 = ORIENTED_EDGE ( 'NONE', *, *, #14255, .T. ) ;
#10924 = AXIS2_PLACEMENT_3D ( 'NONE', #2453, #60494, #29187 ) ;
#10925 = EDGE_CURVE ( 'NONE', #23974, #31182, #64895, .T. ) ;
#10926 = CARTESIAN_POINT ( 'NONE',  ( -444.4229916354184979, 394.6798985497181320, 96.05029585798874336 ) ) ;
#10927 = VECTOR ( 'NONE', #60724, 1000.000000000000000 ) ;
#10928 = CARTESIAN_POINT ( 'NONE',  ( 150.4550062612852628, 52.39582885725848627, 39.61425003142517198 ) ) ;
#10929 = CARTESIAN_POINT ( 'NONE',  ( 69.72789637502502558, 15.37065610545704253, 33.95776896090188757 ) ) ;
#10930 = EDGE_CURVE ( 'NONE', #11717, #61489, #53330, .T. ) ;
#10931 = DIRECTION ( 'NONE',  ( -2.724194322196142817E-16, 0.6427876096865404731, 0.7660444431189771253 ) ) ;
#10932 = DIRECTION ( 'NONE',  ( -1.000000000000000000, 0.000000000000000000, 0.000000000000000000 ) ) ;
#10933 = DIRECTION ( 'NONE',  ( -0.000000000000000000, -0.000000000000000000, -1.000000000000000000 ) ) ;
#10934 = FACE_OUTER_BOUND ( 'NONE', #53819, .T. ) ;
#10935 = AXIS2_PLACEMENT_3D ( 'NONE', #21876, #32787, #32098 ) ;
#10936 = CARTESIAN_POINT ( 'NONE',  ( -143.8756912989387047, 60.83492035645716811, -64.19810953127340269 ) ) ;
#10937 = EDGE_LOOP ( 'NONE', ( #52914, #66851, #14980, #28136 ) ) ;
#10938 = EDGE_CURVE ( 'NONE', #38117, #51614, #60367, .T. ) ;
#10939 = CARTESIAN_POINT ( 'NONE',  ( 2.700000000000004619, 0.000000000000000000, -24.69999999999999929 ) ) ;
#10940 = AXIS2_PLACEMENT_3D ( 'NONE', #11016, #37398, #28235 ) ;
#10941 = CARTESIAN_POINT ( 'NONE',  ( -7.825402957745083654, 6.891034867348166948, -77.26262132240753999 ) ) ;
#10942 = CARTESIAN_POINT ( 'NONE',  ( -175.1895962157337010, 90.99110972060685754, 57.94477835241939090 ) ) ;
#10943 = DIRECTION ( 'NONE',  ( 1.000000000000000000, 0.000000000000000000, -0.000000000000000000 ) ) ;
#10944 = CARTESIAN_POINT ( 'NONE',  ( -118.8691191306315034, 43.21907118237573542, -39.77302265458806119 ) ) ;
#10945 = CARTESIAN_POINT ( 'NONE',  ( -86.16710354151693707, 26.41338104675948628, 11.30814425100590981 ) ) ;
#10946 = AXIS2_PLACEMENT_3D ( 'NONE', #10163, #47109, #63301 ) ;
#10947 = CARTESIAN_POINT ( 'NONE',  ( 0.000000000000000000, 0.000000000000000000, 0.000000000000000000 ) ) ;
#10948 = B_SPLINE_CURVE_WITH_KNOTS ( 'NONE', 3,
 ( #36946, #64018, #10541, #37623, #15147, #53785, #32017, #63683, #68938, #64354, #47143, #68606, #58056, #53445, #14793, #16168, #41879, #9876, #27064, #333, #4583, #21787, #36257, #57713, #9527, #26051, #13256, #60119, #61437, #7637, #29088, #13593, #66731, #18527, #61767, #34715, #11939, #43236, #33411, #11231, #38674, #55817, #50535, #7970, #23807, #56153, #1042, #27765 ),
 .UNSPECIFIED., .F., .F.,
 ( 4, 2, 2, 2, 2, 2, 2, 2, 2, 2, 2, 2, 2, 2, 2, 2, 2, 2, 2, 2, 2, 2, 2, 4 ),
 ( 0.02746511744866864113, 0.02914922134997090242, 0.03083332525127316370, 0.03251742915257542499, 0.03335948110322658339, 0.03420153305387774179, 0.03504358500452890712, 0.03588563695518006552, 0.03756974085648233375, 0.03841179280713347827, 0.03925384475778461585, 0.04009589670843575343, 0.04093794865908689795, 0.04262205256038916618, 0.04430615646169144134, 0.04514820841234259974, 0.04599026036299375120, 0.04767436426429605412, 0.04935846816559835704, 0.05020052011624950850, 0.05104257206690067383, 0.05272667596820304614, 0.05356872791885423923, 0.05441077986950544620 ),
 .UNSPECIFIED. ) ;
#10949 = CARTESIAN_POINT ( 'NONE',  ( 111.6145892210130199, 21.48294702482179375, -4.743341903180122721 ) ) ;
#10950 = CARTESIAN_POINT ( 'NONE',  ( -71.79801807585624829, 19.82313861722078485, -93.28382037184846354 ) ) ;
#10951 = CARTESIAN_POINT ( 'NONE',  ( 70.46452034227871764, 14.52462608639675601, 9.463287704965392066 ) ) ;
#10952 = DIRECTION ( 'NONE',  ( 0.9362348706397417564, -0.3513748240813305279, 0.000000000000000000 ) ) ;
#10953 = CARTESIAN_POINT ( 'NONE',  ( 42.60735219095521131, 9.864569470531383999, -90.02523864352265548 ) ) ;
#10954 = ORIENTED_EDGE ( 'NONE', *, *, #41139, .T. ) ;
#10955 = CIRCLE ( 'NONE', #27833, 65.36598343705435354 ) ;
#10956 = CARTESIAN_POINT ( 'NONE',  ( -35.38962320578855980, 11.29584325137388134, 17.25183784669100362 ) ) ;
#10957 = ORIENTED_EDGE ( 'NONE', *, *, #33293, .F. ) ;
#10958 = CARTESIAN_POINT ( 'NONE',  ( 109.9975424824652634, 295.8720703627916464, 535.5371946177799600 ) ) ;
#10959 = VERTEX_POINT ( 'NONE', #33646 ) ;
#10960 = ADVANCED_FACE ( 'NONE', ( #1274 ), #17086, .T. ) ;
#10961 = CARTESIAN_POINT ( 'NONE',  ( 20.74561700410410836, 7.717362891868937425, -64.21423502926538163 ) ) ;
#10962 = CARTESIAN_POINT ( 'NONE',  ( 117.1441767749777227, 33.33376675874068695, 93.81895193412631784 ) ) ;
#10963 = DIRECTION ( 'NONE',  ( 1.000000000000000000, 0.000000000000000000, 0.000000000000000000 ) ) ;
#10964 = DIRECTION ( 'NONE',  ( 0.000000000000000000, -0.000000000000000000, 1.000000000000000000 ) ) ;
#10965 = DIRECTION ( 'NONE',  ( 0.000000000000000000, 0.000000000000000000, -1.000000000000000000 ) ) ;
#10966 = DIRECTION ( 'NONE',  ( -0.000000000000000000, -0.000000000000000000, -1.000000000000000000 ) ) ;
#10967 = B_SPLINE_CURVE_WITH_KNOTS ( 'NONE', 3,
 ( #18782, #12823, #7547, #29680, #13846, #55011, #49728, #29007, #28286, #41277, #4666, #68687, #19825, #19468, #26132, #30726, #14201, #68361, #47229, #14877, #62738, #35659, #63425, #69023, #8927, #57452, #42310, #20850, #52173, #3993, #30033, #9961, #3299, #63771, #35308, #68020, #20499, #46193, #25460, #14542, #36002, #52844, #41964, #47567 ),
 .UNSPECIFIED., .F., .F.,
 ( 4, 2, 2, 2, 2, 2, 2, 2, 2, 2, 2, 2, 2, 2, 2, 2, 2, 2, 2, 2, 2, 4 ),
 ( 0.000000000000000000, 0.003518733725596323494, 0.004398417156995387996, 0.005278100588394452931, 0.007037467451192651324, 0.007917150882591747485, 0.008796834313990845380, 0.01055620117678908107, 0.01231556803958732023, 0.01319525147098642159, 0.01407493490238551775, 0.01495461833378461738, 0.01583430176518371701, 0.01671398519658281664, 0.01759366862798191627, 0.01935303549078009819, 0.02111240235357827663, 0.02199208578497733116, 0.02287176921637638222, 0.02463113607917447739, 0.02639050294197257604, 0.02814986980477066775 ),
 .UNSPECIFIED. ) ;
#10968 = CARTESIAN_POINT ( 'NONE',  ( 196.9999999999999716, 1.500000000000015321, -48.49999999999998579 ) ) ;
#10969 = CARTESIAN_POINT ( 'NONE',  ( -125.8938041572051389, 47.69968343338780414, -8.069153307770243089 ) ) ;
#10970 = VERTEX_POINT ( 'NONE', #27649 ) ;
#10971 = ORIENTED_EDGE ( 'NONE', *, *, #63782, .F. ) ;
#10972 = CARTESIAN_POINT ( 'NONE',  ( 34.45972925205163051, 8.830088223935240066, 58.59592793524065257 ) ) ;
#10973 = CARTESIAN_POINT ( 'NONE',  ( -166.2053056899074761, 81.18967388993337408, 62.24998455618286641 ) ) ;
#10974 = CYLINDRICAL_SURFACE ( 'NONE', #18393, 5.000000000000000888 ) ;
#10975 = LINE ( 'NONE', #25797, #56619 ) ;
#10976 = ORIENTED_EDGE ( 'NONE', *, *, #21815, .F. ) ;
#10977 = CARTESIAN_POINT ( 'NONE',  ( 93.72059824125561533, 23.03897520779758423, 12.86014247970559410 ) ) ;
#10978 = CARTESIAN_POINT ( 'NONE',  ( 188.5838389098762775, 88.03667982118680868, -16.57130179220268573 ) ) ;
#10979 = CARTESIAN_POINT ( 'NONE',  ( 212.1976655298229275, 119.0878071902807562, 9.685308493262699159 ) ) ;
#10980 = CIRCLE ( 'NONE', #18831, 185.0000000000000000 ) ;
#10981 = CARTESIAN_POINT ( 'NONE',  ( -84.89017518714956623, 25.87942398301715130, -92.09563210729065474 ) ) ;
#10982 = CARTESIAN_POINT ( 'NONE',  ( 46.50704915687941821, 9.440294391580033917, -13.86102426116064557 ) ) ;
#10983 = DIRECTION ( 'NONE',  ( -1.000000000000000000, 0.000000000000000000, 0.000000000000000000 ) ) ;
#10984 = FACE_BOUND ( 'NONE', #48313, .T. ) ;
#10985 = CARTESIAN_POINT ( 'NONE',  ( -50.92620509423088038, 55.07344309828769724, 170.0000000000000000 ) ) ;
#10986 = B_SPLINE_CURVE_WITH_KNOTS ( 'NONE', 3,
 ( #57170, #8642, #30094, #66698, #51549, #18493, #24814, #61400, #13225, #34687, #46249, #8983, #56122, #63823, #47284, #4724, #5754, #46953, #21588, #48300, #41675, #64511, #26536, #25856, #10686, #15635, #37084, #43038, #52569, #68738, #36749, #47970, #134, #31467, #20554, #5422, #10015, #52903, #31136, #4392, #20218, #32162, #42018, #26190 ),
 .UNSPECIFIED., .F., .F.,
 ( 4, 2, 2, 2, 2, 2, 2, 2, 2, 2, 2, 2, 2, 2, 2, 2, 2, 2, 2, 2, 2, 4 ),
 ( 1.387778780781445676E-17, 0.003433139681083829942, 0.004291424601354737987, 0.005149709521625646033, 0.006866279362167389266, 0.007724564282438267822, 0.008582849202709144643, 0.009441134122980024065, 0.01029941904325090002, 0.01201598888379267101, 0.01373255872433444200, 0.01459084364460533703, 0.01544912856487623380, 0.01630741348514713057, 0.01716569840541802561, 0.01888226824595980180, 0.02059883808650157105, 0.02145712300677249038, 0.02231540792704340623, 0.02403197776758515466, 0.02574854760812689963, 0.02746511744866864460 ),
 .UNSPECIFIED. ) ;
#10987 = VECTOR ( 'NONE', #48855, 1000.000000000000000 ) ;
#10988 = ORIENTED_EDGE ( 'NONE', *, *, #26678, .F. ) ;
#10989 = VECTOR ( 'NONE', #60744, 1000.000000000000000 ) ;
#10990 = CARTESIAN_POINT ( 'NONE',  ( -95.54114085644955878, 29.48728305236672398, 94.99999999999866418 ) ) ;
#10991 = CARTESIAN_POINT ( 'NONE',  ( 0.000000000000000000, -26.09918303830819397, 30.00000000000000000 ) ) ;
#10992 = CARTESIAN_POINT ( 'NONE',  ( -47.94960849910473399, 13.92522873833625852, 67.11944450877264501 ) ) ;
#10993 = DIRECTION ( 'NONE',  ( -0.6910626489868580968, -0.7227948638273978821, 0.000000000000000000 ) ) ;
#10994 = DIRECTION ( 'NONE',  ( 1.000000000000000000, 7.993605777301127091E-15, 0.000000000000000000 ) ) ;
#10995 = FACE_OUTER_BOUND ( 'NONE', #10723, .T. ) ;
#10996 = AXIS2_PLACEMENT_3D ( 'NONE', #56114, #29383, #40621 ) ;
#10997 = EDGE_CURVE ( 'NONE', #27271, #21605, #49442, .T. ) ;
#10998 = EDGE_LOOP ( 'NONE', ( #64553, #57549, #21744, #31268 ) ) ;
#10999 = CARTESIAN_POINT ( 'NONE',  ( 62.52742438962776106, 12.55954017561947822, 17.96841034875761878 ) ) ;
#11000 = CARTESIAN_POINT ( 'NONE',  ( -57.42615654242918311, 15.33060010148602537, 71.78055872622512368 ) ) ;
#11001 = ORIENTED_EDGE ( 'NONE', *, *, #47714, .F. ) ;
#11002 = VECTOR ( 'NONE', #44534, 1000.000000000000000 ) ;
#11003 = VERTEX_POINT ( 'NONE', #928 ) ;
#11004 = CARTESIAN_POINT ( 'NONE',  ( 32.66637210955355641, 8.640188015362515017, 94.41850791232543827 ) ) ;
#11005 = CARTESIAN_POINT ( 'NONE',  ( 39.40195752203892710, 8.409560354027375340, -77.46436805589148378 ) ) ;
#11006 = CARTESIAN_POINT ( 'NONE',  ( 107.9362503323352769, 27.82881837607801856, 44.26364398048654181 ) ) ;
#11007 = ORIENTED_EDGE ( 'NONE', *, *, #19603, .F. ) ;
#11008 = CARTESIAN_POINT ( 'NONE',  ( -62.30100056228381078, 16.74548393487071607, -67.56937781552855427 ) ) ;
#11009 = CARTESIAN_POINT ( 'NONE',  ( 31.91375106836930797, 7.553354707452895944, -16.76326003512198781 ) ) ;
#11010 = CARTESIAN_POINT ( 'NONE',  ( -78.66644367742109978, 23.39876645725289706, -88.80455181264524356 ) ) ;
#11011 = CARTESIAN_POINT ( 'NONE',  ( 164.8818489117101365, 63.65095510281860669, 89.38953086370848666 ) ) ;
#11012 = CARTESIAN_POINT ( 'NONE',  ( 90.30166390191405412, 20.70652093100729019, 30.65456310424210784 ) ) ;
#11013 = B_SPLINE_CURVE_WITH_KNOTS ( 'NONE', 3,
 ( #58779, #43640, #20815, #64069, #15881, #5660, #48215, #65118, #32416, #63737, #42944, #26097, #59474, #10594, #48554, #36996, #38030, #64414, #32065, #21169, #54544, #42614, #58436, #10945, #748, #11284, #16223, #38375, #5333, #37678, #389, #21845, #26788, #43290, #11634, #32754, #59124, #64766, #33108, #54185, #6006, #27466, #47526, #48910, #42274, #15545 ),
 .UNSPECIFIED., .F., .F.,
 ( 4, 2, 2, 2, 2, 2, 2, 2, 2, 2, 2, 2, 2, 2, 2, 2, 2, 2, 2, 2, 2, 2, 4 ),
 ( 0.02420077021543441328, 0.02572112563160186202, 0.02648130333968560374, 0.02724148104776934545, 0.02876183646393683582, 0.02952201417202058101, 0.03028219188010432619, 0.03180254729627181309, 0.03332290271243929652, 0.03408308042052303477, 0.03484325812860676608, 0.03636361354477423563, 0.03712379125285796694, 0.03788396896094169825, 0.03864414666902542955, 0.03940432437710916086, 0.04092467979327661654, 0.04244503520944406527, 0.04396539062561151401, 0.04548574604177896274, 0.04624592374986269405, 0.04700610145794641148, 0.04852645687411390879 ),
 .UNSPECIFIED. ) ;
#11014 = ORIENTED_EDGE ( 'NONE', *, *, #8349, .T. ) ;
#11015 = EDGE_CURVE ( 'NONE', #32122, #29231, #579, .T. ) ;
#11016 = CARTESIAN_POINT ( 'NONE',  ( 0.000000000000000000, 0.000000000000000000, -9.500000000000000000 ) ) ;
#11017 = CARTESIAN_POINT ( 'NONE',  ( 8.000000000000007105, 249.8719672152120381, -95.00000000000133582 ) ) ;
#11018 = CARTESIAN_POINT ( 'NONE',  ( 10.82760985890677574, 7.398654328676807168, 43.16107762503957446 ) ) ;
#11019 = CARTESIAN_POINT ( 'NONE',  ( 63.82878426028240426, 12.86248996312277804, -89.44302009434157696 ) ) ;
#11020 = LINE ( 'NONE', #25922, #41851 ) ;
#11021 = CARTESIAN_POINT ( 'NONE',  ( -85.63158118751694303, 26.18843205417604025, 94.40781586612253307 ) ) ;
#11023 = VERTEX_POINT ( 'NONE', #59646 ) ;
#11022 = DIRECTION ( 'NONE',  ( 0.000000000000000000, 0.000000000000000000, -1.000000000000000000 ) ) ;
#11024 = ORIENTED_EDGE ( 'NONE', *, *, #58374, .T. ) ;
#11025 = EDGE_CURVE ( 'NONE', #805, #29948, #22729, .T. ) ;
#11026 = ORIENTED_EDGE ( 'NONE', *, *, #27865, .T. ) ;
#11027 = CARTESIAN_POINT ( 'NONE',  ( -14.94265033805046095, 7.459411036484907775, -18.48943493301132435 ) ) ;
#11028 = CARTESIAN_POINT ( 'NONE',  ( -170.7899427064031386, 86.05659250431358487, 84.87755278391203717 ) ) ;
#11029 = FACE_OUTER_BOUND ( 'NONE', #32271, .T. ) ;
#11030 = CARTESIAN_POINT ( 'NONE',  ( 26.99999999999999645, -30.00000000000000355, 15.00000000000000000 ) ) ;
#11031 = CARTESIAN_POINT ( 'NONE',  ( -59.95412189755936794, 17.09836075175412873, -48.41403164313221907 ) ) ;
#11032 = PLANE ( 'NONE',  #7375 ) ;
#11033 = CIRCLE ( 'NONE', #35768, 242.4895526022646379 ) ;
#11034 = CARTESIAN_POINT ( 'NONE',  ( 153.2282895792480417, 54.42637815496165388, -76.65839619712716058 ) ) ;
#11035 = CARTESIAN_POINT ( 'NONE',  ( 18.89064107370902335, 6.619789970027396997, -9.341755237627822339 ) ) ;
#11036 = ORIENTED_EDGE ( 'NONE', *, *, #6430, .T. ) ;
#11037 = DIRECTION ( 'NONE',  ( -1.000000000000000000, 0.000000000000000000, 0.000000000000000000 ) ) ;
#11038 = ORIENTED_EDGE ( 'NONE', *, *, #69516, .T. ) ;
#11039 = ORIENTED_EDGE ( 'NONE', *, *, #23029, .T. ) ;
#11040 = EDGE_CURVE ( 'NONE', #55571, #44856, #16581, .T. ) ;
#11041 = CARTESIAN_POINT ( 'NONE',  ( 68.94948716683070700, 15.16699441119058100, -20.98926308138244679 ) ) ;
#11042 = DIRECTION ( 'NONE',  ( -0.000000000000000000, -1.000000000000000000, -0.000000000000000000 ) ) ;
#11044 = ADVANCED_FACE ( 'NONE', ( #49090 ), #6197, .T. ) ;
#11043 = CARTESIAN_POINT ( 'NONE',  ( -152.5101325120252795, 68.10842280990928543, 18.26319916783852904 ) ) ;
#11045 = ADVANCED_FACE ( 'NONE', ( #16406 ), #3153, .T. ) ;
#11046 = PRESENTATION_LAYER_ASSIGNMENT (  '', '', ( #26819 ) ) ;
#11047 = CARTESIAN_POINT ( 'NONE',  ( 187.5325688887159572, 85.37769363979907666, -39.85688821852441777 ) ) ;
#11048 = LINE ( 'NONE', #32509, #50557 ) ;
#11049 = CARTESIAN_POINT ( 'NONE',  ( -153.9360907722259242, 69.37825751209838643, 85.85008364023016725 ) ) ;
#11050 = ORIENTED_EDGE ( 'NONE', *, *, #66030, .F. ) ;
#11051 = ORIENTED_EDGE ( 'NONE', *, *, #39858, .T. ) ;
#11052 = ORIENTED_EDGE ( 'NONE', *, *, #53882, .F. ) ;
#11053 = CARTESIAN_POINT ( 'NONE',  ( -151.6797345123119101, 67.37848486615945376, -8.276130779850848995 ) ) ;
#11054 = DIRECTION ( 'NONE',  ( 1.000000000000000000, 0.000000000000000000, -0.000000000000000000 ) ) ;
#11055 = B_SPLINE_CURVE_WITH_KNOTS ( 'NONE', 3,
 ( #20726, #31625, #3180, #30948, #52396, #67544, #19341, #35533, #8805, #43891, #27372, #26696, #16481, #38634, #6267, #15792, #48811, #65374, #63978, #37936, #54441, #59381, #11193, #22453, #5909, #652, #1001, #43545, #21751, #53060, #292, #21080, #49162, #47791, #60076, #37235, #4889, #17160, #48128, #48458, #27029, #42523, #10506, #58686 ),
 .UNSPECIFIED., .F., .F.,
 ( 4, 2, 2, 2, 2, 2, 2, 2, 2, 2, 2, 2, 2, 2, 2, 2, 2, 2, 2, 2, 2, 4 ),
 ( 0.000000000000000000, 0.001476829494128818624, 0.002215244241193236718, 0.002953658988257660233, 0.004430488482386508997, 0.005907317976515357762, 0.007384147470644206526, 0.008122562217708613128, 0.008860976964773019729, 0.01033780645890184161, 0.01181463595303066175, 0.01255305070009507355, 0.01329146544715948536, 0.01476829494128835060, 0.01550670968835276588, 0.01624512443541718462, 0.01772195392954600476, 0.01919878342367482491, 0.01993719817073923845, 0.02067561291780365199, 0.02215244241193248947, 0.02362927190606133043 ),
 .UNSPECIFIED. ) ;
#11056 = CARTESIAN_POINT ( 'NONE',  ( -32.41982179707235900, 9.753975577087189208, 57.10945888221309730 ) ) ;
#11057 = DIRECTION ( 'NONE',  ( 0.000000000000000000, 0.000000000000000000, 1.000000000000000000 ) ) ;
#11058 = VERTEX_POINT ( 'NONE', #17811 ) ;
#11059 = CARTESIAN_POINT ( 'NONE',  ( -10.00000000000000000, 1.224646799147353256E-15, -50.00000000000000711 ) ) ;
#11060 = DIRECTION ( 'NONE',  ( 0.000000000000000000, 1.000000000000000000, 0.000000000000000000 ) ) ;
#11061 = DIRECTION ( 'NONE',  ( -0.000000000000000000, -1.000000000000000000, -0.000000000000000000 ) ) ;
#11062 = DIRECTION ( 'NONE',  ( 0.000000000000000000, 0.000000000000000000, -1.000000000000000000 ) ) ;
#11063 = CARTESIAN_POINT ( 'NONE',  ( -422.6627218934914367, 0.000000000000000000, -146.4497041420118251 ) ) ;
#11064 = CARTESIAN_POINT ( 'NONE',  ( -444.4229916354184979, 394.6798985497180752, -129.3091912309550935 ) ) ;
#11065 = CARTESIAN_POINT ( 'NONE',  ( 23.09541709302173018, 6.844586979481589673, 62.65178007441200947 ) ) ;
#11066 = CARTESIAN_POINT ( 'NONE',  ( -49.42000000000000171, -26.09918303830819397, 20.41169613715280207 ) ) ;
#11067 = CARTESIAN_POINT ( 'NONE',  ( -2.000000000000000000, -2.000000000000000000, 0.000000000000000000 ) ) ;
#11068 = ORIENTED_EDGE ( 'NONE', *, *, #54016, .F. ) ;
#11069 = CARTESIAN_POINT ( 'NONE',  ( -31.11269837220801193, 36.11269837220812207, 0.000000000000000000 ) ) ;
#11070 = SHAPE_DEFINITION_REPRESENTATION ( #55795, #2894 ) ;
#11071 = LINE ( 'NONE', #53631, #43086 ) ;
#11072 = CARTESIAN_POINT ( 'NONE',  ( -126.3458714439411068, 46.79154809309477514, -49.91370389823397602 ) ) ;
#11073 = CARTESIAN_POINT ( 'NONE',  ( 41.81982603358024875, 8.735900550613184379, -62.84812721213725695 ) ) ;
#11074 = CARTESIAN_POINT ( 'NONE',  ( 56.52885800925554349, 12.28784885070978738, -73.86213855357162572 ) ) ;
#11075 = EDGE_LOOP ( 'NONE', ( #20004, #53474, #62375, #7123, #60136, #46985, #59718, #34816 ) ) ;
#11076 = EDGE_CURVE ( 'NONE', #60572, #10912, #5842, .T. ) ;
#11077 = ORIENTED_EDGE ( 'NONE', *, *, #13353, .T. ) ;
#11078 = B_SPLINE_CURVE_WITH_KNOTS ( 'NONE', 3,
 ( #34446, #23873, #18241, #39013, #29837, #22825 ),
 .UNSPECIFIED., .F., .F.,
 ( 4, 2, 4 ),
 ( 0.03218941534092207429, 0.06469837595388627793, 0.09720733656685046076 ),
 .UNSPECIFIED. ) ;
#11079 = DIRECTION ( 'NONE',  ( 0.4738686624730094610, -0.8805955318567322276, 0.000000000000000000 ) ) ;
#11080 = CARTESIAN_POINT ( 'NONE',  ( 197.2847860006354210, 98.30530166401518954, 8.711940037960845373 ) ) ;
#11081 = ORIENTED_EDGE ( 'NONE', *, *, #5183, .F. ) ;
#11082 = ADVANCED_FACE ( 'NONE', ( #65292 ), #65651, .F. ) ;
#11083 = ORIENTED_EDGE ( 'NONE', *, *, #45213, .F. ) ;
#11084 = CARTESIAN_POINT ( 'NONE',  ( 181.5079096844946775, 80.47139261082472217, 29.30859410551139277 ) ) ;
#11085 = PLANE ( 'NONE',  #16711 ) ;
#11086 = ORIENTED_EDGE ( 'NONE', *, *, #66647, .T. ) ;
#11087 = CARTESIAN_POINT ( 'NONE',  ( 115.7612476187724013, 32.64200929566222698, 69.05872566142198821 ) ) ;
#11088 = CARTESIAN_POINT ( 'NONE',  ( 141.9165763529819344, 242.0000000000000000, 129.0000000000000000 ) ) ;
#11089 = VECTOR ( 'NONE', #49055, 1000.000000000000000 ) ;
#11090 = CARTESIAN_POINT ( 'NONE',  ( 139.3041645503688244, 46.00819478311335331, 58.69386422334632414 ) ) ;
#11091 = CARTESIAN_POINT ( 'NONE',  ( -74.19961951691013269, 20.67022044985854023, -48.64513555268851519 ) ) ;
#11092 = CARTESIAN_POINT ( 'NONE',  ( 161.9809705076523301, 61.24480272096906930, -91.30888859218912046 ) ) ;
#11093 = VECTOR ( 'NONE', #11949, 999.9999999999998863 ) ;
#11094 = CARTESIAN_POINT ( 'NONE',  ( 92.51858280840787074, 21.51505926344915309, -47.99226530103682364 ) ) ;
#11095 = DIRECTION ( 'NONE',  ( 0.000000000000000000, 0.000000000000000000, 1.000000000000000000 ) ) ;
#11096 = EDGE_CURVE ( 'NONE', #3858, #51807, #16747, .T. ) ;
#11097 = ORIENTED_EDGE ( 'NONE', *, *, #14685, .T. ) ;
#11099 = ORIENTED_EDGE ( 'NONE', *, *, #68923, .T. ) ;
#11098 = EDGE_CURVE ( 'NONE', #31799, #51103, #12183, .T. ) ;
#11100 = CARTESIAN_POINT ( 'NONE',  ( 50.97490815085634352, 6.000000000000000000, -9.435653166495500344 ) ) ;
#11101 = FACE_OUTER_BOUND ( 'NONE', #15793, .T. ) ;
#11102 = DIRECTION ( 'NONE',  ( -0.9999168736529502333, 0.000000000000000000, 0.01289363347198224652 ) ) ;
#11103 = EDGE_CURVE ( 'NONE', #43378, #57196, #55074, .T. ) ;
#11104 = FACE_OUTER_BOUND ( 'NONE', #30669, .T. ) ;
#11106 = VERTEX_POINT ( 'NONE', #49794 ) ;
#11105 = CARTESIAN_POINT ( 'NONE',  ( -144.7571537022063808, 60.25265659240449878, -48.12163853905629907 ) ) ;
#11107 = FACE_OUTER_BOUND ( 'NONE', #9131, .T. ) ;
#11108 = ADVANCED_FACE ( 'NONE', ( #66014 ), #39265, .F. ) ;
#11109 = ORIENTED_EDGE ( 'NONE', *, *, #4123, .F. ) ;
#11110 = CARTESIAN_POINT ( 'NONE',  ( -143.2471548081022945, 59.04577938365766698, 60.90355539476639990 ) ) ;
#11111 = FACE_OUTER_BOUND ( 'NONE', #61284, .T. ) ;
#11112 = FACE_OUTER_BOUND ( 'NONE', #3171, .T. ) ;
#11113 = CARTESIAN_POINT ( 'NONE',  ( 63.01563776193090405, 13.70579113808098093, -8.876140241706053757 ) ) ;
#11114 = CARTESIAN_POINT ( 'NONE',  ( -430.1627218934916073, 399.9999999999998863, -123.9497041420119530 ) ) ;
#11115 = CARTESIAN_POINT ( 'NONE',  ( 197.3685896092615906, 96.80423329231983587, 8.239818201410752607 ) ) ;
#11116 = LINE ( 'NONE', #37856, #66202 ) ;
#11117 = LINE ( 'NONE', #26271, #68809 ) ;
#11118 = VERTEX_POINT ( 'NONE', #32249 ) ;
#11119 = ORIENTED_EDGE ( 'NONE', *, *, #16639, .F. ) ;
#11120 = EDGE_CURVE ( 'NONE', #16987, #44224, #64599, .T. ) ;
#11121 = CARTESIAN_POINT ( 'NONE',  ( 188.5662303205147055, 86.51341602961784361, -69.97109685562328707 ) ) ;
#11122 = FACE_OUTER_BOUND ( 'NONE', #37349, .T. ) ;
#11123 = DIRECTION ( 'NONE',  ( -0.000000000000000000, -0.000000000000000000, 1.000000000000000000 ) ) ;
#11125 = EDGE_CURVE ( 'NONE', #45414, #51882, #31112, .T. ) ;
#11124 = DIRECTION ( 'NONE',  ( -0.7071067811865474617, 0.000000000000000000, 0.7071067811865474617 ) ) ;
#11126 = ADVANCED_FACE ( 'NONE', ( #50851 ), #18847, .T. ) ;
#11127 = DIRECTION ( 'NONE',  ( 1.000000000000000000, 0.000000000000000000, -0.000000000000000000 ) ) ;
#11128 = CARTESIAN_POINT ( 'NONE',  ( -76.33235143960692426, 22.51916353135074544, -62.32845455250863154 ) ) ;
#11129 = CARTESIAN_POINT ( 'NONE',  ( 66.94365390260637128, 14.65531706601759865, -49.61441550408923007 ) ) ;
#11130 = CARTESIAN_POINT ( 'NONE',  ( -122.3759299995709284, 45.41285412136510757, 31.47923061853353488 ) ) ;
#11131 = LINE ( 'NONE', #54020, #35184 ) ;
#11132 = ORIENTED_EDGE ( 'NONE', *, *, #23759, .F. ) ;
#11133 = CARTESIAN_POINT ( 'NONE',  ( -25.07735481787161191, 9.648965052008787069, 6.892143237745487205 ) ) ;
#11134 = VERTEX_POINT ( 'NONE', #45572 ) ;
#11135 = CARTESIAN_POINT ( 'NONE',  ( -13.78709718204647494, 7.352743657744182926, -47.49489084203693068 ) ) ;
#11136 = CARTESIAN_POINT ( 'NONE',  ( 188.9999999999999432, 225.0000000000000000, 0.000000000000000000 ) ) ;
#11137 = CARTESIAN_POINT ( 'NONE',  ( -149.5074843970971301, -170.0000000000000000, 30.72082123989904900 ) ) ;
#11138 = CARTESIAN_POINT ( 'NONE',  ( 111.1865443042261603, 30.43181341527237649, 2.811416016180984023 ) ) ;
#11139 = LINE ( 'NONE', #32604, #5179 ) ;
#11140 = VECTOR ( 'NONE', #51084, 1000.000000000000000 ) ;
#11141 = CARTESIAN_POINT ( 'NONE',  ( -99.10904156412041743, 32.31949011661294691, -62.54589874766276836 ) ) ;
#11142 = DIRECTION ( 'NONE',  ( -0.000000000000000000, -0.000000000000000000, -1.000000000000000000 ) ) ;
#11143 = VECTOR ( 'NONE', #50892, 1000.000000000000000 ) ;
#11144 = ORIENTED_EDGE ( 'NONE', *, *, #55497, .F. ) ;
#11145 = CARTESIAN_POINT ( 'NONE',  ( 133.8566784816069344, -170.0000000000000000, 10.16579024853168889 ) ) ;
#11146 = CYLINDRICAL_SURFACE ( 'NONE', #64538, 5.000000000000004441 ) ;
#11147 = ORIENTED_EDGE ( 'NONE', *, *, #25287, .F. ) ;
#11148 = CARTESIAN_POINT ( 'NONE',  ( 56.52885800925551507, 12.28784885070979449, 60.36061439874682577 ) ) ;
#11149 = DIRECTION ( 'NONE',  ( -0.000000000000000000, -0.000000000000000000, -1.000000000000000000 ) ) ;
#11150 = CARTESIAN_POINT ( 'NONE',  ( -28.13266652174640114, 9.071935854491421480, 17.60819673564329335 ) ) ;
#11151 = CARTESIAN_POINT ( 'NONE',  ( -15.55634918610408945, -26.11269837220804035, 0.000000000000000000 ) ) ;
#11152 = CARTESIAN_POINT ( 'NONE',  ( -1.876547441458561227, 6.576559737910138814, 33.04152043553114027 ) ) ;
#11153 = CARTESIAN_POINT ( 'NONE',  ( -104.5730787903383145, 33.96058035148152499, -62.20252787994973431 ) ) ;
#11154 = CARTESIAN_POINT ( 'NONE',  ( 82.33194843254320006, 19.05534674436356113, 84.71864657193529524 ) ) ;
#11155 = ORIENTED_EDGE ( 'NONE', *, *, #61473, .F. ) ;
#11156 = CARTESIAN_POINT ( 'NONE',  ( 643.1876992948958787, 1011.457451940547003, 612.5068267248708480 ) ) ;
#11157 = VECTOR ( 'NONE', #55500, 1000.000000000000000 ) ;
#11158 = CARTESIAN_POINT ( 'NONE',  ( -836.0476379851789943, -568.5227338237882577, 10.00000000000000000 ) ) ;
#11159 = CARTESIAN_POINT ( 'NONE',  ( -128.9925397612933011, 48.56800623462828526, 4.441519302985077466 ) ) ;
#11160 = CARTESIAN_POINT ( 'NONE',  ( -167.4844853368928455, 82.52074065752739784, -47.16599507922662582 ) ) ;
#11161 = ITEM_DEFINED_TRANSFORMATION ( 'NONE', 'NONE', #61332,  #66832 ) ;
#11162 = CARTESIAN_POINT ( 'NONE',  ( -127.6894679065405143, 48.89973668460849865, -35.11786550867761036 ) ) ;
#11163 = VERTEX_POINT ( 'NONE', #50158 ) ;
#11164 = CARTESIAN_POINT ( 'NONE',  ( 47.99999999999997158, 19.99999999999996447, 4.000000000000000000 ) ) ;
#11165 = CARTESIAN_POINT ( 'NONE',  ( -10.96274578891745755, -22.46815979931523799, 0.000000000000000000 ) ) ;
#11166 = CARTESIAN_POINT ( 'NONE',  ( 204.6977192012829789, 108.0580384837234931, -9.481380442157895772 ) ) ;
#11167 = DIRECTION ( 'NONE',  ( -0.000000000000000000, -0.000000000000000000, -1.000000000000000000 ) ) ;
#11168 = ADVANCED_FACE ( 'NONE', ( #8647, #7945 ), #29397, .T. ) ;
#11169 = FACE_OUTER_BOUND ( 'NONE', #34042, .T. ) ;
#11170 = ORIENTED_EDGE ( 'NONE', *, *, #37793, .T. ) ;
#11171 = CARTESIAN_POINT ( 'NONE',  ( 230.9999999999999432, 0.000000000000000000, -2.000000000000000000 ) ) ;
#11172 = CARTESIAN_POINT ( 'NONE',  ( 110.2429982417149432, 28.88204397445228722, -62.76698815611734972 ) ) ;
#11173 = CARTESIAN_POINT ( 'NONE',  ( 110.2429982417149290, 28.88204397445231209, -50.92243756565370916 ) ) ;
#11174 = VECTOR ( 'NONE', #49172, 1000.000000000000114 ) ;
#11175 = ORIENTED_EDGE ( 'NONE', *, *, #35410, .T. ) ;
#11176 = EDGE_CURVE ( 'NONE', #41448, #55844, #1986, .T. ) ;
#11177 = CARTESIAN_POINT ( 'NONE',  ( 60.58000000000000540, -26.09918303830819397, 15.41169613715280562 ) ) ;
#11178 = ORIENTED_EDGE ( 'NONE', *, *, #42162, .F. ) ;
#11179 = CARTESIAN_POINT ( 'NONE',  ( -119.3119126656025770, 42.31023367294505988, -92.49952378818520060 ) ) ;
#11180 = LINE ( 'NONE', #22092, #48397 ) ;
#11181 = CIRCLE ( 'NONE', #47144, 65.36598343705435354 ) ;
#11182 = EDGE_CURVE ( 'NONE', #44112, #5953, #40299, .T. ) ;
#11184 = ORIENTED_EDGE ( 'NONE', *, *, #19229, .T. ) ;
#11183 = DIRECTION ( 'NONE',  ( 0.000000000000000000, 0.000000000000000000, 1.000000000000000000 ) ) ;
#11185 = CARTESIAN_POINT ( 'NONE',  ( 164.3702714028688092, 63.22112480708617710, 39.86111796590435574 ) ) ;
#11186 = DIRECTION ( 'NONE',  ( -0.000000000000000000, 1.000000000000000000, -0.000000000000000000 ) ) ;
#11187 = VECTOR ( 'NONE', #67603, 1000.000000000000000 ) ;
#11188 = CARTESIAN_POINT ( 'NONE',  ( -77.71801202538874520, 23.03755222122951096, -35.16063552580117602 ) ) ;
#11189 = ORIENTED_EDGE ( 'NONE', *, *, #33754, .F. ) ;
#11190 = FACE_OUTER_BOUND ( 'NONE', #28622, .T. ) ;
#11191 = DIRECTION ( 'NONE',  ( -0.000000000000000000, -0.000000000000000000, -1.000000000000000000 ) ) ;
#11192 = CARTESIAN_POINT ( 'NONE',  ( 15.55634918610400241, -10.55634918610406281, 0.000000000000000000 ) ) ;
#11193 = CARTESIAN_POINT ( 'NONE',  ( -38.92726670956011503, 10.94099576009806007, -70.15049777360351868 ) ) ;
#11194 = ORIENTED_EDGE ( 'NONE', *, *, #17132, .T. ) ;
#11195 = EDGE_LOOP ( 'NONE', ( #43138, #50240, #35379, #36120, #11963, #1632, #41191, #63277, #68258, #42912 ) ) ;
#11196 = EDGE_LOOP ( 'NONE', ( #8971, #27558 ) ) ;
#11197 = VECTOR ( 'NONE', #34857, 1000.000000000000000 ) ;
#11199 = EDGE_CURVE ( 'NONE', #43402, #64171, #13568, .T. ) ;
#11198 = CARTESIAN_POINT ( 'NONE',  ( -190.6985136298601731, 109.1272424661242582, 94.99999999999866418 ) ) ;
#11200 = CARTESIAN_POINT ( 'NONE',  ( -48.41612563322100016, 13.00196567016870297, 94.99999999999866418 ) ) ;
#11201 = CYLINDRICAL_SURFACE ( 'NONE', #29050, 35.00000000000000000 ) ;
#11202 = CARTESIAN_POINT ( 'NONE',  ( -156.7487895666416193, 70.57327586518564999, -71.13043712117229234 ) ) ;
#11203 = CARTESIAN_POINT ( 'NONE',  ( 65.61520826398337647, 13.28986957332403840, 83.93644943505340450 ) ) ;
#11204 = EDGE_CURVE ( 'NONE', #28933, #37212, #6545, .T. ) ;
#11205 = LINE ( 'NONE', #31985, #66301 ) ;
#11206 = CARTESIAN_POINT ( 'NONE',  ( 181.0840389613909736, 80.03940679743415387, -89.91415884680696990 ) ) ;
#11207 = DIRECTION ( 'NONE',  ( -4.463998536185269061E-17, -2.459865942543005358E-16, 1.000000000000000000 ) ) ;
#11208 = ORIENTED_EDGE ( 'NONE', *, *, #8825, .F. ) ;
#11209 = DIRECTION ( 'NONE',  ( 0.000000000000000000, 0.000000000000000000, -1.000000000000000000 ) ) ;
#11210 = ORIENTED_EDGE ( 'NONE', *, *, #50771, .F. ) ;
#11211 = DIRECTION ( 'NONE',  ( 0.000000000000000000, 0.000000000000000000, 1.000000000000000000 ) ) ;
#11212 =( REPRESENTATION_RELATIONSHIP ('NONE','NONE', #40274, #15003 ) REPRESENTATION_RELATIONSHIP_WITH_TRANSFORMATION ( #879 )SHAPE_REPRESENTATION_RELATIONSHIP( ) );
#11213 = CARTESIAN_POINT ( 'NONE',  ( 211.7451286015360381, 116.5372661580811240, -68.08724388832010277 ) ) ;
#11214 = DIRECTION ( 'NONE',  ( 0.7071067811865474617, 9.058225723175622340E-16, -0.7071067811865474617 ) ) ;
#11215 = CARTESIAN_POINT ( 'NONE',  ( -74.19961951691011848, 20.67022044985851181, 5.043965628238842314 ) ) ;
#11216 = DIRECTION ( 'NONE',  ( 0.000000000000000000, -0.7071067811865475727, 0.7071067811865475727 ) ) ;
#11217 = LINE ( 'NONE', #32684, #6428 ) ;
#11218 = CARTESIAN_POINT ( 'NONE',  ( 198.5547391818673191, 98.28306391574493261, 94.71473285867655534 ) ) ;
#11219 = AXIS2_PLACEMENT_3D ( 'NONE', #57524, #29747, #30792 ) ;
#11220 = CARTESIAN_POINT ( 'NONE',  ( 150.4550062612852912, 52.39582885725846495, -40.91940173996584917 ) ) ;
#11221 = CARTESIAN_POINT ( 'NONE',  ( 163.2911130186310515, 63.63047778106597718, -65.73252438383109109 ) ) ;
#11222 = VERTEX_POINT ( 'NONE', #51555 ) ;
#11223 = PLANE ( 'NONE',  #17333 ) ;
#11224 = DIRECTION ( 'NONE',  ( -0.000000000000000000, 1.000000000000000000, -0.000000000000000000 ) ) ;
#11225 = EDGE_LOOP ( 'NONE', ( #35621, #9387, #63231, #16757 ) ) ;
#11226 = ORIENTED_EDGE ( 'NONE', *, *, #50364, .T. ) ;
#11227 = CARTESIAN_POINT ( 'NONE',  ( -85.75222301046102302, 25.14826148333820299, 40.42695221713501041 ) ) ;
#11228 = CARTESIAN_POINT ( 'NONE',  ( 157.2533363798598600, 58.75760182111574181, -77.96873488960133614 ) ) ;
#11229 = CARTESIAN_POINT ( 'NONE',  ( 442.3372781065085633, 395.0000000000001137, -141.4497041420118251 ) ) ;
#11230 = CARTESIAN_POINT ( 'NONE',  ( -23.98903001682803193, 8.486614814224621384, 63.56679523331560944 ) ) ;
#11231 = CARTESIAN_POINT ( 'NONE',  ( -146.5268141329886760, 61.69196909035593990, 18.26230962334813768 ) ) ;
#11232 = ORIENTED_EDGE ( 'NONE', *, *, #23537, .F. ) ;
#11233 = ORIENTED_EDGE ( 'NONE', *, *, #56157, .F. ) ;
#11234 = VECTOR ( 'NONE', #23749, 1000.000000000000000 ) ;
#11235 = CARTESIAN_POINT ( 'NONE',  ( 0.000000000000000000, 0.000000000000000000, -9.500000000000000000 ) ) ;
#11236 = PRODUCT_RELATED_PRODUCT_CATEGORY ( 'part', '', ( #51893 ) ) ;
#11237 = EDGE_LOOP ( 'NONE', ( #63243, #586 ) ) ;
#11238 = CARTESIAN_POINT ( 'NONE',  ( 37.70910994512001224, 9.209110272746709569, -23.58583660981673802 ) ) ;
#11239 = CARTESIAN_POINT ( 'NONE',  ( -148.0058283997321666, 64.22864592525515093, 30.86948728267493181 ) ) ;
#11240 = CARTESIAN_POINT ( 'NONE',  ( 58.09436971064710775, 11.58462396079456802, 69.83830878865299496 ) ) ;
#11241 = CARTESIAN_POINT ( 'NONE',  ( -7.825402957745081878, 7.899365992529270741, 56.96013162991089018 ) ) ;
#11242 = EDGE_CURVE ( 'NONE', #52636, #58090, #2668, .T. ) ;
#11243 = CARTESIAN_POINT ( 'NONE',  ( -28.53072891721389581, 10.14951062022288042, -89.57987656953713440 ) ) ;
#11244 = FACE_BOUND ( 'NONE', #14499, .T. ) ;
#11245 = EDGE_CURVE ( 'NONE', #55744, #30631, #39607, .T. ) ;
#11246 = DIRECTION ( 'NONE',  ( 0.000000000000000000, 1.000000000000000000, 0.000000000000000000 ) ) ;
#11247 = ORIENTED_EDGE ( 'NONE', *, *, #39470, .T. ) ;
#11248 = VERTEX_POINT ( 'NONE', #3361 ) ;
#11249 = CARTESIAN_POINT ( 'NONE',  ( -3.660532965668827021, 7.124194613927616437, 6.003346013664852075E-15 ) ) ;
#11250 = DIRECTION ( 'NONE',  ( 1.000000000000000000, 0.000000000000000000, -0.000000000000000000 ) ) ;
#11251 = DIRECTION ( 'NONE',  ( -0.000000000000000000, 1.000000000000000000, -0.000000000000000000 ) ) ;
#11252 = DIRECTION ( 'NONE',  ( 0.3090169943749582759, -0.9510565162951500895, 0.000000000000000000 ) ) ;
#11253 = CARTESIAN_POINT ( 'NONE',  ( 65.62848231372478836, 13.29388722724788074, 30.27865613481686680 ) ) ;
#11254 = AXIS2_PLACEMENT_3D ( 'NONE', #49886, #1710, #66096 ) ;
#11255 = EDGE_LOOP ( 'NONE', ( #61520, #57948, #35538, #31993 ) ) ;
#11256 = EDGE_CURVE ( 'NONE', #35316, #30444, #62095, .T. ) ;
#11257 = CARTESIAN_POINT ( 'NONE',  ( 81.57482918025355900, 17.75786713398421668, 15.91392937073483260 ) ) ;
#11258 = EDGE_LOOP ( 'NONE', ( #59654, #69321, #293, #21113 ) ) ;
#11259 = CARTESIAN_POINT ( 'NONE',  ( 18.89356949897823768, 62.19351277735707839, 73.58025477438755502 ) ) ;
#11260 = EDGE_LOOP ( 'NONE', ( #56105, #28464, #10356, #52863 ) ) ;
#11261 = EDGE_CURVE ( 'NONE', #3613, #52201, #17162, .T. ) ;
#11262 = EDGE_CURVE ( 'NONE', #28403, #58183, #46959, .T. ) ;
#11263 = ORIENTED_EDGE ( 'NONE', *, *, #41915, .F. ) ;
#11264 = DIRECTION ( 'NONE',  ( 1.387778780781445922E-16, -1.000000000000000000, -1.232595164407830946E-32 ) ) ;
#11265 = VECTOR ( 'NONE', #67403, 1000.000000000000000 ) ;
#11266 = CARTESIAN_POINT ( 'NONE',  ( 93.85846834761623825, 22.01563781856521373, 8.354306518833805484 ) ) ;
#11267 = DIRECTION ( 'NONE',  ( 0.000000000000000000, 0.000000000000000000, 1.000000000000000000 ) ) ;
#11268 = VERTEX_POINT ( 'NONE', #35725 ) ;
#11269 = DIRECTION ( 'NONE',  ( 0.000000000000000000, 0.000000000000000000, 1.000000000000000000 ) ) ;
#11270 = CARTESIAN_POINT ( 'NONE',  ( -442.9409111889697215, 394.9999999999998863, 99.62207883810852138 ) ) ;
#11271 = CARTESIAN_POINT ( 'NONE',  ( 150.4544126017351289, 52.39556706174410294, 34.24499968066869826 ) ) ;
#11272 = CARTESIAN_POINT ( 'NONE',  ( -180.4614954900548582, 97.28277348252828460, -43.78069842929563293 ) ) ;
#11273 = LINE ( 'NONE', #31369, #39250 ) ;
#11274 = CARTESIAN_POINT ( 'NONE',  ( -34.29440389294403246, 17.09499999999999886, 4.000000000000000000 ) ) ;
#11275 = CARTESIAN_POINT ( 'NONE',  ( -439.4229916354183274, 388.0000000000064233, 96.05029585798874336 ) ) ;
#11276 = ORIENTED_EDGE ( 'NONE', *, *, #30052, .F. ) ;
#11277 = CARTESIAN_POINT ( 'NONE',  ( 133.8566784816069060, 42.60093787723654657, -62.86786152285933582 ) ) ;
#11278 = DIRECTION ( 'NONE',  ( 0.000000000000000000, 0.000000000000000000, 1.000000000000000000 ) ) ;
#11279 = ORIENTED_EDGE ( 'NONE', *, *, #23203, .T. ) ;
#11280 = FACE_BOUND ( 'NONE', #24325, .T. ) ;
#11281 = CARTESIAN_POINT ( 'NONE',  ( -3.244108878396728901, 6.635632329121488482, -63.80409075740015368 ) ) ;
#11282 = FACE_OUTER_BOUND ( 'NONE', #5199, .T. ) ;
#11283 = CARTESIAN_POINT ( 'NONE',  ( -122.8202784017355214, 45.69728649588466141, -35.56839789957883369 ) ) ;
#11284 = CARTESIAN_POINT ( 'NONE',  ( -86.10360257264198935, 26.38663017581290759, 12.07582342592019309 ) ) ;
#11285 = DIRECTION ( 'NONE',  ( -1.000000000000000000, 0.000000000000000000, 0.000000000000000000 ) ) ;
#11286 = EDGE_CURVE ( 'NONE', #2336, #16002, #3726, .T. ) ;
#11287 = CARTESIAN_POINT ( 'NONE',  ( 111.6210066600218198, 21.48343462569976836, 4.741142292097735300 ) ) ;
#11288 = CARTESIAN_POINT ( 'NONE',  ( 0.000000000000000000, 0.000000000000000000, 41.38025477438755928 ) ) ;
#11289 = CARTESIAN_POINT ( 'NONE',  ( 0.000000000000000000, 0.000000000000000000, 40.00000000000003553 ) ) ;
#11290 = CARTESIAN_POINT ( 'NONE',  ( 112.1164716692773595, 29.75790342121401366, 17.54430536651847206 ) ) ;
#11291 = CARTESIAN_POINT ( 'NONE',  ( 91.50468583833760761, 22.21368636549395603, -22.19755133611119291 ) ) ;
#11292 = EDGE_LOOP ( 'NONE', ( #36058, #8717, #26015, #4098 ) ) ;
#11293 = CARTESIAN_POINT ( 'NONE',  ( -31.43908319763711390, 10.61114334766715928, 18.37190381572551701 ) ) ;
#11294 = ORIENTED_EDGE ( 'NONE', *, *, #5550, .F. ) ;
#11295 = CARTESIAN_POINT ( 'NONE',  ( 44.01696072966019102, -47.84694004974149095, 3.061616997868437868E-16 ) ) ;
#11296 = CARTESIAN_POINT ( 'NONE',  ( 84.74089592029042706, 19.84571403269345424, -77.42846521137805382 ) ) ;
#11297 = CARTESIAN_POINT ( 'NONE',  ( 39.40195752203892710, 8.409560354027400209, 56.75838489642694640 ) ) ;
#11298 = CARTESIAN_POINT ( 'NONE',  ( 31.11269837220806522, 4.999999999999936939, 2.000000000000001776 ) ) ;
#11299 = CARTESIAN_POINT ( 'NONE',  ( -36.11269837220806522, 5.594483210025202879E-14, 85.00100000000000477 ) ) ;
#11300 = VECTOR ( 'NONE', #3043, 1000.000000000000000 ) ;
#11301 = CARTESIAN_POINT ( 'NONE',  ( -29.50439180771546432, 10.29976981300626804, -50.07971974204068744 ) ) ;
#11302 = PRODUCT_DEFINITION_SHAPE ( 'NONE', 'NONE',  #69610 ) ;
#11303 = CARTESIAN_POINT ( 'NONE',  ( 5.799999999999999822, 0.000000000000000000, 0.000000000000000000 ) ) ;
#11304 = CIRCLE ( 'NONE', #50635, 65.36598343705435354 ) ;
#11305 = CARTESIAN_POINT ( 'NONE',  ( 0.000000000000000000, 0.000000000000000000, -50.00000000000000711 ) ) ;
#11306 = DIRECTION ( 'NONE',  ( 1.000000000000000000, 0.000000000000000000, 0.000000000000000000 ) ) ;
#11307 = ORIENTED_EDGE ( 'NONE', *, *, #47001, .T. ) ;
#11308 = ORIENTED_EDGE ( 'NONE', *, *, #63943, .F. ) ;
#11309 = CARTESIAN_POINT ( 'NONE',  ( 33.93974911725171495, 8.773765372885565128, 59.11309198735373371 ) ) ;
#11310 = VECTOR ( 'NONE', #906, 1000.000000000000000 ) ;
#11311 = CARTESIAN_POINT ( 'NONE',  ( -59.49248125703533674, -30.03746431348988111, 34.48241823988799837 ) ) ;
#11312 = CARTESIAN_POINT ( 'NONE',  ( -168.7314919967217861, 83.83749564070829763, -9.267934599853210997 ) ) ;
#11313 = PRODUCT_DEFINITION_CONTEXT ( 'detailed design', #58366, 'design' ) ;
#11314 = CIRCLE ( 'NONE', #55152, 4.999999999999997335 ) ;
#11315 = CARTESIAN_POINT ( 'NONE',  ( 65.79663946071997316, 14.37086544438438196, -89.94145055465119754 ) ) ;
#11316 = ORIENTED_EDGE ( 'NONE', *, *, #46935, .T. ) ;
#11317 = EDGE_CURVE ( 'NONE', #53112, #14479, #18751, .T. ) ;
#11318 = CARTESIAN_POINT ( 'NONE',  ( 282.5093869099858921, 21.56904524376771093, 4.337160898883471560 ) ) ;
#11319 = ADVANCED_FACE ( 'NONE', ( #44084 ), #38475, .F. ) ;
#11320 = CARTESIAN_POINT ( 'NONE',  ( 186.5979919519637349, 85.84756789133378163, -11.79079488912463880 ) ) ;
#11321 = CARTESIAN_POINT ( 'NONE',  ( 207.8398359204633721, 112.5208221429021478, 3.049908702302650099 ) ) ;
#11322 = CARTESIAN_POINT ( 'NONE',  ( -15.55634918610405748, -15.55634918610400774, 2.000000000000001776 ) ) ;
#11323 = CARTESIAN_POINT ( 'NONE',  ( 40.37438610703018327, 8.537526699166107846, -23.72814077592008175 ) ) ;
#11324 = CARTESIAN_POINT ( 'NONE',  ( 45.78444578631987127, 59.41672343742573759, 170.0000000000000000 ) ) ;
#11325 = LINE ( 'NONE', #58148, #47506 ) ;
#11326 = CARTESIAN_POINT ( 'NONE',  ( -45.81425895439360829, -46.10914959592906825, 170.0000000000000000 ) ) ;
#11327 = EDGE_CURVE ( 'NONE', #31093, #11589, #48655, .T. ) ;
#11328 = ADVANCED_FACE ( 'NONE', ( #494 ), #64865, .F. ) ;
#11329 = ORIENTED_EDGE ( 'NONE', *, *, #32716, .T. ) ;
#11330 = LINE ( 'NONE', #43340, #958 ) ;
#11331 = CARTESIAN_POINT ( 'NONE',  ( -37.98601804829808515, 14.28438006995824772, -11.98601804829809581 ) ) ;
#11332 = EDGE_CURVE ( 'NONE', #16701, #21755, #63840, .T. ) ;
#11333 = CARTESIAN_POINT ( 'NONE',  ( -51.77431913897920879, 14.86466849149171132, 71.42491583832892843 ) ) ;
#11334 = LINE ( 'NONE', #54234, #9663 ) ;
#11335 = DIRECTION ( 'NONE',  ( -0.000000000000000000, -0.000000000000000000, -1.000000000000000000 ) ) ;
#11336 = LINE ( 'NONE', #54236, #62534 ) ;
#11337 = VERTEX_POINT ( 'NONE', #43395 ) ;
#11338 = DIRECTION ( 'NONE',  ( -0.000000000000000000, -0.000000000000000000, -1.000000000000000000 ) ) ;
#11339 = CARTESIAN_POINT ( 'NONE',  ( 6.400000000000000355, 9.237604307034018802, 0.000000000000000000 ) ) ;
#11340 = ORIENTED_EDGE ( 'NONE', *, *, #51826, .T. ) ;
#11341 = ORIENTED_EDGE ( 'NONE', *, *, #28573, .T. ) ;
#11342 = DIRECTION ( 'NONE',  ( -0.8090169943749506709, 0.5877852522924686962, 0.000000000000000000 ) ) ;
#11343 = DIRECTION ( 'NONE',  ( -1.000000000000000000, -1.001918829714556097E-14, 9.899279560275163638E-15 ) ) ;
#11344 = CARTESIAN_POINT ( 'NONE',  ( 102.7425154123292543, 25.56407025871218863, 36.86950736794638317 ) ) ;
#11345 = ADVANCED_FACE ( 'NONE', ( #59224 ), #48305, .F. ) ;
#11346 = EDGE_LOOP ( 'NONE', ( #40918, #19517, #66865, #43879 ) ) ;
#11347 = EDGE_CURVE ( 'NONE', #50582, #10403, #7975, .T. ) ;
#11348 = CARTESIAN_POINT ( 'NONE',  ( -61.75956139478098805, 16.58288496614414598, -72.92701606488500943 ) ) ;
#11349 = AXIS2_PLACEMENT_3D ( 'NONE', #23558, #44995, #66478 ) ;
#11350 = CARTESIAN_POINT ( 'NONE',  ( 39.40195752203892710, 8.409560354027398432, -23.77526687496409608 ) ) ;
#11351 = FACE_OUTER_BOUND ( 'NONE', #54085, .T. ) ;
#11352 = CARTESIAN_POINT ( 'NONE',  ( -157.0069571479807280, 72.18154199622283329, -69.45793912688546357 ) ) ;
#11353 = LINE ( 'NONE', #47013, #68761 ) ;
#11354 = DIRECTION ( 'NONE',  ( 1.000000000000000000, 0.000000000000000000, 0.000000000000000000 ) ) ;
#11355 = VECTOR ( 'NONE', #55299, 1000.000000000000000 ) ;
#11356 = AXIS2_PLACEMENT_3D ( 'NONE', #58095, #9916, #57404 ) ;
#11357 = CARTESIAN_POINT ( 'NONE',  ( -48.58279704072702998, 14.07632445131079635, -38.91481426334084404 ) ) ;
#11358 = DIRECTION ( 'NONE',  ( 0.000000000000000000, 0.000000000000000000, 1.000000000000000000 ) ) ;
#11359 = CARTESIAN_POINT ( 'NONE',  ( 13.84704553156522522, 7.452804552247573433, 30.26612764413199486 ) ) ;
#11360 = DIRECTION ( 'NONE',  ( 0.000000000000000000, -1.000000000000000000, 0.000000000000000000 ) ) ;
#11361 = PLANE ( 'NONE',  #55610 ) ;
#11363 = EDGE_LOOP ( 'NONE', ( #13795, #2521, #45036, #49200 ) ) ;
#11362 = CARTESIAN_POINT ( 'NONE',  ( 15.55634918610409656, 31.11269837220803325, 85.00100000000000477 ) ) ;
#11364 = VERTEX_POINT ( 'NONE', #7531 ) ;
#11365 = AXIS2_PLACEMENT_3D ( 'NONE', #47209, #14859, #20478 ) ;
#11366 = ORIENTED_EDGE ( 'NONE', *, *, #43567, .T. ) ;
#11367 = CARTESIAN_POINT ( 'NONE',  ( -15.13254930056756109, 7.477527548005403979, -14.36566954603158131 ) ) ;
#11368 = CARTESIAN_POINT ( 'NONE',  ( -52.66507163626135224, 14.05394608175174476, 44.94350458795448588 ) ) ;
#11369 = DIRECTION ( 'NONE',  ( 0.000000000000000000, -1.000000000000000000, -1.110223024625156171E-16 ) ) ;
#11370 = CARTESIAN_POINT ( 'NONE',  ( -12.99999999999999822, 10.00000000000000000, -17.00000000000000355 ) ) ;
#11371 = CARTESIAN_POINT ( 'NONE',  ( -61.10880364359507411, 17.43879918625639647, -47.14754783338620570 ) ) ;
#11372 = CARTESIAN_POINT ( 'NONE',  ( -15.27733754929849574, 8.502213909106947298, -15.09477148241088784 ) ) ;
#11373 = DIRECTION ( 'NONE',  ( -0.000000000000000000, -0.000000000000000000, -1.000000000000000000 ) ) ;
#11374 = CARTESIAN_POINT ( 'NONE',  ( 22.18075376363910323, 11.79626863379964696, 0.000000000000000000 ) ) ;
#11375 = EDGE_LOOP ( 'NONE', ( #16067, #20445, #32376, #28073 ) ) ;
#11376 = CARTESIAN_POINT ( 'NONE',  ( -23.73638277007033182, -7.847555861075553807, 0.000000000000000000 ) ) ;
#11377 = ORIENTED_EDGE ( 'NONE', *, *, #26096, .T. ) ;
#11378 = ORIENTED_EDGE ( 'NONE', *, *, #58832, .T. ) ;
#11379 = LINE ( 'NONE', #60283, #27564 ) ;
#11380 = CARTESIAN_POINT ( 'NONE',  ( 0.3167204509598451900, -8.479269695850872424, 1.313474075707216748 ) ) ;
#11381 = CARTESIAN_POINT ( 'NONE',  ( -24.85653282846401879, 9.618702155736652770, 94.99999999999866418 ) ) ;
#11382 = CARTESIAN_POINT ( 'NONE',  ( 115.7731501832036116, 32.64791439093735903, -21.66803278067574468 ) ) ;
#11383 = CARTESIAN_POINT ( 'NONE',  ( -102.2801239173131194, 32.78103895658057354, 18.67452391595144334 ) ) ;
#11384 = CARTESIAN_POINT ( 'NONE',  ( 19.54475376904848716, 6.649964688461122542, 44.01079968644612705 ) ) ;
#11385 = CARTESIAN_POINT ( 'NONE',  ( 137.4031600461560743, 44.79620770172221000, -23.29145164325822392 ) ) ;
#11386 = ORIENTED_EDGE ( 'NONE', *, *, #7295, .F. ) ;
#11387 = EDGE_LOOP ( 'NONE', ( #29145, #59839 ) ) ;
#11388 = ORIENTED_EDGE ( 'NONE', *, *, #22251, .T. ) ;
#11389 = CARTESIAN_POINT ( 'NONE',  ( 0.000000000000000000, 6.000000000000000000, -3.000000000000030198 ) ) ;
#11390 = CARTESIAN_POINT ( 'NONE',  ( 49.99999999999998579, -19.99999999999996447, 2.000000000000015543 ) ) ;
#11391 = CARTESIAN_POINT ( 'NONE',  ( 0.000000000000000000, 0.000000000000000000, 0.000000000000000000 ) ) ;
#11392 = CARTESIAN_POINT ( 'NONE',  ( -33.13098007862451055, 9.875138601866709109, 71.87171333366060821 ) ) ;
#11393 = CARTESIAN_POINT ( 'NONE',  ( -154.0718453320783112, 68.14976693162388699, -21.42403036335299049 ) ) ;
#11394 = ORIENTED_EDGE ( 'NONE', *, *, #59630, .F. ) ;
#11395 = CARTESIAN_POINT ( 'NONE',  ( 188.5838389098762775, 88.03667982118678026, 63.96234997918834608 ) ) ;
#11396 = CARTESIAN_POINT ( 'NONE',  ( -155.7495771807047049, 69.65980221699317099, 60.87747373296404163 ) ) ;
#11397 = AXIS2_PLACEMENT_3D ( 'NONE', #37835, #5128, #64569 ) ;
#11398 = CYLINDRICAL_SURFACE ( 'NONE', #8164, 60.00000000000000000 ) ;
#11399 = CARTESIAN_POINT ( 'NONE',  ( 103.4696172145934980, 25.87254488218942683, 13.49709838995913280 ) ) ;
#11400 = CARTESIAN_POINT ( 'NONE',  ( 0.1285234777257801275, -24.99966963213046611, 0.000000000000000000 ) ) ;
#11401 = DIRECTION ( 'NONE',  ( -0.000000000000000000, -0.000000000000000000, -1.000000000000000000 ) ) ;
#11402 = DIRECTION ( 'NONE',  ( -0.000000000000000000, -0.000000000000000000, -1.000000000000000000 ) ) ;
#11403 = DIRECTION ( 'NONE',  ( -0.000000000000000000, -0.000000000000000000, -1.000000000000000000 ) ) ;
#11404 = CARTESIAN_POINT ( 'NONE',  ( 15.78827728214693060, 7.507518794609573831, 18.17015708224157322 ) ) ;
#11405 = EDGE_CURVE ( 'NONE', #49946, #69216, #29774, .T. ) ;
#11406 = AXIS2_PLACEMENT_3D ( 'NONE', #9156, #42198, #15469 ) ;
#11407 = AXIS2_PLACEMENT_3D ( 'NONE', #49219, #58735, #10556 ) ;
#11408 = ORIENTED_EDGE ( 'NONE', *, *, #24486, .F. ) ;
#11409 = DIRECTION ( 'NONE',  ( 0.000000000000000000, 1.000000000000000000, 0.000000000000000000 ) ) ;
#11410 = ADVANCED_FACE ( 'NONE', ( #52154 ), #57780, .T. ) ;
#11411 = CLOSED_SHELL ( 'NONE', ( #11814, #48594, #51527, #41201, #53636, #22060 ) ) ;
#11412 = CARTESIAN_POINT ( 'NONE',  ( -132.2352756077771687, 50.81350938245624604, -73.27096579721956005 ) ) ;
#11413 = CARTESIAN_POINT ( 'NONE',  ( -131.2803255164625114, 50.14412978403780841, -37.18907415913850656 ) ) ;
#11414 = CYLINDRICAL_SURFACE ( 'NONE', #54777, 65.36598343705435354 ) ;
#11415 = CARTESIAN_POINT ( 'NONE',  ( 59.08202327466403858, 12.82375733818951069, -63.67486918714139676 ) ) ;
#11416 = ORIENTED_EDGE ( 'NONE', *, *, #59692, .T. ) ;
#11417 = VERTEX_POINT ( 'NONE', #63753 ) ;
#11418 = CARTESIAN_POINT ( 'NONE',  ( -128.7359537904937099, 48.39323004177004606, -89.14970310811136756 ) ) ;
#11419 = CARTESIAN_POINT ( 'NONE',  ( 0.000000000000000000, 0.000000000000000000, 7.000000000000000000 ) ) ;
#11420 = EDGE_LOOP ( 'NONE', ( #22996, #29787, #1762, #26593 ) ) ;
#11421 = EDGE_LOOP ( 'NONE', ( #7711, #36469, #60361, #60525, #30083, #55207, #49804, #8486, #2813 ) ) ;
#11422 = CARTESIAN_POINT ( 'NONE',  ( 178.1999009735082211, 75.73911533785329198, -36.79823857645895657 ) ) ;
#11423 = CARTESIAN_POINT ( 'NONE',  ( -7.486743542469090684, -64.58150799671139453, 170.0000000000000000 ) ) ;
#11424 = ADVANCED_FACE ( 'NONE', ( #58125 ), #68002, .T. ) ;
#11425 = ORIENTED_EDGE ( 'NONE', *, *, #64872, .T. ) ;
#11426 = CARTESIAN_POINT ( 'NONE',  ( -17.50000000000000000, 207.5000000000000284, 1.999999999999998224 ) ) ;
#11427 = CARTESIAN_POINT ( 'NONE',  ( 135.6647932137617829, 43.70902528961478595, 71.14781748300585207 ) ) ;
#11428 = CARTESIAN_POINT ( 'NONE',  ( -71.26675986148643460, 19.63956187826083166, -41.36718459057324537 ) ) ;
#11429 = CARTESIAN_POINT ( 'NONE',  ( -189.8133172329396814, 108.7279284458360564, 94.99999999999866418 ) ) ;
#11430 = CARTESIAN_POINT ( 'NONE',  ( 90.91465859190773813, 20.92790537681857543, -49.48152920833616264 ) ) ;
#11431 = CARTESIAN_POINT ( 'NONE',  ( -189.7987719395349302, 107.8653664616570609, 41.30349450692464330 ) ) ;
#11432 = ORIENTED_EDGE ( 'NONE', *, *, #37152, .F. ) ;
#11433 = VERTEX_POINT ( 'NONE', #19803 ) ;
#11434 = CARTESIAN_POINT ( 'NONE',  ( 112.1012908502484748, 29.75117929736500599, -50.69241971753201170 ) ) ;
#11435 = FACE_BOUND ( 'NONE', #39026, .T. ) ;
#11436 = CARTESIAN_POINT ( 'NONE',  ( -149.0764453401867513, 65.13297611514538232, -49.81283053149199702 ) ) ;
#11437 = CARTESIAN_POINT ( 'NONE',  ( -65.99999999999998579, 29.79383981485516841, -1.674068137902818041E-14 ) ) ;
#11439 = VERTEX_POINT ( 'NONE', #9247 ) ;
#11438 = CARTESIAN_POINT ( 'NONE',  ( -144.3945994505580757, 59.96115386701889349, -47.80521614277407139 ) ) ;
#11440 = CARTESIAN_POINT ( 'NONE',  ( 55.51528220483960041, 12.08323518953685571, 10.70683319743981343 ) ) ;
#11441 = AXIS2_PLACEMENT_3D ( 'NONE', #66148, #1764, #17586 ) ;
#11442 = ORIENTED_EDGE ( 'NONE', *, *, #63589, .T. ) ;
#11443 = AXIS2_PLACEMENT_3D ( 'NONE', #36901, #58340, #11527 ) ;
#11444 = DIRECTION ( 'NONE',  ( -0.000000000000000000, 1.000000000000000000, -0.000000000000000000 ) ) ;
#11445 = CYLINDRICAL_SURFACE ( 'NONE', #7573, 5.000000000000004441 ) ;
#11446 = DIRECTION ( 'NONE',  ( 1.000000000000000000, 0.000000000000000000, -1.156482317317871232E-16 ) ) ;
#11447 = DIRECTION ( 'NONE',  ( 0.000000000000000000, 0.000000000000000000, -1.000000000000000000 ) ) ;
#11448 = VECTOR ( 'NONE', #21763, 1000.000000000000000 ) ;
#11449 =( GEOMETRIC_REPRESENTATION_CONTEXT ( 3 ) GLOBAL_UNCERTAINTY_ASSIGNED_CONTEXT ( ( #14872 ) ) GLOBAL_UNIT_ASSIGNED_CONTEXT ( ( #5288, #42902, #58396 ) ) REPRESENTATION_CONTEXT ( 'NONE', 'WORKASPACE' ) );
#11450 = DIRECTION ( 'NONE',  ( 0.000000000000000000, 0.000000000000000000, -1.000000000000000000 ) ) ;
#11451 = CARTESIAN_POINT ( 'NONE',  ( 88.52345267551655184, 20.07594890262053511, -77.42696361605551658 ) ) ;
#11452 = CARTESIAN_POINT ( 'NONE',  ( 197.8436586345019919, 97.39326576892285914, 6.765139324472087878 ) ) ;
#11453 = CARTESIAN_POINT ( 'NONE',  ( -98.67723517640905584, 30.98797878696539243, 17.75677604357209916 ) ) ;
#11454 = CARTESIAN_POINT ( 'NONE',  ( -48.00000000000000711, -20.00000000000000355, 4.000000000000000000 ) ) ;
#11455 = ORIENTED_EDGE ( 'NONE', *, *, #3580, .F. ) ;
#11456 = ORIENTED_EDGE ( 'NONE', *, *, #42622, .T. ) ;
#11457 = AXIS2_PLACEMENT_3D ( 'NONE', #64665, #48804, #6964 ) ;
#11458 = CARTESIAN_POINT ( 'NONE',  ( 44.86216938219163097, 9.182565662897481218, 32.26643658086751998 ) ) ;
#11459 = AXIS2_PLACEMENT_3D ( 'NONE', #28055, #65006, #65353 ) ;
#11460 = DIRECTION ( 'NONE',  ( -0.000000000000000000, -0.000000000000000000, 1.000000000000000000 ) ) ;
#11461 = DIRECTION ( 'NONE',  ( 0.000000000000000000, 0.000000000000000000, 1.000000000000000000 ) ) ;
#11462 = LINE ( 'NONE', #32589, #28432 ) ;
#11463 = CARTESIAN_POINT ( 'NONE',  ( 204.6977192012829789, 108.0580384837234789, -36.32593103262158252 ) ) ;
#11464 = EDGE_CURVE ( 'NONE', #17465, #51505, #59157, .T. ) ;
#11465 = CARTESIAN_POINT ( 'NONE',  ( -73.09214866197368110, 21.34321757515765228, -74.50211547328287054 ) ) ;
#11466 = CARTESIAN_POINT ( 'NONE',  ( 11.29825944729730303, 74.09495289493001735, 41.38025477438755928 ) ) ;
#11467 = CARTESIAN_POINT ( 'NONE',  ( 45.35621884287173344, 10.27694987765648449, -47.70637205503341960 ) ) ;
#11468 = PLANE ( 'NONE',  #56521 ) ;
#11469 = ORIENTED_EDGE ( 'NONE', *, *, #24848, .T. ) ;
#11470 = CARTESIAN_POINT ( 'NONE',  ( -30.00000000000000355, -27.00000000000000355, 0.000000000000000000 ) ) ;
#11471 = ORIENTED_EDGE ( 'NONE', *, *, #10875, .T. ) ;
#11472 = EDGE_CURVE ( 'NONE', #18508, #14330, #15533, .T. ) ;
#11473 = CARTESIAN_POINT ( 'NONE',  ( -7.825402957745087207, 6.891034867348159842, -35.41807073194381417 ) ) ;
#11474 = CARTESIAN_POINT ( 'NONE',  ( 76.57571471437145760, 6.000000000000000000, -30.00000000000000000 ) ) ;
#11475 = CARTESIAN_POINT ( 'NONE',  ( 91.12448333640236342, 22.07449368110501098, 58.03361031003960591 ) ) ;
#11476 = CARTESIAN_POINT ( 'NONE',  ( 154.0293889979056985, 55.02370422818215445, -23.46008922554802467 ) ) ;
#11477 = CARTESIAN_POINT ( 'NONE',  ( 36.30999198706538778, 9.040534725358941870, 17.40661586187119880 ) ) ;
#11478 = CARTESIAN_POINT ( 'NONE',  ( 39.40195752203892710, -170.0000000000000000, -62.46436805589144114 ) ) ;
#11479 = CARTESIAN_POINT ( 'NONE',  ( 113.9789034327318689, 31.76692991242614639, -90.59633938589010427 ) ) ;
#11480 = CARTESIAN_POINT ( 'NONE',  ( 212.0873499799464525, 117.0618137521297228, 91.69696597238002767 ) ) ;
#11481 = CARTESIAN_POINT ( 'NONE',  ( 45.74764628539747235, 59.37057832282332726, 41.38025477438755928 ) ) ;
#11482 = ORIENTED_EDGE ( 'NONE', *, *, #49312, .F. ) ;
#11483 = CARTESIAN_POINT ( 'NONE',  ( 59.29474530993688575, 12.86968658439548641, 70.67399659177640103 ) ) ;
#11484 = FACE_OUTER_BOUND ( 'NONE', #40433, .T. ) ;
#11485 = ADVANCED_FACE ( 'NONE', ( #15562 ), #4650, .T. ) ;
#11486 = DIRECTION ( 'NONE',  ( 1.000000000000000000, 0.000000000000000000, 0.000000000000000000 ) ) ;
#11487 = CARTESIAN_POINT ( 'NONE',  ( -0.5780275525703870709, 6.527356703336897326, 35.66970812953940140 ) ) ;
#11488 = LINE ( 'NONE', #249, #38980 ) ;
#11489 = EDGE_CURVE ( 'NONE', #36015, #6906, #35979, .T. ) ;
#11490 = ORIENTED_EDGE ( 'NONE', *, *, #64711, .F. ) ;
#11491 = CARTESIAN_POINT ( 'NONE',  ( 848.0071894358330837, 612.7234514542420811, 794.5748919860991464 ) ) ;
#11492 = ADVANCED_FACE ( 'NONE', ( #63054 ), #36325, .T. ) ;
#11493 = CARTESIAN_POINT ( 'NONE',  ( -3.000000000000002665, 0.000000000000000000, -24.69999999999999929 ) ) ;
#11494 = DIRECTION ( 'NONE',  ( 0.000000000000000000, 0.000000000000000000, 1.000000000000000000 ) ) ;
#11495 = LINE ( 'NONE', #38242, #10989 ) ;
#11496 = ITEM_DEFINED_TRANSFORMATION ( 'NONE', 'NONE', #28797,  #66832 ) ;
#11497 = CARTESIAN_POINT ( 'NONE',  ( -131.3096895243911035, 51.39228038925232056, -37.20263158582804408 ) ) ;
#11498 = ORIENTED_EDGE ( 'NONE', *, *, #40421, .F. ) ;
#11499 = CARTESIAN_POINT ( 'NONE',  ( 437.3372781065086201, 0.000000000000000000, -141.4497041420118251 ) ) ;
#11500 = AXIS2_PLACEMENT_3D ( 'NONE', #61577, #28157, #60528 ) ;
#11501 = CARTESIAN_POINT ( 'NONE',  ( 311.9975424824652350, 170.0000000000000284, 354.1673509436691347 ) ) ;
#11502 = CARTESIAN_POINT ( 'NONE',  ( 198.8732368717152212, 100.3103976497391017, -12.24965016599340473 ) ) ;
#11503 = VECTOR ( 'NONE', #57608, 1000.000000000000000 ) ;
#11504 = CARTESIAN_POINT ( 'NONE',  ( -3.253130881186334200, 7.643323950922368049, -75.72777455412368397 ) ) ;
#11505 = CARTESIAN_POINT ( 'NONE',  ( 183.2136430849848239, 6.000000000000000000, -14.43565316649556074 ) ) ;
#11506 = EDGE_CURVE ( 'NONE', #62757, #49352, #7842, .T. ) ;
#11507 = EDGE_LOOP ( 'NONE', ( #3646, #35535, #17041, #24530 ) ) ;
#11508 = CARTESIAN_POINT ( 'NONE',  ( -15.55634918610403439, 2.818925648462311528E-14, 0.000000000000000000 ) ) ;
#11509 = CARTESIAN_POINT ( 'NONE',  ( 79.52639011421921111, 18.17129627604989750, 12.82766093010378938 ) ) ;
#11510 = B_SPLINE_CURVE_WITH_KNOTS ( 'NONE', 3,
 ( #6208, #64610, #21690, #22743, #28362, #16421, #22389, #49809, #42793, #38567, #60015, #32263, #17455, #53695, #64261, #5515, #11834, #33311, #26970, #44178, #38933, #60381, #48400, #43141, #7956, #2678, #55436, #45235, #61072, #29075, #12899, #28722, #34358, #66715, #35039, #13920, #24144, #35384, #50862, #45585, #44547, #51218, #40309, #56842, #23792, #56482, #2339, #67066, #18861, #29411, #50519, #66028, #13243, #61754 ),
 .UNSPECIFIED., .F., .F.,
 ( 4, 2, 2, 2, 2, 2, 2, 2, 2, 2, 2, 2, 2, 2, 2, 2, 2, 2, 2, 2, 2, 2, 2, 2, 2, 2, 4 ),
 ( 0.000000000000000000, 0.001958949513879419679, 0.002938424270819129519, 0.003917899027758839359, 0.004897373784698549198, 0.005876848541638259038, 0.006856323298577968878, 0.007835798055517678717, 0.008815272812457388557, 0.009794747569397098397, 0.01175369708327649206, 0.01273317184021620536, 0.01371264659715591867, 0.01567159611103534703, 0.01763054562491477364, 0.01958949513879420026, 0.02056896989573392398, 0.02154844465267364770, 0.02252791940961337142, 0.02350739416655309513, 0.02546634368043251828, 0.02644581843737221771, 0.02742529319431191714, 0.02840476795125161658, 0.02938424270819131601, 0.03036371746513101544, 0.03134319222207071487 ),
 .UNSPECIFIED. ) ;
#11511 = CARTESIAN_POINT ( 'NONE',  ( -95.88693721180808893, 30.76307528361165922, 41.94858041200124177 ) ) ;
#11512 = ADVANCED_FACE ( 'NONE', ( #65483 ), #1112, .F. ) ;
#11513 = EDGE_CURVE ( 'NONE', #37653, #8034, #65133, .T. ) ;
#11514 = EDGE_CURVE ( 'NONE', #19832, #29554, #53517, .T. ) ;
#11515 = LINE ( 'NONE', #9198, #39329 ) ;
#11517 = VERTEX_POINT ( 'NONE', #59488 ) ;
#11516 = CARTESIAN_POINT ( 'NONE',  ( 117.3246714514015849, 33.42485879931865611, 7.745107550458741663 ) ) ;
#11518 = LINE ( 'NONE', #54072, #31710 ) ;
#11519 = EDGE_LOOP ( 'NONE', ( #42567, #36572 ) ) ;
#11520 = ORIENTED_EDGE ( 'NONE', *, *, #67129, .T. ) ;
#11521 = CARTESIAN_POINT ( 'NONE',  ( -71.26675986148644881, 19.63956187826082456, -14.52263400010955330 ) ) ;
#11522 = CARTESIAN_POINT ( 'NONE',  ( -35.00000000000000000, 225.0000000000000000, 2.000000000000000000 ) ) ;
#11524 = EDGE_LOOP ( 'NONE', ( #31151, #7487, #34608, #36208 ) ) ;
#11523 = DIRECTION ( 'NONE',  ( -0.000000000000000000, -0.000000000000000000, -1.000000000000000000 ) ) ;
#11525 = CARTESIAN_POINT ( 'NONE',  ( 161.7209903610254855, 61.03262545641850068, 43.10605864504380236 ) ) ;
#11526 = CARTESIAN_POINT ( 'NONE',  ( 412.3372781065085633, 219.4906275429376308, -146.4497041420117682 ) ) ;
#11527 = DIRECTION ( 'NONE',  ( -1.000000000000000000, 0.000000000000000000, 0.000000000000000000 ) ) ;
#11528 = ORIENTED_EDGE ( 'NONE', *, *, #63282, .F. ) ;
#11529 = CARTESIAN_POINT ( 'NONE',  ( 36.61292551086699376, -65.40035471292219427, 41.38025477438755928 ) ) ;
#11530 = CARTESIAN_POINT ( 'NONE',  ( 9.962235950564874543, 64.23203137738424573, 40.00000000000003553 ) ) ;
#11531 = CARTESIAN_POINT ( 'NONE',  ( 157.1110115425986749, 57.37186251315585395, -89.81328548006501933 ) ) ;
#11532 = CARTESIAN_POINT ( 'NONE',  ( 132.9557829392755082, 42.05591979570418459, 56.39519894757799534 ) ) ;
#11533 = ORIENTED_EDGE ( 'NONE', *, *, #57029, .T. ) ;
#11534 = ORIENTED_EDGE ( 'NONE', *, *, #8440, .T. ) ;
#11535 = ORIENTED_EDGE ( 'NONE', *, *, #18491, .F. ) ;
#11536 = AXIS2_PLACEMENT_3D ( 'NONE', #1455, #6728, #38388 ) ;
#11537 = PLANE ( 'NONE',  #37652 ) ;
#11538 = FACE_OUTER_BOUND ( 'NONE', #5389, .T. ) ;
#11539 = CARTESIAN_POINT ( 'NONE',  ( 63.01563776193091826, 12.67277567978500308, -23.87614024170608218 ) ) ;
#11540 = EDGE_CURVE ( 'NONE', #68125, #66740, #31266, .T. ) ;
#11541 = CARTESIAN_POINT ( 'NONE',  ( -95.39675579260823213, 29.41944805607581159, 94.70441663738500893 ) ) ;
#11542 = CARTESIAN_POINT ( 'NONE',  ( -149.5074843970971301, -170.0000000000000000, -96.00193171241933499 ) ) ;
#11543 = DIRECTION ( 'NONE',  ( -0.000000000000000000, -0.000000000000000000, -1.000000000000000000 ) ) ;
#11544 = CARTESIAN_POINT ( 'NONE',  ( -58.41593024021014458, 16.65492390105237774, 84.79537928362319121 ) ) ;
#11546 = FACE_OUTER_BOUND ( 'NONE', #63868, .T. ) ;
#11545 = VECTOR ( 'NONE', #55450, 1000.000000000000000 ) ;
#11547 = VERTEX_POINT ( 'NONE', #11298 ) ;
#11548 = EDGE_CURVE ( 'NONE', #5953, #28478, #3199, .T. ) ;
#11549 = CARTESIAN_POINT ( 'NONE',  ( -100.2045077988687467, 32.86236599426410976, -88.98416475062359154 ) ) ;
#11550 = EDGE_LOOP ( 'NONE', ( #12840, #44077, #49586, #1937 ) ) ;
#11551 = VECTOR ( 'NONE', #61003, 1000.000000000000000 ) ;
#11552 = PLANE ( 'NONE',  #54314 ) ;
#11553 = CARTESIAN_POINT ( 'NONE',  ( 208.6132326550594485, 111.8685719053116969, -64.25973477317864990 ) ) ;
#11554 = LINE ( 'NONE', #43215, #35467 ) ;
#11555 = CARTESIAN_POINT ( 'NONE',  ( -73.81689110552359523, 20.53332132481499173, 5.347267905733100513 ) ) ;
#11556 = CARTESIAN_POINT ( 'NONE',  ( 63.01563776193090405, 12.67277567978497643, 44.81296093922130552 ) ) ;
#11557 = CARTESIAN_POINT ( 'NONE',  ( 22.28556289340100349, 7.803548444155007147, 33.76024460579878905 ) ) ;
#11558 = VECTOR ( 'NONE', #11037, 1000.000000000000000 ) ;
#11559 = DIRECTION ( 'NONE',  ( 0.000000000000000000, 0.000000000000000000, 1.000000000000000000 ) ) ;
#11560 = DIRECTION ( 'NONE',  ( -0.000000000000000000, -0.000000000000000000, -1.000000000000000000 ) ) ;
#11561 = EDGE_LOOP ( 'NONE', ( #41589, #853 ) ) ;
#11562 = LINE ( 'NONE', #33039, #44295 ) ;
#11563 = CYLINDRICAL_SURFACE ( 'NONE', #66742, 25.00000000000000000 ) ;
#11564 = ORIENTED_EDGE ( 'NONE', *, *, #49135, .T. ) ;
#11565 = CARTESIAN_POINT ( 'NONE',  ( -447.6627218934918915, 390.0000000000064801, -141.4497041420121377 ) ) ;
#11566 = CARTESIAN_POINT ( 'NONE',  ( 23.81581464765709200, 7.603089679099848119, 0.000000000000000000 ) ) ;
#11567 = ORIENTED_EDGE ( 'NONE', *, *, #12315, .T. ) ;
#11568 = EDGE_CURVE ( 'NONE', #28173, #29753, #58795, .T. ) ;
#11569 = CARTESIAN_POINT ( 'NONE',  ( 0.000000000000000000, 0.000000000000000000, 85.00000000000000000 ) ) ;
#11570 = EDGE_CURVE ( 'NONE', #48842, #30587, #49206, .T. ) ;
#11571 = CARTESIAN_POINT ( 'NONE',  ( 156.3797504404255960, 58.07856685387022111, -77.89230977338574746 ) ) ;
#11572 = DIRECTION ( 'NONE',  ( 0.7071067811865474617, 9.058225723175622340E-16, -0.7071067811865474617 ) ) ;
#11573 = EDGE_CURVE ( 'NONE', #27181, #780, #48230, .T. ) ;
#11574 = CARTESIAN_POINT ( 'NONE',  ( 6.400000000000000355, 6.123233995736766282E-16, -5.000000000000000000 ) ) ;
#11575 = CARTESIAN_POINT ( 'NONE',  ( 128.4224537826253822, 38.23837035195746381, -11.48689105586654335 ) ) ;
#11576 = ADVANCED_FACE ( 'NONE', ( #44005 ), #60194, .T. ) ;
#11577 = ORIENTED_EDGE ( 'NONE', *, *, #45926, .T. ) ;
#11578 = VERTEX_POINT ( 'NONE', #55 ) ;
#11579 = CARTESIAN_POINT ( 'NONE',  ( 0.000000000000000000, 0.000000000000000000, -10.00000000000000000 ) ) ;
#11580 = VERTEX_POINT ( 'NONE', #21515 ) ;
#11581 = DIRECTION ( 'NONE',  ( -0.000000000000000000, 1.000000000000000000, -0.000000000000000000 ) ) ;
#11582 = CARTESIAN_POINT ( 'NONE',  ( 4.993259224064100499E-16, 0.3912769055735416113, -8.000000000000000000 ) ) ;
#11583 = CARTESIAN_POINT ( 'NONE',  ( 63.01563776193090405, 12.67277567978497643, 71.65751152968501003 ) ) ;
#11584 = CARTESIAN_POINT ( 'NONE',  ( -0.7076388175553633975, 7.538734751903870546, 62.04576903499332019 ) ) ;
#11585 = DIRECTION ( 'NONE',  ( 1.020422603260505347E-14, -1.000000000000000000, -5.551115123125782702E-17 ) ) ;
#11586 = ORIENTED_EDGE ( 'NONE', *, *, #14158, .T. ) ;
#11587 = STYLED_ITEM ( 'NONE', ( #43412 ), #41290 ) ;
#11588 = CARTESIAN_POINT ( 'NONE',  ( 8.000000000000000000, 3.871967595402137530, -0.4989386132324603595 ) ) ;
#11589 = VERTEX_POINT ( 'NONE', #66891 ) ;
#11590 = ORIENTED_EDGE ( 'NONE', *, *, #19522, .T. ) ;
#11591 = PLANE ( 'NONE',  #23310 ) ;
#11592 = CARTESIAN_POINT ( 'NONE',  ( -2.699999999999990408, 0.000000000000000000, 0.000000000000000000 ) ) ;
#11593 = CARTESIAN_POINT ( 'NONE',  ( -173.1211646369891071, 87.12891641440859303, -7.867406574286297527 ) ) ;
#11594 = DIRECTION ( 'NONE',  ( 1.000000000000000000, 0.000000000000000000, 0.000000000000000000 ) ) ;
#11595 = DIRECTION ( 'NONE',  ( -0.000000000000000000, 0.000000000000000000, -1.000000000000000000 ) ) ;
#11596 = EDGE_CURVE ( 'NONE', #29753, #66023, #24319, .T. ) ;
#11597 = EDGE_CURVE ( 'NONE', #15908, #55797, #27880, .T. ) ;
#11598 = CONICAL_SURFACE ( 'NONE', #53169, 63.58578643762691485, 0.7853981633974497223 ) ;
#11599 = ORIENTED_EDGE ( 'NONE', *, *, #4036, .F. ) ;
#11600 = EDGE_CURVE ( 'NONE', #42836, #44487, #30511, .T. ) ;
#11601 = AXIS2_PLACEMENT_3D ( 'NONE', #57347, #20390, #20743 ) ;
#11602 = CARTESIAN_POINT ( 'NONE',  ( 82.13067365723604496, 17.93447087949265750, 4.346969704001187651 ) ) ;
#11603 = FACE_OUTER_BOUND ( 'NONE', #46869, .T. ) ;
#11604 = AXIS2_PLACEMENT_3D ( 'NONE', #1655, #7287, #59681 ) ;
#11605 = CARTESIAN_POINT ( 'NONE',  ( -71.22878586122430988, 19.62649588091170472, 38.91628792690696059 ) ) ;
#11606 = ORIENTED_EDGE ( 'NONE', *, *, #45679, .T. ) ;
#11607 = FACE_OUTER_BOUND ( 'NONE', #27750, .T. ) ;
#11608 = CIRCLE ( 'NONE', #68900, 74.99999999999998579 ) ;
#11609 = CIRCLE ( 'NONE', #65516, 5.000000000000060396 ) ;
#11610 = VERTEX_POINT ( 'NONE', #18686 ) ;
#11611 = CARTESIAN_POINT ( 'NONE',  ( 7.345652830558766055, -4.996589667937388235, -0.4964154566688021020 ) ) ;
#11612 = CARTESIAN_POINT ( 'NONE',  ( 10.55634918610397577, -26.11269837220809364, 85.00100000000000477 ) ) ;
#11613 = FACE_OUTER_BOUND ( 'NONE', #444, .T. ) ;
#11614 = EDGE_LOOP ( 'NONE', ( #60041, #48564, #58806, #22707 ) ) ;
#11615 = B_SPLINE_CURVE_WITH_KNOTS ( 'NONE', 3,
 ( #29175, #50620, #51670, #46377, #30557, #14389, #62573, #57293, #67177, #52009, #24938, #45698, #45344, #3824, #56592, #40073, #24603, #3476, #40761, #18964, #61859, #35841, #51330, #13008, #67856, #66825, #25294, #35140, #3145, #46729, #40412, #68199, #24257, #8414, #2438, #13684, #34466, #20008, #61180, #29867, #34807, #19650, #55908, #18618, #46036, #56245 ),
 .UNSPECIFIED., .F., .F.,
 ( 4, 2, 2, 2, 2, 2, 2, 2, 2, 2, 2, 2, 2, 2, 2, 2, 2, 2, 2, 2, 2, 2, 4 ),
 ( 0.02584318557310390577, 0.02743529570732764628, 0.02823135077443950786, 0.02902740584155136944, 0.03061951597577508913, 0.03221162610999880882, 0.03380373624422253198, 0.03459979131133437275, 0.03539584637844622045, 0.03619190144555806121, 0.03698795651266990892, 0.03858006664689361820, 0.03937612171400548672, 0.04017217678111735524, 0.04096823184822921682, 0.04176428691534107840, 0.04335639704956481544, 0.04494850718378853860, 0.04654061731801227564, 0.04813272745223600574, 0.04892878251934786732, 0.04972483758645972890, 0.05131694772068347288 ),
 .UNSPECIFIED. ) ;
#11616 = CARTESIAN_POINT ( 'NONE',  ( 0.000000000000000000, -6.928203230275509661, -3.999999999999999112 ) ) ;
#11617 = DIRECTION ( 'NONE',  ( 0.000000000000000000, 0.000000000000000000, 1.000000000000000000 ) ) ;
#11618 = LINE ( 'NONE', #55582, #66913 ) ;
#11619 = FACE_OUTER_BOUND ( 'NONE', #21673, .T. ) ;
#11620 = CARTESIAN_POINT ( 'NONE',  ( -130.2196570250629293, 49.40815211106347959, -21.71403809251050632 ) ) ;
#11621 = B_SPLINE_CURVE_WITH_KNOTS ( 'NONE', 3,
 ( #52545, #26163, #63802, #69415, #54249, #39489, #38446, #7496, #65535, #815, #7130, #55665, #54609, #49327, #28947, #65896, #6071, #28591, #27533, #66590, #12413, #1157, #12761, #18379, #17693, #28226, #22609, #60596, #49676, #12063, #44054, #22967, #23326, #1505, #33535, #39155, #22267, #48975, #17328, #43701, #54961, #60942, #33175, #38803 ),
 .UNSPECIFIED., .F., .F.,
 ( 4, 2, 2, 2, 2, 2, 2, 2, 2, 2, 2, 2, 2, 2, 2, 2, 2, 2, 2, 2, 2, 4 ),
 ( 0.000000000000000000, 0.003360573201437855057, 0.004200716501797282718, 0.005040859802156710812, 0.006721146402875505417, 0.007561289703234871061, 0.008401433003594235838, 0.009241576303953601482, 0.01008171960431296713, 0.01176200620503169321, 0.01260214950539103804, 0.01344229280575038113, 0.01428243610610972943, 0.01512257940646907425, 0.01680286600718778819, 0.01764300930754715210, 0.01848315260790651948, 0.02016343920862523342, 0.02184372580934394389, 0.02352401241006265437, 0.02520429901078136831, 0.02688458561150008225 ),
 .UNSPECIFIED. ) ;
#11622 = DIRECTION ( 'NONE',  ( -0.000000000000000000, -0.000000000000000000, -1.000000000000000000 ) ) ;
#11623 = APPLICATION_CONTEXT ( 'automotive_design' ) ;
#11624 = FACE_OUTER_BOUND ( 'NONE', #49379, .T. ) ;
#11625 = ORIENTED_EDGE ( 'NONE', *, *, #6427, .F. ) ;
#11626 = DIRECTION ( 'NONE',  ( -9.109522253334603153E-16, -1.000000000000000000, -9.109522253334599209E-16 ) ) ;
#11627 = CARTESIAN_POINT ( 'NONE',  ( -190.6985136298601731, 109.1272424661242582, -95.00000000000133582 ) ) ;
#11628 = ORIENTED_EDGE ( 'NONE', *, *, #69087, .T. ) ;
#11629 = FACE_BOUND ( 'NONE', #32798, .T. ) ;
#11630 = CARTESIAN_POINT ( 'NONE',  ( -0.3258398948454878097, 6.518608385615803691, -70.26394939446382182 ) ) ;
#11631 = CARTESIAN_POINT ( 'NONE',  ( -180.0094637318086939, 96.72611451757710199, 62.18543092603484723 ) ) ;
#11632 = CARTESIAN_POINT ( 'NONE',  ( 115.2709090239982714, 31.27821204311961267, -91.53183796548907480 ) ) ;
#11633 = DIRECTION ( 'NONE',  ( 0.000000000000000000, 0.000000000000000000, 1.000000000000000000 ) ) ;
#11634 = CARTESIAN_POINT ( 'NONE',  ( -84.23336401058614342, 25.60798568215574278, 16.12318571503568165 ) ) ;
#11635 = CARTESIAN_POINT ( 'NONE',  ( -55.15976438495108169, -34.41253982194112382, 43.58025477438756923 ) ) ;
#11636 = CARTESIAN_POINT ( 'NONE',  ( 112.2165994398967399, 21.53656025449836164, -4.493648593974088890 ) ) ;
#11637 = CARTESIAN_POINT ( 'NONE',  ( -74.26325512636837800, 20.69286162067376367, -90.21751194609112190 ) ) ;
#11638 = DIRECTION ( 'NONE',  ( 0.000000000000000000, 0.000000000000000000, 1.000000000000000000 ) ) ;
#11639 = CARTESIAN_POINT ( 'NONE',  ( 158.3604774538084712, 58.34594647925808886, 17.52526914281743231 ) ) ;
#11640 = CARTESIAN_POINT ( 'NONE',  ( 94.11733320392093560, 23.18939451097131865, -16.97069168030737174 ) ) ;
#11641 = VERTEX_POINT ( 'NONE', #39108 ) ;
#11642 = EDGE_CURVE ( 'NONE', #68503, #49852, #2507, .T. ) ;
#11643 = VECTOR ( 'NONE', #49675, 1000.000000000000000 ) ;
#11644 = CARTESIAN_POINT ( 'NONE',  ( -31.43908319763709969, 10.61114334766715572, 3.371903815725488585 ) ) ;
#11645 = ORIENTED_EDGE ( 'NONE', *, *, #2017, .T. ) ;
#11646 = LINE ( 'NONE', #27836, #12727 ) ;
#11647 = CARTESIAN_POINT ( 'NONE',  ( 79.92842440418704086, 18.29578799637230802, -73.57133314052174455 ) ) ;
#11648 = MECHANICAL_DESIGN_GEOMETRIC_PRESENTATION_REPRESENTATION (  '', ( #63384 ), #45406 ) ;
#11649 = CARTESIAN_POINT ( 'NONE',  ( 103.5783816667154014, 27.01328802396631801, 87.34340838971257881 ) ) ;
#11650 = DIRECTION ( 'NONE',  ( -0.000000000000000000, 1.000000000000000000, -0.000000000000000000 ) ) ;
#11651 = CARTESIAN_POINT ( 'NONE',  ( 110.2429982417149290, 28.88204397445231209, 56.45576479620100940 ) ) ;
#11652 = DIRECTION ( 'NONE',  ( -0.000000000000000000, -1.000000000000000000, -0.000000000000000000 ) ) ;
#11653 = CARTESIAN_POINT ( 'NONE',  ( -48.23389383802714292, 13.99288361739332309, -72.69372053434236136 ) ) ;
#11654 = AXIS2_PLACEMENT_3D ( 'NONE', #23374, #44819, #33227 ) ;
#11655 = DIRECTION ( 'NONE',  ( -0.000000000000000000, 1.000000000000000000, -0.000000000000000000 ) ) ;
#11656 = DIRECTION ( 'NONE',  ( 0.000000000000000000, 0.000000000000000000, 1.000000000000000000 ) ) ;
#11657 = EDGE_LOOP ( 'NONE', ( #8692, #66557, #51021, #55382 ) ) ;
#11658 = VECTOR ( 'NONE', #32677, 1000.000000000000000 ) ;
#11659 = VERTEX_POINT ( 'NONE', #39437 ) ;
#11660 = EDGE_CURVE ( 'NONE', #8487, #47971, #58067, .T. ) ;
#11661 = VECTOR ( 'NONE', #11251, 1000.000000000000000 ) ;
#11662 = CARTESIAN_POINT ( 'NONE',  ( 33.44035656425386094, 8.720466003183668491, 68.83548946330709839 ) ) ;
#11663 = DIRECTION ( 'NONE',  ( -0.000000000000000000, 1.000000000000000000, -0.000000000000000000 ) ) ;
#11664 = CARTESIAN_POINT ( 'NONE',  ( -166.5742238910466142, 81.57147158222488770, 61.49679445346814077 ) ) ;
#11665 = AXIS2_PLACEMENT_3D ( 'NONE', #59698, #43868, #61112 ) ;
#11666 = DIRECTION ( 'NONE',  ( 1.000000000000000000, 1.387778780781446908E-16, 0.000000000000000000 ) ) ;
#11667 = ADVANCED_FACE ( 'NONE', ( #23957 ), #34869, .T. ) ;
#11668 = ADVANCED_FACE ( 'NONE', ( #67240 ), #45055, .F. ) ;
#11669 = VECTOR ( 'NONE', #50266, 1000.000000000000000 ) ;
#11670 = CARTESIAN_POINT ( 'NONE',  ( -450.6627218934913230, 177.8591479523843475, 78.55029585798814651 ) ) ;
#11671 = ORIENTED_EDGE ( 'NONE', *, *, #66153, .T. ) ;
#11672 = CARTESIAN_POINT ( 'NONE',  ( 103.9685899589048148, 27.18106603025992740, -47.53878293330955529 ) ) ;
#11673 = CARTESIAN_POINT ( 'NONE',  ( 188.5651904823862424, 88.01586411309104108, -16.26953988692886099 ) ) ;
#11674 = CARTESIAN_POINT ( 'NONE',  ( -81.90266786693715062, 23.58030232261292269, -8.987966624609327937 ) ) ;
#11675 = DIRECTION ( 'NONE',  ( 0.000000000000000000, 4.930380657631322689E-32, 1.000000000000000000 ) ) ;
#11676 = CARTESIAN_POINT ( 'NONE',  ( 43.35980717318837208, 8.957244490220903188, -9.899856988890338272 ) ) ;
#11677 = CARTESIAN_POINT ( 'NONE',  ( 212.0180052085437978, 116.9552462415715297, -15.31765953654469925 ) ) ;
#11678 = FACE_BOUND ( 'NONE', #45570, .T. ) ;
#11679 = CARTESIAN_POINT ( 'NONE',  ( -61.51762070241281322, 16.51067482779403761, -38.90611071093341877 ) ) ;
#11680 = B_SPLINE_CURVE_WITH_KNOTS ( 'NONE', 3,
 ( #28365, #55803, #49812, #50523, #12543, #51221 ),
 .UNSPECIFIED., .F., .F.,
 ( 4, 2, 4 ),
 ( 0.03218932648122787427, 0.06469831129177408546, 0.09720729610232028972 ),
 .UNSPECIFIED. ) ;
#11681 = ORIENTED_EDGE ( 'NONE', *, *, #47864, .F. ) ;
#11682 = DIRECTION ( 'NONE',  ( 0.000000000000000000, 0.000000000000000000, 1.000000000000000000 ) ) ;
#11683 = CARTESIAN_POINT ( 'NONE',  ( 94.14197848494939080, 23.19876128416615657, -43.31134344884397080 ) ) ;
#11684 = CARTESIAN_POINT ( 'NONE',  ( -51.77779688167512262, 14.86590802019196822, 57.91026681902796014 ) ) ;
#11685 = CARTESIAN_POINT ( 'NONE',  ( 31.11269837220800127, -31.11269837220812562, 85.00100000000000477 ) ) ;
#11686 = CARTESIAN_POINT ( 'NONE',  ( 150.2794558856211040, 52.26944788078751003, 12.26467988490533578 ) ) ;
#11687 = CARTESIAN_POINT ( 'NONE',  ( 64.16679220703380793, -10.37413986118096254, 40.00000000000003553 ) ) ;
#11688 = EDGE_LOOP ( 'NONE', ( #68596, #34512, #59088, #39837 ) ) ;
#11689 = EDGE_CURVE ( 'NONE', #192, #7572, #65842, .T. ) ;
#11690 = CARTESIAN_POINT ( 'NONE',  ( 55.61382797299288683, 11.07686102552914953, 9.233553562912945267 ) ) ;
#11691 = LINE ( 'NONE', #44401, #11355 ) ;
#11692 = EDGE_LOOP ( 'NONE', ( #15774, #5253, #25792, #8364 ) ) ;
#11693 = ORIENTED_EDGE ( 'NONE', *, *, #24005, .F. ) ;
#11694 = VECTOR ( 'NONE', #27800, 1000.000000000000000 ) ;
#11695 = CARTESIAN_POINT ( 'NONE',  ( -4.606165167168883666E-15, -7.321656987762866997, 3.318518101603013193 ) ) ;
#11696 = CARTESIAN_POINT ( 'NONE',  ( -5.000000000000058620, -31.11269837220806878, 2.000000000000001776 ) ) ;
#11697 = CARTESIAN_POINT ( 'NONE',  ( 103.0026233023292974, 25.67408295205787994, 35.08790048083266555 ) ) ;
#11698 = VERTEX_POINT ( 'NONE', #2166 ) ;
#11699 = AXIS2_PLACEMENT_3D ( 'NONE', #55002, #28272, #20157 ) ;
#11700 = EDGE_LOOP ( 'NONE', ( #28380, #69331, #41144, #54488 ) ) ;
#11701 = CARTESIAN_POINT ( 'NONE',  ( -35.00000000000000000, 225.0000000000000000, 0.000000000000000000 ) ) ;
#11702 = CARTESIAN_POINT ( 'NONE',  ( 412.0000000000000000, -2.000000000000000000, 380.0000000000000000 ) ) ;
#11703 = CARTESIAN_POINT ( 'NONE',  ( -152.5101325120252795, 68.10842280990925701, -62.27045260355250633 ) ) ;
#11704 = CARTESIAN_POINT ( 'NONE',  ( 63.98689050258325750, 13.93365232918668362, 17.92090484651062354 ) ) ;
#11705 = VECTOR ( 'NONE', #14627, 1000.000000000000000 ) ;
#11706 = DIRECTION ( 'NONE',  ( 0.7071067811865473507, -6.441404958702665783E-16, -0.7071067811865477948 ) ) ;
#11707 = VECTOR ( 'NONE', #40828, 1000.000000000000000 ) ;
#11708 = AXIS2_PLACEMENT_3D ( 'NONE', #29359, #36020, #8254 ) ;
#11709 = CARTESIAN_POINT ( 'NONE',  ( -52.45048892661850459, 15.03803514841137812, -35.67804398155381307 ) ) ;
#11710 = VECTOR ( 'NONE', #26587, 1000.000000000000000 ) ;
#11711 = DIRECTION ( 'NONE',  ( 0.000000000000000000, 0.000000000000000000, 1.000000000000000000 ) ) ;
#11712 = LINE ( 'NONE', #50053, #58748 ) ;
#11713 = DIRECTION ( 'NONE',  ( -1.000000000000000000, 0.000000000000000000, 0.000000000000000000 ) ) ;
#11714 = CARTESIAN_POINT ( 'NONE',  ( 87.95968186927227350, 19.87904650044665900, 83.51289166538627740 ) ) ;
#11716 = ORIENTED_EDGE ( 'NONE', *, *, #46142, .F. ) ;
#11715 = CARTESIAN_POINT ( 'NONE',  ( 181.0840389613909736, -170.0000000000000000, 90.49769528643878402 ) ) ;
#11717 = VERTEX_POINT ( 'NONE', #54907 ) ;
#11718 = VERTEX_POINT ( 'NONE', #29573 ) ;
#11719 = CARTESIAN_POINT ( 'NONE',  ( -13.78293860383718972, 7.352367295275504588, -11.49084393374748281 ) ) ;
#11720 = CARTESIAN_POINT ( 'NONE',  ( -47.95468448182521826, 12.89252559348045857, 40.25230722566315933 ) ) ;
#11721 = CARTESIAN_POINT ( 'NONE',  ( -44.29440389294402536, 17.09499999999999886, 0.000000000000000000 ) ) ;
#11722 = CARTESIAN_POINT ( 'NONE',  ( 6.375108774214766072E-14, 31.11269837220806167, 85.00100000000000477 ) ) ;
#11723 = ADVANCED_FACE ( 'NONE', ( #40139 ), #19024, .T. ) ;
#11724 = CARTESIAN_POINT ( 'NONE',  ( -61.76386578474846090, 17.63453064612501819, -46.10104452603333414 ) ) ;
#11725 = EDGE_CURVE ( 'NONE', #61254, #58982, #40475, .T. ) ;
#11726 = CARTESIAN_POINT ( 'NONE',  ( -11.13714165684778656, 8.138643170880696331, -22.80719565481673072 ) ) ;
#11727 = DIRECTION ( 'NONE',  ( 1.000000000000000000, 0.000000000000000000, 0.000000000000000000 ) ) ;
#11728 = FACE_OUTER_BOUND ( 'NONE', #41382, .T. ) ;
#11729 = ORIENTED_EDGE ( 'NONE', *, *, #3580, .T. ) ;
#11730 = EDGE_CURVE ( 'NONE', #14469, #33967, #20016, .T. ) ;
#11731 = CARTESIAN_POINT ( 'NONE',  ( -4.999999999999922728, 46.66904755831208718, 0.000000000000000000 ) ) ;
#11732 = EDGE_LOOP ( 'NONE', ( #15192, #67050, #64033, #53010 ) ) ;
#11733 = ORIENTED_EDGE ( 'NONE', *, *, #52690, .F. ) ;
#11734 = CARTESIAN_POINT ( 'NONE',  ( -142.9843132609582028, 60.12226089556227748, 15.08661930014882024 ) ) ;
#11735 = CARTESIAN_POINT ( 'NONE',  ( 116.4569059613810680, 31.86445263670867334, 94.99999999999866418 ) ) ;
#11736 = DIRECTION ( 'NONE',  ( 0.000000000000000000, 0.000000000000000000, 1.000000000000000000 ) ) ;
#11737 = CARTESIAN_POINT ( 'NONE',  ( -84.49322488516129681, 0.000000000000000000, 43.58025477438756212 ) ) ;
#11738 = DIRECTION ( 'NONE',  ( -0.000000000000000000, -0.000000000000000000, -1.000000000000000000 ) ) ;
#11739 = CARTESIAN_POINT ( 'NONE',  ( 140.8855094313933307, 47.03549517811091363, -14.04929102430893018 ) ) ;
#11740 = VERTEX_POINT ( 'NONE', #28897 ) ;
#11741 = ORIENTED_EDGE ( 'NONE', *, *, #14944, .T. ) ;
#11742 = VERTEX_POINT ( 'NONE', #18329 ) ;
#11743 = AXIS2_PLACEMENT_3D ( 'NONE', #30170, #40369, #29126 ) ;
#11744 = CARTESIAN_POINT ( 'NONE',  ( -452.6627218934914367, 399.9999999999998863, -146.4497041420118251 ) ) ;
#11745 = CARTESIAN_POINT ( 'NONE',  ( -11.57931195747592668, 7.164335452024273465, 17.28240326270761784 ) ) ;
#11746 = CARTESIAN_POINT ( 'NONE',  ( 34.45817031441435319, 7.817703378455683527, -75.62602997148037787 ) ) ;
#11747 = FACE_OUTER_BOUND ( 'NONE', #2542, .T. ) ;
#11748 = ADVANCED_FACE ( 'NONE', ( #17641 ), #61249, .F. ) ;
#11749 = EDGE_CURVE ( 'NONE', #28072, #38689, #51039, .T. ) ;
#11750 = CARTESIAN_POINT ( 'NONE',  ( -37.07602570886409410, 10.58457435034603122, 59.58909574225179995 ) ) ;
#11751 = CARTESIAN_POINT ( 'NONE',  ( 200.8303160266299017, 102.8412051751308809, 69.99246994815830192 ) ) ;
#11752 = ORIENTED_EDGE ( 'NONE', *, *, #36138, .F. ) ;
#11753 = AXIS2_PLACEMENT_3D ( 'NONE', #26484, #5702, #31417 ) ;
#11754 = DIRECTION ( 'NONE',  ( 0.000000000000000000, 0.000000000000000000, -1.000000000000000000 ) ) ;
#11755 = CARTESIAN_POINT ( 'NONE',  ( 204.6977192012829505, 108.0580384837234931, -78.17048162308530834 ) ) ;
#11756 = DIRECTION ( 'NONE',  ( 0.000000000000000000, 0.000000000000000000, 1.000000000000000000 ) ) ;
#11757 = DIRECTION ( 'NONE',  ( 1.000000000000000000, 0.000000000000000000, 0.000000000000000000 ) ) ;
#11758 = DIRECTION ( 'NONE',  ( -1.850169831522831466E-16, 1.000000000000000000, 1.110223024625156294E-16 ) ) ;
#11759 = PLANE ( 'NONE',  #8418 ) ;
#11760 = CARTESIAN_POINT ( 'NONE',  ( -25.99999999999998934, 0.000000000000000000, -50.00000000000000000 ) ) ;
#11761 =( GEOMETRIC_REPRESENTATION_CONTEXT ( 3 ) GLOBAL_UNCERTAINTY_ASSIGNED_CONTEXT ( ( #50093 ) ) GLOBAL_UNIT_ASSIGNED_CONTEXT ( ( #61431, #56148, #17464 ) ) REPRESENTATION_CONTEXT ( 'NONE', 'WORKASPACE' ) );
#11762 = CARTESIAN_POINT ( 'NONE',  ( 20.74852474914887424, 6.709938988646750424, 70.00598210749363659 ) ) ;
#11763 = DIRECTION ( 'NONE',  ( 0.000000000000000000, 0.000000000000000000, 1.000000000000000000 ) ) ;
#11764 = CARTESIAN_POINT ( 'NONE',  ( 13.84937401517046851, 6.446378549072247388, -62.61427068757215153 ) ) ;
#11765 = VECTOR ( 'NONE', #41046, 1000.000000000000000 ) ;
#11766 = CIRCLE ( 'NONE', #51098, 25.00000000000395772 ) ;
#11767 = B_SPLINE_CURVE_WITH_KNOTS ( 'NONE', 3,
 ( #55032, #6854, #886, #44488, #12842, #60320 ),
 .UNSPECIFIED., .F., .F.,
 ( 4, 2, 4 ),
 ( 0.02753256083616404531, 0.02987018135583072859, 0.03220780187549741186 ),
 .UNSPECIFIED. ) ;
#11768 = ORIENTED_EDGE ( 'NONE', *, *, #57745, .F. ) ;
#11769 = CARTESIAN_POINT ( 'NONE',  ( -8.000000000000000000, 3.115336682266996338, -0.3193931313915024384 ) ) ;
#11770 = DIRECTION ( 'NONE',  ( -0.000000000000000000, -1.000000000000000000, -0.000000000000000000 ) ) ;
#11771 = DIRECTION ( 'NONE',  ( 0.000000000000000000, 0.000000000000000000, 1.000000000000000000 ) ) ;
#11772 = CARTESIAN_POINT ( 'NONE',  ( 46.89006465517229572, 9.501960077668742954, -69.47552966857396939 ) ) ;
#11773 = CARTESIAN_POINT ( 'NONE',  ( 56.94505604581136282, 12.37336791557970272, -74.47650229381035558 ) ) ;
#11774 = ORIENTED_EDGE ( 'NONE', *, *, #55986, .T. ) ;
#11775 = ORIENTED_EDGE ( 'NONE', *, *, #59603, .T. ) ;
#11776 = DIRECTION ( 'NONE',  ( -0.000000000000000000, 1.000000000000000000, -0.000000000000000000 ) ) ;
#11777 = CARTESIAN_POINT ( 'NONE',  ( 24.39800339187844003, 60.26242556095705538, 170.0000000000000000 ) ) ;
#11778 = VERTEX_POINT ( 'NONE', #34178 ) ;
#11779 = VERTEX_POINT ( 'NONE', #7785 ) ;
#11780 = CARTESIAN_POINT ( 'NONE',  ( 174.6176230994778109, 72.30829341023249413, -39.88575702694497238 ) ) ;
#11781 = DIRECTION ( 'NONE',  ( 1.000000000000000000, 0.000000000000000000, 0.000000000000000000 ) ) ;
#11782 = ORIENTED_EDGE ( 'NONE', *, *, #48104, .T. ) ;
#11783 = CYLINDRICAL_SURFACE ( 'NONE', #44688, 7.500000000000013323 ) ;
#11784 = CARTESIAN_POINT ( 'NONE',  ( 139.6326990672751549, 46.22017155708130076, 59.06439119612976896 ) ) ;
#11785 = CARTESIAN_POINT ( 'NONE',  ( -75.64857587248467041, 21.19501514561450151, -35.74525540028072612 ) ) ;
#11786 = FACE_OUTER_BOUND ( 'NONE', #1150, .T. ) ;
#11787 = DIRECTION ( 'NONE',  ( 0.000000000000000000, 0.000000000000000000, 1.000000000000000000 ) ) ;
#11788 = CARTESIAN_POINT ( 'NONE',  ( -55.05276343752909440, 15.72344139423348430, -23.37177340799619785 ) ) ;
#11789 = ORIENTED_EDGE ( 'NONE', *, *, #4233, .T. ) ;
#11790 = CARTESIAN_POINT ( 'NONE',  ( 113.4351684956570381, 30.38657459074488543, -50.22549693574652707 ) ) ;
#11791 = VECTOR ( 'NONE', #17720, 1000.000000000000000 ) ;
#11792 = CARTESIAN_POINT ( 'NONE',  ( -78.18897186942405142, 23.21604822208489338, 18.57365054920947856 ) ) ;
#11793 = CARTESIAN_POINT ( 'NONE',  ( -142.0860844253783171, 59.41107357617637774, -43.43222315112575416 ) ) ;
#11794 = LINE ( 'NONE', #42430, #6187 ) ;
#11795 = AXIS2_PLACEMENT_3D ( 'NONE', #35959, #31375, #58102 ) ;
#11797 = VERTEX_POINT ( 'NONE', #28177 ) ;
#11796 = CARTESIAN_POINT ( 'NONE',  ( 111.9975424824652634, 170.0000000000000284, 354.1673509436691347 ) ) ;
#11798 = LINE ( 'NONE', #6536, #64524 ) ;
#11799 = ADVANCED_FACE ( 'NONE', ( #22913, #60890 ), #52419, .T. ) ;
#11800 = AXIS2_PLACEMENT_3D ( 'NONE', #43232, #65057, #64706 ) ;
#11801 = AXIS2_PLACEMENT_3D ( 'NONE', #52268, #41025, #62482 ) ;
#11802 = VERTEX_POINT ( 'NONE', #68925 ) ;
#11803 = CARTESIAN_POINT ( 'NONE',  ( -144.9439644317224634, 60.40328483334192811, 59.10885205279113563 ) ) ;
#11804 = DIRECTION ( 'NONE',  ( -1.850169831522831466E-16, 1.000000000000000000, 1.110223024625156294E-16 ) ) ;
#11805 = CARTESIAN_POINT ( 'NONE',  ( 64.98797965777978902, 1.250000000000011990, 40.00000000000003553 ) ) ;
#11806 =( GEOMETRIC_REPRESENTATION_CONTEXT ( 3 ) GLOBAL_UNCERTAINTY_ASSIGNED_CONTEXT ( ( #39538 ) ) GLOBAL_UNIT_ASSIGNED_CONTEXT ( ( #37800, #513, #38141 ) ) REPRESENTATION_CONTEXT ( 'NONE', 'WORKASPACE' ) );
#11808 = CARTESIAN_POINT ( 'NONE',  ( 92.21252738308862718, 22.47457138983956426, 32.18003665462427421 ) ) ;
#11807 = CONICAL_SURFACE ( 'NONE', #20800, 74.95140232871122521, 0.8777644062502172329 ) ;
#11809 = EDGE_CURVE ( 'NONE', #57714, #8357, #35203, .T. ) ;
#11810 = CARTESIAN_POINT ( 'NONE',  ( -165.6754884515988522, -170.0000000000000000, -95.00000000000133582 ) ) ;
#11811 = DIRECTION ( 'NONE',  ( 1.000000000000000000, 0.000000000000000000, -0.000000000000000000 ) ) ;
#11812 = CARTESIAN_POINT ( 'NONE',  ( 94.02921784728462740, 22.08005910033070407, -68.91924186718193823 ) ) ;
#11813 = AXIS2_PLACEMENT_3D ( 'NONE', #29215, #42438, #18665 ) ;
#11814 = ADVANCED_FACE ( 'NONE', ( #47465 ), #57354, .F. ) ;
#11815 = CARTESIAN_POINT ( 'NONE',  ( -26.28838098083469887, -20.64471174685882815, 6.893342936425401746 ) ) ;
#11816 = CARTESIAN_POINT ( 'NONE',  ( 92.91022130985207639, 22.73448145304546131, 94.99999999999866418 ) ) ;
#11817 = ORIENTED_EDGE ( 'NONE', *, *, #59760, .F. ) ;
#11818 = ORIENTED_EDGE ( 'NONE', *, *, #17427, .F. ) ;
#11819 = EDGE_CURVE ( 'NONE', #30259, #53637, #18799, .T. ) ;
#11820 = CARTESIAN_POINT ( 'NONE',  ( 46.76970795284346138, 9.482505412758886365, 38.87896366950010218 ) ) ;
#11821 = DIRECTION ( 'NONE',  ( 0.000000000000000000, 0.000000000000000000, 1.000000000000000000 ) ) ;
#11822 = DIRECTION ( 'NONE',  ( 0.000000000000000000, 0.000000000000000000, 1.000000000000000000 ) ) ;
#11823 = DIRECTION ( 'NONE',  ( -0.000000000000000000, -0.000000000000000000, -1.000000000000000000 ) ) ;
#11824 = CARTESIAN_POINT ( 'NONE',  ( 212.0075063341773216, 118.7912820769029167, -45.53480672108666027 ) ) ;
#11825 = DIRECTION ( 'NONE',  ( -1.000000000000000000, 0.000000000000000000, 0.000000000000000000 ) ) ;
#11826 = DIRECTION ( 'NONE',  ( 0.5407162030609375947, -0.6444004775717707689, -0.5407162030609372616 ) ) ;
#11827 = CARTESIAN_POINT ( 'NONE',  ( 42.71247067544614140, 9.879726907348455711, -49.85411309355188081 ) ) ;
#11829 = DIRECTION ( 'NONE',  ( 0.000000000000000000, 1.000000000000000000, 0.000000000000000000 ) ) ;
#11828 = B_SPLINE_CURVE_WITH_KNOTS ( 'NONE', 3,
 ( #1540, #44807, #44085, #66285, #7532, #39187 ),
 .UNSPECIFIED., .F., .F.,
 ( 4, 2, 4 ),
 ( 2.380731629557410192E-07, 0.002336973833157566377, 0.004673709593152176531 ),
 .UNSPECIFIED. ) ;
#11830 = ORIENTED_EDGE ( 'NONE', *, *, #19401, .T. ) ;
#11831 = CARTESIAN_POINT ( 'NONE',  ( -24.32471770265758337, 9.546495606312142002, 8.447192770170387277 ) ) ;
#11832 = ORIENTED_EDGE ( 'NONE', *, *, #9610, .T. ) ;
#11833 = CARTESIAN_POINT ( 'NONE',  ( -65.36598343705435354, 0.000000000000000000, 41.38025477438755928 ) ) ;
#11834 = CARTESIAN_POINT ( 'NONE',  ( -84.60829019729341383, 24.67443150164869436, 87.01983487678488416 ) ) ;
#11835 = CARTESIAN_POINT ( 'NONE',  ( -8.000000000000000000, 4.618802153517024500, -8.785468820183664818 ) ) ;
#11836 = ADVANCED_FACE ( 'NONE', ( #9861 ), #32254, .F. ) ;
#11837 = CARTESIAN_POINT ( 'NONE',  ( 127.2107679985236217, 38.70844091144994792, 40.52525586269725721 ) ) ;
#11838 = CARTESIAN_POINT ( 'NONE',  ( 35.44311777160621801, 8.940232499250164722, 16.94408402799438207 ) ) ;
#11839 = DIRECTION ( 'NONE',  ( -1.000000000000000000, 0.000000000000000000, 0.000000000000000000 ) ) ;
#11840 = DIRECTION ( 'NONE',  ( -0.3930250316539278255, 0.9195277725514487965, 0.000000000000000000 ) ) ;
#11841 = DIRECTION ( 'NONE',  ( 0.000000000000000000, 1.000000000000000000, 0.000000000000000000 ) ) ;
#11842 = PLANE ( 'NONE',  #10197 ) ;
#11843 = DIRECTION ( 'NONE',  ( 0.000000000000000000, 0.000000000000000000, 1.000000000000000000 ) ) ;
#11844 = ORIENTED_EDGE ( 'NONE', *, *, #7613, .T. ) ;
#11845 = CARTESIAN_POINT ( 'NONE',  ( 55.76255201544532270, 12.13275766515752352, 62.18578305727515243 ) ) ;
#11846 = CARTESIAN_POINT ( 'NONE',  ( -26.49516976694651049, 8.831756547364873811, 16.53298603352267193 ) ) ;
#11847 = DIRECTION ( 'NONE',  ( 0.000000000000000000, 0.000000000000000000, 1.000000000000000000 ) ) ;
#11848 = CARTESIAN_POINT ( 'NONE',  ( -4.000000000000009770, -6.928203230275505220, 0.000000000000000000 ) ) ;
#11849 = CARTESIAN_POINT ( 'NONE',  ( 88.27048647651604085, 21.05338532470119262, 83.57569936033996782 ) ) ;
#11850 = AXIS2_PLACEMENT_3D ( 'NONE', #55413, #1973, #39938 ) ;
#11851 = ORIENTED_EDGE ( 'NONE', *, *, #35357, .T. ) ;
#11852 = VECTOR ( 'NONE', #54905, 1000.000000000000000 ) ;
#11853 = CARTESIAN_POINT ( 'NONE',  ( 403.0071894358330837, 616.3301249052418598, 794.5748919861035802 ) ) ;
#11854 = LINE ( 'NONE', #60399, #36336 ) ;
#11855 = CARTESIAN_POINT ( 'NONE',  ( -130.5740389938243027, 49.65308610043480542, 17.15553663445870569 ) ) ;
#11856 = LINE ( 'NONE', #34023, #28999 ) ;
#11857 = CONTEXT_DEPENDENT_SHAPE_REPRESENTATION ( #30148, #25528 ) ;
#11858 = CARTESIAN_POINT ( 'NONE',  ( -133.3923804760465543, 52.87100816290222838, -42.98098741808147594 ) ) ;
#11859 = VERTEX_POINT ( 'NONE', #41177 ) ;
#11861 = CARTESIAN_POINT ( 'NONE',  ( -120.4816138481824908, 43.03185659245511374, -47.62858304183759373 ) ) ;
#11860 = AXIS2_PLACEMENT_3D ( 'NONE', #22780, #28766, #2039 ) ;
#11862 = VECTOR ( 'NONE', #57382, 1000.000000000000000 ) ;
#11863 = DIRECTION ( 'NONE',  ( -9.109522253334613014E-16, -1.000000000000000000, 3.889846672687432470E-31 ) ) ;
#11864 = AXIS2_PLACEMENT_3D ( 'NONE', #14386, #20005, #62570 ) ;
#11865 = LINE ( 'NONE', #49837, #50431 ) ;
#11866 = AXIS2_PLACEMENT_3D ( 'NONE', #32228, #27277, #16725 ) ;
#11867 = CARTESIAN_POINT ( 'NONE',  ( -173.1211646369891355, -170.0000000000000000, -49.71195716475001092 ) ) ;
#11868 = VECTOR ( 'NONE', #16576, 1000.000000000000000 ) ;
#11869 = FACE_OUTER_BOUND ( 'NONE', #1889, .T. ) ;
#11870 = ORIENTED_EDGE ( 'NONE', *, *, #25827, .F. ) ;
#11871 = CARTESIAN_POINT ( 'NONE',  ( -58.75378739419587504, 16.75118858561006263, 4.431123600893071668 ) ) ;
#11872 = DIRECTION ( 'NONE',  ( -0.000000000000000000, -0.000000000000000000, -1.000000000000000000 ) ) ;
#11873 = CARTESIAN_POINT ( 'NONE',  ( -152.4930836497867404, 68.09400557494207362, 31.33700391404592267 ) ) ;
#11874 = DIRECTION ( 'NONE',  ( 0.000000000000000000, 0.000000000000000000, 1.000000000000000000 ) ) ;
#11876 = ORIENTED_EDGE ( 'NONE', *, *, #41160, .T. ) ;
#11875 = CARTESIAN_POINT ( 'NONE',  ( -173.1211646369891355, 88.63826465341151106, -76.55650775521370122 ) ) ;
#11877 = EDGE_CURVE ( 'NONE', #25430, #13094, #43478, .T. ) ;
#11878 = CARTESIAN_POINT ( 'NONE',  ( 410.0000000000000000, 0.000000000000000000, 2.000000000000000000 ) ) ;
#11879 = VERTEX_POINT ( 'NONE', #26034 ) ;
#11880 = ORIENTED_EDGE ( 'NONE', *, *, #66545, .T. ) ;
#11881 = CARTESIAN_POINT ( 'NONE',  ( -120.5463017468902223, 43.07239852585537676, -90.83929640405872874 ) ) ;
#11882 = DIRECTION ( 'NONE',  ( 0.000000000000000000, 0.000000000000000000, 1.000000000000000000 ) ) ;
#11884 = ORIENTED_EDGE ( 'NONE', *, *, #67906, .T. ) ;
#11883 = CARTESIAN_POINT ( 'NONE',  ( -11.56945424397729205, 8.173256823723107800, -76.26585737041517632 ) ) ;
#11885 = LINE ( 'NONE', #44596, #56651 ) ;
#11886 = CARTESIAN_POINT ( 'NONE',  ( -7.825402957745085430, -170.0000000000000000, -77.26262132240753999 ) ) ;
#11887 = DIRECTION ( 'NONE',  ( 0.000000000000000000, 0.000000000000000000, 1.000000000000000000 ) ) ;
#11888 = ORIENTED_EDGE ( 'NONE', *, *, #36705, .T. ) ;
#11889 = CARTESIAN_POINT ( 'NONE',  ( -143.6098676033357435, 60.62137621171688551, -91.34574462907563941 ) ) ;
#11890 = EDGE_CURVE ( 'NONE', #46362, #8192, #56659, .T. ) ;
#11891 = CIRCLE ( 'NONE', #13079, 65.36598343705435354 ) ;
#11892 = CARTESIAN_POINT ( 'NONE',  ( -36.37663950036511551, 10.45389057208229033, -10.30609290290592028 ) ) ;
#11893 = CARTESIAN_POINT ( 'NONE',  ( 183.2136430849847955, 6.000000000000000000, -36.68900338898718871 ) ) ;
#11894 = CARTESIAN_POINT ( 'NONE',  ( 133.8566784816069344, 42.60093787723652525, 56.35489142945903751 ) ) ;
#11895 = CARTESIAN_POINT ( 'NONE',  ( 21.44191228441539820, 7.755009954762319246, 59.40633199949923693 ) ) ;
#11896 = VERTEX_POINT ( 'NONE', #3207 ) ;
#11897 = EDGE_LOOP ( 'NONE', ( #34288, #67277, #15013, #55475 ) ) ;
#11898 = AXIS2_PLACEMENT_3D ( 'NONE', #593, #21349, #64613 ) ;
#11899 = ORIENTED_EDGE ( 'NONE', *, *, #69174, .F. ) ;
#11900 = ADVANCED_FACE ( 'NONE', ( #30624 ), #3535, .F. ) ;
#11901 = CARTESIAN_POINT ( 'NONE',  ( 207.3579397550547299, 110.0617317161169240, -90.49398837928671924 ) ) ;
#11902 = CARTESIAN_POINT ( 'NONE',  ( -104.1225399044495674, 34.86084180570097857, 3.900553033110677692 ) ) ;
#11903 = AXIS2_PLACEMENT_3D ( 'NONE', #1219, #44831, #1564 ) ;
#11904 = CIRCLE ( 'NONE', #31997, 24.99999999999985434 ) ;
#11905 = CARTESIAN_POINT ( 'NONE',  ( -84.49322488516129681, 0.000000000000000000, 43.58025477438756212 ) ) ;
#11906 = CARTESIAN_POINT ( 'NONE',  ( -35.99432170610151616, 10.38324794858010591, -48.79525134090449967 ) ) ;
#11907 = CARTESIAN_POINT ( 'NONE',  ( -95.06174767693123329, 29.26266015133881737, 93.77071720667551347 ) ) ;
#11908 = FACE_OUTER_BOUND ( 'NONE', #66461, .T. ) ;
#11909 = CARTESIAN_POINT ( 'NONE',  ( -130.1964689553232972, 49.39217932424203639, 71.12517339982724707 ) ) ;
#11910 = CARTESIAN_POINT ( 'NONE',  ( -71.23176719684944658, 20.69188312694499032, -14.75110734384959166 ) ) ;
#11911 = AXIS2_PLACEMENT_3D ( 'NONE', #57071, #29989, #14155 ) ;
#11912 = DIRECTION ( 'NONE',  ( 0.9362348706397369824, 0.3513748240813435175, 0.000000000000000000 ) ) ;
#11913 = ORIENTED_EDGE ( 'NONE', *, *, #57575, .T. ) ;
#11915 = AXIS2_PLACEMENT_3D ( 'NONE', #58362, #5586, #64687 ) ;
#11914 = CARTESIAN_POINT ( 'NONE',  ( -99.01653716841812525, 32.27413039285141139, -89.43734291363955435 ) ) ;
#11916 = CYLINDRICAL_SURFACE ( 'NONE', #22859, 7.500000000000013323 ) ;
#11917 = VERTEX_POINT ( 'NONE', #13747 ) ;
#11918 = CARTESIAN_POINT ( 'NONE',  ( 182.7720841008444097, 80.32850885226588389, 29.49789156618269104 ) ) ;
#11919 = ADVANCED_FACE ( 'NONE', ( #25701 ), #68593, .T. ) ;
#11920 = CARTESIAN_POINT ( 'NONE',  ( 442.3372781065085633, 395.0000000000001137, -141.4497041420118251 ) ) ;
#11921 = CARTESIAN_POINT ( 'NONE',  ( -71.41745561414262511, 19.69148172991712187, 13.06265200711892582 ) ) ;
#11922 = CARTESIAN_POINT ( 'NONE',  ( -118.7011544766493500, 43.11604763363181547, 67.10580360906620001 ) ) ;
#11923 = CARTESIAN_POINT ( 'NONE',  ( -47.95468448182520405, 12.89252559348046567, 13.40775663519948679 ) ) ;
#11924 = EDGE_CURVE ( 'NONE', #69210, #11023, #67920, .T. ) ;
#11925 = CARTESIAN_POINT ( 'NONE',  ( 0.1317522424472107878, 1.959574484719855736, -8.000000000000000000 ) ) ;
#11926 = ADVANCED_FACE ( 'NONE', ( #51728 ), #36243, .F. ) ;
#11927 = CARTESIAN_POINT ( 'NONE',  ( -2.645508037661904233, -7.710219529346618472, -9.431901280394557219 ) ) ;
#11928 = VERTEX_POINT ( 'NONE', #8479 ) ;
#11929 = FACE_OUTER_BOUND ( 'NONE', #40187, .T. ) ;
#11930 = CARTESIAN_POINT ( 'NONE',  ( -189.0973937025975999, 108.4049737838939222, 89.83184869644205151 ) ) ;
#11931 = ORIENTED_EDGE ( 'NONE', *, *, #43815, .F. ) ;
#11932 = CARTESIAN_POINT ( 'NONE',  ( 98.48662049252135375, -156.6058287036421461, 0.000000000000000000 ) ) ;
#11933 = LINE ( 'NONE', #42641, #20697 ) ;
#11934 = ORIENTED_EDGE ( 'NONE', *, *, #42075, .F. ) ;
#11935 = CARTESIAN_POINT ( 'NONE',  ( -83.14462298835724141, 24.07775853418030110, 31.88262967278052784 ) ) ;
#11936 = CARTESIAN_POINT ( 'NONE',  ( -25.07735481787161547, 9.648965052008781740, -73.64150853364553484 ) ) ;
#11937 = CARTESIAN_POINT ( 'NONE',  ( 46.65860211212412167, 10.48377752989033773, 39.37290686888943014 ) ) ;
#11938 = CARTESIAN_POINT ( 'NONE',  ( -30.95355748062276291, 9.511738996772320931, 57.06100499665286918 ) ) ;
#11939 = CARTESIAN_POINT ( 'NONE',  ( -145.3109762780891003, 60.69959559383372749, 17.60952691763336375 ) ) ;
#11940 = VERTEX_POINT ( 'NONE', #30281 ) ;
#11941 = ORIENTED_EDGE ( 'NONE', *, *, #45340, .F. ) ;
#11942 = CARTESIAN_POINT ( 'NONE',  ( -65.36598343705435354, 0.000000000000000000, 41.38025477438755928 ) ) ;
#11943 = EDGE_LOOP ( 'NONE', ( #55108, #57726, #64257, #269 ) ) ;
#11944 = CARTESIAN_POINT ( 'NONE',  ( 32.90051628396145134, 8.664124555952444240, -20.04662842472982121 ) ) ;
#11945 = CARTESIAN_POINT ( 'NONE',  ( -417.6627218934913799, 0.000000000000000000, -146.4497041420118251 ) ) ;
#11946 = CARTESIAN_POINT ( 'NONE',  ( -6.843910203392213454, 7.836697961436718707, 18.22254118960022140 ) ) ;
#11947 = CARTESIAN_POINT ( 'NONE',  ( 141.1579982455003233, 47.21428277316857702, 92.45156317765301424 ) ) ;
#11948 = PRODUCT ( 'shaft', 'shaft', '', ( #64547 ) ) ;
#11949 = DIRECTION ( 'NONE',  ( -0.4738686624729966379, -0.8805955318567391110, 0.000000000000000000 ) ) ;
#11950 = DIRECTION ( 'NONE',  ( -0.000000000000000000, -0.000000000000000000, 1.000000000000000000 ) ) ;
#11951 = CIRCLE ( 'NONE', #69290, 8.000000000000000000 ) ;
#11952 = VERTEX_POINT ( 'NONE', #36593 ) ;
#11953 = CARTESIAN_POINT ( 'NONE',  ( 8.000000000000000000, 4.618802153517024500, -0.7145311798163346273 ) ) ;
#11954 = EDGE_LOOP ( 'NONE', ( #34367, #18717 ) ) ;
#11955 = ORIENTED_EDGE ( 'NONE', *, *, #37368, .F. ) ;
#11956 = CYLINDRICAL_SURFACE ( 'NONE', #65996, 7.500000000000013323 ) ;
#11957 = CARTESIAN_POINT ( 'NONE',  ( 412.3372781065085633, 179.4906275429376024, -144.4497041420117682 ) ) ;
#11958 = AXIS2_PLACEMENT_3D ( 'NONE', #13416, #34879, #56317 ) ;
#11959 = CARTESIAN_POINT ( 'NONE',  ( 157.4703587214989398, -170.0000000000000000, -77.96873488960135035 ) ) ;
#11960 = CARTESIAN_POINT ( 'NONE',  ( -125.8938041572051105, 47.69968343338781125, -88.60280507916129977 ) ) ;
#11961 = DIRECTION ( 'NONE',  ( 0.9989930665413143673, 0.04486483035051862939, -2.310635633156372120E-16 ) ) ;
#11962 = CIRCLE ( 'NONE', #36677, 65.36598343705435354 ) ;
#11963 = ORIENTED_EDGE ( 'NONE', *, *, #22370, .T. ) ;
#11964 = EDGE_CURVE ( 'NONE', #36942, #9188, #46862, .T. ) ;
#11965 = VERTEX_POINT ( 'NONE', #2688 ) ;
#11966 = CARTESIAN_POINT ( 'NONE',  ( 79.38459371357855332, 17.07499996355402061, 12.37235545723701691 ) ) ;
#11967 = VERTEX_POINT ( 'NONE', #63323 ) ;
#11968 = CARTESIAN_POINT ( 'NONE',  ( -72.76696720809546548, 20.16136115364206916, 42.57569858987972822 ) ) ;
#11969 = ORIENTED_EDGE ( 'NONE', *, *, #7224, .F. ) ;
#11970 = EDGE_CURVE ( 'NONE', #34424, #65974, #14095, .T. ) ;
#11971 = AXIS2_PLACEMENT_3D ( 'NONE', #3792, #57263, #13652 ) ;
#11972 = CARTESIAN_POINT ( 'NONE',  ( 131.9963487224087544, 40.31229003000635913, -89.93695264016190549 ) ) ;
#11973 = ORIENTED_EDGE ( 'NONE', *, *, #38417, .F. ) ;
#11974 = CARTESIAN_POINT ( 'NONE',  ( -123.6618353044034819, 46.23845779494349983, 4.100425436027088644 ) ) ;
#11975 = CARTESIAN_POINT ( 'NONE',  ( 91.67571176799447130, 21.20498955963028465, 4.813890606363044000 ) ) ;
#11976 = DIRECTION ( 'NONE',  ( -0.6910626489868685329, 0.7227948638273878901, 0.000000000000000000 ) ) ;
#11977 = ORIENTED_EDGE ( 'NONE', *, *, #32971, .F. ) ;
#11978 = DIRECTION ( 'NONE',  ( 0.000000000000000000, 0.000000000000000000, -1.000000000000000000 ) ) ;
#11979 = EDGE_CURVE ( 'NONE', #21301, #16538, #15131, .T. ) ;
#11980 = EDGE_CURVE ( 'NONE', #20401, #50694, #23794, .T. ) ;
#11981 = PRESENTATION_STYLE_ASSIGNMENT (( #60160 ) ) ;
#11982 = CARTESIAN_POINT ( 'NONE',  ( 33.75794032130628608, 8.754084575552409930, 42.37720922280519886 ) ) ;
#11983 = CARTESIAN_POINT ( 'NONE',  ( -180.6209674222602359, 97.47999311542514533, -42.37861601742196882 ) ) ;
#11984 = FACE_BOUND ( 'NONE', #51693, .T. ) ;
#11985 = CARTESIAN_POINT ( 'NONE',  ( 111.9975424824652634, 20.00000000000003197, 536.6193948016162949 ) ) ;
#11986 = DIRECTION ( 'NONE',  ( -1.000000000000000000, 0.000000000000000000, 0.000000000000000000 ) ) ;
#11988 = ORIENTED_EDGE ( 'NONE', *, *, #55941, .F. ) ;
#11987 = ADVANCED_FACE ( 'NONE', ( #16503 ), #26380, .T. ) ;
#11989 = CARTESIAN_POINT ( 'NONE',  ( 136.7690435008551049, 44.39743995805024213, -77.28318001848430185 ) ) ;
#11990 = CARTESIAN_POINT ( 'NONE',  ( -147.7925265216585444, 64.04960911618974251, -76.46199663651751166 ) ) ;
#11991 = VERTEX_POINT ( 'NONE', #11556 ) ;
#11992 = EDGE_CURVE ( 'NONE', #53816, #62932, #6296, .T. ) ;
#11993 = FACE_BOUND ( 'NONE', #51805, .T. ) ;
#11994 = CARTESIAN_POINT ( 'NONE',  ( -6.840981040171505434, 6.828436339979227832, -62.31109642460706510 ) ) ;
#11995 = CARTESIAN_POINT ( 'NONE',  ( -178.2448732545371115, 94.58403736950708662, 70.66284363813151970 ) ) ;
#11996 = DIRECTION ( 'NONE',  ( 0.000000000000000000, 0.000000000000000000, 1.000000000000000000 ) ) ;
#11997 = DIRECTION ( 'NONE',  ( 0.7530714660036099684, 0.6579387259397136978, 0.000000000000000000 ) ) ;
#11998 = CARTESIAN_POINT ( 'NONE',  ( -6.843910203392213454, 7.836697961436722260, 45.06709178006389038 ) ) ;
#11999 = CARTESIAN_POINT ( 'NONE',  ( 8.000000000000007105, 249.8719672152120381, 94.99999999999866418 ) ) ;
#12000 = CARTESIAN_POINT ( 'NONE',  ( 113.9761838721218368, 21.78940454476515853, 3.049139182071525678 ) ) ;
#12001 = CARTESIAN_POINT ( 'NONE',  ( -6.125624616441583292, 7.794071945221087816, -8.764598286888389822 ) ) ;
#12002 = CARTESIAN_POINT ( 'NONE',  ( -15.27733754929849930, 8.502213909106947298, 38.59432969851645367 ) ) ;
#12003 = CARTESIAN_POINT ( 'NONE',  ( 116.8937673311172887, 32.08228998570057655, 6.790944445358706894 ) ) ;
#12004 = CARTESIAN_POINT ( 'NONE',  ( 94.11595392909974578, 23.18887043179185525, -15.96272041242249884 ) ) ;
#12005 = ORIENTED_EDGE ( 'NONE', *, *, #21449, .T. ) ;
#12006 = CARTESIAN_POINT ( 'NONE',  ( -38.16652041892307778, 11.81761816422915956, 7.520151233602119234 ) ) ;
#12007 = ORIENTED_EDGE ( 'NONE', *, *, #15952, .F. ) ;
#12008 = CARTESIAN_POINT ( 'NONE',  ( -14.86595946517991429, -20.25193917588099524, 0.000000000000000000 ) ) ;
#12009 = CARTESIAN_POINT ( 'NONE',  ( 79.22872707466395070, 18.07970189365808622, -68.92354796247994386 ) ) ;
#12010 = VECTOR ( 'NONE', #48767, 1000.000000000000000 ) ;
#12011 = CARTESIAN_POINT ( 'NONE',  ( 106.8650810127286235, 28.45160516703612075, 84.09606632055420050 ) ) ;
#12012 = DIRECTION ( 'NONE',  ( -0.8805955318567391110, 0.4738686624729966379, 2.500042656554809847E-16 ) ) ;
#12013 = CARTESIAN_POINT ( 'NONE',  ( -15.21063934378433657, 7.484993339139951019, 89.95709727327218275 ) ) ;
#12014 = ADVANCED_FACE ( 'NONE', ( #47818 ), #37257, .T. ) ;
#12015 = EDGE_CURVE ( 'NONE', #25148, #2042, #63692, .T. ) ;
#12016 = CARTESIAN_POINT ( 'NONE',  ( 133.8566784816069344, 42.60093787723652525, -51.02331093239568816 ) ) ;
#12017 = CARTESIAN_POINT ( 'NONE',  ( 0.000000000000000000, 6.928203230275505220, -4.000000000000007994 ) ) ;
#12018 = CARTESIAN_POINT ( 'NONE',  ( -77.82491691702773551, 23.07808431488692946, -88.83991494168476777 ) ) ;
#12019 = ADVANCED_FACE ( 'NONE', ( #32347 ), #53084, .F. ) ;
#12020 = CARTESIAN_POINT ( 'NONE',  ( -188.6739852773921200, 108.2139733222100375, -67.25001060397961794 ) ) ;
#12021 = ORIENTED_EDGE ( 'NONE', *, *, #47787, .F. ) ;
#12022 = ORIENTED_EDGE ( 'NONE', *, *, #68445, .T. ) ;
#12023 = CARTESIAN_POINT ( 'NONE',  ( 311.9975424824652350, 307.8795515535290974, 6.994434899193393562 ) ) ;
#12024 = CARTESIAN_POINT ( 'NONE',  ( 177.7889574972182345, 75.33777460203559428, 56.90074107153713356 ) ) ;
#12025 = DIRECTION ( 'NONE',  ( 0.000000000000000000, 1.000000000000000000, -0.000000000000000000 ) ) ;
#12026 = CARTESIAN_POINT ( 'NONE',  ( -22.06416059020174103, -12.01293505575318044, 3.061616997868437868E-16 ) ) ;
#12027 = AXIS2_PLACEMENT_3D ( 'NONE', #22798, #17512, #48807 ) ;
#12028 = CARTESIAN_POINT ( 'NONE',  ( -166.7136514167008841, 81.71618216218793407, -19.27443722847174712 ) ) ;
#12029 = LINE ( 'NONE', #27852, #18305 ) ;
#12030 = EDGE_LOOP ( 'NONE', ( #60262, #3030, #68455, #32444, #32513 ) ) ;
#12031 = CARTESIAN_POINT ( 'NONE',  ( 92.21252738308859875, 22.47457138983955360, 5.335486064160578579 ) ) ;
#12032 = LINE ( 'NONE', #39126, #903 ) ;
#12033 = CARTESIAN_POINT ( 'NONE',  ( 10.31616749326173377, 7.393414706728906438, 59.22449557915167162 ) ) ;
#12034 = B_SPLINE_CURVE_WITH_KNOTS ( 'NONE', 3,
 ( #52225, #14259, #51879, #63822, #9673, #31134, #35718, #37083, #25855, #58525, #47283, #5066, #16659, #53929, #16316, #1530, #37419, #59216, #53589, #27557, #17352, #59557, #38827, #48644, #32841, #65203, #16998, #5752, #22289, #60276, #27913, #6099, #59907, #6803, #38113, #37772, #21586, #1184, #28255, #11035, #64857, #48298, #32498, #487, #131 ),
 .UNSPECIFIED., .F., .F.,
 ( 4, 2, 2, 1, 2, 2, 2, 2, 2, 2, 2, 2, 2, 2, 2, 2, 2, 2, 2, 2, 2, 2, 4 ),
 ( 0.02345095402629350512, 0.02491692321306681820, 0.02564990780645347995, 0.02638289239984013823, 0.02711587699322679998, 0.02784886158661346173, 0.02931483077338677828, 0.03004781536677343656, 0.03078079996016009484, 0.03224676914693341834, 0.03297975374032006968, 0.03371273833370672102, 0.03517870752048002370, 0.03664467670725332638, 0.03737766130063997772, 0.03811064589402662905, 0.03957661508079992480, 0.04104258426757322747, 0.04250855345434652321, 0.04324153804773317455, 0.04397452264111982589, 0.04544049182789310082, 0.04690646101466638962 ),
 .UNSPECIFIED. ) ;
#12035 = CARTESIAN_POINT ( 'NONE',  ( -20.55634918610411077, -41.66904755831209428, 2.000000000000001776 ) ) ;
#12036 = CARTESIAN_POINT ( 'NONE',  ( 46.65037935242575884, 9.463293687292223311, -14.33328965919755404 ) ) ;
#12037 = CARTESIAN_POINT ( 'NONE',  ( 205.1049299651095623, 106.9023875785546096, -9.481380442157899324 ) ) ;
#12038 = FACE_BOUND ( 'NONE', #3398, .T. ) ;
#12039 = CARTESIAN_POINT ( 'NONE',  ( -58.76006735892197952, 15.70681061434692616, -49.24053391377918132 ) ) ;
#12040 = ORIENTED_EDGE ( 'NONE', *, *, #2084, .T. ) ;
#12041 = DIRECTION ( 'NONE',  ( -0.000000000000000000, 1.000000000000000000, -0.000000000000000000 ) ) ;
#12042 = FACE_OUTER_BOUND ( 'NONE', #65774, .T. ) ;
#12043 = CARTESIAN_POINT ( 'NONE',  ( -52.67596829228263289, 15.09584868440940220, 57.53187801079657504 ) ) ;
#12044 = CARTESIAN_POINT ( 'NONE',  ( -180.3161328724958139, 97.10341277064807741, 13.61587359508545880 ) ) ;
#12045 = CARTESIAN_POINT ( 'NONE',  ( 210.9631450001601252, 117.1791136960929833, 59.39267853008134068 ) ) ;
#12046 = DIRECTION ( 'NONE',  ( -1.000000000000000000, 0.000000000000000000, 0.000000000000000000 ) ) ;
#12047 = VECTOR ( 'NONE', #5888, 1000.000000000000000 ) ;
#12048 = ORIENTED_EDGE ( 'NONE', *, *, #6511, .T. ) ;
#12049 = CARTESIAN_POINT ( 'NONE',  ( 56.53635105806417016, 11.26263375223564012, 6.682842904946032725 ) ) ;
#12050 = CARTESIAN_POINT ( 'NONE',  ( 0.000000000000000000, 0.000000000000000000, 0.000000000000000000 ) ) ;
#12051 = ORIENTED_EDGE ( 'NONE', *, *, #38853, .F. ) ;
#12052 = VECTOR ( 'NONE', #17020, 1000.000000000000000 ) ;
#12053 = ORIENTED_EDGE ( 'NONE', *, *, #58139, .T. ) ;
#12054 = EDGE_CURVE ( 'NONE', #44813, #11517, #5594, .T. ) ;
#12055 = CARTESIAN_POINT ( 'NONE',  ( 410.0000000000000000, 0.000000000000000000, -90.00000000000000000 ) ) ;
#12056 = CARTESIAN_POINT ( 'NONE',  ( -56.72676045871359918, 16.18052435693491375, -23.18658342442263987 ) ) ;
#12057 = CARTESIAN_POINT ( 'NONE',  ( 104.7147873368644753, 26.40702926859708910, 42.20357219318257336 ) ) ;
#12058 = APPLICATION_CONTEXT ( 'automotive_design' ) ;
#12059 = VERTEX_POINT ( 'NONE', #48832 ) ;
#12060 = AXIS2_PLACEMENT_3D ( 'NONE', #26984, #27675, #49116 ) ;
#12061 = ORIENTED_EDGE ( 'NONE', *, *, #57323, .T. ) ;
#12062 = LINE ( 'NONE', #33534, #26268 ) ;
#12063 = CARTESIAN_POINT ( 'NONE',  ( 164.1352994389932292, 64.33767534192701021, 33.45996833887929967 ) ) ;
#12064 = VECTOR ( 'NONE', #26160, 1000.000000000000000 ) ;
#12065 = CARTESIAN_POINT ( 'NONE',  ( -151.6797345123118248, 67.37848486615943955, -61.96523196077820472 ) ) ;
#12066 = CARTESIAN_POINT ( 'NONE',  ( 69.48877314113909165, 15.30784187978993138, 14.26448168032291086 ) ) ;
#12067 = CARTESIAN_POINT ( 'NONE',  ( 5.355005115540897975, 6.145890662064648069, -9.417753204360288066 ) ) ;
#12068 = AXIS2_PLACEMENT_3D ( 'NONE', #11985, #37667, #27812 ) ;
#12069 = EDGE_CURVE ( 'NONE', #41387, #22570, #36934, .T. ) ;
#12070 = CARTESIAN_POINT ( 'NONE',  ( -49.12372073857199695, 14.20664392157176437, -47.33574279618618164 ) ) ;
#12071 = AXIS2_PLACEMENT_3D ( 'NONE', #4718, #63816, #37077 ) ;
#12072 = DIRECTION ( 'NONE',  ( -0.000000000000000000, 1.000000000000000000, -0.000000000000000000 ) ) ;
#12073 = CARTESIAN_POINT ( 'NONE',  ( -133.1640943168118838, 52.70734926280010058, -13.70763724439404108 ) ) ;
#12074 = EDGE_CURVE ( 'NONE', #33561, #54282, #62412, .T. ) ;
#12075 = CARTESIAN_POINT ( 'NONE',  ( -36.11269837220806522, 5.594483210025202879E-14, 85.00100000000000477 ) ) ;
#12076 = CARTESIAN_POINT ( 'NONE',  ( 149.0250918491436778, 6.000000000000000000, -9.435653166495526989 ) ) ;
#12077 = EDGE_CURVE ( 'NONE', #52163, #34907, #60800, .T. ) ;
#12078 = DIRECTION ( 'NONE',  ( -0.000000000000000000, 1.000000000000000000, -0.000000000000000000 ) ) ;
#12080 = ORIENTED_EDGE ( 'NONE', *, *, #37816, .F. ) ;
#12079 = FACE_OUTER_BOUND ( 'NONE', #60763, .T. ) ;
#12081 = VERTEX_POINT ( 'NONE', #17185 ) ;
#12082 = ADVANCED_FACE ( 'NONE', ( #56222 ), #51347, .T. ) ;
#12083 = EDGE_LOOP ( 'NONE', ( #52099, #51515 ) ) ;
#12084 = CARTESIAN_POINT ( 'NONE',  ( -14.19447842053093645, 7.389800932646227061, -12.10543927043131518 ) ) ;
#12085 = CARTESIAN_POINT ( 'NONE',  ( -165.7123887345808555, 80.68215826500505727, 90.82995548501529015 ) ) ;
#12086 = CARTESIAN_POINT ( 'NONE',  ( -48.57297291660696459, 13.03920345822338511, -19.68077099140970532 ) ) ;
#12087 = CARTESIAN_POINT ( 'NONE',  ( 105.8203563788591026, 26.88901185006195860, -10.51577773048208364 ) ) ;
#12088 = CARTESIAN_POINT ( 'NONE',  ( -31.43908319763709969, 10.61114334766715928, 72.06100499665289760 ) ) ;
#12089 = CARTESIAN_POINT ( 'NONE',  ( -4.164416015345870470, 64.86646004871185767, 73.58025477438755502 ) ) ;
#12090 = CARTESIAN_POINT ( 'NONE',  ( -71.43874587651173158, 19.69883891272895227, -71.47845090063621853 ) ) ;
#12091 = CARTESIAN_POINT ( 'NONE',  ( 6.590627171038061505, 57.96611128877285779, 27.58472369369409094 ) ) ;
#12092 = VERTEX_POINT ( 'NONE', #18597 ) ;
#12093 = DIRECTION ( 'NONE',  ( 0.9959742939952397345, -0.08963930890342655666, 0.000000000000000000 ) ) ;
#12094 = VERTEX_POINT ( 'NONE', #40053 ) ;
#12095 = VERTEX_POINT ( 'NONE', #55886 ) ;
#12096 = CARTESIAN_POINT ( 'NONE',  ( 65.40383840050409958, 14.27443447873231186, -23.50236838888156043 ) ) ;
#12097 = FILL_AREA_STYLE_COLOUR ( '', #43955 ) ;
#12098 = CARTESIAN_POINT ( 'NONE',  ( 50.97490815085634352, 6.000000000000000000, -41.68900338898716740 ) ) ;
#12099 = CARTESIAN_POINT ( 'NONE',  ( -94.85061234775061223, 29.16417548023186157, -43.57258393726064583 ) ) ;
#12100 = EDGE_CURVE ( 'NONE', #2893, #44947, #27719, .T. ) ;
#12102 = DIRECTION ( 'NONE',  ( 1.000000000000000000, 0.000000000000000000, 0.000000000000000000 ) ) ;
#12101 = AXIS2_PLACEMENT_3D ( 'NONE', #31864, #64208, #26585 ) ;
#12103 = DIRECTION ( 'NONE',  ( 0.000000000000000000, -0.000000000000000000, -1.000000000000000000 ) ) ;
#12104 = EDGE_CURVE ( 'NONE', #4696, #34928, #66806, .T. ) ;
#12105 = LINE ( 'NONE', #18080, #19464 ) ;
#12106 = ORIENTED_EDGE ( 'NONE', *, *, #38790, .F. ) ;
#12107 = B_SPLINE_CURVE_WITH_KNOTS ( 'NONE', 3,
 ( #24105, #41651, #2994, #24792, #50822, #62769 ),
 .UNSPECIFIED., .F., .F.,
 ( 4, 2, 4 ),
 ( 2.380731630023936087E-07, 0.002336973833157593699, 0.004673709593152186939 ),
 .UNSPECIFIED. ) ;
#12108 = VERTEX_POINT ( 'NONE', #61509 ) ;
#12109 = ORIENTED_EDGE ( 'NONE', *, *, #39188, .T. ) ;
#12110 = VECTOR ( 'NONE', #66719, 1000.000000000000000 ) ;
#12111 = DIRECTION ( 'NONE',  ( -0.000000000000000000, -0.000000000000000000, -1.000000000000000000 ) ) ;
#12112 = CARTESIAN_POINT ( 'NONE',  ( -15.27748264047829529, 7.491388194171917370, 11.75137412820307858 ) ) ;
#12113 = CARTESIAN_POINT ( 'NONE',  ( -190.6985136298601731, 109.1272424661242582, 94.99999999999866418 ) ) ;
#12114 = CARTESIAN_POINT ( 'NONE',  ( 57.39083379741710900, 11.43779987330584191, -21.36185840037164496 ) ) ;
#12115 = AXIS2_PLACEMENT_3D ( 'NONE', #67006, #8601, #3312 ) ;
#12116 = UNCERTAINTY_MEASURE_WITH_UNIT (LENGTH_MEASURE( 1.000000000000000082E-05 ), #53269, 'distance_accuracy_value', 'NONE');
#12117 = DIRECTION ( 'NONE',  ( -1.000000000000000000, 0.000000000000000000, 0.000000000000000000 ) ) ;
#12118 = CARTESIAN_POINT ( 'NONE',  ( -36.84489839129339828, 53.54860840895182150, 40.00000000000003553 ) ) ;
#12119 = ORIENTED_EDGE ( 'NONE', *, *, #35751, .T. ) ;
#12120 = CIRCLE ( 'NONE', #63789, 24.99999999999985434 ) ;
#12121 = DIRECTION ( 'NONE',  ( -0.000000000000000000, 1.000000000000000000, -0.000000000000000000 ) ) ;
#12122 = CARTESIAN_POINT ( 'NONE',  ( -155.5978531700835958, 69.52241200678679434, 69.44947247927566991 ) ) ;
#12123 = CARTESIAN_POINT ( 'NONE',  ( -4.506365319453816909, 7.705038994660847962, -49.64818903867375610 ) ) ;
#12124 = DIRECTION ( 'NONE',  ( 0.000000000000000000, 0.000000000000000000, 1.000000000000000000 ) ) ;
#12125 = CARTESIAN_POINT ( 'NONE',  ( -165.8758279540429896, 79.40953312850696477, -93.88874443287481597 ) ) ;
#12126 = DIRECTION ( 'NONE',  ( 1.000000000000000000, 0.000000000000000000, 0.000000000000000000 ) ) ;
#12127 = FACE_BOUND ( 'NONE', #65489, .T. ) ;
#12128 = DIRECTION ( 'NONE',  ( -0.000000000000000000, 1.000000000000000000, -0.000000000000000000 ) ) ;
#12129 = VECTOR ( 'NONE', #38920, 1000.000000000000000 ) ;
#12130 = ORIENTED_EDGE ( 'NONE', *, *, #9343, .F. ) ;
#12131 = CARTESIAN_POINT ( 'NONE',  ( -20.63749999999999574, 0.000000000000000000, 0.000000000000000000 ) ) ;
#12132 = CARTESIAN_POINT ( 'NONE',  ( -130.1964689553233256, 49.39217932424207902, -63.09757955249121864 ) ) ;
#12133 = CARTESIAN_POINT ( 'NONE',  ( -102.7447593990059005, 34.14748189312171434, -76.85912785543963821 ) ) ;
#12134 = CARTESIAN_POINT ( 'NONE',  ( 0.000000000000000000, 0.000000000000000000, 0.000000000000000000 ) ) ;
#12135 = CARTESIAN_POINT ( 'NONE',  ( -19.56458807131854627, 15.75959024859389324, 0.000000000000000000 ) ) ;
#12136 = VERTEX_POINT ( 'NONE', #29490 ) ;
#12137 = PRODUCT_RELATED_PRODUCT_CATEGORY ( 'part', '', ( #36034 ) ) ;
#12138 = ORIENTED_EDGE ( 'NONE', *, *, #17286, .T. ) ;
#12139 = LINE ( 'NONE', #49745, #23570 ) ;
#12140 = EDGE_CURVE ( 'NONE', #60658, #57264, #39705, .T. ) ;
#12141 = CARTESIAN_POINT ( 'NONE',  ( 186.5227155285546417, 84.28235524483832819, 85.32269636523660949 ) ) ;
#12142 = ORIENTED_EDGE ( 'NONE', *, *, #7636, .F. ) ;
#12143 = VERTEX_POINT ( 'NONE', #65753 ) ;
#12144 = EDGE_CURVE ( 'NONE', #41500, #34341, #36731, .T. ) ;
#12145 = CARTESIAN_POINT ( 'NONE',  ( 178.4027079424739952, 75.93756746109791322, -36.71741922764324784 ) ) ;
#12146 = CARTESIAN_POINT ( 'NONE',  ( 162.0862735437575282, 62.63196145447161456, 4.134242840469689817 ) ) ;
#12147 = DIRECTION ( 'NONE',  ( -1.000000000000000000, 0.000000000000000000, 0.000000000000000000 ) ) ;
#12148 = EDGE_LOOP ( 'NONE', ( #3835, #10275 ) ) ;
#12149 = CARTESIAN_POINT ( 'NONE',  ( -78.66644367742111399, -170.0000000000000000, -15.77090004125421352 ) ) ;
#12150 = CARTESIAN_POINT ( 'NONE',  ( -72.62976060914745347, 18.74780984163036024, 170.0000000000000000 ) ) ;
#12151 = CARTESIAN_POINT ( 'NONE',  ( -71.56718866013696356, 19.74312628447964357, -40.14419485704286927 ) ) ;
#12152 = FACE_OUTER_BOUND ( 'NONE', #3705, .T. ) ;
#12153 = CARTESIAN_POINT ( 'NONE',  ( 92.21267147730743829, 21.40196534721315302, -38.29018140383976032 ) ) ;
#12154 = CARTESIAN_POINT ( 'NONE',  ( -47.79955240516188297, 13.88975739862081937, -17.84404308398329064 ) ) ;
#12155 = EDGE_CURVE ( 'NONE', #9288, #3940, #6645, .T. ) ;
#12156 = ORIENTED_EDGE ( 'NONE', *, *, #53282, .F. ) ;
#12157 = CARTESIAN_POINT ( 'NONE',  ( 8.000000000000003553, -4.618802153517020948, -0.7145311798163346273 ) ) ;
#12158 = DIRECTION ( 'NONE',  ( 0.000000000000000000, 0.000000000000000000, 1.000000000000000000 ) ) ;
#12159 = EDGE_CURVE ( 'NONE', #14540, #43079, #56548, .T. ) ;
#12160 = CARTESIAN_POINT ( 'NONE',  ( -29.68020330876228385, 0.000000000000000000, 4.368699068434031219 ) ) ;
#12161 = VECTOR ( 'NONE', #62752, 1000.000000000000000 ) ;
#12162 = EDGE_CURVE ( 'NONE', #59386, #13106, #39256, .T. ) ;
#12163 = CARTESIAN_POINT ( 'NONE',  ( 150.3360255159550150, -170.0000000000000000, -95.00000000000133582 ) ) ;
#12165 = ORIENTED_EDGE ( 'NONE', *, *, #42088, .T. ) ;
#12164 = LINE ( 'NONE', #39588, #30963 ) ;
#12166 = DIRECTION ( 'NONE',  ( -0.8160245890732938934, -0.5780171883497599028, 0.000000000000000000 ) ) ;
#12167 = AXIS2_PLACEMENT_3D ( 'NONE', #7759, #65812, #33789 ) ;
#12168 = ORIENTED_EDGE ( 'NONE', *, *, #47153, .T. ) ;
#12169 = LINE ( 'NONE', #17796, #15529 ) ;
#12170 = CYLINDRICAL_SURFACE ( 'NONE', #35634, 7.500000000000020428 ) ;
#12171 = CARTESIAN_POINT ( 'NONE',  ( 4.000000000000011546, -6.928203230275505220, -9.500000000000000000 ) ) ;
#12172 = CYLINDRICAL_SURFACE ( 'NONE', #65307, 23.97499999999999787 ) ;
#12173 = CARTESIAN_POINT ( 'NONE',  ( -119.6995109608660925, 42.54844499216733311, 60.72834450685288488 ) ) ;
#12174 = AXIS2_PLACEMENT_3D ( 'NONE', #16240, #54557, #17276 ) ;
#12175 = CARTESIAN_POINT ( 'NONE',  ( 40.38495044702527537, 9.554194848483444247, 3.117968398919370276 ) ) ;
#12176 = CARTESIAN_POINT ( 'NONE',  ( 94.06703982324145841, 22.09435144471460433, -69.16872801670120907 ) ) ;
#12177 = DIRECTION ( 'NONE',  ( 1.000000000000000000, 0.000000000000000000, 0.000000000000000000 ) ) ;
#12178 = DIRECTION ( 'NONE',  ( 0.000000000000000000, 0.000000000000000000, -1.000000000000000000 ) ) ;
#12179 = ORIENTED_EDGE ( 'NONE', *, *, #50604, .F. ) ;
#12180 = ORIENTED_EDGE ( 'NONE', *, *, #21909, .F. ) ;
#12181 = CARTESIAN_POINT ( 'NONE',  ( 43.14712943604301643, 8.926114770663669873, 43.91642105177349720 ) ) ;
#12182 = CARTESIAN_POINT ( 'NONE',  ( 201.5903370237274430, 102.1785392640257726, -23.82087321366149979 ) ) ;
#12183 = LINE ( 'NONE', #23085, #26681 ) ;
#12184 = LINE ( 'NONE', #39608, #26178 ) ;
#12185 = CARTESIAN_POINT ( 'NONE',  ( 211.8382652195006983, 118.5282575235990237, -41.50942527998029163 ) ) ;
#12186 = DIRECTION ( 'NONE',  ( 1.000000000000000000, 0.000000000000000000, -0.000000000000000000 ) ) ;
#12187 = CARTESIAN_POINT ( 'NONE',  ( -109.3553681454883844, 36.52260784104394276, 62.32349516983876470 ) ) ;
#12188 = CARTESIAN_POINT ( 'NONE',  ( -25.80058235236790409, 8.733375263008339218, -37.84754545538757498 ) ) ;
#12189 = EDGE_CURVE ( 'NONE', #18870, #67789, #45680, .T. ) ;
#12190 = FACE_OUTER_BOUND ( 'NONE', #62376, .T. ) ;
#12191 = EDGE_LOOP ( 'NONE', ( #9539, #10424, #53606, #20953 ) ) ;
#12192 = CARTESIAN_POINT ( 'NONE',  ( -23.99957301099517792, 9.503061049698493079, 9.889415725718228245 ) ) ;
#12193 = ORIENTED_EDGE ( 'NONE', *, *, #16765, .F. ) ;
#12194 = DIRECTION ( 'NONE',  ( 0.000000000000000000, 0.000000000000000000, 1.000000000000000000 ) ) ;
#12195 = DIRECTION ( 'NONE',  ( 0.000000000000000000, -1.000000000000000000, 0.000000000000000000 ) ) ;
#12196 = DIRECTION ( 'NONE',  ( 1.000000000000000000, 0.000000000000000000, 0.000000000000000000 ) ) ;
#12197 = CARTESIAN_POINT ( 'NONE',  ( 128.3889472838589256, 39.37765603157610173, 42.16720712859076770 ) ) ;
#12198 = LINE ( 'NONE', #49457, #14178 ) ;
#12199 = FACE_OUTER_BOUND ( 'NONE', #3317, .T. ) ;
#12200 = DIRECTION ( 'NONE',  ( -0.5000000000000012212, -0.8660254037844380415, 0.000000000000000000 ) ) ;
#12201 = CARTESIAN_POINT ( 'NONE',  ( 6.400000000000000355, 4.618802153517001408, -8.000000000000000000 ) ) ;
#12202 = CARTESIAN_POINT ( 'NONE',  ( 210.5879448407857808, 114.7852148663112359, 85.74156794298586703 ) ) ;
#12203 = PLANE ( 'NONE',  #14036 ) ;
#12204 = ORIENTED_EDGE ( 'NONE', *, *, #5483, .T. ) ;
#12205 = LINE ( 'NONE', #951, #39649 ) ;
#12206 = DIRECTION ( 'NONE',  ( -0.6427876096865403621, 0.7660444431189770143, -5.360859406683936151E-17 ) ) ;
#12207 = CARTESIAN_POINT ( 'NONE',  ( -15.07235766390728848, 8.482541916553470784, 8.823573041229387570 ) ) ;
#12208 = CYLINDRICAL_SURFACE ( 'NONE', #56816, 5.000000000000170530 ) ;
#12209 = CARTESIAN_POINT ( 'NONE',  ( -103.2129897037410871, 33.25684593987698889, -61.90293558496989590 ) ) ;
#12210 = CARTESIAN_POINT ( 'NONE',  ( 126.4633682455861816, 38.28837286275646079, -15.39085948919035829 ) ) ;
#12211 = AXIS2_PLACEMENT_3D ( 'NONE', #6861, #65977, #55386 ) ;
#12212 = ORIENTED_EDGE ( 'NONE', *, *, #20251, .F. ) ;
#12213 = DIRECTION ( 'NONE',  ( 1.000000000000000000, 0.000000000000000000, 0.000000000000000000 ) ) ;
#12214 = FACE_OUTER_BOUND ( 'NONE', #69097, .T. ) ;
#12215 = DIRECTION ( 'NONE',  ( 0.000000000000000000, 0.000000000000000000, -1.000000000000000000 ) ) ;
#12216 = CARTESIAN_POINT ( 'NONE',  ( -165.6397095829521788, 80.60756690931943069, -42.82113700829442138 ) ) ;
#12217 = EDGE_CURVE ( 'NONE', #22100, #56047, #13186, .T. ) ;
#12218 = VECTOR ( 'NONE', #7687, 1000.000000000000227 ) ;
#12219 = CARTESIAN_POINT ( 'NONE',  ( -165.6438506416219241, 79.17342941146682733, 91.39850628321933357 ) ) ;
#12220 = VERTEX_POINT ( 'NONE', #46353 ) ;
#12221 = DIRECTION ( 'NONE',  ( -1.000000000000000000, 0.000000000000000000, 0.000000000000000000 ) ) ;
#12222 = CARTESIAN_POINT ( 'NONE',  ( 46.39999999999999858, 0.000000000000000000, 4.171999999999999709 ) ) ;
#12223 = ADVANCED_FACE ( 'NONE', ( #67155 ), #52333, .F. ) ;
#12224 = CARTESIAN_POINT ( 'NONE',  ( 44.99999999999999289, 20.00000000000000355, 4.000000000000000000 ) ) ;
#12225 = EDGE_CURVE ( 'NONE', #49213, #30161, #52668, .T. ) ;
#12226 = CARTESIAN_POINT ( 'NONE',  ( -0.8863172752569257185, 7.545240277686259489, -66.88547064642474993 ) ) ;
#12227 = EDGE_CURVE ( 'NONE', #27706, #49790, #6392, .T. ) ;
#12228 = LINE ( 'NONE', #39652, #2126 ) ;
#12229 = VERTEX_POINT ( 'NONE', #30199 ) ;
#12230 = CARTESIAN_POINT ( 'NONE',  ( 6.400000000000000355, -4.618802153517016507, -8.000000000000000000 ) ) ;
#12231 = CARTESIAN_POINT ( 'NONE',  ( 197.3054165770396935, 96.72615186924558373, -45.13381048724120603 ) ) ;
#12232 = EDGE_CURVE ( 'NONE', #27095, #56869, #26641, .T. ) ;
#12233 = CARTESIAN_POINT ( 'NONE',  ( -95.05323930133205579, 30.36974142673411947, 40.08974556234316822 ) ) ;
#12234 = CARTESIAN_POINT ( 'NONE',  ( 23.28785143291466042, 6.856621069835718174, -43.52013114503547087 ) ) ;
#12236 = ORIENTED_EDGE ( 'NONE', *, *, #32185, .F. ) ;
#12235 = CARTESIAN_POINT ( 'NONE',  ( 116.8917656767876423, 33.20682060519247614, 13.74620126077677007 ) ) ;
#12237 = B_SPLINE_CURVE_WITH_KNOTS ( 'NONE', 3,
 ( #57820, #31096, #64469, #47930, #58486, #11000, #52193, #4011, #25477, #46916, #52534, #47247, #9979, #68380, #4688, #20181, #41639, #63093, #14897, #68706, #41980, #21222, #15254, #42668, #36714, #60930, #27878, #50030, #16622, #66236, #18026, #38793, #28216, #48608, #44761, #16960, #22257, #53895, #49317, #28576, #59874, #446, #38079, #32809, #49665, #5717, #17318 ),
 .UNSPECIFIED., .F., .F.,
 ( 4, 2, 2, 2, 2, 2, 2, 2, 2, 2, 2, 2, 1, 2, 2, 2, 2, 2, 2, 2, 2, 2, 2, 4 ),
 ( 0.000000000000000000, 0.001493793014771585851, 0.002240689522157379536, 0.002987586029543173004, 0.004481379044314756470, 0.005228275551700559479, 0.005975172059086361620, 0.007468965073857955494, 0.008215861581243747228, 0.008962758088629538961, 0.01045655110340111375, 0.01120344761078690202, 0.01195034411817268681, 0.01269724062555847161, 0.01344413713294425813, 0.01493793014771582772, 0.01568482665510160037, 0.01643172316248737302, 0.01792551617725893220, 0.01941930919203049138, 0.02016620569941626404, 0.02091310220680203669, 0.02240689522157357505, 0.02390068823634511341 ),
 .UNSPECIFIED. ) ;
#12238 = CARTESIAN_POINT ( 'NONE',  ( 181.0840389613909736, 80.03940679743415387, 71.15314469597512925 ) ) ;
#12239 = EDGE_LOOP ( 'NONE', ( #21012, #18495, #11733, #34173 ) ) ;
#12240 = EDGE_LOOP ( 'NONE', ( #41352, #43715, #51214, #45345 ) ) ;
#12241 = CARTESIAN_POINT ( 'NONE',  ( 180.2565361171340612, 79.19912802278402353, 29.34240539128484215 ) ) ;
#12242 = EDGE_CURVE ( 'NONE', #58547, #40273, #69531, .T. ) ;
#12243 = LINE ( 'NONE', #23146, #31562 ) ;
#12245 = ORIENTED_EDGE ( 'NONE', *, *, #42965, .T. ) ;
#12244 = CARTESIAN_POINT ( 'NONE',  ( -12.40598104375063393, 8.242193636955557068, -63.80355163731987744 ) ) ;
#12246 = CARTESIAN_POINT ( 'NONE',  ( 161.7048274740121201, 61.01946783654762640, 30.70182928664277355 ) ) ;
#12247 = DIRECTION ( 'NONE',  ( 0.000000000000000000, -1.000000000000000000, 0.000000000000000000 ) ) ;
#12248 = CARTESIAN_POINT ( 'NONE',  ( -78.18897186942400879, 23.21604822208488983, -35.11545063171787007 ) ) ;
#12249 = ORIENTED_EDGE ( 'NONE', *, *, #63682, .T. ) ;
#12250 = B_SPLINE_CURVE_WITH_KNOTS ( 'NONE', 3,
 ( #47252, #43696, #65528, #22604, #11006, #54954, #33530, #5722, #22263, #16967, #65174, #12057, #38438, #43354, #6775, #27884, #16628, #54605, #1500, #65892, #5393, #17324, #6433, #11344, #6066, #59879, #49671, #11697, #26846, #38799, #32469, #64828, #32815, #53900, #48273, #54245, #39151, #38084, #33171, #64475, #27528, #22960, #17687, #48969 ),
 .UNSPECIFIED., .F., .F.,
 ( 4, 2, 2, 2, 2, 2, 2, 2, 2, 2, 2, 2, 2, 2, 2, 2, 2, 2, 2, 2, 2, 4 ),
 ( 0.000000000000000000, 0.001533942663855609968, 0.003067885327711219936, 0.004601827991566829687, 0.005368799323494632611, 0.006135770655422436402, 0.007669713319278056995, 0.008436684651205868593, 0.009203655983133680191, 0.01073759864698928777, 0.01150456997891710111, 0.01227154131084491617, 0.01303851264277272777, 0.01380548397470054110, 0.01533942663855617124, 0.01687336930241179617, 0.01840731196626742283, 0.01994125463012304950, 0.02070822596205086283, 0.02147519729397867616, 0.02300913995783434099, 0.02454308262169000582 ),
 .UNSPECIFIED. ) ;
#12251 = CARTESIAN_POINT ( 'NONE',  ( 5.000000000000000888, 6.123233995736767268E-16, -9.474599999999998801 ) ) ;
#12252 = CARTESIAN_POINT ( 'NONE',  ( -37.07602570886410831, 10.58457435034602589, -20.94455602913923187 ) ) ;
#12253 = CARTESIAN_POINT ( 'NONE',  ( 150.3360255159550150, 52.31024849487489803, -95.00000000000133582 ) ) ;
#12254 = CARTESIAN_POINT ( 'NONE',  ( -126.7944042662568478, 48.29830493043728268, 3.815832165402863296 ) ) ;
#12255 = CARTESIAN_POINT ( 'NONE',  ( 22.15943197741200876, 7.796127622097904109, 60.39464998070587853 ) ) ;
#12256 = ORIENTED_EDGE ( 'NONE', *, *, #9008, .T. ) ;
#12257 = VECTOR ( 'NONE', #61557, 1000.000000000000000 ) ;
#12258 = ORIENTED_EDGE ( 'NONE', *, *, #31652, .F. ) ;
#12259 = ORIENTED_EDGE ( 'NONE', *, *, #4218, .F. ) ;
#12260 = CARTESIAN_POINT ( 'NONE',  ( 45.78444578632068840, -59.41672343742509810, 43.58025477438756212 ) ) ;
#12261 = COLOUR_RGB ( '',0.7921568627450980005, 0.8196078431372548767, 0.9333333333333333481 ) ;
#12262 = CARTESIAN_POINT ( 'NONE',  ( -106.4728934171453716, 36.10295170132727094, 4.951394827835590817 ) ) ;
#12263 = DIRECTION ( 'NONE',  ( -0.000000000000000000, 1.000000000000000000, -0.000000000000000000 ) ) ;
#12264 = CARTESIAN_POINT ( 'NONE',  ( -95.10076455013715702, 29.28088892350594108, 89.51400794333316924 ) ) ;
#12265 = CARTESIAN_POINT ( 'NONE',  ( 8.828807734113986783, 74.48902371486718721, 43.58025477438756923 ) ) ;
#12266 = CARTESIAN_POINT ( 'NONE',  ( -128.7810612886105446, 48.42424427998344072, 58.03872734881966977 ) ) ;
#12267 = CARTESIAN_POINT ( 'NONE',  ( -73.09214866197368110, 21.34321757515764162, -20.81301429235548994 ) ) ;
#12268 = ORIENTED_EDGE ( 'NONE', *, *, #2084, .F. ) ;
#12269 = CARTESIAN_POINT ( 'NONE',  ( 79.19132716134490124, 17.01584750883626995, 63.06170514846407116 ) ) ;
#12270 = ORIENTED_EDGE ( 'NONE', *, *, #30171, .T. ) ;
#12271 = CARTESIAN_POINT ( 'NONE',  ( 33.76124497394584267, 7.742545529019359662, 42.38094193253945008 ) ) ;
#12272 = ORIENTED_EDGE ( 'NONE', *, *, #38557, .T. ) ;
#12273 = CARTESIAN_POINT ( 'NONE',  ( -36.11269837220804391, 20.55634918610408945, 0.000000000000000000 ) ) ;
#12274 = PLANE ( 'NONE',  #28789 ) ;
#12275 = CARTESIAN_POINT ( 'NONE',  ( 329.1355598199468204, 190.0000000000000000, -129.5087625010780812 ) ) ;
#12276 = CARTESIAN_POINT ( 'NONE',  ( 0.000000000000000000, 0.000000000000000000, -5.000000000000000000 ) ) ;
#12277 = DIRECTION ( 'NONE',  ( -0.000000000000000000, -0.000000000000000000, 1.000000000000000000 ) ) ;
#12278 = CARTESIAN_POINT ( 'NONE',  ( 149.9872551245001375, 52.05943539582081314, -43.04961227817129554 ) ) ;
#12279 = PLANE ( 'NONE',  #68177 ) ;
#12280 = ORIENTED_EDGE ( 'NONE', *, *, #25736, .F. ) ;
#12281 = EDGE_CURVE ( 'NONE', #9081, #43408, #15395, .T. ) ;
#12282 = CARTESIAN_POINT ( 'NONE',  ( -31.11269837220806878, 5.000000000000056843, 2.000000000000001776 ) ) ;
#12283 = CARTESIAN_POINT ( 'NONE',  ( -189.8133172329396814, 108.7279284458360564, 94.99999999999866418 ) ) ;
#12284 = ORIENTED_EDGE ( 'NONE', *, *, #8092, .F. ) ;
#12285 = DIRECTION ( 'NONE',  ( -1.850169831522831466E-16, 1.000000000000000000, 1.110223024625156294E-16 ) ) ;
#12286 = CARTESIAN_POINT ( 'NONE',  ( 110.2429982417149574, -170.0000000000000000, -77.76698815611739235 ) ) ;
#12287 = ORIENTED_EDGE ( 'NONE', *, *, #27947, .F. ) ;
#12288 = CARTESIAN_POINT ( 'NONE',  ( -81.67992981004164221, 23.49232121719083111, 31.04606863069344769 ) ) ;
#12289 = CARTESIAN_POINT ( 'NONE',  ( 150.2193536046551401, 53.46717047532149536, -72.40446139084801302 ) ) ;
#12290 = CARTESIAN_POINT ( 'NONE',  ( 42.71680114082826663, 9.880016734137544887, 44.15935619967898873 ) ) ;
#12291 = FACE_OUTER_BOUND ( 'NONE', #11225, .T. ) ;
#12292 = B_SPLINE_CURVE_WITH_KNOTS ( 'NONE', 3,
 ( #10539, #9874, #30985, #52082, #4582, #53444 ),
 .UNSPECIFIED., .F., .F.,
 ( 4, 2, 4 ),
 ( 1.095770181107970753E-06, 0.03239442681617710901, 0.06478775786217311206 ),
 .UNSPECIFIED. ) ;
#12293 = ORIENTED_EDGE ( 'NONE', *, *, #16445, .T. ) ;
#12294 = ORIENTED_EDGE ( 'NONE', *, *, #61559, .T. ) ;
#12295 = AXIS2_PLACEMENT_3D ( 'NONE', #53675, #32581, #15711 ) ;
#12296 = CARTESIAN_POINT ( 'NONE',  ( 181.0840389613909736, -170.0000000000000000, -24.38050707541595230 ) ) ;
#12297 = ORIENTED_EDGE ( 'NONE', *, *, #62855, .T. ) ;
#12298 = CARTESIAN_POINT ( 'NONE',  ( 32.37980458033285203, 8.611076697115699119, -13.62945249871878772 ) ) ;
#12299 = CARTESIAN_POINT ( 'NONE',  ( 429.8372781065087338, 400.0000000000066507, 91.05029585798857283 ) ) ;
#12300 = SURFACE_STYLE_FILL_AREA ( #1752 ) ;
#12301 = CARTESIAN_POINT ( 'NONE',  ( -1.096061481932296022, 7.553048580900439291, 61.13948011263546789 ) ) ;
#12302 = CARTESIAN_POINT ( 'NONE',  ( 199.3120637967379025, 100.8716943732679141, -92.27816652752858317 ) ) ;
#12303 = ADVANCED_FACE ( 'NONE', ( #25954 ), #28273, .F. ) ;
#12304 = LINE ( 'NONE', #39385, #5830 ) ;
#12305 = ORIENTED_EDGE ( 'NONE', *, *, #28347, .T. ) ;
#12306 = B_SPLINE_CURVE_WITH_KNOTS ( 'NONE', 3,
 ( #62129, #35405, #20595, #56868, #9362, #47324, #46645, #57212, #4093, #24855, #25558, #19926, #3397, #58235, #46992, #41028, #30473, #51923, #10052, #68454, #3735, #68781, #67771, #68120, #42058, #30827, #8687, #63179, #67422, #52943, #20261, #46293, #14976, #36442, #41381, #62838, #57895, #14639, #36103, #9715, #31180, #4430, #25894, #63517, #26915, #32538, #63866, #42406 ),
 .UNSPECIFIED., .F., .F.,
 ( 4, 2, 2, 2, 2, 2, 2, 2, 2, 2, 2, 2, 2, 2, 2, 2, 2, 2, 2, 2, 2, 2, 2, 4 ),
 ( 0.000000000000000000, 0.003619254076116482609, 0.004524067595145613886, 0.005428881114174745164, 0.007238508152232934860, 0.008143321671262049657, 0.009048135190291161853, 0.01085776222834937237, 0.01176257574737846201, 0.01266738926640754818, 0.01357220278543663783, 0.01447701630446572574, 0.01538182982349481191, 0.01628664334252390156, 0.01719145686155298947, 0.01809627038058207738, 0.01900108389961116875, 0.01990589741864025666, 0.02171552445669843595, 0.02262033797572754468, 0.02352515149475665340, 0.02533477853281487086, 0.02714440557087308831, 0.02895403260893130923 ),
 .UNSPECIFIED. ) ;
#12307 = CARTESIAN_POINT ( 'NONE',  ( 0.000000000000000000, 0.000000000000000000, 40.00000000000003553 ) ) ;
#12308 = ORIENTED_EDGE ( 'NONE', *, *, #33768, .T. ) ;
#12309 = AXIS2_PLACEMENT_3D ( 'NONE', #47606, #10666, #43369 ) ;
#12310 = ORIENTED_EDGE ( 'NONE', *, *, #6159, .T. ) ;
#12311 = CARTESIAN_POINT ( 'NONE',  ( 160.5141379054754225, 60.05651755415397730, -9.910344286968784999 ) ) ;
#12312 = CYLINDRICAL_SURFACE ( 'NONE', #63138, 19.99999999999998934 ) ;
#12313 = DIRECTION ( 'NONE',  ( -1.000000000000000000, 0.000000000000000000, 0.000000000000000000 ) ) ;
#12314 = CARTESIAN_POINT ( 'NONE',  ( -132.7932380098740452, 52.44226555691696490, -93.12280453660946478 ) ) ;
#12315 = EDGE_CURVE ( 'NONE', #26262, #26264, #1108, .T. ) ;
#12316 = CARTESIAN_POINT ( 'NONE',  ( 10.18313842235669320, -65.86279891076495119, 34.48241823979989107 ) ) ;
#12317 = ORIENTED_EDGE ( 'NONE', *, *, #47261, .F. ) ;
#12318 = EDGE_LOOP ( 'NONE', ( #38470, #65477 ) ) ;
#12319 = CARTESIAN_POINT ( 'NONE',  ( 12.46277766093406569, 6.416700641561365437, 44.25508861672395966 ) ) ;
#12320 = ORIENTED_EDGE ( 'NONE', *, *, #50891, .T. ) ;
#12321 = CARTESIAN_POINT ( 'NONE',  ( 16.78635691501517613, 6.000000000000000000, -46.68900338898716029 ) ) ;
#12322 = ADVANCED_FACE ( 'NONE', ( #23010 ), #44462, .T. ) ;
#12323 = VERTEX_POINT ( 'NONE', #2951 ) ;
#12324 = CARTESIAN_POINT ( 'NONE',  ( -146.1260528621668300, 61.36307454672304118, -75.86784781446887393 ) ) ;
#12325 = VECTOR ( 'NONE', #37666, 1000.000000000000000 ) ;
#12326 = CARTESIAN_POINT ( 'NONE',  ( 93.32502112557682494, 21.81526022999040038, 6.952080423476055593 ) ) ;
#12327 = CARTESIAN_POINT ( 'NONE',  ( 417.3372781065086770, 0.000000000000000000, 113.5502958579881749 ) ) ;
#12328 = ORIENTED_EDGE ( 'NONE', *, *, #37731, .F. ) ;
#12329 = PLANE ( 'NONE',  #6444 ) ;
#12330 = B_SPLINE_CURVE_WITH_KNOTS ( 'NONE', 3,
 ( #34453, #44639, #61843, #55530, #2425, #17909, #29495, #18252, #29157, #66462, #23882, #24589, #66122, #18951, #50959, #13333, #45684, #46022, #55180, #67489, #13668, #39024, #39363, #35123 ),
 .UNSPECIFIED., .F., .F.,
 ( 4, 2, 2, 2, 2, 2, 2, 2, 2, 2, 2, 4 ),
 ( 0.01118858214005710207, 0.01260300539470554995, 0.01401742864935399957, 0.01543185190400244745, 0.01613906353132666879, 0.01684627515865088840, 0.01826069841329931720, 0.01896791004062353680, 0.01967512166794775641, 0.02108954492259615746, 0.02179675654992035971, 0.02250396817724456891 ),
 .UNSPECIFIED. ) ;
#12332 = DIRECTION ( 'NONE',  ( -0.000000000000000000, 1.000000000000000000, -0.000000000000000000 ) ) ;
#12331 =( BOUNDED_CURVE ( )  B_SPLINE_CURVE ( 3, ( #16395, #37495, #64233, #62248 ),
 .UNSPECIFIED., .F., .F. ) 
 B_SPLINE_CURVE_WITH_KNOTS ( ( 4, 4 ),
 ( 1.655128935956321114E-13, 1.570796326794890563 ),
 .UNSPECIFIED. ) 
 CURVE ( )  GEOMETRIC_REPRESENTATION_ITEM ( )  RATIONAL_B_SPLINE_CURVE ( ( 1.000000000000000000, 0.8047378541244054606, 0.8047378541244054606, 1.000000000000000000 ) ) 
 REPRESENTATION_ITEM ( '' )  );
#12333 = DIRECTION ( 'NONE',  ( -0.9959742939952397345, 0.08963930890342655666, 0.000000000000000000 ) ) ;
#12334 = DIRECTION ( 'NONE',  ( -0.000000000000000000, 1.000000000000000000, -0.000000000000000000 ) ) ;
#12335 = PLANE ( 'NONE',  #24693 ) ;
#12336 = CARTESIAN_POINT ( 'NONE',  ( -145.0695669462244553, 60.50477348111340348, -89.95188078407383614 ) ) ;
#12337 = CARTESIAN_POINT ( 'NONE',  ( 126.8015497489690091, 37.32461426945040728, -72.92606890101930617 ) ) ;
#12338 = ORIENTED_EDGE ( 'NONE', *, *, #2017, .F. ) ;
#12339 = CARTESIAN_POINT ( 'NONE',  ( 86.62931800182293784, -170.0000000000000000, 10.36753698201563267 ) ) ;
#12340 = CARTESIAN_POINT ( 'NONE',  ( -417.6627218934914367, 399.9999999999998863, -146.4497041420118251 ) ) ;
#12341 = EDGE_LOOP ( 'NONE', ( #58911, #42681, #58237, #62569 ) ) ;
#12342 = VECTOR ( 'NONE', #48912, 1000.000000000000000 ) ;
#12343 = CARTESIAN_POINT ( 'NONE',  ( -151.6797345123119101, 67.37848486615946797, -35.12068137031451442 ) ) ;
#12344 = CARTESIAN_POINT ( 'NONE',  ( 17.98081503251148661, 17.36923402935782690, 0.000000000000000000 ) ) ;
#12345 = CARTESIAN_POINT ( 'NONE',  ( -38.93938005333175312, 11.96888249046460828, 37.95614235521382085 ) ) ;
#12346 = CARTESIAN_POINT ( 'NONE',  ( -143.2498117110515068, 60.33382252735059126, -19.61078403914306989 ) ) ;
#12347 = CARTESIAN_POINT ( 'NONE',  ( -30.00000000000000355, 26.99999999999999645, 15.00000000000000000 ) ) ;
#12348 = CARTESIAN_POINT ( 'NONE',  ( 39.71871838048090808, 33.04133019307971608, 26.66469104408690782 ) ) ;
#12349 = CARTESIAN_POINT ( 'NONE',  ( -42.32797523529043104, -61.85511477251480983, 41.38025477438755928 ) ) ;
#12350 = DIRECTION ( 'NONE',  ( -0.000000000000000000, -0.000000000000000000, -1.000000000000000000 ) ) ;
#12351 = CARTESIAN_POINT ( 'NONE',  ( -2.172839205444460742, 7.595638683704371452, -21.02768760144151727 ) ) ;
#12352 = CARTESIAN_POINT ( 'NONE',  ( 58.32618493680805472, -1.250000000000021982, 27.58472315868180402 ) ) ;
#12353 = CARTESIAN_POINT ( 'NONE',  ( 117.3281529665582212, 32.29994712002883972, 12.77937192486413842 ) ) ;
#12354 = DIRECTION ( 'NONE',  ( 0.000000000000000000, 6.123233995736870806E-17, -1.000000000000000000 ) ) ;
#12355 = ORIENTED_EDGE ( 'NONE', *, *, #28194, .T. ) ;
#12356 = CARTESIAN_POINT ( 'NONE',  ( -95.20053778133915046, 30.43887292928078026, -45.04236790332991092 ) ) ;
#12357 = ORIENTED_EDGE ( 'NONE', *, *, #58353, .F. ) ;
#12358 = CARTESIAN_POINT ( 'NONE',  ( -40.13282190614798850, -1.847197903505587038E-12, -9.999999999999998224 ) ) ;
#12359 = DIRECTION ( 'NONE',  ( 0.000000000000000000, 0.000000000000000000, 1.000000000000000000 ) ) ;
#12360 = CARTESIAN_POINT ( 'NONE',  ( 114.2394011608742517, 31.89382501980991691, 84.44551190695648302 ) ) ;
#12361 = CARTESIAN_POINT ( 'NONE',  ( 0.000000000000000000, 0.000000000000000000, 2.000000000000000000 ) ) ;
#12362 = DIRECTION ( 'NONE',  ( 0.000000000000000000, 0.000000000000000000, 1.000000000000000000 ) ) ;
#12363 = VECTOR ( 'NONE', #69040, 999.9999999999998863 ) ;
#12364 = CARTESIAN_POINT ( 'NONE',  ( 8.000000000000007105, 249.8719672152120381, 94.99999999999866418 ) ) ;
#12365 = EDGE_CURVE ( 'NONE', #11740, #53513, #1919, .T. ) ;
#12366 = DIRECTION ( 'NONE',  ( 0.000000000000000000, 0.000000000000000000, -1.000000000000000000 ) ) ;
#12367 = CARTESIAN_POINT ( 'NONE',  ( 21.98745393275290994, -71.71550996510497100, 170.0000000000000000 ) ) ;
#12368 = ORIENTED_EDGE ( 'NONE', *, *, #23031, .T. ) ;
#12369 = VERTEX_POINT ( 'NONE', #18086 ) ;
#12370 = CARTESIAN_POINT ( 'NONE',  ( 31.11269837220806522, -6.375108774214766072E-14, 85.00100000000000477 ) ) ;
#12371 = CARTESIAN_POINT ( 'NONE',  ( -50.92620509423012720, -55.07344309828840068, 170.0000000000000000 ) ) ;
#12372 = FACE_OUTER_BOUND ( 'NONE', #13779, .T. ) ;
#12373 = EDGE_CURVE ( 'NONE', #38945, #39183, #25551, .T. ) ;
#12374 = CARTESIAN_POINT ( 'NONE',  ( -166.9992034932274976, 82.01285191063135471, 69.52895971928450081 ) ) ;
#12375 = CYLINDRICAL_SURFACE ( 'NONE', #57720, 7.500000000000027534 ) ;
#12376 = VECTOR ( 'NONE', #36580, 1000.000000000000000 ) ;
#12377 = CARTESIAN_POINT ( 'NONE',  ( 0.000000000000000000, 0.000000000000000000, -2.500000000000002220 ) ) ;
#12378 = ORIENTED_EDGE ( 'NONE', *, *, #52356, .F. ) ;
#12379 = CARTESIAN_POINT ( 'NONE',  ( 93.43270425363544973, 22.93046121381056324, 7.201044160860008425 ) ) ;
#12380 = B_SPLINE_CURVE_WITH_KNOTS ( 'NONE', 3,
 ( #42387, #41363, #35742, #57539, #19907, #20239, #63850, #9696, #15658, #10366, #53267, #62816, #47992, #62466, #51905, #36082, #53617, #6491, #38859, #5778, #15993, #27236, #11395, #43756, #65228, #32520, #864, #17379, #27937, #54302, #38492, #55010, #16687, #64532, #156, #49380, #6832, #16342, #43409, #28285, #49727, #48669, #48323, #21276, #22317, #59579, #21614, #22663 ),
 .UNSPECIFIED., .F., .F.,
 ( 4, 2, 2, 2, 2, 2, 2, 2, 2, 2, 2, 2, 2, 2, 2, 2, 2, 2, 2, 2, 2, 2, 2, 4 ),
 ( 0.000000000000000000, 0.003619254076116254926, 0.004524067595145328524, 0.005428881114174403423, 0.007238508152232576640, 0.008143321671261699243, 0.009048135190290820112, 0.01085776222834899767, 0.01176257574737808557, 0.01266738926640717348, 0.01357220278543626139, 0.01447701630446534930, 0.01538182982349443895, 0.01628664334252354767, 0.01719145686155265640, 0.01809627038058176512, 0.01900108389961087385, 0.01990589741863998258, 0.02171552445669825207, 0.02262033797572739202, 0.02352515149475653197, 0.02533477853281481534, 0.02714440557087309525, 0.02895403260893137515 ),
 .UNSPECIFIED. ) ;
#12381 = CARTESIAN_POINT ( 'NONE',  ( 23.28845814680232351, 7.864847136539609096, -43.50557691085024459 ) ) ;
#12382 = CARTESIAN_POINT ( 'NONE',  ( 74.95140232871122521, 0.000000000000000000, 41.38025477438755928 ) ) ;
#12383 = FACE_OUTER_BOUND ( 'NONE', #58298, .T. ) ;
#12384 = CARTESIAN_POINT ( 'NONE',  ( 211.1200456646896555, 115.5868795682033152, -13.09781155935739960 ) ) ;
#12385 = FACE_BOUND ( 'NONE', #6381, .T. ) ;
#12386 = EDGE_CURVE ( 'NONE', #54975, #36640, #28636, .T. ) ;
#12387 = CARTESIAN_POINT ( 'NONE',  ( 160.5018603162735360, 61.33906090758085838, 56.87936049605382038 ) ) ;
#12388 = EDGE_CURVE ( 'NONE', #21328, #1580, #62020, .T. ) ;
#12389 = EDGE_CURVE ( 'NONE', #64513, #59450, #34268, .T. ) ;
#12390 = ORIENTED_EDGE ( 'NONE', *, *, #36064, .T. ) ;
#12391 = DIRECTION ( 'NONE',  ( 0.7071067811865543451, 7.105427357601001070E-15, 0.7071067811865408004 ) ) ;
#12392 = CYLINDRICAL_SURFACE ( 'NONE', #22659, 7.500000000000020428 ) ;
#12393 = CARTESIAN_POINT ( 'NONE',  ( -51.66904755831212981, -15.55634918610397222, 0.000000000000000000 ) ) ;
#12394 = CARTESIAN_POINT ( 'NONE',  ( -173.5372686962700470, 89.10569330281725797, 3.977144016177344366 ) ) ;
#12395 = EDGE_CURVE ( 'NONE', #28933, #35756, #38098, .T. ) ;
#12396 = CARTESIAN_POINT ( 'NONE',  ( 209.6698611676811481, 115.2210955123518232, 69.18533967789782935 ) ) ;
#12397 = VECTOR ( 'NONE', #34260, 1000.000000000000000 ) ;
#12398 = CARTESIAN_POINT ( 'NONE',  ( 84.28078136020374700, 18.63296074526051527, -63.03926293933237446 ) ) ;
#12399 = ORIENTED_EDGE ( 'NONE', *, *, #8502, .F. ) ;
#12400 = CARTESIAN_POINT ( 'NONE',  ( -64.97888516016278970, 7.103257987405393159, 6.377659838150127454E-18 ) ) ;
#12401 = CARTESIAN_POINT ( 'NONE',  ( 100.0000000000000284, -5.000000000000000000, 18.50000000000000000 ) ) ;
#12402 = ORIENTED_EDGE ( 'NONE', *, *, #37306, .T. ) ;
#12403 = DIRECTION ( 'NONE',  ( -0.000000000000000000, 1.000000000000000000, -0.000000000000000000 ) ) ;
#12404 = ORIENTED_EDGE ( 'NONE', *, *, #67194, .T. ) ;
#12405 = CARTESIAN_POINT ( 'NONE',  ( -125.8938041572051105, 46.49392987655492959, -49.91370389823397602 ) ) ;
#12406 = CARTESIAN_POINT ( 'NONE',  ( -61.36325649057781817, -43.03793052543183251, 41.38025477438755928 ) ) ;
#12407 = DIRECTION ( 'NONE',  ( 1.000000000000000000, 2.465190328815660250E-32, 0.000000000000000000 ) ) ;
#12409 = EDGE_LOOP ( 'NONE', ( #44300, #52366 ) ) ;
#12408 = ADVANCED_FACE ( 'NONE', ( #45852 ), #18426, .T. ) ;
#12410 = ORIENTED_EDGE ( 'NONE', *, *, #55652, .F. ) ;
#12411 = CARTESIAN_POINT ( 'NONE',  ( 39.40195752203891999, 9.424259417798145577, 71.75838489642698903 ) ) ;
#12412 = EDGE_CURVE ( 'NONE', #65444, #12143, #56757, .T. ) ;
#12414 = ADVANCED_FACE ( 'NONE', ( #24410 ), #7180, .F. ) ;
#12413 = CARTESIAN_POINT ( 'NONE',  ( 164.8908506817023465, 64.97619709085121542, 38.03401370118700697 ) ) ;
#12415 = CIRCLE ( 'NONE', #16862, 27.00000000000000000 ) ;
#12416 = EDGE_CURVE ( 'NONE', #21755, #48801, #29673, .T. ) ;
#12417 = CARTESIAN_POINT ( 'NONE',  ( 105.2529848321548371, 27.73895015262026220, 4.662269661841498269 ) ) ;
#12418 = DIRECTION ( 'NONE',  ( 0.000000000000000000, 0.000000000000000000, 1.000000000000000000 ) ) ;
#12419 = CARTESIAN_POINT ( 'NONE',  ( 4.680456609903976606, 6.535341423375584213, -9.483111142572232310 ) ) ;
#12420 = DIRECTION ( 'NONE',  ( 0.000000000000000000, 0.000000000000000000, 1.000000000000000000 ) ) ;
#12421 = CARTESIAN_POINT ( 'NONE',  ( -50.52615126106341137, 14.55080735582892792, 4.973081677751911123 ) ) ;
#12422 = CARTESIAN_POINT ( 'NONE',  ( -132.8150886319751578, 52.45790550853839562, -18.46974180303275759 ) ) ;
#12423 = CARTESIAN_POINT ( 'NONE',  ( -156.1728533452998136, 71.41054633671237184, -92.55438097918974449 ) ) ;
#12424 = CARTESIAN_POINT ( 'NONE',  ( 7.632783294297949638E-15, 0.000000000000000000, 55.00000000000001421 ) ) ;
#12425 = CARTESIAN_POINT ( 'NONE',  ( 93.98790819024357290, 22.06436042159637267, 92.50594887766449403 ) ) ;
#12427 = VERTEX_POINT ( 'NONE', #51135 ) ;
#12426 = CYLINDRICAL_SURFACE ( 'NONE', #26530, 8.000000000000000000 ) ;
#12428 = EDGE_LOOP ( 'NONE', ( #62003, #34423, #45220, #33438 ) ) ;
#12429 = AXIS2_PLACEMENT_3D ( 'NONE', #47040, #29826, #41426 ) ;
#12430 = ORIENTED_EDGE ( 'NONE', *, *, #5991, .F. ) ;
#12431 = CARTESIAN_POINT ( 'NONE',  ( 0.01688885742776587845, -6.535341423375587766, 4.680456609903974829 ) ) ;
#12432 = CYLINDRICAL_SURFACE ( 'NONE', #51812, 5.000000000000004441 ) ;
#12433 = CARTESIAN_POINT ( 'NONE',  ( -439.4229916354183274, 388.0000000000064233, 96.05029585798874336 ) ) ;
#12434 = CARTESIAN_POINT ( 'NONE',  ( -78.66644367742111399, 22.32174330031317311, -35.11545063171788428 ) ) ;
#12435 = CARTESIAN_POINT ( 'NONE',  ( -37.39246151129639628, 11.66872370876248688, 69.14885973024283317 ) ) ;
#12436 = CARTESIAN_POINT ( 'NONE',  ( 42.52268464718238050, 51.31691565899355822, 34.48241795236666718 ) ) ;
#12437 = CARTESIAN_POINT ( 'NONE',  ( -71.41745561414265353, 19.69148172991711832, -67.47099976427212198 ) ) ;
#12438 = CARTESIAN_POINT ( 'NONE',  ( -14.94265033805045917, 7.459411036484911328, 35.19966624791602783 ) ) ;
#12439 = ORIENTED_EDGE ( 'NONE', *, *, #1437, .T. ) ;
#12440 = DIRECTION ( 'NONE',  ( 0.000000000000000000, -0.000000000000000000, -1.000000000000000000 ) ) ;
#12441 = ORIENTED_EDGE ( 'NONE', *, *, #3358, .T. ) ;
#12442 = ORIENTED_EDGE ( 'NONE', *, *, #15120, .F. ) ;
#12443 = CARTESIAN_POINT ( 'NONE',  ( -142.0084862216822614, 59.34995487985341356, 11.95469468336700203 ) ) ;
#12444 = CARTESIAN_POINT ( 'NONE',  ( 204.6977192012829789, 106.3443248447423599, -51.32593103262161094 ) ) ;
#12445 = CARTESIAN_POINT ( 'NONE',  ( -33.97247179057541899, 11.04235163581741119, 84.33913446809840764 ) ) ;
#12446 = VECTOR ( 'NONE', #36680, 1000.000000000000000 ) ;
#12447 = CARTESIAN_POINT ( 'NONE',  ( 110.7117404013331452, 30.20916032354564607, -24.07788697519003662 ) ) ;
#12448 = DIRECTION ( 'NONE',  ( -0.000000000000000000, 1.000000000000000000, -0.000000000000000000 ) ) ;
#12449 = LINE ( 'NONE', #22649, #10127 ) ;
#12450 = CARTESIAN_POINT ( 'NONE',  ( 138.2136629441929188, 45.30947856186674727, -22.80172309817044862 ) ) ;
#12451 = VERTEX_POINT ( 'NONE', #50090 ) ;
#12452 = EDGE_LOOP ( 'NONE', ( #45552, #44496 ) ) ;
#12453 = VERTEX_POINT ( 'NONE', #39536 ) ;
#12454 = EDGE_CURVE ( 'NONE', #28975, #1146, #69115, .T. ) ;
#12455 =( NAMED_UNIT ( * ) SI_UNIT ( $, .STERADIAN. ) SOLID_ANGLE_UNIT ( ) );
#12456 = LINE ( 'NONE', #40231, #58846 ) ;
#12457 = CARTESIAN_POINT ( 'NONE',  ( 32.29989959354725926, 7.591763852038296179, -67.54129983209111288 ) ) ;
#12458 = CARTESIAN_POINT ( 'NONE',  ( 47.70222499156840712, -57.81185381817577706, 41.38025477438755928 ) ) ;
#12459 = DIRECTION ( 'NONE',  ( -0.000000000000000000, -0.000000000000000000, -1.000000000000000000 ) ) ;
#12460 = CARTESIAN_POINT ( 'NONE',  ( 197.2199569260504006, 98.22436319491369261, 64.21605170112221117 ) ) ;
#12461 = ORIENTED_EDGE ( 'NONE', *, *, #1270, .F. ) ;
#12462 = CARTESIAN_POINT ( 'NONE',  ( -62.49137879463568623, 17.85440472148627933, -68.57102818547264178 ) ) ;
#12463 = FACE_OUTER_BOUND ( 'NONE', #19621, .T. ) ;
#12464 = CARTESIAN_POINT ( 'NONE',  ( -3.255961059272216573, 7.643453059677442596, -36.95062769347506304 ) ) ;
#12465 = CARTESIAN_POINT ( 'NONE',  ( 41.72486082342823721, -50.31647622756196370, 43.58025477438756212 ) ) ;
#12466 = CARTESIAN_POINT ( 'NONE',  ( -171.0814041607219451, 84.88598211196837440, 4.247423101093799502 ) ) ;
#12467 = DIRECTION ( 'NONE',  ( -0.000000000000000000, -0.000000000000000000, -1.000000000000000000 ) ) ;
#12468 = FACE_BOUND ( 'NONE', #47026, .T. ) ;
#12469 = ADVANCED_FACE ( 'NONE', ( #39879, #61340 ), #34625, .T. ) ;
#12470 = CARTESIAN_POINT ( 'NONE',  ( -189.4409533487738031, 107.3684567050774774, 90.35742019377735801 ) ) ;
#12471 = EDGE_CURVE ( 'NONE', #61576, #59809, #44689, .T. ) ;
#12472 = ADVANCED_FACE ( 'NONE', ( #33088 ), #1424, .F. ) ;
#12473 = EDGE_CURVE ( 'NONE', #4596, #53834, #60856, .T. ) ;
#12474 = EDGE_LOOP ( 'NONE', ( #65195, #66234 ) ) ;
#12475 = DIRECTION ( 'NONE',  ( 1.387778780781446169E-16, -1.000000000000000000, -3.469446951953615421E-17 ) ) ;
#12476 = VECTOR ( 'NONE', #45844, 1000.000000000000000 ) ;
#12477 = CARTESIAN_POINT ( 'NONE',  ( -132.8123438040339863, 51.22132183644642112, -66.35088960131899682 ) ) ;
#12478 = LINE ( 'NONE', #1569, #18550 ) ;
#12479 = DIRECTION ( 'NONE',  ( 4.906538933386759377E-15, 0.7071067811865474617, -0.7071067811865474617 ) ) ;
#12480 = ADVANCED_FACE ( 'NONE', ( #65450 ), #12329, .F. ) ;
#12481 = CARTESIAN_POINT ( 'NONE',  ( 62.52762183777206673, 13.59210632617624626, -62.56524142263337751 ) ) ;
#12482 = VECTOR ( 'NONE', #4100, 1000.000000000000000 ) ;
#12483 = ORIENTED_EDGE ( 'NONE', *, *, #28078, .T. ) ;
#12484 = CARTESIAN_POINT ( 'NONE',  ( -30.00000000000000355, -27.00000000000000355, 12.00000000000000000 ) ) ;
#12485 = CARTESIAN_POINT ( 'NONE',  ( 188.1716167230092367, 86.07821889697497397, 88.01412198095141548 ) ) ;
#12486 = VERTEX_POINT ( 'NONE', #28146 ) ;
#12487 = CONICAL_SURFACE ( 'NONE', #51799, 4.171999999999999709, 0.7853981633974437271 ) ;
#12488 = VERTEX_POINT ( 'NONE', #55227 ) ;
#12489 = CARTESIAN_POINT ( 'NONE',  ( 174.9042454172880809, 72.57746269938728290, -39.44483778160518028 ) ) ;
#12490 = CARTESIAN_POINT ( 'NONE',  ( -177.1539090641757923, 91.73101548694630480, -62.71746391358476558 ) ) ;
#12491 = DIRECTION ( 'NONE',  ( 0.000000000000000000, 0.000000000000000000, 1.000000000000000000 ) ) ;
#12492 = VERTEX_POINT ( 'NONE', #12678 ) ;
#12493 = CARTESIAN_POINT ( 'NONE',  ( 117.4806398654733925, 33.50379325299403632, 61.92154777411960964 ) ) ;
#12494 = CARTESIAN_POINT ( 'NONE',  ( -178.5835577246387800, 93.42126246260829703, 6.332233931154211959 ) ) ;
#12495 = DIRECTION ( 'NONE',  ( 1.000000000000000000, 1.387778780781446908E-16, 0.000000000000000000 ) ) ;
#12496 = VECTOR ( 'NONE', #52986, 1000.000000000000000 ) ;
#12497 = EDGE_CURVE ( 'NONE', #39103, #46320, #17244, .T. ) ;
#12499 = EDGE_CURVE ( 'NONE', #12094, #56059, #68028, .T. ) ;
#12498 = LINE ( 'NONE', #22695, #22497 ) ;
#12500 = CARTESIAN_POINT ( 'NONE',  ( 21.11067624421128386, 6.728538062205546844, -91.35668824920195163 ) ) ;
#12501 = CARTESIAN_POINT ( 'NONE',  ( -189.2739965869454863, 107.1373753350176941, 37.54313195747183585 ) ) ;
#12502 = EDGE_CURVE ( 'NONE', #42723, #41204, #48536, .T. ) ;
#12503 = ORIENTED_EDGE ( 'NONE', *, *, #67282, .T. ) ;
#12504 = CARTESIAN_POINT ( 'NONE',  ( -124.9927180788553898, 45.90286323198618135, -8.109744398480245309 ) ) ;
#12505 = CARTESIAN_POINT ( 'NONE',  ( -74.79539698934962644, 21.95498232236882075, 4.645315566659635742 ) ) ;
#12506 = CARTESIAN_POINT ( 'NONE',  ( -143.2498117110514784, 60.33382252735058415, -46.45533462960677440 ) ) ;
#12507 = LINE ( 'NONE', #12163, #5037 ) ;
#12509 = ORIENTED_EDGE ( 'NONE', *, *, #61698, .F. ) ;
#12508 = DIRECTION ( 'NONE',  ( 2.377681859532301304E-16, -7.725556675377196710E-17, 1.000000000000000000 ) ) ;
#12510 = CARTESIAN_POINT ( 'NONE',  ( 79.52861599156693728, 17.11914630560288231, -45.78734971095504136 ) ) ;
#12511 = ORIENTED_EDGE ( 'NONE', *, *, #46833, .F. ) ;
#12512 = CARTESIAN_POINT ( 'NONE',  ( -127.6992109187852265, 47.69334801994796891, 30.82611642083012882 ) ) ;
#12513 = CARTESIAN_POINT ( 'NONE',  ( 84.72546926745364715, 19.84015517905188020, 44.48241298831661084 ) ) ;
#12514 = CARTESIAN_POINT ( 'NONE',  ( -8.663926357539105894, 23.45072237844991747, 0.000000000000000000 ) ) ;
#12515 = CARTESIAN_POINT ( 'NONE',  ( 92.53033045403535084, 22.59263332688195192, 32.55674288556603102 ) ) ;
#12516 = CARTESIAN_POINT ( 'NONE',  ( 141.2366329129481244, 46.06278879703611295, -18.04134848091257837 ) ) ;
#12517 = FACE_OUTER_BOUND ( 'NONE', #3484, .T. ) ;
#12518 = CARTESIAN_POINT ( 'NONE',  ( 17.85632111170821190, 7.582480637908914467, -89.48644972445111989 ) ) ;
#12519 = CARTESIAN_POINT ( 'NONE',  ( -34.39004539972345498, 0.000000000000000000, 5.000000000000000000 ) ) ;
#12520 = ORIENTED_EDGE ( 'NONE', *, *, #12074, .T. ) ;
#12521 = EDGE_LOOP ( 'NONE', ( #53310, #62518, #64465, #27014 ) ) ;
#12522 = VECTOR ( 'NONE', #11409, 1000.000000000000000 ) ;
#12523 = CARTESIAN_POINT ( 'NONE',  ( 45.34143264614441904, 9.256465810451196319, 32.82761261990431478 ) ) ;
#12524 = CARTESIAN_POINT ( 'NONE',  ( 199.3743599161302882, 99.31857334527873604, -11.67350270838394266 ) ) ;
#12525 = DIRECTION ( 'NONE',  ( 1.000000000000000000, 0.000000000000000000, -0.000000000000000000 ) ) ;
#12526 = CARTESIAN_POINT ( 'NONE',  ( 0.000000000000000000, 0.000000000000000000, 0.000000000000000000 ) ) ;
#12527 = CARTESIAN_POINT ( 'NONE',  ( 206.2957331585308793, 110.2946564621822887, -51.19906654808809066 ) ) ;
#12528 = AXIS2_PLACEMENT_3D ( 'NONE', #6770, #39144, #46134 ) ;
#12529 = CARTESIAN_POINT ( 'NONE',  ( -73.80418150970714919, 21.59712875466424364, -75.19184975933067960 ) ) ;
#12530 = CARTESIAN_POINT ( 'NONE',  ( 0.7145311798163274108, 9.237604307034018802, -2.124379920709345337E-16 ) ) ;
#12531 = CARTESIAN_POINT ( 'NONE',  ( -24.94151142167918067, 8.614613465433007988, -46.59531917729278661 ) ) ;
#12532 = CARTESIAN_POINT ( 'NONE',  ( 164.3577270662354977, 63.21061577643038731, -73.44943585255833796 ) ) ;
#12533 = PRODUCT_DEFINITION_SHAPE ( 'NONE', 'NONE',  #69601 ) ;
#12534 = VERTEX_POINT ( 'NONE', #21824 ) ;
#12535 = ORIENTED_EDGE ( 'NONE', *, *, #45821, .T. ) ;
#12536 = AXIS2_PLACEMENT_3D ( 'NONE', #6358, #43281, #15869 ) ;
#12537 = MECHANICAL_DESIGN_GEOMETRIC_PRESENTATION_REPRESENTATION (  '', ( #8013 ), #6908 ) ;
#12538 = DIRECTION ( 'NONE',  ( -0.000000000000000000, 1.000000000000000000, -0.000000000000000000 ) ) ;
#12539 = EDGE_CURVE ( 'NONE', #6204, #67474, #22183, .T. ) ;
#12540 = CARTESIAN_POINT ( 'NONE',  ( -31.11269837220809364, -15.55634918610397754, 0.000000000000000000 ) ) ;
#12541 = CARTESIAN_POINT ( 'NONE',  ( -80.54757501605355685, 23.04700348514568020, 72.02692194415921279 ) ) ;
#12542 = CARTESIAN_POINT ( 'NONE',  ( 130.7260570116703775, 40.73146260246711847, 43.84148412689328467 ) ) ;
#12543 = CARTESIAN_POINT ( 'NONE',  ( -66.47744250486724127, 4.728025645033430813, 34.48241823979542886 ) ) ;
#12544 = CARTESIAN_POINT ( 'NONE',  ( 400.0000000000000000, 2.449293598294706513E-15, -20.00000000000000000 ) ) ;
#12545 = STYLED_ITEM ( 'NONE', ( #54284 ), #16293 ) ;
#12546 = CARTESIAN_POINT ( 'NONE',  ( -99.10904156412046007, 32.31949011661293270, -8.856797566735396643 ) ) ;
#12547 = CARTESIAN_POINT ( 'NONE',  ( 56.52885800925552218, 12.28784885070978561, 33.51606380828312126 ) ) ;
#12548 = CARTESIAN_POINT ( 'NONE',  ( 32.21680480348707221, 7.583440910203144369, 88.92743217354535545 ) ) ;
#12549 = CARTESIAN_POINT ( 'NONE',  ( 410.0000000000000000, 0.000000000000000000, 0.000000000000000000 ) ) ;
#12550 = EDGE_LOOP ( 'NONE', ( #41664, #54442 ) ) ;
#12551 = FACE_OUTER_BOUND ( 'NONE', #3744, .T. ) ;
#12552 = PLANE ( 'NONE',  #13817 ) ;
#12553 = CARTESIAN_POINT ( 'NONE',  ( -189.7334103489410211, 107.7745063523401114, -44.80734569376801346 ) ) ;
#12554 = EDGE_CURVE ( 'NONE', #59695, #25409, #43625, .T. ) ;
#12555 = DIRECTION ( 'NONE',  ( 1.000000000000000000, 0.000000000000000000, 0.000000000000000000 ) ) ;
#12556 = CARTESIAN_POINT ( 'NONE',  ( -109.7290872258106731, 36.72869630780158445, -70.37839858795491921 ) ) ;
#12557 = CARTESIAN_POINT ( 'NONE',  ( 128.4157044224114657, 39.39296260757096491, -21.86358749922995059 ) ) ;
#12558 = EDGE_CURVE ( 'NONE', #6777, #9445, #46317, .T. ) ;
#12559 = EDGE_CURVE ( 'NONE', #43039, #22496, #1991, .T. ) ;
#12560 = VERTEX_POINT ( 'NONE', #44325 ) ;
#12561 = DIRECTION ( 'NONE',  ( 0.9995598612609390976, 0.02966620562209615342, -9.873200265418058740E-15 ) ) ;
#12562 = CARTESIAN_POINT ( 'NONE',  ( 444.9999999999999432, -35.00000000000000000, -2.000000000000000000 ) ) ;
#12563 = CARTESIAN_POINT ( 'NONE',  ( 290.0000000000000568, 5.000000000000000888, 18.50000000000000000 ) ) ;
#12564 = CARTESIAN_POINT ( 'NONE',  ( -166.3231866619663890, 81.31146386205591625, -39.03154315301186017 ) ) ;
#12565 = ADVANCED_FACE ( 'NONE', ( #16896 ), #17605, .T. ) ;
#12566 = CARTESIAN_POINT ( 'NONE',  ( -74.58602291351357394, -7.967916035252095242, 170.0000000000000000 ) ) ;
#12567 = ORIENTED_EDGE ( 'NONE', *, *, #34694, .T. ) ;
#12568 = CARTESIAN_POINT ( 'NONE',  ( -118.4063383664800000, 41.75753822095644097, -41.90331656875046917 ) ) ;
#12569 = CARTESIAN_POINT ( 'NONE',  ( 76.57571471437145760, 10.00000000000000000, -30.00000000000000000 ) ) ;
#12570 = LINE ( 'NONE', #65338, #5522 ) ;
#12571 = CARTESIAN_POINT ( 'NONE',  ( -7.825402957745081878, 7.899365992529270741, -77.26262132240753999 ) ) ;
#12572 = B_SPLINE_CURVE_WITH_KNOTS ( 'NONE', 3,
 ( #2516, #40833, #35564, #19728 ),
 .UNSPECIFIED., .F., .F.,
 ( 4, 4 ),
 ( 9.900409499046083621E-07, 0.05658314289920116785 ),
 .UNSPECIFIED. ) ;
#12573 =( REPRESENTATION_RELATIONSHIP ('NONE','NONE', #40274, #64096 ) REPRESENTATION_RELATIONSHIP_WITH_TRANSFORMATION ( #39988 )SHAPE_REPRESENTATION_RELATIONSHIP( ) );
#12574 = DIRECTION ( 'NONE',  ( -1.000000000000000000, 2.279101714840934323E-64, -7.703719777548945123E-34 ) ) ;
#12575 = ORIENTED_EDGE ( 'NONE', *, *, #35158, .T. ) ;
#12576 = CARTESIAN_POINT ( 'NONE',  ( 162.8616317072115578, 63.27292930957019479, -92.08433922111466075 ) ) ;
#12577 = CARTESIAN_POINT ( 'NONE',  ( 201.9777685760379313, 102.6876480786893069, -50.82744265795196981 ) ) ;
#12578 = CARTESIAN_POINT ( 'NONE',  ( 112.3013380801408658, 400.0000000000066507, -133.9497041420121377 ) ) ;
#12579 = CIRCLE ( 'NONE', #9209, 5.000000000000000888 ) ;
#12580 = FACE_OUTER_BOUND ( 'NONE', #14407, .T. ) ;
#12581 = AXIS2_PLACEMENT_3D ( 'NONE', #5902, #54435, #10846 ) ;
#12583 = ORIENTED_EDGE ( 'NONE', *, *, #67031, .T. ) ;
#12582 = CARTESIAN_POINT ( 'NONE',  ( -422.6627218934914936, 394.9999999999956799, 83.55029585799226766 ) ) ;
#12584 = ADVANCED_FACE ( 'NONE', ( #39069 ), #27446, .F. ) ;
#12585 = CARTESIAN_POINT ( 'NONE',  ( 60.40277045393653310, 12.08176563382369828, 44.34733751979118210 ) ) ;
#12586 = ORIENTED_EDGE ( 'NONE', *, *, #58368, .T. ) ;
#12587 = AXIS2_PLACEMENT_3D ( 'NONE', #19788, #37331, #68992 ) ;
#12588 =( GEOMETRIC_REPRESENTATION_CONTEXT ( 3 ) GLOBAL_UNCERTAINTY_ASSIGNED_CONTEXT ( ( #66299 ) ) GLOBAL_UNIT_ASSIGNED_CONTEXT ( ( #52001, #41456, #58642 ) ) REPRESENTATION_CONTEXT ( 'NONE', 'WORKASPACE' ) );
#12589 = ORIENTED_EDGE ( 'NONE', *, *, #62499, .F. ) ;
#12590 = CARTESIAN_POINT ( 'NONE',  ( -74.17694007417657076, 20.66176641130876845, -9.743324496515986866 ) ) ;
#12591 = CARTESIAN_POINT ( 'NONE',  ( -36.80719415492644941, 11.55793080356381175, -91.25128724788480383 ) ) ;
#12593 = VERTEX_POINT ( 'NONE', #48888 ) ;
#12592 = CARTESIAN_POINT ( 'NONE',  ( -10.23531775138760835, 8.068923942586302189, -76.86913210980220867 ) ) ;
#12594 = CARTESIAN_POINT ( 'NONE',  ( -95.31607127852431915, 30.49332874523306458, 88.90476004080002781 ) ) ;
#12595 = CLOSED_SHELL ( 'NONE', ( #59211, #38605, #8657, #14556, #18517, #15863, #67916, #11424, #28835, #39977, #66406, #55361, #1296, #20248, #9603, #15227, #15490, #24645, #15173, #41841, #23292, #41050, #33464, #55568, #60821, #23493, #34149, #7062, #32269, #40119, #55264, #14692, #23516, #44855, #47740, #5048, #9546, #66904, #48472, #6191, #36845, #8123, #8991, #28954, #55573, #19866, #40643, #9625, #49293, #34029, #35606, #68244, #66564, #14512, #33898, #38651, #725, #7314, #67207, #56054, #33634, #32156, #60426, #38700, #45393, #52469, #52703, #9535, #22154, #58929, #9707, #47018, #17805, #44803, #40720, #63294, #6827, #15156, #40903, #20194, #3897, #39533, #60102, #58517, #30390, #27440, #54525, #21566, #17701, #23433, #29915, #40197, #24947, #11168, #35009, #33281, #5464, #54061, #2153, #17973, #22020, #61940, #57215, #32081, #55937, #65515, #13714, #35408, #61877, #43963, #36874, #41235, #13971, #62254, #49537, #40840, #11576, #10593, #6846, #54461, #6193, #24470, #50829, #11044, #2700, #67084, #9292, #44457, #10459, #69160, #17106, #68443, #16104, #18733, #44324, #36300, #46059, #29732, #67742, #46204, #45493, #16295, #28284, #45181, #55755, #54422, #39112, #43266, #39636, #57664, #35112, #33117, #13880, #23740, #26623, #22466, #20017, #61880, #55343, #57941, #58826, #17373, #40654, #65836, #30006, #8924, #42795, #66083, #33522, #25851, #66648, #48897, #18684, #1295, #18849, #43722, #42691, #1345, #27863, #64188, #21599, #46375, #60191, #25761, #58590, #65737, #64858, #51767, #17659, #10241, #13908, #40100, #37137, #66627, #32541, #13744, #12565, #64365, #8532, #47297, #9128, #15001, #11919, #46199, #14945, #64217, #41198, #58032, #47214, #37381, #52042, #60526, #9460, #64322, #27944, #21812, #60124, #41720, #45583, #39491, #68227, #62956, #52167, #16497, #59074, #27872, #51408, #7640, #53181, #10418, #10019, #53242, #54560, #7226, #1604, #4671, #44544, #11667, #64083, #29080, #36614, #3818, #68318, #44996, #38912, #67455, #52850, #19777, #23285, #52162, #2218, #45730, #60073, #4780, #61132, #67073, #50916, #34827, #9208, #17956, #4401, #9790, #39942, #5707, #11748, #2714, #35998, #63040, #12480, #26702, #47460, #22733, #24869, #48034, #3523, #36275, #63999, #5386, #37884, #23170, #30568, #407, #49662, #52951, #8593, #16486, #775, #1127, #65295, #15408, #56467, #63218, #30732, #37064, #41299, #63638, #56698, #13518, #35588, #27206, #24056, #65434, #44938, #16504, #7862, #55503, #15870, #52038, #13344, #5826, #49483, #26181, #53594, #60500, #13683, #61929, #2719, #23441, #23594, #56934, #1693, #31210, #9444, #3560, #60360, #38104, #5148, #11045, #36558, #24073, #65744, #44747, #49121, #40569, #7689, #64402, #62492, #54361, #12646, #16203, #26522, #69319, #57185, #69124, #19683, #42556, #34085, #44567, #39950, #28991, #962, #18182, #60431, #7743 ) ) ;
#12596 = CARTESIAN_POINT ( 'NONE',  ( -28.13128612339710344, 10.08889185338653327, 44.46541057415654308 ) ) ;
#12597 = FACE_BOUND ( 'NONE', #39765, .T. ) ;
#12598 = ORIENTED_EDGE ( 'NONE', *, *, #14397, .T. ) ;
#12599 = CARTESIAN_POINT ( 'NONE',  ( 207.4566510040494904, 111.9649643341356438, -77.64771060859440865 ) ) ;
#12600 = CARTESIAN_POINT ( 'NONE',  ( 0.000000000000000000, 5.000000000000000000, 2.000000000000001776 ) ) ;
#12601 = CARTESIAN_POINT ( 'NONE',  ( -175.1968289912784371, 90.99944698359489337, 45.54112020630180524 ) ) ;
#12602 = CARTESIAN_POINT ( 'NONE',  ( -132.8257891167039020, 52.46553896898735303, 14.15040099157313236 ) ) ;
#12603 = CARTESIAN_POINT ( 'NONE',  ( 16.77480716385437987, 7.540753720029939267, 56.90830145484930114 ) ) ;
#12604 = EDGE_LOOP ( 'NONE', ( #14217, #30313, #39326, #17948 ) ) ;
#12605 = EDGE_LOOP ( 'NONE', ( #13770, #54497 ) ) ;
#12606 = ORIENTED_EDGE ( 'NONE', *, *, #34401, .T. ) ;
#12607 = LINE ( 'NONE', #39683, #31749 ) ;
#12608 = CARTESIAN_POINT ( 'NONE',  ( -107.0809603157386363, 36.42942792191065138, 16.95719255189394303 ) ) ;
#12609 = DIRECTION ( 'NONE',  ( -1.000000000000000000, 0.000000000000000000, 0.000000000000000000 ) ) ;
#12610 = CARTESIAN_POINT ( 'NONE',  ( -36.37371824399145481, 10.45334302951138739, -48.48679871522361395 ) ) ;
#12611 = CARTESIAN_POINT ( 'NONE',  ( -105.2142611701586503, 34.29582324647149250, 84.77962915760878104 ) ) ;
#12612 = LINE ( 'NONE', #24216, #42663 ) ;
#12613 = EDGE_CURVE ( 'NONE', #16637, #60863, #54522, .T. ) ;
#12614 = CARTESIAN_POINT ( 'NONE',  ( -59.94154301275507635, -45.09516516490467808, 170.0000000000000000 ) ) ;
#12615 = CARTESIAN_POINT ( 'NONE',  ( -75.00636493611885669, 22.03142602679956497, -9.206886202885991466 ) ) ;
#12617 = EDGE_LOOP ( 'NONE', ( #21075, #40042 ) ) ;
#12616 = EDGE_CURVE ( 'NONE', #25903, #6273, #27806, .T. ) ;
#12618 = CARTESIAN_POINT ( 'NONE',  ( 82.34195123877069022, 18.00239921638039320, 70.21512810070214528 ) ) ;
#12619 = ORIENTED_EDGE ( 'NONE', *, *, #24226, .T. ) ;
#12620 = CARTESIAN_POINT ( 'NONE',  ( 32.15641333221390141, 7.577415570152253643, 39.36641614295111680 ) ) ;
#12621 = EDGE_CURVE ( 'NONE', #21254, #22088, #6357, .T. ) ;
#12622 = FACE_OUTER_BOUND ( 'NONE', #13723, .T. ) ;
#12623 = CARTESIAN_POINT ( 'NONE',  ( 181.9406741394861342, 79.47484497224790800, 44.27164137268504618 ) ) ;
#12624 = LINE ( 'NONE', #23874, #55752 ) ;
#12625 = CARTESIAN_POINT ( 'NONE',  ( -452.6627218934914367, 399.9999999999998863, -111.4497041420118251 ) ) ;
#12626 = CARTESIAN_POINT ( 'NONE',  ( -120.6420427933462207, 44.31795133507805673, 59.60453931232847680 ) ) ;
#12627 = EDGE_CURVE ( 'NONE', #68773, #3776, #58768, .T. ) ;
#12628 = CARTESIAN_POINT ( 'NONE',  ( -51.99406906667274342, 13.88268392809765572, 17.82498527766545848 ) ) ;
#12629 = AXIS2_PLACEMENT_3D ( 'NONE', #11592, #33073, #54500 ) ;
#12630 = LINE ( 'NONE', #18599, #46130 ) ;
#12631 = CARTESIAN_POINT ( 'NONE',  ( 162.8034185388970627, 63.22443559329411755, -75.76383047087158218 ) ) ;
#12632 = ORIENTED_EDGE ( 'NONE', *, *, #36373, .T. ) ;
#12633 = CARTESIAN_POINT ( 'NONE',  ( -173.1211646369891355, 88.63826465341151106, 30.82169460664101734 ) ) ;
#12634 = CARTESIAN_POINT ( 'NONE',  ( -154.7934364910360330, 68.79594655117534785, -10.14203366738286860 ) ) ;
#12635 = ORIENTED_EDGE ( 'NONE', *, *, #51653, .T. ) ;
#12636 = DIRECTION ( 'NONE',  ( -0.04486483035051862939, 0.9989930665413143673, 1.037707659396819425E-17 ) ) ;
#12637 = LINE ( 'NONE', #10278, #44125 ) ;
#12638 = DIRECTION ( 'NONE',  ( 0.000000000000000000, -1.000000000000000000, -1.385458760688113094E-14 ) ) ;
#12639 = ORIENTED_EDGE ( 'NONE', *, *, #42706, .F. ) ;
#12640 = CARTESIAN_POINT ( 'NONE',  ( -84.22570405563701001, 24.51726571826274537, 42.97634706641604652 ) ) ;
#12641 = CARTESIAN_POINT ( 'NONE',  ( 150.2060369882285329, 53.45752899907539302, -68.58311478360899116 ) ) ;
#12642 = CARTESIAN_POINT ( 'NONE',  ( 42.48820792780864508, 9.847387255477762835, 30.57387150330147563 ) ) ;
#12643 = VECTOR ( 'NONE', #62882, 1000.000000000000000 ) ;
#12644 = CARTESIAN_POINT ( 'NONE',  ( 139.6203063421346826, 45.01495791936837065, -48.34818717462631099 ) ) ;
#12645 = EDGE_CURVE ( 'NONE', #63246, #16366, #42603, .T. ) ;
#12646 = ADVANCED_FACE ( 'NONE', ( #378 ), #48204, .F. ) ;
#12647 = ORIENTED_EDGE ( 'NONE', *, *, #2837, .F. ) ;
#12648 = AXIS2_PLACEMENT_3D ( 'NONE', #42834, #10146, #31607 ) ;
#12649 = LINE ( 'NONE', #55545, #62635 ) ;
#12650 = EDGE_LOOP ( 'NONE', ( #64800, #1066, #39049, #26063 ) ) ;
#12651 = CARTESIAN_POINT ( 'NONE',  ( 133.8566784816069344, -170.0000000000000000, -16.67876034193198365 ) ) ;
#12652 = CARTESIAN_POINT ( 'NONE',  ( 26.11269837220809364, 15.55634918610396866, 0.000000000000000000 ) ) ;
#12653 = PRESENTATION_STYLE_ASSIGNMENT (( #29179 ) ) ;
#12654 = CARTESIAN_POINT ( 'NONE',  ( -1.095583923122883663, 7.553030873957007785, 67.77975244133044441 ) ) ;
#12655 = DIRECTION ( 'NONE',  ( 0.000000000000000000, 0.000000000000000000, 1.000000000000000000 ) ) ;
#12656 = LINE ( 'NONE', #13015, #66385 ) ;
#12657 = ORIENTED_EDGE ( 'NONE', *, *, #52712, .F. ) ;
#12658 = DIRECTION ( 'NONE',  ( 0.000000000000000000, 0.000000000000000000, 1.000000000000000000 ) ) ;
#12659 = ORIENTED_EDGE ( 'NONE', *, *, #55904, .T. ) ;
#12660 = CARTESIAN_POINT ( 'NONE',  ( 161.7048274740120917, 61.01946783654760509, -22.98727189428458573 ) ) ;
#12661 = FACE_OUTER_BOUND ( 'NONE', #14836, .T. ) ;
#12662 = CARTESIAN_POINT ( 'NONE',  ( -60.41792053122280493, 24.01035990323433822, 43.58025477438756923 ) ) ;
#12663 = CARTESIAN_POINT ( 'NONE',  ( 140.2332932573541484, 45.41010019581508317, -66.38781847616553478 ) ) ;
#12664 = CARTESIAN_POINT ( 'NONE',  ( 11.29825944729837062, -74.09495289492984682, 41.38025477438755928 ) ) ;
#12665 = ORIENTED_EDGE ( 'NONE', *, *, #3026, .T. ) ;
#12666 = DIRECTION ( 'NONE',  ( -0.000000000000000000, 1.000000000000000000, -0.000000000000000000 ) ) ;
#12667 = CARTESIAN_POINT ( 'NONE',  ( 13.37820144534468803, 6.435512790162280616, 44.62119266632897308 ) ) ;
#12668 = ORIENTED_EDGE ( 'NONE', *, *, #36855, .T. ) ;
#12669 = CARTESIAN_POINT ( 'NONE',  ( -62.45176220516619736, 16.79101814080731714, -68.30864959305280593 ) ) ;
#12670 = CARTESIAN_POINT ( 'NONE',  ( 131.2736393829322878, 39.88634239355057076, -90.16109689038154329 ) ) ;
#12671 = VECTOR ( 'NONE', #6342, 1000.000000000000000 ) ;
#12672 = ORIENTED_EDGE ( 'NONE', *, *, #67075, .F. ) ;
#12673 = CARTESIAN_POINT ( 'NONE',  ( -125.8938041572051389, 47.69968343338778283, 3.775397282693376155 ) ) ;
#12674 = DIRECTION ( 'NONE',  ( 0.3930250316539148359, 0.9195277725514544587, 0.000000000000000000 ) ) ;
#12675 = CARTESIAN_POINT ( 'NONE',  ( 2.905661822261151883E-14, 20.55634918610402906, 0.000000000000000000 ) ) ;
#12676 = VECTOR ( 'NONE', #33989, 1000.000000000000000 ) ;
#12677 = ORIENTED_EDGE ( 'NONE', *, *, #69390, .T. ) ;
#12678 = CARTESIAN_POINT ( 'NONE',  ( -58.00979178563811445, -29.32343869649178814, 170.0000000000000000 ) ) ;
#12679 = VECTOR ( 'NONE', #16689, 1000.000000000000000 ) ;
#12680 = CARTESIAN_POINT ( 'NONE',  ( 70.21232668545647471, 15.49872527826561885, 88.86438496759851091 ) ) ;
#12681 = CARTESIAN_POINT ( 'NONE',  ( 37.70910994512001935, 9.209110272746713122, 30.10326457111060705 ) ) ;
#12682 = CARTESIAN_POINT ( 'NONE',  ( -180.5801285865472039, 97.42945596116099694, -43.01106670952992062 ) ) ;
#12683 = CARTESIAN_POINT ( 'NONE',  ( -133.3958821919892728, 51.63629593114587379, -16.08335082672273231 ) ) ;
#12684 = AXIS2_PLACEMENT_3D ( 'NONE', #20845, #41961, #42306 ) ;
#12685 = CARTESIAN_POINT ( 'NONE',  ( 153.8366942494331226, 54.87992279068316748, 70.31910049688980280 ) ) ;
#12686 = CARTESIAN_POINT ( 'NONE',  ( 128.3856248084844083, 38.21741401878864508, -75.52143459682376658 ) ) ;
#12687 = B_SPLINE_CURVE_WITH_KNOTS ( 'NONE', 3,
 ( #11466, #43131, #54374, #59316, #32593, #21682 ),
 .UNSPECIFIED., .F., .F.,
 ( 4, 2, 4 ),
 ( 1.095770181098974840E-06, 0.03239442681617710901, 0.06478775786217311206 ),
 .UNSPECIFIED. ) ;
#12688 = ORIENTED_EDGE ( 'NONE', *, *, #16764, .F. ) ;
#12689 = CARTESIAN_POINT ( 'NONE',  ( 140.5958192060901411, 46.84598876498521491, -73.66959190929182455 ) ) ;
#12690 = DIRECTION ( 'NONE',  ( -0.000000000000000000, 1.000000000000000000, -0.000000000000000000 ) ) ;
#12691 = ORIENTED_EDGE ( 'NONE', *, *, #6365, .F. ) ;
#12692 = CIRCLE ( 'NONE', #1439, 74.95140232871122521 ) ;
#12693 = CARTESIAN_POINT ( 'NONE',  ( -156.4797890011541597, 71.69341087347112307, -45.08998991706700110 ) ) ;
#12694 = CARTESIAN_POINT ( 'NONE',  ( 207.4610690199662315, 111.9701171077052209, -9.997192138305063480 ) ) ;
#12695 = CARTESIAN_POINT ( 'NONE',  ( -38.87871322265798568, 11.95691939779334945, 38.69778012508339060 ) ) ;
#12696 = CARTESIAN_POINT ( 'NONE',  ( -169.8842709557924877, 83.59602878049474839, -48.99215875544830112 ) ) ;
#12697 = DIRECTION ( 'NONE',  ( -0.000000000000000000, 1.000000000000000000, -0.000000000000000000 ) ) ;
#12698 = CYLINDRICAL_SURFACE ( 'NONE', #41552, 66.50000000000000000 ) ;
#12699 = CARTESIAN_POINT ( 'NONE',  ( -48.99162761293256096, 13.13973062091724131, -73.98514508948782975 ) ) ;
#12700 = CARTESIAN_POINT ( 'NONE',  ( 204.6977192012829789, 106.3443248447423599, -51.32593103262161094 ) ) ;
#12701 = EDGE_CURVE ( 'NONE', #26321, #28516, #37102, .T. ) ;
#12702 = CARTESIAN_POINT ( 'NONE',  ( -14.33060720034884028, 8.412649192293189415, 33.85085847379210833 ) ) ;
#12703 = CARTESIAN_POINT ( 'NONE',  ( 115.0692128464502417, 31.17922615202198600, 16.02821217000574094 ) ) ;
#12704 = CARTESIAN_POINT ( 'NONE',  ( 51.39999999999999858, 0.000000000000000000, 4.171999999999999709 ) ) ;
#12705 = EDGE_LOOP ( 'NONE', ( #58243, #17081, #64936, #66962 ) ) ;
#12706 = DIRECTION ( 'NONE',  ( -0.000000000000000000, -0.000000000000000000, -1.000000000000000000 ) ) ;
#12708 = ORIENTED_EDGE ( 'NONE', *, *, #10854, .T. ) ;
#12707 = ADVANCED_FACE ( 'NONE', ( #5995 ), #29, .F. ) ;
#12709 = DIRECTION ( 'NONE',  ( 0.000000000000000000, 1.000000000000000000, -0.000000000000000000 ) ) ;
#12710 = CARTESIAN_POINT ( 'NONE',  ( 82.73618382051373032, 19.18661415186666730, -63.75104638294856585 ) ) ;
#12711 = CARTESIAN_POINT ( 'NONE',  ( 44.35071890818839790, 9.104600422692275430, 69.91515779349310833 ) ) ;
#12712 = CARTESIAN_POINT ( 'NONE',  ( 0.000000000000000000, 0.000000000000000000, 0.000000000000000000 ) ) ;
#12713 = EDGE_CURVE ( 'NONE', #22712, #49636, #17250, .T. ) ;
#12714 = CARTESIAN_POINT ( 'NONE',  ( -125.8938041572051389, -170.0000000000000000, -42.41370389823394760 ) ) ;
#12715 = CARTESIAN_POINT ( 'NONE',  ( -3.973643313806734888E-15, 6.732211846623391338, -4.339467034331192075 ) ) ;
#12716 = DIRECTION ( 'NONE',  ( 1.697742017499683849E-16, -1.665334536937734564E-16, 1.000000000000000000 ) ) ;
#12717 = CARTESIAN_POINT ( 'NONE',  ( 47.73902449249074920, -57.85799893277823713, 170.0000000000000000 ) ) ;
#12718 = ORIENTED_EDGE ( 'NONE', *, *, #4375, .F. ) ;
#12719 = ORIENTED_EDGE ( 'NONE', *, *, #46763, .F. ) ;
#12720 = CARTESIAN_POINT ( 'NONE',  ( 46.68054346512387554, 9.468156054376091646, -95.00000000000133582 ) ) ;
#12721 = CARTESIAN_POINT ( 'NONE',  ( 173.6710158776850506, 71.42507420636735560, 62.47632899483146218 ) ) ;
#12722 = DIRECTION ( 'NONE',  ( 0.9839295885986295565, 0.1785568947986370392, 0.000000000000000000 ) ) ;
#12723 = CARTESIAN_POINT ( 'NONE',  ( 447.3372781065085633, 370.0000000000043769, 113.5502958579838122 ) ) ;
#12724 = VECTOR ( 'NONE', #21195, 1000.000000000000114 ) ;
#12725 = CARTESIAN_POINT ( 'NONE',  ( -173.1211646369891355, 88.63826465341151106, -22.86740657428632773 ) ) ;
#12726 = EDGE_CURVE ( 'NONE', #11163, #11222, #1083, .T. ) ;
#12727 = VECTOR ( 'NONE', #39433, 1000.000000000000000 ) ;
#12728 = CYLINDRICAL_SURFACE ( 'NONE', #65623, 2.999999999999999112 ) ;
#12729 = ORIENTED_EDGE ( 'NONE', *, *, #35915, .T. ) ;
#12730 = CARTESIAN_POINT ( 'NONE',  ( 103.5589117581614715, 27.00490790413960340, -39.98222358844557078 ) ) ;
#12731 = DIRECTION ( 'NONE',  ( 0.000000000000000000, 0.000000000000000000, -1.000000000000000000 ) ) ;
#12732 = CARTESIAN_POINT ( 'NONE',  ( 12.47451846520756646, 7.423604437114563304, 57.62656840523505508 ) ) ;
#12733 = B_SPLINE_CURVE_WITH_KNOTS ( 'NONE', 3,
 ( #61746, #46610, #19889, #51210, #41348, #14604, #36066, #45227, #3022, #39955, #24132, #61411, #18852, #57523, #45927, #34695, #9329, #56836, #56130, #7948, #45574, #67056, #40637, #62097, #15643, #59228, #57865, #69090, #37783, #26546, #64518, #11047, #142, #52237, #9682, #31819, #37430, #15302, #32171, #48309, #53250, #5080, #31147, #4060 ),
 .UNSPECIFIED., .F., .F.,
 ( 4, 2, 2, 2, 2, 2, 2, 2, 2, 2, 2, 2, 2, 2, 2, 2, 2, 2, 2, 2, 2, 4 ),
 ( 0.02814986980477068509, 0.02995274102020801035, 0.03085417662792665563, 0.03175561223564530439, 0.03355848345108267822, 0.03536135466652005899, 0.03716422588195743976, 0.03896709709739482053, 0.03986853270511350744, 0.04076996831283219436, 0.04167140392055088821, 0.04257283952826957513, 0.04347427513598826204, 0.04437571074370695590, 0.04527714635142564281, 0.04617858195914432973, 0.04798145317458171744, 0.04978432439001911902, 0.05158719560545652061, 0.05339006682089390832, 0.05519293803633130990, 0.05699580925176869761 ),
 .UNSPECIFIED. ) ;
#12734 = DIRECTION ( 'NONE',  ( 0.000000000000000000, 0.000000000000000000, -1.000000000000000000 ) ) ;
#12735 = CARTESIAN_POINT ( 'NONE',  ( -55.05276343752910151, -170.0000000000000000, 18.47277718246750311 ) ) ;
#12736 = FACE_BOUND ( 'NONE', #67574, .T. ) ;
#12737 = AXIS2_PLACEMENT_3D ( 'NONE', #58509, #15273, #6084 ) ;
#12738 = CIRCLE ( 'NONE', #23984, 65.36598343705435354 ) ;
#12739 = AXIS2_PLACEMENT_3D ( 'NONE', #11760, #33932, #1562 ) ;
#12740 = ORIENTED_EDGE ( 'NONE', *, *, #33364, .F. ) ;
#12741 = DIRECTION ( 'NONE',  ( 0.000000000000000000, 0.000000000000000000, 1.000000000000000000 ) ) ;
#12742 = CARTESIAN_POINT ( 'NONE',  ( -439.4229916354183842, 394.9999999999955094, 96.05029585799300662 ) ) ;
#12743 = AXIS2_PLACEMENT_3D ( 'NONE', #49363, #1197, #66290 ) ;
#12744 = CARTESIAN_POINT ( 'NONE',  ( 31.96192885395476324, 8.569232728322415227, -68.98636584908359737 ) ) ;
#12745 = DIRECTION ( 'NONE',  ( 1.000000000000000000, 0.000000000000000000, 0.000000000000000000 ) ) ;
#12746 = CARTESIAN_POINT ( 'NONE',  ( 207.2640160519426615, 111.6867652229576464, 56.50203771818474507 ) ) ;
#12747 = CARTESIAN_POINT ( 'NONE',  ( -149.5074843970971301, -170.0000000000000000, -22.96827994102829962 ) ) ;
#12748 = ORIENTED_EDGE ( 'NONE', *, *, #34428, .T. ) ;
#12749 = CARTESIAN_POINT ( 'NONE',  ( 59.29615173875417611, 11.84060224810188089, 3.951100658409211430 ) ) ;
#12750 = CARTESIAN_POINT ( 'NONE',  ( 201.5876148766342624, 103.8397408698165236, -36.98778679194309404 ) ) ;
#12751 = ORIENTED_EDGE ( 'NONE', *, *, #54559, .F. ) ;
#12752 =( BOUNDED_CURVE ( )  B_SPLINE_CURVE ( 3, ( #20410, #41877, #58051, #67250 ),
 .UNSPECIFIED., .F., .F. ) 
 B_SPLINE_CURVE_WITH_KNOTS ( ( 4, 4 ),
 ( 1.570796326794905440, 3.141592653589794004 ),
 .UNSPECIFIED. ) 
 CURVE ( )  GEOMETRIC_REPRESENTATION_ITEM ( )  RATIONAL_B_SPLINE_CURVE ( ( 1.000000000000000000, 0.8047378541243668248, 0.8047378541243668248, 1.000000000000000000 ) ) 
 REPRESENTATION_ITEM ( '' )  );
#12753 = CARTESIAN_POINT ( 'NONE',  ( 0.000000000000000000, 0.000000000000000000, -5.000000000000000000 ) ) ;
#12754 = ORIENTED_EDGE ( 'NONE', *, *, #12217, .T. ) ;
#12755 = CARTESIAN_POINT ( 'NONE',  ( 0.000000000000000000, 0.000000000000000000, 40.00000000000003553 ) ) ;
#12756 = CARTESIAN_POINT ( 'NONE',  ( 0.000000000000000000, 70.00000000000000000, 0.000000000000000000 ) ) ;
#12757 = CARTESIAN_POINT ( 'NONE',  ( 87.59078297315399197, 20.81577753000344799, -77.61960893227724512 ) ) ;
#12758 = VERTEX_POINT ( 'NONE', #21484 ) ;
#12759 = ORIENTED_EDGE ( 'NONE', *, *, #53426, .F. ) ;
#12760 = CARTESIAN_POINT ( 'NONE',  ( 43.96062659677686213, 10.06332325923986026, 70.23394607708451076 ) ) ;
#12761 = CARTESIAN_POINT ( 'NONE',  ( 164.9700808964341547, 65.04346068891115351, 37.19820718134189264 ) ) ;
#12762 = CARTESIAN_POINT ( 'NONE',  ( -156.8773151811563480, 72.06122063279303802, -67.73783947574408160 ) ) ;
#12763 = CARTESIAN_POINT ( 'NONE',  ( 63.99027454648603452, 13.93445177372599098, 3.016241708314831627 ) ) ;
#12764 = CARTESIAN_POINT ( 'NONE',  ( 153.2523375521184050, 55.69936538551846184, 3.858872989883677107 ) ) ;
#12765 = VERTEX_POINT ( 'NONE', #64057 ) ;
#12766 = EDGE_CURVE ( 'NONE', #2857, #3113, #37314, .T. ) ;
#12767 = CARTESIAN_POINT ( 'NONE',  ( 70.34686579112810989, 18.11777090454212313, 3.061616997868437868E-16 ) ) ;
#12768 = CARTESIAN_POINT ( 'NONE',  ( 62.04382205963242569, 13.48099884269680082, -35.76789042656609752 ) ) ;
#12769 = VECTOR ( 'NONE', #59939, 1000.000000000000114 ) ;
#12770 = CARTESIAN_POINT ( 'NONE',  ( -132.5976199670998597, 52.30296609017644016, -18.94205205907401179 ) ) ;
#12771 = DIRECTION ( 'NONE',  ( 0.4738686624729966379, 0.8805955318567391110, 0.000000000000000000 ) ) ;
#12772 = CARTESIAN_POINT ( 'NONE',  ( 117.3281529665582070, 32.29994712002883972, -14.06517866559955010 ) ) ;
#12773 = CARTESIAN_POINT ( 'NONE',  ( 94.05139011108599334, 22.08843705196240137, 89.76976943065523074 ) ) ;
#12775 = ORIENTED_EDGE ( 'NONE', *, *, #29341, .T. ) ;
#12774 = DIRECTION ( 'NONE',  ( -0.000000000000000000, 1.000000000000000000, -0.000000000000000000 ) ) ;
#12776 = ORIENTED_EDGE ( 'NONE', *, *, #2246, .F. ) ;
#12777 = ORIENTED_EDGE ( 'NONE', *, *, #32544, .F. ) ;
#12778 = VECTOR ( 'NONE', #15574, 1000.000000000000227 ) ;
#12779 = CARTESIAN_POINT ( 'NONE',  ( 43.97326221476412655, 9.047815246749991047, 16.53542767223330046 ) ) ;
#12780 = CARTESIAN_POINT ( 'NONE',  ( -178.6094373798883623, 95.02303223604788229, 86.89060986716357604 ) ) ;
#12781 = DIRECTION ( 'NONE',  ( 0.000000000000000000, 0.000000000000000000, -1.000000000000000000 ) ) ;
#12782 = CARTESIAN_POINT ( 'NONE',  ( 103.5588133492864671, 25.91050225236393345, -20.01717663906335787 ) ) ;
#12783 = CARTESIAN_POINT ( 'NONE',  ( 197.6145711261845292, 97.10888456119687362, 7.316670231408826552 ) ) ;
#12785 = EDGE_CURVE ( 'NONE', #68142, #60670, #36778, .T. ) ;
#12784 = AXIS2_PLACEMENT_3D ( 'NONE', #26372, #49179, #54102 ) ;
#12786 = CARTESIAN_POINT ( 'NONE',  ( 211.3754067703094108, 117.8127004712419819, 93.81656004356196377 ) ) ;
#12787 = AXIS2_PLACEMENT_3D ( 'NONE', #29347, #56779, #14551 ) ;
#12788 = EDGE_CURVE ( 'NONE', #35305, #62075, #59114, .T. ) ;
#12789 = DIRECTION ( 'NONE',  ( -0.000000000000000000, 1.000000000000000000, -0.000000000000000000 ) ) ;
#12790 = CARTESIAN_POINT ( 'NONE',  ( -75.43953471070999228, 21.11829282998124668, -76.24709388609002758 ) ) ;
#12791 = CARTESIAN_POINT ( 'NONE',  ( -12.78015296493258290, 7.264294661536300879, 43.26710858275960447 ) ) ;
#12792 = ORIENTED_EDGE ( 'NONE', *, *, #35023, .F. ) ;
#12793 = VECTOR ( 'NONE', #14214, 1000.000000000000000 ) ;
#12794 = CARTESIAN_POINT ( 'NONE',  ( 86.62931800182293784, 20.48449268398423584, -35.82156419891171595 ) ) ;
#12795 = VERTEX_POINT ( 'NONE', #43629 ) ;
#12796 = VERTEX_POINT ( 'NONE', #32743 ) ;
#12797 = CARTESIAN_POINT ( 'NONE',  ( 63.01563776193091826, 13.70579113808095073, -23.87614024170608218 ) ) ;
#12798 = CARTESIAN_POINT ( 'NONE',  ( 183.9887307715837039, 83.05100282186909055, -63.65145494335473586 ) ) ;
#12799 = AXIS2_PLACEMENT_3D ( 'NONE', #37614, #63674, #58717 ) ;
#12800 = CARTESIAN_POINT ( 'NONE',  ( -167.1619226259399227, 82.18315278115417755, 33.76076489396710656 ) ) ;
#12801 = EDGE_CURVE ( 'NONE', #30210, #58410, #28151, .T. ) ;
#12802 = CARTESIAN_POINT ( 'NONE',  ( 117.3246714514015849, 33.42485879931864190, -19.09944304000492821 ) ) ;
#12803 = CARTESIAN_POINT ( 'NONE',  ( -44.99999999999998579, -25.00000000000000000, 2.000000000000015543 ) ) ;
#12804 = CARTESIAN_POINT ( 'NONE',  ( 0.000000000000000000, 0.000000000000000000, 0.000000000000000000 ) ) ;
#12805 = CARTESIAN_POINT ( 'NONE',  ( 139.3041645503688528, 46.00819478311336042, -21.83978754804469702 ) ) ;
#12806 = ORIENTED_EDGE ( 'NONE', *, *, #36825, .F. ) ;
#12807 = ORIENTED_EDGE ( 'NONE', *, *, #56224, .T. ) ;
#12808 = EDGE_LOOP ( 'NONE', ( #2644, #35837 ) ) ;
#12809 = DIRECTION ( 'NONE',  ( 0.5877852522924802425, -0.8090169943749422332, 2.500042656554809847E-16 ) ) ;
#12810 = LINE ( 'NONE', #1918, #36419 ) ;
#12811 = DIRECTION ( 'NONE',  ( 0.000000000000000000, 0.000000000000000000, 1.000000000000000000 ) ) ;
#12812 = CARTESIAN_POINT ( 'NONE',  ( 62.04326772936978784, 12.44884401098615179, -23.82859654250995973 ) ) ;
#12813 = EDGE_CURVE ( 'NONE', #51672, #64960, #59807, .T. ) ;
#12814 = B_SPLINE_CURVE_WITH_KNOTS ( 'NONE', 3,
 ( #26343, #68883, #31281, #16469, #4199, #26001, #68558, #15778, #5561, #37577, #47778, #64661, #15445, #37224, #10492, #31964, #59024, #53390, #10840, #9475, #30935, #25663, #47096, #20361, #41828, #63284, #15096, #36552, #58004, #9823, #52707, #47428, #42168, #46716, #19286, #41449, #51994, #40744, #8402, #57281, #56231, #62902, #30543, #46024, #56938, #61517, #51657 ),
 .UNSPECIFIED., .F., .F.,
 ( 4, 2, 2, 2, 2, 2, 2, 2, 2, 2, 2, 2, 1, 2, 2, 2, 2, 2, 2, 2, 2, 2, 2, 4 ),
 ( 0.000000000000000000, 0.001493793014771570673, 0.002240689522157353081, 0.002987586029543135707, 0.004481379044314673203, 0.005228275551700448456, 0.005975172059086222842, 0.007468965073857801971, 0.008215861581243587633, 0.008962758088629372427, 0.01045655110340091946, 0.01120344761078670252, 0.01195034411817248732, 0.01269724062555827211, 0.01344413713294406211, 0.01493793014771565252, 0.01568482665510143731, 0.01643172316248721690, 0.01792551617725878302, 0.01941930919203034914, 0.02016620569941613914, 0.02091310220680193260, 0.02240689522157351954, 0.02390068823634510300 ),
 .UNSPECIFIED. ) ;
#12815 = UNCERTAINTY_MEASURE_WITH_UNIT (LENGTH_MEASURE( 1.000000000000000082E-05 ), #48462, 'distance_accuracy_value', 'NONE');
#12816 = DIRECTION ( 'NONE',  ( -0.000000000000000000, -0.000000000000000000, -1.000000000000000000 ) ) ;
#12817 = EDGE_CURVE ( 'NONE', #8346, #30965, #60372, .T. ) ;
#12818 = CARTESIAN_POINT ( 'NONE',  ( -8.000000000000000000, -0.7805016046291022302, -9.500000000000003553 ) ) ;
#12819 = EDGE_CURVE ( 'NONE', #23331, #35061, #33095, .T. ) ;
#12820 = ORIENTED_EDGE ( 'NONE', *, *, #31011, .T. ) ;
#12821 = DIRECTION ( 'NONE',  ( 0.6910626489868580968, 0.7227948638273978821, 0.000000000000000000 ) ) ;
#12822 = CARTESIAN_POINT ( 'NONE',  ( -62.29496909743952671, 17.79481128341706153, -67.59550361844860333 ) ) ;
#12823 = CARTESIAN_POINT ( 'NONE',  ( 180.2473887773228114, 77.76029175826236894, -63.06960825634326540 ) ) ;
#12824 = CARTESIAN_POINT ( 'NONE',  ( -173.1211646369891071, 87.12891641440859303, -34.71195716474998960 ) ) ;
#12825 = LINE ( 'NONE', #53187, #68882 ) ;
#12826 = CARTESIAN_POINT ( 'NONE',  ( -171.4867114763003997, 85.32693843184996751, 4.145646873760804318 ) ) ;
#12827 = DIRECTION ( 'NONE',  ( 0.000000000000000000, 0.000000000000000000, -1.000000000000000000 ) ) ;
#12828 = FACE_BOUND ( 'NONE', #48721, .T. ) ;
#12829 = CARTESIAN_POINT ( 'NONE',  ( -189.2550107216115407, 107.1111757360096703, 92.75985481009226419 ) ) ;
#12830 = VECTOR ( 'NONE', #65445, 1000.000000000000000 ) ;
#12831 = CARTESIAN_POINT ( 'NONE',  ( -6.126800896373023164, 6.786243985899684361, 57.15086958430494235 ) ) ;
#12832 = ORIENTED_EDGE ( 'NONE', *, *, #2302, .F. ) ;
#12834 = CARTESIAN_POINT ( 'NONE',  ( 278.6977768404063340, 21.46141967451381305, -4.838576272177869342 ) ) ;
#12833 = AXIS2_PLACEMENT_3D ( 'NONE', #23455, #44893, #66375 ) ;
#12835 = CARTESIAN_POINT ( 'NONE',  ( 290.0000000000000568, 5.000000000000000888, 18.50000000000000000 ) ) ;
#12836 = CARTESIAN_POINT ( 'NONE',  ( 39.40195752203892710, -170.0000000000000000, -69.96436805589145536 ) ) ;
#12837 = DIRECTION ( 'NONE',  ( -0.8584487936018727616, 0.5128992774058949156, 0.000000000000000000 ) ) ;
#12838 = CARTESIAN_POINT ( 'NONE',  ( 230.9999999999999432, 0.000000000000000000, 0.000000000000000000 ) ) ;
#12839 = VECTOR ( 'NONE', #64526, 1000.000000000000000 ) ;
#12840 = ORIENTED_EDGE ( 'NONE', *, *, #53641, .F. ) ;
#12841 = VECTOR ( 'NONE', #23232, 1000.000000000000000 ) ;
#12842 = CARTESIAN_POINT ( 'NONE',  ( 0.4973051450610691537, -3.866309095671421669, -8.000000000000001776 ) ) ;
#12843 = AXIS2_PLACEMENT_3D ( 'NONE', #50297, #2117, #23567 ) ;
#12844 = LINE ( 'NONE', #44121, #37169 ) ;
#12845 = VERTEX_POINT ( 'NONE', #54531 ) ;
#12846 = ORIENTED_EDGE ( 'NONE', *, *, #66990, .F. ) ;
#12847 = CIRCLE ( 'NONE', #24040, 65.00000000000000000 ) ;
#12848 = CARTESIAN_POINT ( 'NONE',  ( -6.000000000000000000, 23.07878402833891229, -5.000000000000000000 ) ) ;
#12849 = CARTESIAN_POINT ( 'NONE',  ( -180.3153482337534967, 95.51031295027651424, -66.91522547114587383 ) ) ;
#12850 = DIRECTION ( 'NONE',  ( -0.000000000000000000, -0.000000000000000000, -1.000000000000000000 ) ) ;
#12851 = VERTEX_POINT ( 'NONE', #22536 ) ;
#12852 = DIRECTION ( 'NONE',  ( -0.000000000000000000, -0.000000000000000000, -1.000000000000000000 ) ) ;
#12853 = DIRECTION ( 'NONE',  ( -0.000000000000000000, -0.000000000000000000, 1.000000000000000000 ) ) ;
#12854 = CARTESIAN_POINT ( 'NONE',  ( -1.319107422865895218, 6.554467368239826008, 7.008176618785499912 ) ) ;
#12855 = CARTESIAN_POINT ( 'NONE',  ( -79.61235761536670452, 23.76245710489568452, 30.46282415610054883 ) ) ;
#12856 = CARTESIAN_POINT ( 'NONE',  ( 88.99522780200241812, 20.24180937454204354, -36.20046504712779267 ) ) ;
#12857 = CARTESIAN_POINT ( 'NONE',  ( -47.94536219817735656, 13.92422159065987231, -18.31751929704889292 ) ) ;
#12858 = EDGE_CURVE ( 'NONE', #31241, #21633, #44666, .T. ) ;
#12859 = B_SPLINE_CURVE_WITH_KNOTS ( 'NONE', 3,
 ( #27715, #12248, #11188, #49157, #996, #43883, #65369, #17152, #38625, #2051, #23852, #45290, #50228, #13978, #12954, #23504, #44946, #35439, #56899, #29121, #40364, #66430, #34414, #8366, #24551, #18221, #61810, #24888, #50921, #29814, #39671, #61479, #29463, #8715, #56191, #56539, #50572, #51276, #30167, #13300, #55859, #13628, #3088, #45987, #61126 ),
 .UNSPECIFIED., .F., .F.,
 ( 4, 2, 2, 2, 2, 2, 2, 2, 2, 2, 2, 1, 2, 2, 2, 2, 2, 2, 2, 2, 2, 2, 4 ),
 ( 0.000000000000000000, 0.001512548138464682489, 0.002268822207697023842, 0.003025096276929364978, 0.004537644415394018194, 0.005293918484626360631, 0.006050192553858702200, 0.007562740692323368860, 0.009075288830788036387, 0.01058783696925270565, 0.01134411103848502814, 0.01210038510771735236, 0.01285665917694967832, 0.01361293324618200427, 0.01512548138464661976, 0.01588175545387892837, 0.01663802952311124045, 0.01815057766157585767, 0.01966312580004047836, 0.02041939986927279044, 0.02117567393850510599, 0.02268822207696976137, 0.02420077021543442022 ),
 .UNSPECIFIED. ) ;
#12860 = ORIENTED_EDGE ( 'NONE', *, *, #50914, .T. ) ;
#12862 = EDGE_CURVE ( 'NONE', #52936, #36476, #16571, .T. ) ;
#12861 = CARTESIAN_POINT ( 'NONE',  ( 116.1021807117071774, 31.68810634233423684, -38.71412669113463068 ) ) ;
#12863 = CARTESIAN_POINT ( 'NONE',  ( -71.27103490383370854, 20.70545763375145398, 12.34733277340642665 ) ) ;
#12864 = CARTESIAN_POINT ( 'NONE',  ( 43.97326221476411945, 9.047815246749959073, -37.15367350869404817 ) ) ;
#12865 = CARTESIAN_POINT ( 'NONE',  ( -422.6627218934913230, 1.665334536937734811E-13, 108.5502958579881749 ) ) ;
#12867 = ORIENTED_EDGE ( 'NONE', *, *, #35697, .F. ) ;
#12866 = CARTESIAN_POINT ( 'NONE',  ( -125.3944660332519447, 46.16494358222053762, 84.30437107587852097 ) ) ;
#12868 = CARTESIAN_POINT ( 'NONE',  ( 85.67452303415196013, 19.09699411916382772, -35.86737280937732208 ) ) ;
#12869 = ORIENTED_EDGE ( 'NONE', *, *, #554, .T. ) ;
#12870 = CARTESIAN_POINT ( 'NONE',  ( -147.7845268487069461, 62.73119438705056439, 72.37768481507308138 ) ) ;
#12871 = CARTESIAN_POINT ( 'NONE',  ( 81.04027388895738682, 18.64386073872847760, 42.23734901537720532 ) ) ;
#12872 = LINE ( 'NONE', #67381, #29833 ) ;
#12873 = EDGE_CURVE ( 'NONE', #67246, #34459, #3595, .T. ) ;
#12874 = DIRECTION ( 'NONE',  ( 1.000000000000000000, 1.387778780781445676E-16, 0.000000000000000000 ) ) ;
#12875 = EDGE_CURVE ( 'NONE', #65549, #44262, #29212, .T. ) ;
#12876 = CARTESIAN_POINT ( 'NONE',  ( 139.1353280997809634, 44.70436000187870462, -11.34540700426408932 ) ) ;
#12877 = CARTESIAN_POINT ( 'NONE',  ( 230.9999999999999432, 192.0000000000000000, 0.000000000000000000 ) ) ;
#12878 = CARTESIAN_POINT ( 'NONE',  ( -179.8989115484066872, 96.59045402602909292, -12.14446317899465733 ) ) ;
#12879 = AXIS2_PLACEMENT_3D ( 'NONE', #16393, #38187, #37846 ) ;
#12880 = CARTESIAN_POINT ( 'NONE',  ( 0.000000000000000000, 0.000000000000000000, 43.58025477438756212 ) ) ;
#12881 = ORIENTED_EDGE ( 'NONE', *, *, #65354, .F. ) ;
#12882 = ORIENTED_EDGE ( 'NONE', *, *, #3026, .F. ) ;
#12883 = ADVANCED_FACE ( 'NONE', ( #44330 ), #65817, .F. ) ;
#12884 = CARTESIAN_POINT ( 'NONE',  ( 10.55634918610397577, -31.11269837220809364, 2.000000000000000000 ) ) ;
#12885 = DIRECTION ( 'NONE',  ( -1.357354004351002108E-18, 4.918261777702510883E-18, -1.000000000000000000 ) ) ;
#12886 = FACE_OUTER_BOUND ( 'NONE', #67029, .T. ) ;
#12887 = CARTESIAN_POINT ( 'NONE',  ( 207.4610690199661747, 111.9701171077051924, -36.84174272876874312 ) ) ;
#12888 = LINE ( 'NONE', #6557, #6793 ) ;
#12889 = CARTESIAN_POINT ( 'NONE',  ( -108.0980548770427987, 35.83569586822709141, 69.62243089452121581 ) ) ;
#12890 =( GEOMETRIC_REPRESENTATION_CONTEXT ( 3 ) GLOBAL_UNCERTAINTY_ASSIGNED_CONTEXT ( ( #45856 ) ) GLOBAL_UNIT_ASSIGNED_CONTEXT ( ( #67079, #13588, #18869 ) ) REPRESENTATION_CONTEXT ( 'NONE', 'WORKASPACE' ) );
#12891 = CARTESIAN_POINT ( 'NONE',  ( -28.35330809568270638, 9.105138953156432180, -35.97708236689904027 ) ) ;
#12892 = CARTESIAN_POINT ( 'NONE',  ( -65.36598343705435354, 0.000000000000000000, 41.38025477438755928 ) ) ;
#12893 = ORIENTED_EDGE ( 'NONE', *, *, #10483, .F. ) ;
#12894 = EDGE_LOOP ( 'NONE', ( #27729, #38228, #17677, #63180 ) ) ;
#12895 = CIRCLE ( 'NONE', #18509, 65.00000000000000000 ) ;
#12896 = EDGE_LOOP ( 'NONE', ( #41554, #46784, #22278, #37922 ) ) ;
#12897 = PLANE ( 'NONE',  #33004 ) ;
#12898 = VECTOR ( 'NONE', #28139, 1000.000000000000227 ) ;
#12899 = CARTESIAN_POINT ( 'NONE',  ( -75.69395121710529395, 21.21099447234451318, 84.69349098787803598 ) ) ;
#12900 = LINE ( 'NONE', #34704, #47549 ) ;
#12901 = CARTESIAN_POINT ( 'NONE',  ( -41.05116106442372370, -31.37049930917697083, 26.66469066592269144 ) ) ;
#12902 = DIRECTION ( 'NONE',  ( 1.000000000000000000, 1.387778780781445676E-16, -1.110223024625156294E-16 ) ) ;
#12903 = CARTESIAN_POINT ( 'NONE',  ( 6.400000000000000355, 4.618802153517001408, -8.000000000000000000 ) ) ;
#12904 = CARTESIAN_POINT ( 'NONE',  ( -99.10674985723794350, 32.31836975419499680, -22.48196502616453785 ) ) ;
#12905 = EDGE_CURVE ( 'NONE', #52426, #26511, #7420, .T. ) ;
#12906 = ADVANCED_FACE ( 'NONE', ( #19001 ), #17611, .T. ) ;
#12907 = EDGE_CURVE ( 'NONE', #66812, #69029, #47186, .T. ) ;
#12908 = CARTESIAN_POINT ( 'NONE',  ( 55.77012379229940819, 12.13428856597100669, 39.26591085917196011 ) ) ;
#12909 = CARTESIAN_POINT ( 'NONE',  ( 40.06683191176360737, 8.496734820196639504, 83.62526394863175483 ) ) ;
#12910 = CARTESIAN_POINT ( 'NONE',  ( 33.53140150161104316, 18.57796495195515618, 13.32819397642333747 ) ) ;
#12911 = ORIENTED_EDGE ( 'NONE', *, *, #15175, .T. ) ;
#12912 = LINE ( 'NONE', #5865, #11545 ) ;
#12913 = LINE ( 'NONE', #62114, #64422 ) ;
#12915 = EDGE_CURVE ( 'NONE', #52201, #3613, #58891, .T. ) ;
#12914 = CARTESIAN_POINT ( 'NONE',  ( -14.56151485655250255, 8.434196591921333308, 7.436944112387903871 ) ) ;
#12916 = PLANE ( 'NONE',  #54578 ) ;
#12917 = CARTESIAN_POINT ( 'NONE',  ( -103.2169245450825343, 33.25885825286820108, -76.81501985536182531 ) ) ;
#12918 = CARTESIAN_POINT ( 'NONE',  ( 132.0563630623056781, 41.51825634609595284, -23.96314219444095883 ) ) ;
#12919 = EDGE_LOOP ( 'NONE', ( #14814, #33641, #50662, #31863 ) ) ;
#12920 = CARTESIAN_POINT ( 'NONE',  ( 697.7645910007584007, 891.0064415309029755, 698.5068267248682332 ) ) ;
#12921 = CARTESIAN_POINT ( 'NONE',  ( 15.55634918610397399, -31.11269837220809364, 2.000000000000001776 ) ) ;
#12922 = LINE ( 'NONE', #12563, #63487 ) ;
#12923 = CARTESIAN_POINT ( 'NONE',  ( 0.08224679563971618035, -7.710515798486367700, -2.644994884459106910 ) ) ;
#12924 = ITEM_DEFINED_TRANSFORMATION ( 'NONE', 'NONE', #47854,  #66832 ) ;
#12925 = CARTESIAN_POINT ( 'NONE',  ( -166.1340766777337024, 79.67347379767349480, 89.26157043849886463 ) ) ;
#12926 = EDGE_LOOP ( 'NONE', ( #24749, #49931, #4449, #16861, #54293, #15648 ) ) ;
#12927 = CARTESIAN_POINT ( 'NONE',  ( -120.1259246007803227, 42.81147313035988589, -37.59277727144264958 ) ) ;
#12928 = CARTESIAN_POINT ( 'NONE',  ( -142.0251973982165623, 58.08401473564116202, -16.05535940763569158 ) ) ;
#12929 = CARTESIAN_POINT ( 'NONE',  ( -0.7076388175553578463, 7.538734751903871434, -72.17698391732507446 ) ) ;
#12930 = CIRCLE ( 'NONE', #35366, 5.000000000000004441 ) ;
#12931 = CARTESIAN_POINT ( 'NONE',  ( 0.000000000000000000, 0.000000000000000000, 41.38025477438755928 ) ) ;
#12932 = VERTEX_POINT ( 'NONE', #24983 ) ;
#12933 = CARTESIAN_POINT ( 'NONE',  ( -56.72676045871359918, 16.18052435693490665, 3.657967166041028229 ) ) ;
#12934 = CARTESIAN_POINT ( 'NONE',  ( 0.000000000000000000, -31.50328976398030534, -9.999999999999998224 ) ) ;
#12935 = VECTOR ( 'NONE', #50668, 1000.000000000000000 ) ;
#12936 = DIRECTION ( 'NONE',  ( 1.261617073437677999E-16, 0.000000000000000000, 1.000000000000000000 ) ) ;
#12937 = CARTESIAN_POINT ( 'NONE',  ( 23.23895241123075905, 6.853530908437206470, -44.00714248153148134 ) ) ;
#12938 = VECTOR ( 'NONE', #34200, 1000.000000000000114 ) ;
#12940 = EDGE_LOOP ( 'NONE', ( #6089, #37237 ) ) ;
#12939 = CARTESIAN_POINT ( 'NONE',  ( -56.97107423601132581, 15.20373812575555839, 3.706198643034869011 ) ) ;
#12941 =( GEOMETRIC_REPRESENTATION_CONTEXT ( 3 ) GLOBAL_UNCERTAINTY_ASSIGNED_CONTEXT ( ( #50779 ) ) GLOBAL_UNIT_ASSIGNED_CONTEXT ( ( #35744, #8668, #15315 ) ) REPRESENTATION_CONTEXT ( 'NONE', 'WORKASPACE' ) );
#12942 = CARTESIAN_POINT ( 'NONE',  ( 0.000000000000000000, 0.000000000000000000, -2.000000000000000000 ) ) ;
#12943 = VECTOR ( 'NONE', #47430, 1000.000000000000000 ) ;
#12944 = VERTEX_POINT ( 'NONE', #35874 ) ;
#12945 = ORIENTED_EDGE ( 'NONE', *, *, #66738, .F. ) ;
#12947 = EDGE_CURVE ( 'NONE', #34313, #35904, #63649, .T. ) ;
#12946 = DIRECTION ( 'NONE',  ( -0.000000000000000000, 0.000000000000000000, -1.000000000000000000 ) ) ;
#12948 = AXIS2_PLACEMENT_3D ( 'NONE', #36428, #57883, #43795 ) ;
#12949 = CARTESIAN_POINT ( 'NONE',  ( -34.73299709025328497, 11.17736532835359320, -89.76496422446544443 ) ) ;
#12951 = ORIENTED_EDGE ( 'NONE', *, *, #31782, .F. ) ;
#12950 = DIRECTION ( 'NONE',  ( 1.000000000000000000, 0.000000000000000000, -0.000000000000000000 ) ) ;
#12952 = DIRECTION ( 'NONE',  ( -0.000000000000000000, -0.000000000000000000, -1.000000000000000000 ) ) ;
#12953 = CARTESIAN_POINT ( 'NONE',  ( -30.94745021534355800, 10.53010394565407282, 45.21645440618919309 ) ) ;
#12954 = CARTESIAN_POINT ( 'NONE',  ( -72.78270026377323632, 21.23376443558121451, -37.93819681164344360 ) ) ;
#12955 = ORIENTED_EDGE ( 'NONE', *, *, #42458, .F. ) ;
#12956 = CARTESIAN_POINT ( 'NONE',  ( 211.8345664497466316, 118.5225165986914391, -72.99828217273564235 ) ) ;
#12957 = EDGE_CURVE ( 'NONE', #34803, #30932, #56987, .T. ) ;
#12958 = FACE_OUTER_BOUND ( 'NONE', #68382, .T. ) ;
#12959 = CARTESIAN_POINT ( 'NONE',  ( -173.1211646369891355, 88.63826465341152527, 45.82169460664104577 ) ) ;
#12960 = DIRECTION ( 'NONE',  ( 0.000000000000000000, 0.000000000000000000, 1.000000000000000000 ) ) ;
#12961 = EDGE_CURVE ( 'NONE', #28268, #20719, #62643, .T. ) ;
#12962 = CARTESIAN_POINT ( 'NONE',  ( 17.48988570800758424, 7.568061572928495906, 71.66776098152827501 ) ) ;
#12963 = ORIENTED_EDGE ( 'NONE', *, *, #4208, .F. ) ;
#12964 = ADVANCED_FACE ( 'NONE', ( #41498 ), #31295, .T. ) ;
#12965 = ORIENTED_EDGE ( 'NONE', *, *, #14226, .T. ) ;
#12966 = ORIENTED_EDGE ( 'NONE', *, *, #56443, .T. ) ;
#12967 = CARTESIAN_POINT ( 'NONE',  ( 210.6484376398113625, 114.8762597311295366, -92.94483523309006046 ) ) ;
#12968 = CARTESIAN_POINT ( 'NONE',  ( -32.41982179707236611, 9.753975577087194537, -50.26874347964162837 ) ) ;
#12969 = LINE ( 'NONE', #34432, #30403 ) ;
#12970 = CARTESIAN_POINT ( 'NONE',  ( -142.6264002846223775, 58.55577336362199503, 35.22544109792448097 ) ) ;
#12971 = DIRECTION ( 'NONE',  ( 0.000000000000000000, 0.000000000000000000, -1.000000000000000000 ) ) ;
#12972 = CARTESIAN_POINT ( 'NONE',  ( 563.4809901518626702, 190.0000000000000000, 57.79371821540657095 ) ) ;
#12973 = ORIENTED_EDGE ( 'NONE', *, *, #3493, .T. ) ;
#12974 = CARTESIAN_POINT ( 'NONE',  ( 84.05098130332766004, 18.55728792516086756, 71.10367255945043041 ) ) ;
#12975 = ORIENTED_EDGE ( 'NONE', *, *, #17452, .F. ) ;
#12976 = AXIS2_PLACEMENT_3D ( 'NONE', #51362, #18657, #35529 ) ;
#12977 = CARTESIAN_POINT ( 'NONE',  ( 32.29989959354726636, 7.591763852038292626, 39.83690252976357726 ) ) ;
#12978 = CARTESIAN_POINT ( 'NONE',  ( -20.55634918610411077, -46.66904755831208718, 85.00100000000000477 ) ) ;
#12979 = LINE ( 'NONE', #66803, #354 ) ;
#12980 = CARTESIAN_POINT ( 'NONE',  ( -3.841371665203041630E-11, 0.000000000000000000, 10.00000000000000000 ) ) ;
#12981 = AXIS2_PLACEMENT_3D ( 'NONE', #37255, #53428, #3885 ) ;
#12982 = CARTESIAN_POINT ( 'NONE',  ( -119.1605144823340083, 43.39823405392971267, 61.65073838172952492 ) ) ;
#12983 = CARTESIAN_POINT ( 'NONE',  ( -47.55360235114365963, 12.79819361309566617, 10.46016547731527702 ) ) ;
#12984 = FACE_OUTER_BOUND ( 'NONE', #19722, .T. ) ;
#12985 = ADVANCED_FACE ( 'NONE', ( #4548 ), #9490, .F. ) ;
#12987 = CARTESIAN_POINT ( 'NONE',  ( 0.000000000000000000, 0.000000000000000000, 0.000000000000000000 ) ) ;
#12986 = VECTOR ( 'NONE', #17139, 1000.000000000000000 ) ;
#12988 = AXIS2_PLACEMENT_3D ( 'NONE', #28204, #55634, #23640 ) ;
#12989 = ORIENTED_EDGE ( 'NONE', *, *, #36999, .T. ) ;
#12990 = DIRECTION ( 'NONE',  ( -0.2225209339563184729, 0.9749279121818227312, 0.000000000000000000 ) ) ;
#12991 = CARTESIAN_POINT ( 'NONE',  ( -155.2912910578197057, 69.24479901948497229, -10.68701328854503174 ) ) ;
#12992 = ORIENTED_EDGE ( 'NONE', *, *, #26604, .F. ) ;
#12993 = AXIS2_PLACEMENT_3D ( 'NONE', #24255, #45696, #18962 ) ;
#12994 = CARTESIAN_POINT ( 'NONE',  ( -44.99999999999998579, 25.00000000000000000, 2.000000000000015543 ) ) ;
#12995 = CARTESIAN_POINT ( 'NONE',  ( -60.98168946575805904, 17.40090852531919552, 69.28151032968872869 ) ) ;
#12997 = EDGE_CURVE ( 'NONE', #10658, #4373, #11055, .T. ) ;
#12996 = LINE ( 'NONE', #13338, #8367 ) ;
#12998 = VERTEX_POINT ( 'NONE', #43197 ) ;
#12999 = DIRECTION ( 'NONE',  ( 0.000000000000000000, 0.000000000000000000, -1.000000000000000000 ) ) ;
#13000 = CIRCLE ( 'NONE', #52291, 74.95140232871122521 ) ;
#13001 = CARTESIAN_POINT ( 'NONE',  ( -12.78015296493257402, 7.264294661536300879, -64.11109377909512830 ) ) ;
#13002 = CARTESIAN_POINT ( 'NONE',  ( -38.16002576456689610, 10.79155573432543491, 34.37876793671505737 ) ) ;
#13003 = CARTESIAN_POINT ( 'NONE',  ( -27.70005010046228833, 9.007417901453017350, 71.06713019032800105 ) ) ;
#13004 = VECTOR ( 'NONE', #11626, 1000.000000000000000 ) ;
#13005 = APPLICATION_CONTEXT ( 'automotive_design' ) ;
#13006 = ORIENTED_EDGE ( 'NONE', *, *, #22230, .T. ) ;
#13007 =( NAMED_UNIT ( * ) SI_UNIT ( $, .STERADIAN. ) SOLID_ANGLE_UNIT ( ) );
#13008 = CARTESIAN_POINT ( 'NONE',  ( -118.3927673406137302, 41.74929850983304647, 38.35786790901878618 ) ) ;
#13009 = ORIENTED_EDGE ( 'NONE', *, *, #49203, .T. ) ;
#13010 = CYLINDRICAL_SURFACE ( 'NONE', #17739, 7.500000000000013323 ) ;
#13011 = DIRECTION ( 'NONE',  ( 1.000000000000000000, 0.000000000000000000, 0.000000000000000000 ) ) ;
#13012 = CARTESIAN_POINT ( 'NONE',  ( -4.071369321747701164, 7.682719369516283869, 17.28235958677781525 ) ) ;
#13013 = CARTESIAN_POINT ( 'NONE',  ( 88.52345267551653762, 20.07594890262052800, 56.79578933626290649 ) ) ;
#13014 = CARTESIAN_POINT ( 'NONE',  ( 15.55634918610396511, -41.66904755831214402, 2.000000000000001776 ) ) ;
#13015 = CARTESIAN_POINT ( 'NONE',  ( 3.000000000000028866, 0.000000000000000000, -3.000000000000030198 ) ) ;
#13016 = LINE ( 'NONE', #49929, #20048 ) ;
#13017 = ORIENTED_EDGE ( 'NONE', *, *, #59463, .T. ) ;
#13018 = CARTESIAN_POINT ( 'NONE',  ( 164.9534461562627143, 63.71129898458563190, -17.35706065313273783 ) ) ;
#13019 = FACE_OUTER_BOUND ( 'NONE', #6249, .T. ) ;
#13020 = CARTESIAN_POINT ( 'NONE',  ( 65.62848231372477414, 13.29388722724787719, 57.12320672528056775 ) ) ;
#13021 = CARTESIAN_POINT ( 'NONE',  ( -126.3063800003736077, 47.97292241606065488, -88.60280507916129977 ) ) ;
#13022 = DIRECTION ( 'NONE',  ( 0.000000000000000000, -0.000000000000000000, 1.000000000000000000 ) ) ;
#13023 = PRODUCT_RELATED_PRODUCT_CATEGORY ( 'part', '', ( #30563 ) ) ;
#13024 = ORIENTED_EDGE ( 'NONE', *, *, #61996, .F. ) ;
#13025 = EDGE_CURVE ( 'NONE', #60434, #18072, #48054, .T. ) ;
#13026 = CARTESIAN_POINT ( 'NONE',  ( 157.4703587214989113, 58.92748579479260229, -9.279633708673953763 ) ) ;
#13027 = FACE_OUTER_BOUND ( 'NONE', #36972, .T. ) ;
#13028 = ORIENTED_EDGE ( 'NONE', *, *, #66972, .T. ) ;
#13029 = AXIS2_PLACEMENT_3D ( 'NONE', #6180, #59296, #49077 ) ;
#13031 = ADVANCED_FACE ( 'NONE', ( #56198 ), #1348, .F. ) ;
#13030 = CARTESIAN_POINT ( 'NONE',  ( -60.65612136648954333, 16.25551606627059087, -64.55169377915926532 ) ) ;
#13032 = DIRECTION ( 'NONE',  ( 0.000000000000000000, 0.000000000000000000, 1.000000000000000000 ) ) ;
#13033 = CIRCLE ( 'NONE', #63580, 242.4895526022646379 ) ;
#13034 = ORIENTED_EDGE ( 'NONE', *, *, #49141, .F. ) ;
#13035 = CARTESIAN_POINT ( 'NONE',  ( -142.9730935922299579, 58.82921737386681826, -65.46680488933378683 ) ) ;
#13036 = CARTESIAN_POINT ( 'NONE',  ( 87.11228333101215071, 19.58587579906928866, 17.86753698201565399 ) ) ;
#13037 = DIRECTION ( 'NONE',  ( -0.000000000000000000, -0.000000000000000000, 1.000000000000000000 ) ) ;
#13038 = CIRCLE ( 'NONE', #25394, 10.00000000000000178 ) ;
#13039 = ORIENTED_EDGE ( 'NONE', *, *, #35506, .T. ) ;
#13040 = AXIS2_PLACEMENT_3D ( 'NONE', #11853, #27332, #58997 ) ;
#13041 = CARTESIAN_POINT ( 'NONE',  ( -98.68609963468202295, 32.11186931716881787, 17.77450552764720371 ) ) ;
#13042 = CARTESIAN_POINT ( 'NONE',  ( 69.71545454699229083, 15.36735235725339699, 87.61477549632385831 ) ) ;
#13043 = CARTESIAN_POINT ( 'NONE',  ( 32.66364305947234925, 8.639871491745262588, 40.74384643876327772 ) ) ;
#13044 = AXIS2_PLACEMENT_3D ( 'NONE', #38825, #34938, #28253 ) ;
#13045 = CARTESIAN_POINT ( 'NONE',  ( 81.76212856587196143, 18.87332718082996408, -22.18841434000387025 ) ) ;
#13046 = CARTESIAN_POINT ( 'NONE',  ( 110.2429982417149574, -170.0000000000000000, 2.766663615273646126 ) ) ;
#13047 = CARTESIAN_POINT ( 'NONE',  ( 151.7956716830626362, 53.36999433148316285, 68.66416584447760840 ) ) ;
#13048 = EDGE_CURVE ( 'NONE', #67011, #5837, #34760, .T. ) ;
#13049 = FACE_OUTER_BOUND ( 'NONE', #2371, .T. ) ;
#13050 = VERTEX_POINT ( 'NONE', #66438 ) ;
#13051 = FACE_BOUND ( 'NONE', #60200, .T. ) ;
#13053 = EDGE_CURVE ( 'NONE', #41640, #4543, #15655, .T. ) ;
#13052 = CARTESIAN_POINT ( 'NONE',  ( -11.13714165684777768, 8.138643170880696331, 57.72645611657431886 ) ) ;
#13054 = VERTEX_POINT ( 'NONE', #18226 ) ;
#13055 = CARTESIAN_POINT ( 'NONE',  ( -149.5074843970970733, 65.50121172469319220, -34.81283053149196149 ) ) ;
#13056 = CARTESIAN_POINT ( 'NONE',  ( 29.99999999999999645, -30.00000000000000355, 15.00000000000000000 ) ) ;
#13057 = CARTESIAN_POINT ( 'NONE',  ( -1.455067768715155863, 7.566780179921178906, 41.58164679007672504 ) ) ;
#13058 = CARTESIAN_POINT ( 'NONE',  ( -13.97522410592632625, 7.369766281240364592, -92.29298810122654118 ) ) ;
#13059 = CARTESIAN_POINT ( 'NONE',  ( -47.60396279792517760, 12.80997843568595940, -70.56710525558601432 ) ) ;
#13060 = CARTESIAN_POINT ( 'NONE',  ( -7.825402957745081878, 7.899365992529268965, -23.57352014148015584 ) ) ;
#13061 = CARTESIAN_POINT ( 'NONE',  ( 6.400000000000000355, 4.618802153517001408, -8.000000000000000000 ) ) ;
#13062 = CARTESIAN_POINT ( 'NONE',  ( -59.56523643198714524, 15.93788386494078502, 16.96843438806351401 ) ) ;
#13063 = EDGE_LOOP ( 'NONE', ( #44716, #16709 ) ) ;
#13064 = DIRECTION ( 'NONE',  ( -1.000000000000000000, 0.000000000000000000, 0.000000000000000000 ) ) ;
#13065 = ORIENTED_EDGE ( 'NONE', *, *, #1437, .F. ) ;
#13066 = CARTESIAN_POINT ( 'NONE',  ( 106.0171289417044136, 26.97542621030654786, -64.06623974535388300 ) ) ;
#13067 = CARTESIAN_POINT ( 'NONE',  ( 44.34689728705970424, 10.12166135033765357, -10.61515644663351310 ) ) ;
#13068 = CARTESIAN_POINT ( 'NONE',  ( 44.34263167748003553, 9.103379693481581825, 58.59462232353900646 ) ) ;
#13069 = CARTESIAN_POINT ( 'NONE',  ( 0.000000000000000000, 0.000000000000000000, 170.0000000000000000 ) ) ;
#13070 = CARTESIAN_POINT ( 'NONE',  ( 30.83327723550665311, -12.90705755941334942, 6.893343212288926658 ) ) ;
#13071 = DIRECTION ( 'NONE',  ( 0.000000000000000000, 0.000000000000000000, 1.000000000000000000 ) ) ;
#13072 = CARTESIAN_POINT ( 'NONE',  ( -76.78936026062119424, 21.61552955137052834, 57.49749715836401975 ) ) ;
#13073 = CARTESIAN_POINT ( 'NONE',  ( -165.9122696334864884, 79.44688201528255433, 63.07591441595136672 ) ) ;
#13074 = ORIENTED_EDGE ( 'NONE', *, *, #36033, .T. ) ;
#13075 = ORIENTED_EDGE ( 'NONE', *, *, #29593, .F. ) ;
#13076 = DIRECTION ( 'NONE',  ( 0.000000000000000000, 1.000000000000000000, 0.000000000000000000 ) ) ;
#13077 = CARTESIAN_POINT ( 'NONE',  ( -11.01093400780253084, 22.58090174195383781, 3.061616997868437868E-16 ) ) ;
#13078 = DIRECTION ( 'NONE',  ( 0.9362348706397417564, -0.3513748240813305279, 0.000000000000000000 ) ) ;
#13079 = AXIS2_PLACEMENT_3D ( 'NONE', #32494, #58521, #49346 ) ;
#13080 = CARTESIAN_POINT ( 'NONE',  ( 110.2429982417149432, 29.99119854320844070, 71.45576479620103783 ) ) ;
#13081 = CARTESIAN_POINT ( 'NONE',  ( 445.3372781065086201, 217.8591479523844612, 78.55029585798806124 ) ) ;
#13082 = VECTOR ( 'NONE', #18171, 1000.000000000000000 ) ;
#13083 = CARTESIAN_POINT ( 'NONE',  ( 55.99998955208977236, 12.18058389017405219, -13.71295351543068541 ) ) ;
#13084 = ORIENTED_EDGE ( 'NONE', *, *, #53959, .T. ) ;
#13085 = CARTESIAN_POINT ( 'NONE',  ( -29.87147652227455907, 68.79592317125366208, 73.58025477438756923 ) ) ;
#13086 = AXIS2_PLACEMENT_3D ( 'NONE', #2118, #66492, #39740 ) ;
#13087 = CARTESIAN_POINT ( 'NONE',  ( 22.28700331106867338, 7.803633676228379557, -39.26703075270760479 ) ) ;
#13088 = CARTESIAN_POINT ( 'NONE',  ( -85.35127931077727226, 24.98147633333000073, -19.18063208637886774 ) ) ;
#13089 = DIRECTION ( 'NONE',  ( -0.000000000000000000, -0.000000000000000000, -1.000000000000000000 ) ) ;
#13090 = CARTESIAN_POINT ( 'NONE',  ( 212.1962110267000412, 117.2292732107321740, -17.35804251465089010 ) ) ;
#13091 = FACE_BOUND ( 'NONE', #30499, .T. ) ;
#13092 = EDGE_CURVE ( 'NONE', #2204, #16163, #67659, .T. ) ;
#13093 = CIRCLE ( 'NONE', #20960, 5.000000000000000888 ) ;
#13094 = VERTEX_POINT ( 'NONE', #23510 ) ;
#13095 = CARTESIAN_POINT ( 'NONE',  ( 442.3372781065083359, 370.0000000000043769, 108.5502958579838833 ) ) ;
#13096 = DIRECTION ( 'NONE',  ( 0.000000000000000000, 0.000000000000000000, 1.000000000000000000 ) ) ;
#13097 = CARTESIAN_POINT ( 'NONE',  ( 38.43102714813441878, 9.298961820315048143, -77.41741745035568556 ) ) ;
#13098 = CARTESIAN_POINT ( 'NONE',  ( -180.0094637318086370, 96.72611451757710199, 8.496329745107461306 ) ) ;
#13099 = CARTESIAN_POINT ( 'NONE',  ( 208.5936709733498162, 113.6229123546138169, 57.12947936804001614 ) ) ;
#13100 = CARTESIAN_POINT ( 'NONE',  ( 15.78827728214693416, -170.0000000000000000, 91.20380885363260859 ) ) ;
#13101 = EDGE_CURVE ( 'NONE', #6090, #32844, #48209, .T. ) ;
#13102 = ORIENTED_EDGE ( 'NONE', *, *, #35948, .T. ) ;
#13103 = CARTESIAN_POINT ( 'NONE',  ( 311.0133388548732114, 190.0000000000000000, -153.4166086460792826 ) ) ;
#13104 = CARTESIAN_POINT ( 'NONE',  ( 204.6977192012829505, 108.0580384837234931, -51.32593103262161094 ) ) ;
#13105 = ADVANCED_FACE ( 'NONE', ( #39677 ), #23857, .F. ) ;
#13106 = VERTEX_POINT ( 'NONE', #55502 ) ;
#13107 = LINE ( 'NONE', #13446, #296 ) ;
#13108 = ORIENTED_EDGE ( 'NONE', *, *, #14132, .F. ) ;
#13109 = CARTESIAN_POINT ( 'NONE',  ( -82.53770812813174018, 23.83403279300014788, -75.88817085053467792 ) ) ;
#13110 = CARTESIAN_POINT ( 'NONE',  ( -60.64199216239839529, 17.30050036439945416, -20.87887065183614865 ) ) ;
#13111 = EDGE_CURVE ( 'NONE', #2381, #50858, #35499, .T. ) ;
#13112 = CARTESIAN_POINT ( 'NONE',  ( 92.95016907945947082, 22.74936990452176033, -74.21060328399696004 ) ) ;
#13113 = EDGE_LOOP ( 'NONE', ( #25821, #26800, #42905, #29775 ) ) ;
#13114 = EDGE_CURVE ( 'NONE', #41523, #63790, #35444, .T. ) ;
#13115 = ORIENTED_EDGE ( 'NONE', *, *, #65510, .F. ) ;
#13116 = CARTESIAN_POINT ( 'NONE',  ( 45.76553115525425852, 10.34124506813255095, 60.28159494287191222 ) ) ;
#13117 = CARTESIAN_POINT ( 'NONE',  ( -105.1578917446807111, 35.40396694227245433, -89.27446617212257252 ) ) ;
#13118 = CARTESIAN_POINT ( 'NONE',  ( 107.9213359589209063, 28.92595015506872969, 17.41395595518270412 ) ) ;
#13119 = ORIENTED_EDGE ( 'NONE', *, *, #18421, .F. ) ;
#13120 = PRODUCT_DEFINITION_SHAPE ( 'NONE', 'NONE',  #69572 ) ;
#13121 = SURFACE_STYLE_FILL_AREA ( #50050 ) ;
#13122 = VECTOR ( 'NONE', #19804, 1000.000000000000000 ) ;
#13123 = CARTESIAN_POINT ( 'NONE',  ( -49.13048465129990205, 14.20828170588045403, 15.60104833568753335 ) ) ;
#13124 = CARTESIAN_POINT ( 'NONE',  ( -14.96769463968061231, 8.472501390435335011, -94.16364436271733496 ) ) ;
#13125 = EDGE_CURVE ( 'NONE', #28478, #3462, #24663, .T. ) ;
#13126 = CARTESIAN_POINT ( 'NONE',  ( 115.0692128464502417, 31.17922615202197889, -10.81633842045794935 ) ) ;
#13127 = CARTESIAN_POINT ( 'NONE',  ( 94.13651963513105159, 22.12061817498822691, 90.79928215880261178 ) ) ;
#13128 = CIRCLE ( 'NONE', #49036, 242.4895526022646379 ) ;
#13130 = EDGE_LOOP ( 'NONE', ( #65191, #46774, #39522, #32891 ) ) ;
#13129 = CARTESIAN_POINT ( 'NONE',  ( -67.03031041878467988, 33.66749151869449008, 43.58025477438756212 ) ) ;
#13131 = ORIENTED_EDGE ( 'NONE', *, *, #47776, .F. ) ;
#13132 = VECTOR ( 'NONE', #36358, 1000.000000000000000 ) ;
#13133 = ORIENTED_EDGE ( 'NONE', *, *, #46371, .T. ) ;
#13134 = CARTESIAN_POINT ( 'NONE',  ( 45.36109889487609337, 9.259412558041150376, 15.14959608583331807 ) ) ;
#13135 = CARTESIAN_POINT ( 'NONE',  ( -180.5668250991443813, 97.41296786328892665, 91.03718869750294118 ) ) ;
#13136 = CARTESIAN_POINT ( 'NONE',  ( -53.13004807512038496, 14.17398740785108657, -8.606103191301974320 ) ) ;
#13137 = CARTESIAN_POINT ( 'NONE',  ( 107.2672065034543039, 27.52931006625853882, -23.46636325839187265 ) ) ;
#13138 = FACE_OUTER_BOUND ( 'NONE', #28425, .T. ) ;
#13139 = CARTESIAN_POINT ( 'NONE',  ( 197.1974290009104891, 96.59277840252784131, 9.539146130048552052 ) ) ;
#13140 = CARTESIAN_POINT ( 'NONE',  ( 197.5344360088799363, 98.61758084709093453, 88.16435646324907793 ) ) ;
#13141 = CARTESIAN_POINT ( 'NONE',  ( 21.80334785612273762, 25.33568910032904142, 6.893343212288939093 ) ) ;
#13142 = DIRECTION ( 'NONE',  ( -0.000000000000000000, 1.000000000000000000, -0.000000000000000000 ) ) ;
#13143 = CARTESIAN_POINT ( 'NONE',  ( -9.763294602873864747, 7.024900256480051119, 44.86506734459265999 ) ) ;
#13144 = ORIENTED_EDGE ( 'NONE', *, *, #66345, .T. ) ;
#13145 = VECTOR ( 'NONE', #34094, 1000.000000000000000 ) ;
#13146 = CARTESIAN_POINT ( 'NONE',  ( 9.280894575734581764, 7.385644305345137717, -19.93533336458542848 ) ) ;
#13147 = ORIENTED_EDGE ( 'NONE', *, *, #67535, .F. ) ;
#13148 = ORIENTED_EDGE ( 'NONE', *, *, #60502, .F. ) ;
#13149 = CARTESIAN_POINT ( 'NONE',  ( -142.9756886485678251, 60.11539876121634052, 7.681077562724933472 ) ) ;
#13150 = CARTESIAN_POINT ( 'NONE',  ( 187.2296622856351576, 86.53808614709454616, -74.87664997496398200 ) ) ;
#13151 = CARTESIAN_POINT ( 'NONE',  ( -38.90277964098074648, 11.96165882689933824, 90.60046426814015774 ) ) ;
#13152 = CARTESIAN_POINT ( 'NONE',  ( -96.43148989374462587, 29.90755650959364331, -37.79297082079260406 ) ) ;
#13153 = CARTESIAN_POINT ( 'NONE',  ( -2.999999999999992450, 0.000000000000000000, 0.000000000000000000 ) ) ;
#13154 = CARTESIAN_POINT ( 'NONE',  ( 15.78827728214693416, 7.507518794609589818, -50.51894409868581448 ) ) ;
#13155 = CARTESIAN_POINT ( 'NONE',  ( 133.6288034103010318, 41.28708886999549321, -51.02331093239571658 ) ) ;
#13156 = EDGE_LOOP ( 'NONE', ( #33249, #52496, #29073, #69310 ) ) ;
#13157 = VERTEX_POINT ( 'NONE', #62870 ) ;
#13158 = CARTESIAN_POINT ( 'NONE',  ( 188.5556894309611948, 88.00527073660660449, 91.18024676934048500 ) ) ;
#13159 = CARTESIAN_POINT ( 'NONE',  ( -57.97933236950880342, -6.473286833963715736, 27.58472369368490718 ) ) ;
#13160 = CARTESIAN_POINT ( 'NONE',  ( -11.01093400780253084, 22.58090174195383781, 3.061616997868437868E-16 ) ) ;
#13161 = CARTESIAN_POINT ( 'NONE',  ( 58.09436971064710775, 11.58462396079456447, -10.69534298273807238 ) ) ;
#13162 = CARTESIAN_POINT ( 'NONE',  ( -442.6627218934916641, 394.9999999999954525, 103.5502958579924808 ) ) ;
#13163 = CARTESIAN_POINT ( 'NONE',  ( 197.5344433744249102, 98.61756151884679866, 65.79699254537881359 ) ) ;
#13164 = EDGE_LOOP ( 'NONE', ( #18745, #61449, #6149, #59596, #62272, #44730, #29807, #17178, #42079, #44013, #63020, #53045, #10738, #24707, #6989, #29935, #11774, #59400, #25229, #9741, #14498, #18149, #35459, #37646, #66195, #26062, #56713, #46817, #33279, #10346, #52068, #44312, #33070, #33354, #47903, #12053, #45951, #65887, #63337, #36333, #39274, #38954, #8962, #11036, #1948, #20229, #49549, #4210, #40522, #11097, #41888, #39240, #26750, #18370, #18420, #8706, #30476, #51438, #11155, #65072, #19943, #57431, #11050, #16553, #44426, #27531, #44587, #61892, #9334, #1388, #10358, #214, #23208, #26556, #34415, #16509, #57033, #50809, #27374, #37339, #24263, #36596, #24600, #37930, #739, #49014, #41492, #44815, #38491, #5551, #7886, #9639, #18806, #60079, #30187, #16284, #51629, #20653, #25220, #6346, #39116, #39403, #47861, #9054, #12575, #21589, #42091, #16232, #42742, #35876, #2424, #20471, #52672, #69095, #48680, #17439, #45096, #62458, #50354, #36635, #3214, #68832, #46667, #37590, #60635, #46008, #5441, #57288, #51205, #43896, #66602, #43166, #45457, #27427, #34065, #53865, #27740, #63793, #7632, #45728, #28127 ) ) ;
#13165 = CARTESIAN_POINT ( 'NONE',  ( 45.89268866913129585, 10.36133864615982780, -66.19858745361412389 ) ) ;
#13166 = CARTESIAN_POINT ( 'NONE',  ( -61.76386578474847511, 17.63453064612502175, -72.94559511649701733 ) ) ;
#13167 = CARTESIAN_POINT ( 'NONE',  ( 201.9721407532275066, 104.3507814346148166, -63.67126515581958301 ) ) ;
#13168 = EDGE_CURVE ( 'NONE', #34560, #66549, #57932, .T. ) ;
#13169 = VECTOR ( 'NONE', #10133, 1000.000000000000000 ) ;
#13170 = CARTESIAN_POINT ( 'NONE',  ( -180.6209440844957896, 95.88392769199009535, -41.89197730208912418 ) ) ;
#13171 = PLANE ( 'NONE',  #23970 ) ;
#13172 = CARTESIAN_POINT ( 'NONE',  ( -165.6212796729685124, 79.15047440262051737, 11.17022651014945289 ) ) ;
#13173 = CARTESIAN_POINT ( 'NONE',  ( -125.8938041572051389, -170.0000000000000000, -76.75825448869764500 ) ) ;
#13174 = FACE_BOUND ( 'NONE', #53592, .T. ) ;
#13175 = DIRECTION ( 'NONE',  ( -0.000000000000000000, -0.000000000000000000, -1.000000000000000000 ) ) ;
#13176 = CIRCLE ( 'NONE', #36765, 60.00000000000000000 ) ;
#13177 = CARTESIAN_POINT ( 'NONE',  ( -5.401648928593175469, 6.744888135494087500, 71.57446707354854709 ) ) ;
#13178 = VERTEX_POINT ( 'NONE', #62526 ) ;
#13179 = VECTOR ( 'NONE', #67585, 1000.000000000000000 ) ;
#13180 = CARTESIAN_POINT ( 'NONE',  ( 275.1691917892559331, 21.96211590856092144, 1.300061720562569301 ) ) ;
#13181 = LINE ( 'NONE', #39904, #30762 ) ;
#13182 = DIRECTION ( 'NONE',  ( -0.000000000000000000, 1.000000000000000000, -0.000000000000000000 ) ) ;
#13183 = DIRECTION ( 'NONE',  ( 0.000000000000000000, 0.000000000000000000, -1.000000000000000000 ) ) ;
#13184 = DIRECTION ( 'NONE',  ( -0.000000000000000000, -1.000000000000000000, -0.000000000000000000 ) ) ;
#13185 = CIRCLE ( 'NONE', #69343, 243.4957430088094839 ) ;
#13186 = CIRCLE ( 'NONE', #15380, 5.000000000000018652 ) ;
#13187 = ORIENTED_EDGE ( 'NONE', *, *, #42078, .T. ) ;
#13188 =( LENGTH_UNIT ( ) NAMED_UNIT ( * ) SI_UNIT ( .MILLI., .METRE. ) );
#13189 = CARTESIAN_POINT ( 'NONE',  ( -449.7337897053567417, 364.9999999999997726, 110.6213636698531673 ) ) ;
#13190 = EDGE_CURVE ( 'NONE', #4577, #23405, #57301, .T. ) ;
#13191 = ORIENTED_EDGE ( 'NONE', *, *, #47317, .F. ) ;
#13192 = ORIENTED_EDGE ( 'NONE', *, *, #41787, .F. ) ;
#13193 = LINE ( 'NONE', #45533, #52142 ) ;
#13194 = CARTESIAN_POINT ( 'NONE',  ( 154.6530827109543509, 56.75509330623211213, 43.86387257709986187 ) ) ;
#13195 = LINE ( 'NONE', #34659, #4378 ) ;
#13196 = ORIENTED_EDGE ( 'NONE', *, *, #60306, .F. ) ;
#13197 = CARTESIAN_POINT ( 'NONE',  ( -3.841371665203041630E-11, 0.000000000000000000, 10.00000000000000000 ) ) ;
#13198 = CARTESIAN_POINT ( 'NONE',  ( 29.99999999999999645, 26.99999999999999289, 15.00000000000000000 ) ) ;
#13199 = CARTESIAN_POINT ( 'NONE',  ( -1.083610669212424105, 6.545642299653493978, 14.09380834579263642 ) ) ;
#13200 = EDGE_CURVE ( 'NONE', #42554, #51645, #17871, .T. ) ;
#13201 = CARTESIAN_POINT ( 'NONE',  ( -81.23268307104839892, 24.39742801172156561, 30.86689043824910073 ) ) ;
#13202 = CARTESIAN_POINT ( 'NONE',  ( 15.78827728214693416, -170.0000000000000000, 37.51470767270523510 ) ) ;
#13203 = CARTESIAN_POINT ( 'NONE',  ( 136.1081004736419686, 42.80058051492063953, 3.007995494952832249 ) ) ;
#13204 = VERTEX_POINT ( 'NONE', #30173 ) ;
#13205 = CARTESIAN_POINT ( 'NONE',  ( -11.75099048680785785, -77.43714764088365143, 73.58025477438756923 ) ) ;
#13206 = CARTESIAN_POINT ( 'NONE',  ( -74.39861643904069410, 21.81123504700007487, 17.24566514567988662 ) ) ;
#13207 = ADVANCED_FACE ( 'NONE', ( #46681, #13987 ), #13638, .F. ) ;
#13208 = CARTESIAN_POINT ( 'NONE',  ( 46.65037935242577305, 9.463293687292225087, -41.17784024966125145 ) ) ;
#13209 = DIRECTION ( 'NONE',  ( 0.8805955318567391110, -0.4738686624729966379, 5.102127870520020458E-18 ) ) ;
#13211 = VERTEX_POINT ( 'NONE', #41067 ) ;
#13210 = CARTESIAN_POINT ( 'NONE',  ( -118.6806115626323930, 41.92435854543968077, 89.72766250507453378 ) ) ;
#13213 = CARTESIAN_POINT ( 'NONE',  ( -78.66644367742109978, 22.32174330031320508, -61.96000122218157458 ) ) ;
#13212 = B_SPLINE_CURVE_WITH_KNOTS ( 'NONE', 3,
 ( #18200, #39654, #1670, #12933, #34736, #45271, #56173, #24179, #11871, #54775, #38967, #65702, #6601, #1320, #60413, #17494, #33694, #23133, #44582, #68132, #8347, #46654, #14312, #3070, #47004, #35068, #67782, #18894, #63188, #30836, #46302, #57221, #61791, #51933, #19937, #29792, #19579, #9727, #24866, #35416, #9036, #41037, #30151, #45629 ),
 .UNSPECIFIED., .F., .F.,
 ( 4, 2, 2, 2, 2, 2, 2, 2, 2, 2, 2, 2, 1, 2, 2, 2, 2, 2, 2, 1, 2, 2, 4 ),
 ( 0.02381751147647563627, 0.02531129726520766482, 0.02605819015957367563, 0.02680508305393968990, 0.02829886884267171498, 0.02979265463140373660, 0.03053954752576975781, 0.03128644042013577209, 0.03278022620886781452, 0.03427401199759985695, 0.03576779778633189938, 0.03651469068069792406, 0.03726158357506394181, 0.03800847646942997343, 0.03875536936379599118, 0.04024915515252804055, 0.04174294094126008992, 0.04323672672999213928, 0.04398361962435816397, 0.04473051251872418865, 0.04547740541309021334, 0.04622429830745623802, 0.04771808409618830821 ),
 .UNSPECIFIED. ) ;
#13214 = EDGE_CURVE ( 'NONE', #16065, #15985, #21273, .T. ) ;
#13215 = ORIENTED_EDGE ( 'NONE', *, *, #61006, .F. ) ;
#13216 = CARTESIAN_POINT ( 'NONE',  ( -146.7345109736526467, 61.86270848728297267, 72.03746416512107942 ) ) ;
#13217 = AXIS2_PLACEMENT_3D ( 'NONE', #47083, #62586, #63271 ) ;
#13218 = DIRECTION ( 'NONE',  ( 0.000000000000000000, 0.000000000000000000, -1.000000000000000000 ) ) ;
#13219 = DIRECTION ( 'NONE',  ( 4.906538933386759377E-15, -0.7071067811865474617, 0.7071067811865474617 ) ) ;
#13220 = DIRECTION ( 'NONE',  ( 1.000000000000000000, 0.000000000000000000, 0.000000000000000000 ) ) ;
#13221 = CARTESIAN_POINT ( 'NONE',  ( 133.8566784816069628, 41.42467568809809819, -9.178760341931967659 ) ) ;
#13222 = VECTOR ( 'NONE', #28910, 1000.000000000000114 ) ;
#13223 = DIRECTION ( 'NONE',  ( 0.000000000000000000, 1.000000000000000000, -0.000000000000000000 ) ) ;
#13224 = CARTESIAN_POINT ( 'NONE',  ( -173.5372686962699902, 89.10569330281722955, -22.86740657428632417 ) ) ;
#13225 = CARTESIAN_POINT ( 'NONE',  ( -154.0775378574014383, 68.15437918458553668, -36.34688571082521236 ) ) ;
#13226 = VERTEX_POINT ( 'NONE', #41417 ) ;
#13227 = ORIENTED_EDGE ( 'NONE', *, *, #41695, .F. ) ;
#13228 = AXIS2_PLACEMENT_3D ( 'NONE', #59850, #23296, #28916 ) ;
#13229 = CARTESIAN_POINT ( 'NONE',  ( 102.8111940033034273, 25.59308899183601227, 64.99745727866086042 ) ) ;
#13230 = DIRECTION ( 'NONE',  ( 0.000000000000000000, 0.000000000000000000, 1.000000000000000000 ) ) ;
#13231 = DIRECTION ( 'NONE',  ( 0.000000000000000000, 0.000000000000000000, 1.000000000000000000 ) ) ;
#13232 = AXIS2_PLACEMENT_3D ( 'NONE', #22531, #21479, #16208 ) ;
#13233 = CARTESIAN_POINT ( 'NONE',  ( 0.000000000000000000, 0.000000000000000000, 41.38025477438755928 ) ) ;
#13234 = DIRECTION ( 'NONE',  ( 0.000000000000000000, 6.779273404243065824E-32, -1.000000000000000000 ) ) ;
#13235 = CARTESIAN_POINT ( 'NONE',  ( -107.0751323097254186, 35.28386110859231906, 59.07576044861188791 ) ) ;
#13236 = DIRECTION ( 'NONE',  ( 0.000000000000000000, 0.000000000000000000, 1.000000000000000000 ) ) ;
#13237 = CARTESIAN_POINT ( 'NONE',  ( 157.4703587214989113, 57.65129005721576760, -77.96873488960135035 ) ) ;
#13238 = ORIENTED_EDGE ( 'NONE', *, *, #53488, .T. ) ;
#13239 = ORIENTED_EDGE ( 'NONE', *, *, #538, .T. ) ;
#13240 = ORIENTED_EDGE ( 'NONE', *, *, #55330, .F. ) ;
#13242 = AXIS2_PLACEMENT_3D ( 'NONE', #32753, #27119, #21844 ) ;
#13241 = LINE ( 'NONE', #7955, #20650 ) ;
#13243 = CARTESIAN_POINT ( 'NONE',  ( -71.82968714595206450, 19.83409541362842887, 94.70823564810032735 ) ) ;
#13244 = LINE ( 'NONE', #28363, #49866 ) ;
#13245 = CARTESIAN_POINT ( 'NONE',  ( 46.68215785206009372, 0.000000000000000000, -77.29788463846088575 ) ) ;
#13246 = CARTESIAN_POINT ( 'NONE',  ( 63.01563776193091826, -170.0000000000000000, -77.56524142263344856 ) ) ;
#13247 = CARTESIAN_POINT ( 'NONE',  ( -58.32502757340553501, 16.62877055630753631, 31.05165587581745967 ) ) ;
#13248 = DIRECTION ( 'NONE',  ( 0.8660254037844379305, -0.5000000000000011102, 0.000000000000000000 ) ) ;
#13249 = CARTESIAN_POINT ( 'NONE',  ( 58.09877917144281412, 12.61383386832654452, 31.62849139763403983 ) ) ;
#13250 = CARTESIAN_POINT ( 'NONE',  ( 42.60443493776924839, 8.846984668533421470, 84.28900201317352980 ) ) ;
#13252 = ORIENTED_EDGE ( 'NONE', *, *, #49764, .T. ) ;
#13251 = EDGE_CURVE ( 'NONE', #19626, #47003, #68157, .T. ) ;
#13253 = CARTESIAN_POINT ( 'NONE',  ( 41.26323129469689377, -6.217756351907037349, 13.79046412291064172 ) ) ;
#13254 = FACE_OUTER_BOUND ( 'NONE', #69197, .T. ) ;
#13255 = CARTESIAN_POINT ( 'NONE',  ( -15.13464256769235838, 8.488509377255647692, 12.46951090161849862 ) ) ;
#13256 = CARTESIAN_POINT ( 'NONE',  ( -142.0685766576042113, 58.11789490499572253, 12.48546705073966123 ) ) ;
#13257 = CARTESIAN_POINT ( 'NONE',  ( 53.32245423372616244, -37.19594572654634845, 41.38025477438755928 ) ) ;
#13258 = CARTESIAN_POINT ( 'NONE',  ( -102.2801239173131052, 32.78103895658057354, -76.85912785543962400 ) ) ;
#13259 = CARTESIAN_POINT ( 'NONE',  ( 181.0840389613909736, 80.03940679743416808, -51.22505766587963905 ) ) ;
#13260 = EDGE_CURVE ( 'NONE', #46584, #50826, #36135, .T. ) ;
#13261 = ORIENTED_EDGE ( 'NONE', *, *, #54911, .T. ) ;
#13262 = CARTESIAN_POINT ( 'NONE',  ( 132.0563630623056781, 41.51825634609595284, -50.80769278490465979 ) ) ;
#13263 = CARTESIAN_POINT ( 'NONE',  ( -38.88884187334148379, 11.95889603743728280, -43.81403857136609048 ) ) ;
#13264 = DIRECTION ( 'NONE',  ( 1.110223024625158749E-14, 0.000000000000000000, 1.000000000000000000 ) ) ;
#13265 = ITEM_DEFINED_TRANSFORMATION ( 'NONE', 'NONE', #64738,  #66832 ) ;
#13266 = CARTESIAN_POINT ( 'NONE',  ( -178.0096424707516576, 92.73811996563144078, 86.29695439451984385 ) ) ;
#13267 = ORIENTED_EDGE ( 'NONE', *, *, #41674, .T. ) ;
#13268 = DIRECTION ( 'NONE',  ( -0.3930250316539147803, -0.9195277725514544587, 0.000000000000000000 ) ) ;
#13269 = AXIS2_PLACEMENT_3D ( 'NONE', #60677, #23411, #61371 ) ;
#13270 = EDGE_CURVE ( 'NONE', #30847, #66603, #26851, .T. ) ;
#13271 = CARTESIAN_POINT ( 'NONE',  ( 64.38365952013991489, 38.46744580544303460, 43.58025477438756212 ) ) ;
#13272 = CARTESIAN_POINT ( 'NONE',  ( 204.3129818922372749, 107.5244029525888436, 2.363170148305748341 ) ) ;
#13273 = EDGE_CURVE ( 'NONE', #2593, #1003, #15018, .T. ) ;
#13274 = VECTOR ( 'NONE', #40926, 999.9999999999998863 ) ;
#13275 = CARTESIAN_POINT ( 'NONE',  ( 162.8241818775801164, 63.24198268785130495, 85.33621435715247117 ) ) ;
#13276 = EDGE_CURVE ( 'NONE', #48827, #33721, #37978, .T. ) ;
#13277 = ORIENTED_EDGE ( 'NONE', *, *, #25240, .F. ) ;
#13278 = CARTESIAN_POINT ( 'NONE',  ( 163.1402336665937582, 63.50458794835979148, -92.38649040534465939 ) ) ;
#13279 = PLANE ( 'NONE',  #57569 ) ;
#13280 = AXIS2_PLACEMENT_3D ( 'NONE', #24520, #61100, #3395 ) ;
#13281 = CARTESIAN_POINT ( 'NONE',  ( -154.8006992380338431, 70.15733562427986669, 43.55549133835197750 ) ) ;
#13282 = ADVANCED_FACE ( 'NONE', ( #38198 ), #43465, .F. ) ;
#13283 = CARTESIAN_POINT ( 'NONE',  ( 23.24028701062093916, 6.853614888934261629, -42.04100009002929994 ) ) ;
#13284 = MECHANICAL_DESIGN_GEOMETRIC_PRESENTATION_REPRESENTATION (  '', ( #63832 ), #66066 ) ;
#13285 = CARTESIAN_POINT ( 'NONE',  ( -2.999999999999994227, 2.486033002269127373E-15, 20.30000000000000071 ) ) ;
#13287 = ORIENTED_EDGE ( 'NONE', *, *, #57997, .T. ) ;
#13286 = CARTESIAN_POINT ( 'NONE',  ( 230.9999999999999432, -57.00000000000007816, -2.000000000000000000 ) ) ;
#13288 = CARTESIAN_POINT ( 'NONE',  ( -1.675000714904271826, 7.575396497802214135, -92.29381673850149070 ) ) ;
#13289 = ORIENTED_EDGE ( 'NONE', *, *, #52180, .F. ) ;
#13290 = ORIENTED_EDGE ( 'NONE', *, *, #57502, .T. ) ;
#13291 = CARTESIAN_POINT ( 'NONE',  ( 176.6156959113759513, 75.60152827082541194, 42.85099558256738561 ) ) ;
#13292 = EDGE_CURVE ( 'NONE', #34263, #37573, #31544, .T. ) ;
#13293 = DIRECTION ( 'NONE',  ( -0.000000000000000000, 1.000000000000000000, -0.000000000000000000 ) ) ;
#13295 = ORIENTED_EDGE ( 'NONE', *, *, #45343, .T. ) ;
#13294 = CARTESIAN_POINT ( 'NONE',  ( -11.79249160485392878, 8.191429102467035150, -63.39294633506229104 ) ) ;
#13296 = DIRECTION ( 'NONE',  ( 0.000000000000000000, 1.000000000000000000, 0.000000000000000000 ) ) ;
#13297 = CARTESIAN_POINT ( 'NONE',  ( -24.32776401346968953, 9.546905915310563984, 40.14952946743263595 ) ) ;
#13298 = EDGE_CURVE ( 'NONE', #33778, #7569, #11116, .T. ) ;
#13299 = ADVANCED_FACE ( 'NONE', ( #32241 ), #37502, .F. ) ;
#13300 = CARTESIAN_POINT ( 'NONE',  ( -75.65611349188964141, 22.26947559308018398, -49.48898812600347696 ) ) ;
#13301 = ADVANCED_FACE ( 'NONE', ( #58606, #58956, #5497, #54005, #27291 ), #10422, .F. ) ;
#13302 = ORIENTED_EDGE ( 'NONE', *, *, #20071, .T. ) ;
#13303 = CARTESIAN_POINT ( 'NONE',  ( 211.1046732743772907, 117.3965485104337461, -66.76179994842109977 ) ) ;
#13304 = CARTESIAN_POINT ( 'NONE',  ( 140.5958192060901695, 46.84598876498520781, 33.70861045256287269 ) ) ;
#13305 = CARTESIAN_POINT ( 'NONE',  ( 117.3246714514015849, 33.42485879931865611, 34.58965814092242397 ) ) ;
#13306 = CARTESIAN_POINT ( 'NONE',  ( -132.2161740628506266, 52.03204870034954155, 7.232691840498619129 ) ) ;
#13307 = CARTESIAN_POINT ( 'NONE',  ( 24.36509522348982060, 70.94296747916789059, 73.58025477438755502 ) ) ;
#13308 = VERTEX_POINT ( 'NONE', #43811 ) ;
#13309 = ORIENTED_EDGE ( 'NONE', *, *, #31825, .F. ) ;
#13310 = ORIENTED_EDGE ( 'NONE', *, *, #30054, .T. ) ;
#13311 = CARTESIAN_POINT ( 'NONE',  ( 211.3773738276420886, 115.9764855123643912, -94.07397666197054775 ) ) ;
#13312 = CYLINDRICAL_SURFACE ( 'NONE', #57160, 7.500000000000013323 ) ;
#13313 = DIRECTION ( 'NONE',  ( 0.000000000000000000, -1.000000000000000000, 0.000000000000000000 ) ) ;
#13314 = CARTESIAN_POINT ( 'NONE',  ( 427.4999999999999432, 207.5000000000000284, -2.000000000000000000 ) ) ;
#13315 = DIRECTION ( 'NONE',  ( -0.000000000000000000, -0.000000000000000000, -1.000000000000000000 ) ) ;
#13316 = CARTESIAN_POINT ( 'NONE',  ( -133.0808647576833437, 51.41195281028754493, 67.12459488774240413 ) ) ;
#13317 = CARTESIAN_POINT ( 'NONE',  ( -73.63128929564827274, 21.53548093502884697, -10.20693752301225921 ) ) ;
#13318 = ORIENTED_EDGE ( 'NONE', *, *, #41240, .F. ) ;
#13319 = CARTESIAN_POINT ( 'NONE',  ( 204.6977192012829789, -170.0000000000000000, -70.67048162308527992 ) ) ;
#13320 = VERTEX_POINT ( 'NONE', #14166 ) ;
#13321 = AXIS2_PLACEMENT_3D ( 'NONE', #51249, #10293, #37041 ) ;
#13322 = DIRECTION ( 'NONE',  ( -6.651034621319910312E-17, 2.409948271074229917E-16, 1.000000000000000000 ) ) ;
#13323 =( NAMED_UNIT ( * ) SI_UNIT ( $, .STERADIAN. ) SOLID_ANGLE_UNIT ( ) );
#13324 = ORIENTED_EDGE ( 'NONE', *, *, #56385, .F. ) ;
#13325 = CARTESIAN_POINT ( 'NONE',  ( 185.5572090022886300, 83.24697331286184010, 42.84673731889779447 ) ) ;
#13326 = LINE ( 'NONE', #56930, #16373 ) ;
#13327 = CIRCLE ( 'NONE', #21149, 24.17157287525367693 ) ;
#13328 = CARTESIAN_POINT ( 'NONE',  ( -119.9771613955297340, 43.90337778233484300, 60.34853762580112146 ) ) ;
#13329 = CARTESIAN_POINT ( 'NONE',  ( -47.68742944762957592, 12.82957801017946764, 12.45128233048862576 ) ) ;
#13330 = CARTESIAN_POINT ( 'NONE',  ( -59.42430146430427129, 27.22983999535711064, 41.38025477438755928 ) ) ;
#13331 = CIRCLE ( 'NONE', #69488, 65.36598343705435354 ) ;
#13332 = EDGE_LOOP ( 'NONE', ( #25977, #62672, #12040, #27905 ) ) ;
#13333 = CARTESIAN_POINT ( 'NONE',  ( -108.4971425592086973, 36.05284916722902722, -92.00252201140912689 ) ) ;
#13334 = CARTESIAN_POINT ( 'NONE',  ( -156.9910258076866398, 70.79617246506501260, -16.04192918424444514 ) ) ;
#13335 = VERTEX_POINT ( 'NONE', #29648 ) ;
#13336 = PLANE ( 'NONE',  #42927 ) ;
#13337 = CARTESIAN_POINT ( 'NONE',  ( -62.14837099232448026, 17.75045801599141626, 67.10412718371505036 ) ) ;
#13338 = CARTESIAN_POINT ( 'NONE',  ( 409.0783954480986608, -1.426547569622074412E-15, 174.7010307253933377 ) ) ;
#13339 = ORIENTED_EDGE ( 'NONE', *, *, #18344, .T. ) ;
#13340 = CARTESIAN_POINT ( 'NONE',  ( 563.4809901518626702, 190.0000000000000000, 57.79371821540657095 ) ) ;
#13341 = CARTESIAN_POINT ( 'NONE',  ( 157.4703587214989113, 58.92748579479259519, -62.96873488960130771 ) ) ;
#13342 = CARTESIAN_POINT ( 'NONE',  ( -100.4466073551323007, 31.85873123265078988, -22.95728695924190887 ) ) ;
#13343 = CARTESIAN_POINT ( 'NONE',  ( 141.2470358420065679, 46.06959063280893218, -42.21817649076449186 ) ) ;
#13344 = ADVANCED_FACE ( 'NONE', ( #35628 ), #35275, .F. ) ;
#13345 = ORIENTED_EDGE ( 'NONE', *, *, #48539, .T. ) ;
#13346 = SHAPE_REPRESENTATION_RELATIONSHIP ( 'NONE' , 'NONE' ,  #35767, #25672 ) ;
#13347 = LINE ( 'NONE', #26823, #13836 ) ;
#13348 = CARTESIAN_POINT ( 'NONE',  ( 0.000000000000000000, 0.000000000000000000, 0.000000000000000000 ) ) ;
#13349 = ORIENTED_EDGE ( 'NONE', *, *, #67439, .T. ) ;
#13350 = CARTESIAN_POINT ( 'NONE',  ( 31.90170717962883273, 8.563261373066630711, -16.03511419624575751 ) ) ;
#13351 = CARTESIAN_POINT ( 'NONE',  ( 183.9986899696430385, 81.60141257362811018, 3.040213554178509803 ) ) ;
#13352 = CARTESIAN_POINT ( 'NONE',  ( 91.49345572560145001, 21.13836538408680710, 58.34269035543120907 ) ) ;
#13353 = EDGE_CURVE ( 'NONE', #8863, #25048, #62814, .T. ) ;
#13355 = EDGE_CURVE ( 'NONE', #8019, #34646, #44528, .T. ) ;
#13354 = DIRECTION ( 'NONE',  ( -0.9362348706397417564, 0.3513748240813305279, 0.000000000000000000 ) ) ;
#13356 = DIRECTION ( 'NONE',  ( 3.557538378468060822E-20, 5.551115123125781470E-17, -1.000000000000000000 ) ) ;
#13357 = CARTESIAN_POINT ( 'NONE',  ( 3.678442866637813759E-12, -65.13282190615278466, -9.999999999999998224 ) ) ;
#13358 = EDGE_CURVE ( 'NONE', #39568, #32990, #26140, .T. ) ;
#13359 = ORIENTED_EDGE ( 'NONE', *, *, #5924, .F. ) ;
#13360 = CARTESIAN_POINT ( 'NONE',  ( -836.0476379851791080, -568.5227338237882577, 0.000000000000000000 ) ) ;
#13361 = CARTESIAN_POINT ( 'NONE',  ( 0.000000000000000000, 0.000000000000000000, 0.000000000000000000 ) ) ;
#13362 = CARTESIAN_POINT ( 'NONE',  ( 66.08620257826612487, 13.40585338179128527, 71.00441744036213265 ) ) ;
#13363 = CARTESIAN_POINT ( 'NONE',  ( 135.6793972494602372, 43.71805072851428520, 2.876098451181287263 ) ) ;
#13364 = PLANE ( 'NONE',  #9474 ) ;
#13365 = ORIENTED_EDGE ( 'NONE', *, *, #3014, .T. ) ;
#13366 = CARTESIAN_POINT ( 'NONE',  ( 68.07999999999999829, -36.09918303830819752, 30.00000000000000000 ) ) ;
#13367 = CARTESIAN_POINT ( 'NONE',  ( 9.416656162223551618, 6.380306691996769253, 41.47870453118932943 ) ) ;
#13368 = ORIENTED_EDGE ( 'NONE', *, *, #150, .T. ) ;
#13369 = CARTESIAN_POINT ( 'NONE',  ( 70.11969827741708627, 15.47408882293424170, 66.61225004732548882 ) ) ;
#13370 = DIRECTION ( 'NONE',  ( -0.000000000000000000, 1.000000000000000000, -0.000000000000000000 ) ) ;
#13371 = VECTOR ( 'NONE', #34034, 1000.000000000000000 ) ;
#13372 = VERTEX_POINT ( 'NONE', #30345 ) ;
#13373 = CARTESIAN_POINT ( 'NONE',  ( 164.0073343966821824, 64.23003864582457823, -39.93842790887263305 ) ) ;
#13374 = CARTESIAN_POINT ( 'NONE',  ( -89.99999999999998579, 1.102182119232617596E-14, 7.000000000000000000 ) ) ;
#13375 = FACE_BOUND ( 'NONE', #53664, .T. ) ;
#13376 = EDGE_CURVE ( 'NONE', #66758, #44768, #16748, .T. ) ;
#13377 = DIRECTION ( 'NONE',  ( 1.000000000000000000, 0.000000000000000000, 0.000000000000000000 ) ) ;
#13378 = ORIENTED_EDGE ( 'NONE', *, *, #37390, .T. ) ;
#13379 = EDGE_CURVE ( 'NONE', #28345, #64668, #29171, .T. ) ;
#13380 = CARTESIAN_POINT ( 'NONE',  ( -101.3502439362134453, 33.43728945125134544, 3.717829675835958803 ) ) ;
#13381 = CARTESIAN_POINT ( 'NONE',  ( 60.45161273195552809, 13.12223384504257062, 83.92330211886128666 ) ) ;
#13382 = CARTESIAN_POINT ( 'NONE',  ( 154.6260751278567227, 56.73429849676967507, -90.36338124960292362 ) ) ;
#13383 = CARTESIAN_POINT ( 'NONE',  ( 83.37782009939536465, 19.39546426214656805, -9.714140923952603757 ) ) ;
#13384 = CARTESIAN_POINT ( 'NONE',  ( -165.6212796729685692, 79.15047440262054579, 38.01477710061311654 ) ) ;
#13385 = CARTESIAN_POINT ( 'NONE',  ( 38.98629290190360308, 9.369974505438298351, -89.30891864635512434 ) ) ;
#13386 = CARTESIAN_POINT ( 'NONE',  ( 126.4324872316702795, 37.11876756822024248, -69.27188833358552245 ) ) ;
#13387 = VERTEX_POINT ( 'NONE', #2921 ) ;
#13388 = CARTESIAN_POINT ( 'NONE',  ( -95.86163447241557378, 30.75089131639700213, 60.95167474732399882 ) ) ;
#13389 = CYLINDRICAL_SURFACE ( 'NONE', #52346, 7.500000000000013323 ) ;
#13390 = ORIENTED_EDGE ( 'NONE', *, *, #31613, .T. ) ;
#13391 = CARTESIAN_POINT ( 'NONE',  ( -156.3734885497381413, 71.59531449004286685, -45.34277193519254467 ) ) ;
#13392 = CARTESIAN_POINT ( 'NONE',  ( 211.3757499519976761, 117.8130818709823444, -13.55636099387667315 ) ) ;
#13393 = CARTESIAN_POINT ( 'NONE',  ( -5.767955557622883589E-14, -31.11269837220806878, 0.000000000000000000 ) ) ;
#13394 = CARTESIAN_POINT ( 'NONE',  ( -196.7348448768811409, -170.0000000000000000, 38.42256797338300345 ) ) ;
#13395 = LINE ( 'NONE', #65470, #11197 ) ;
#13396 = FACE_OUTER_BOUND ( 'NONE', #32596, .T. ) ;
#13397 = CARTESIAN_POINT ( 'NONE',  ( -5.183193881612056408, 7.740932022135017299, -9.050052149217117758 ) ) ;
#13398 = CARTESIAN_POINT ( 'NONE',  ( 174.9042454172879673, 72.57746269938724026, 14.24426339932219321 ) ) ;
#13399 = CARTESIAN_POINT ( 'NONE',  ( -61.51762070241280611, 16.51067482779404116, 14.78299046999394228 ) ) ;
#13400 = ORIENTED_EDGE ( 'NONE', *, *, #41535, .T. ) ;
#13401 = CARTESIAN_POINT ( 'NONE',  ( 29.69502258243432635, -57.82046033912835270, 40.00000000000003553 ) ) ;
#13402 = VERTEX_POINT ( 'NONE', #6887 ) ;
#13403 = CARTESIAN_POINT ( 'NONE',  ( 102.8066580714140628, 25.59117171227001108, -71.27532258126962006 ) ) ;
#13404 = CARTESIAN_POINT ( 'NONE',  ( 40.38132770291768026, 9.553709436640062336, -8.823569451234918759 ) ) ;
#13405 = CARTESIAN_POINT ( 'NONE',  ( 41.35041461497707616, 8.670465437677201237, 71.51759960298838337 ) ) ;
#13406 = CARTESIAN_POINT ( 'NONE',  ( 0.000000000000000000, 0.000000000000000000, 43.58025477438756212 ) ) ;
#13407 = DIRECTION ( 'NONE',  ( 0.7071067811865474617, -0.000000000000000000, -0.7071067811865474617 ) ) ;
#13408 = PRODUCT_RELATED_PRODUCT_CATEGORY ( 'part', '', ( #67620 ) ) ;
#13409 = DIRECTION ( 'NONE',  ( -1.000000000000000000, -0.000000000000000000, -0.000000000000000000 ) ) ;
#13410 = CARTESIAN_POINT ( 'NONE',  ( 55.76286625948333864, 12.13284185313540142, -95.00000000000133582 ) ) ;
#13411 = CARTESIAN_POINT ( 'NONE',  ( -24.39249304643438521, 60.24953346690454481, 73.58025477438756923 ) ) ;
#13412 = VERTEX_POINT ( 'NONE', #66956 ) ;
#13413 = ORIENTED_EDGE ( 'NONE', *, *, #47530, .T. ) ;
#13414 = EDGE_CURVE ( 'NONE', #51882, #3940, #34805, .T. ) ;
#13415 = DIRECTION ( 'NONE',  ( 0.000000000000000000, 1.000000000000000000, 2.184185950696548891E-33 ) ) ;
#13416 = CARTESIAN_POINT ( 'NONE',  ( 26.12852347772543737, 70.00000000000000000, 77.58025477438755502 ) ) ;
#13417 = CARTESIAN_POINT ( 'NONE',  ( -63.73419499958981049, -12.83646726144931449, 41.38025477438755928 ) ) ;
#13418 = CARTESIAN_POINT ( 'NONE',  ( -168.1811549361197251, 83.25427431521133315, 59.51798107920270553 ) ) ;
#13419 = EDGE_CURVE ( 'NONE', #32766, #41495, #62864, .T. ) ;
#13420 = DIRECTION ( 'NONE',  ( 0.000000000000000000, 0.000000000000000000, -1.000000000000000000 ) ) ;
#13421 = CIRCLE ( 'NONE', #2178, 242.4895526022646379 ) ;
#13422 = CARTESIAN_POINT ( 'NONE',  ( 62.04382205963243280, 13.48099884269679904, -8.923339836102410771 ) ) ;
#13423 = ORIENTED_EDGE ( 'NONE', *, *, #47234, .F. ) ;
#13424 = AXIS2_PLACEMENT_3D ( 'NONE', #38160, #34296, #23402 ) ;
#13425 = CARTESIAN_POINT ( 'NONE',  ( -18.89790202299209199, 62.20684691518605547, 41.38025477438755928 ) ) ;
#13426 = CARTESIAN_POINT ( 'NONE',  ( 18.43272992546528144, 7.606837839440253823, -35.99631868335740847 ) ) ;
#13427 = LINE ( 'NONE', #39127, #66473 ) ;
#13428 = LINE ( 'NONE', #6753, #66714 ) ;
#13429 = LINE ( 'NONE', #21129, #25103 ) ;
#13430 = EDGE_CURVE ( 'NONE', #18218, #50410, #17079, .T. ) ;
#13431 = EDGE_CURVE ( 'NONE', #52438, #20401, #37841, .T. ) ;
#13432 = ORIENTED_EDGE ( 'NONE', *, *, #5545, .T. ) ;
#13433 = EDGE_CURVE ( 'NONE', #59702, #59334, #50442, .T. ) ;
#13434 = VERTEX_POINT ( 'NONE', #10597 ) ;
#13435 = DIRECTION ( 'NONE',  ( 0.000000000000000000, 0.000000000000000000, -1.000000000000000000 ) ) ;
#13436 = LINE ( 'NONE', #2879, #61970 ) ;
#13437 = CARTESIAN_POINT ( 'NONE',  ( 45.82394788922798767, 46.11928342727497210, 170.0000000000000000 ) ) ;
#13438 = CARTESIAN_POINT ( 'NONE',  ( -175.1895962157336726, 90.99110972060685754, 4.255677171492019184 ) ) ;
#13439 = LINE ( 'NONE', #24692, #66682 ) ;
#13440 = AXIS2_PLACEMENT_3D ( 'NONE', #61485, #29467, #2743 ) ;
#13441 = CARTESIAN_POINT ( 'NONE',  ( 188.1848725084043110, -170.0000000000000000, -95.00000000000133582 ) ) ;
#13442 = EDGE_LOOP ( 'NONE', ( #2747, #2366 ) ) ;
#13443 = CARTESIAN_POINT ( 'NONE',  ( 0.000000000000000000, 0.000000000000000000, 0.000000000000000000 ) ) ;
#13444 = CARTESIAN_POINT ( 'NONE',  ( 197.2199163281727579, 98.22431253015348318, -44.48933272678075213 ) ) ;
#13445 = ORIENTED_EDGE ( 'NONE', *, *, #8300, .F. ) ;
#13446 = CARTESIAN_POINT ( 'NONE',  ( 31.11269837220800127, -31.11269837220812562, 2.000000000000001776 ) ) ;
#13447 = VERTEX_POINT ( 'NONE', #37330 ) ;
#13448 = B_SPLINE_CURVE_WITH_KNOTS ( 'NONE', 3,
 ( #9084, #68510, #19630, #67831, #46705, #25617, #19987, #68182, #52666, #36851, #14695, #15048, #36158, #4154, #52330, #47051, #10110, #31567, #53698, #42797, #49105, #32266, #37883, #22394, #22045, #236, #5518, #54743, #60384, #26973, #60018, #43144, #64264, #44181, #944, #26640, #11838, #1292, #6568, #11477, #59326, #48757, #69530, #65670, #17458 ),
 .UNSPECIFIED., .F., .F.,
 ( 4, 2, 2, 2, 2, 2, 2, 2, 2, 2, 2, 2, 2, 1, 2, 2, 2, 2, 2, 2, 2, 2, 4 ),
 ( 0.02356759485890611364, 0.02503765354686411301, 0.02577268289084312311, 0.02650771223482213321, 0.02797777092278017075, 0.02944782961073821176, 0.03018285895471723573, 0.03091788829869626318, 0.03238794698665432847, 0.03312297633063336633, 0.03385800567461239724, 0.03532806436257047294, 0.03606309370654951080, 0.03679812305052855559, 0.03753315239450759344, 0.03826818173848663129, 0.03973824042644470700, 0.04120829911440278270, 0.04267835780236085841, 0.04341338714633990320, 0.04414841649031894799, 0.04561847517827702370, 0.04708853386623510634 ),
 .UNSPECIFIED. ) ;
#13449 = CARTESIAN_POINT ( 'NONE',  ( -84.96580414052107244, 24.82184094495577398, -65.38213935470189142 ) ) ;
#13450 = PLANE ( 'NONE',  #28793 ) ;
#13451 = LINE ( 'NONE', #50727, #11140 ) ;
#13452 = ORIENTED_EDGE ( 'NONE', *, *, #59581, .F. ) ;
#13453 = VERTEX_POINT ( 'NONE', #57768 ) ;
#13454 = DIRECTION ( 'NONE',  ( 0.000000000000000000, 0.000000000000000000, -1.000000000000000000 ) ) ;
#13455 = VECTOR ( 'NONE', #40209, 1000.000000000000000 ) ;
#13456 = CARTESIAN_POINT ( 'NONE',  ( -104.9609170480078717, 35.30014942885841833, -89.19597386970725950 ) ) ;
#13457 = CARTESIAN_POINT ( 'NONE',  ( 23.03864809957654103, 6.841061756139154681, 12.60473612569555257 ) ) ;
#13458 = ORIENTED_EDGE ( 'NONE', *, *, #22384, .F. ) ;
#13459 = EDGE_CURVE ( 'NONE', #2018, #65364, #46864, .T. ) ;
#13460 = LINE ( 'NONE', #3255, #8773 ) ;
#13461 = CARTESIAN_POINT ( 'NONE',  ( -55.05276343752909440, 15.72344139423348430, 3.472777182467473800 ) ) ;
#13462 = CARTESIAN_POINT ( 'NONE',  ( -128.1282195935087316, 49.19720162550164844, -22.73222316029650614 ) ) ;
#13463 = DIRECTION ( 'NONE',  ( 0.000000000000000000, -1.000000000000000000, 0.000000000000000000 ) ) ;
#13464 = VECTOR ( 'NONE', #31449, 1000.000000000000000 ) ;
#13465 = CARTESIAN_POINT ( 'NONE',  ( 79.14113188808478583, 18.05280674635440974, -42.83065476743007594 ) ) ;
#13467 = VERTEX_POINT ( 'NONE', #58438 ) ;
#13466 = CARTESIAN_POINT ( 'NONE',  ( 141.9165763529819344, 242.0000000000000000, 129.0000000000000000 ) ) ;
#13468 = ORIENTED_EDGE ( 'NONE', *, *, #51660, .T. ) ;
#13469 = AXIS2_PLACEMENT_3D ( 'NONE', #16621, #22598, #33521 ) ;
#13470 = ORIENTED_EDGE ( 'NONE', *, *, #9830, .F. ) ;
#13471 = CARTESIAN_POINT ( 'NONE',  ( 41.33692564073607656, 8.668977654195478166, 3.319058603837437005 ) ) ;
#13472 = CARTESIAN_POINT ( 'NONE',  ( -180.6114021174235802, 97.46813718571149820, 92.54769712921735447 ) ) ;
#13473 = CARTESIAN_POINT ( 'NONE',  ( 53.32245423372616244, -37.19594572654634845, 170.0000000000000000 ) ) ;
#13474 = CARTESIAN_POINT ( 'NONE',  ( 107.9362503323352627, 27.82881837607800435, -9.425457200440790828 ) ) ;
#13475 = CARTESIAN_POINT ( 'NONE',  ( 203.1420903260745945, 104.2307086582027154, 17.24464569073724718 ) ) ;
#13476 = DIRECTION ( 'NONE',  ( -0.000000000000000000, 0.000000000000000000, 1.000000000000000000 ) ) ;
#13477 = CARTESIAN_POINT ( 'NONE',  ( 211.1620569867183690, 117.4844252930219142, 86.57602862735129179 ) ) ;
#13478 = CARTESIAN_POINT ( 'NONE',  ( 24.36509522348982060, 70.94296747916789059, 170.0000000000000000 ) ) ;
#13479 = CARTESIAN_POINT ( 'NONE',  ( -72.76696720809545127, 20.16136115364207626, -64.80250377197498324 ) ) ;
#13480 = FACE_OUTER_BOUND ( 'NONE', #58726, .T. ) ;
#13481 = VERTEX_POINT ( 'NONE', #67987 ) ;
#13482 = CARTESIAN_POINT ( 'NONE',  ( 11.82929895397813702, 7.412564870773604930, -22.54914669578485942 ) ) ;
#13483 = VERTEX_POINT ( 'NONE', #9926 ) ;
#13484 = ORIENTED_EDGE ( 'NONE', *, *, #14702, .T. ) ;
#13485 = CARTESIAN_POINT ( 'NONE',  ( 110.2429982417149574, -170.0000000000000000, 56.45576479620100940 ) ) ;
#13486 = CARTESIAN_POINT ( 'NONE',  ( 188.5653887627528036, 88.01608521313130495, -71.17894925488377567 ) ) ;
#13487 = CARTESIAN_POINT ( 'NONE',  ( -36.68762645608095596, 11.53530882149086345, 86.01941686338382453 ) ) ;
#13488 = AXIS2_PLACEMENT_3D ( 'NONE', #22899, #7773, #17980 ) ;
#13489 = CARTESIAN_POINT ( 'NONE',  ( -97.85576954355158819, 30.58918648956190367, -36.43939751378721326 ) ) ;
#13490 = EDGE_CURVE ( 'NONE', #19842, #27330, #44579, .T. ) ;
#13491 = DIRECTION ( 'NONE',  ( 1.000000000000000000, 0.000000000000000000, 0.000000000000000000 ) ) ;
#13492 = DIRECTION ( 'NONE',  ( 0.000000000000000000, -0.000000000000000000, -1.000000000000000000 ) ) ;
#13493 = FACE_OUTER_BOUND ( 'NONE', #31970, .T. ) ;
#13494 = CARTESIAN_POINT ( 'NONE',  ( 126.8947007444828614, 37.37669340849691935, -46.32467590398648127 ) ) ;
#13495 = ORIENTED_EDGE ( 'NONE', *, *, #58076, .T. ) ;
#13496 = ORIENTED_EDGE ( 'NONE', *, *, #1490, .T. ) ;
#13497 = EDGE_CURVE ( 'NONE', #39680, #59960, #48556, .T. ) ;
#13498 = B_SPLINE_CURVE_WITH_KNOTS ( 'NONE', 3,
 ( #31050, #16831, #20473, #41935, #41590, #63048, #30697, #6284, #36319, #52492, #43561, #33022, #9588, #27736, #59733, #1015, #10263, #53158, #36667, #22465, #48822, #31387, #58119, #667, #20825, #20136, #9933, #52821, #4644, #65033, #63747, #14853, #46872, #38293, #11544, #47204, #52148, #65388, #26107, #69000, #25775, #49174, #15556, #68336, #57775, #43906, #57428, #37006, #9241, #3965, #25433, #4313, #18582, #2412, #22817, #54813, #34076 ),
 .UNSPECIFIED., .F., .F.,
 ( 4, 2, 2, 2, 2, 2, 2, 2, 2, 2, 2, 2, 2, 2, 2, 2, 2, 2, 2, 1, 2, 2, 2, 2, 2, 2, 2, 2, 4 ),
 ( 0.000000000000000000, 0.001945600724231584880, 0.002918401086347380356, 0.003891201448463174964, 0.004864001810578970006, 0.005836802172694765915, 0.006809602534810560090, 0.007782402896926355132, 0.009728003621157898378, 0.01070080398327367087, 0.01167360434538944162, 0.01264640470750521412, 0.01361920506962098487, 0.01459200543173675736, 0.01556480579385252812, 0.01751040651808407483, 0.01848320688019983171, 0.01945600724231559206, 0.02042880760443134547, 0.02140160796654710582, 0.02237440832866286616, 0.02334720869077861957, 0.02529280941501012639, 0.02626560977712589715, 0.02723841013924166443, 0.02821121050135743172, 0.02918401086347320247, 0.03015681122558896282, 0.03112961158770473011 ),
 .UNSPECIFIED. ) ;
#13499 = CARTESIAN_POINT ( 'NONE',  ( 187.7395187440304483, 87.09941059914879702, 93.95990058528536792 ) ) ;
#13500 = CARTESIAN_POINT ( 'NONE',  ( -41.43037476669420016, -4.983853691429483312, 13.79046412286062306 ) ) ;
#13501 = CARTESIAN_POINT ( 'NONE',  ( 144.4165763529819344, 225.8585178651493663, 138.9999999999999716 ) ) ;
#13502 = EDGE_CURVE ( 'NONE', #63560, #2120, #43992, .T. ) ;
#13503 = CARTESIAN_POINT ( 'NONE',  ( -30.47069031368414826, 9.433993659086572947, -77.11504745095709268 ) ) ;
#13505 = EDGE_CURVE ( 'NONE', #28214, #51807, #31138, .T. ) ;
#13504 = UNCERTAINTY_MEASURE_WITH_UNIT (LENGTH_MEASURE( 1.000000000000000082E-05 ), #30058, 'distance_accuracy_value', 'NONE');
#13506 = VECTOR ( 'NONE', #56837, 1000.000000000000000 ) ;
#13507 = CARTESIAN_POINT ( 'NONE',  ( 110.2429982417149432, 29.99119854320844070, 71.45576479620103783 ) ) ;
#13508 = ORIENTED_EDGE ( 'NONE', *, *, #25356, .F. ) ;
#13509 = CARTESIAN_POINT ( 'NONE',  ( 283.0520942216416529, 21.63891660051134380, -3.973857610334881496 ) ) ;
#13510 = CARTESIAN_POINT ( 'NONE',  ( -62.55184817504201789, 17.87278652436698323, -70.07648453095528396 ) ) ;
#13511 = CARTESIAN_POINT ( 'NONE',  ( 202.7540649946182896, 105.3989460363904698, -77.92562021146432016 ) ) ;
#13512 =( NAMED_UNIT ( * ) SI_UNIT ( $, .STERADIAN. ) SOLID_ANGLE_UNIT ( ) );
#13513 = CARTESIAN_POINT ( 'NONE',  ( 276.2372751229154346, -21.75101418369302309, 3.308700176549365324 ) ) ;
#13514 = CARTESIAN_POINT ( 'NONE',  ( -168.2754450152258130, 81.89160173753974448, -90.15994169745837894 ) ) ;
#13515 = CARTESIAN_POINT ( 'NONE',  ( 0.000000000000000000, 70.00000000000000000, -60.00000000000000000 ) ) ;
#13516 = CARTESIAN_POINT ( 'NONE',  ( -49.45858366215606594, 13.25262207532078129, 59.66029130467421027 ) ) ;
#13517 = EDGE_CURVE ( 'NONE', #55258, #4522, #22205, .T. ) ;
#13518 = ADVANCED_FACE ( 'NONE', ( #43642 ), #1447, .T. ) ;
#13519 = CARTESIAN_POINT ( 'NONE',  ( -99.40806599580240288, 31.34569488980110208, -89.27206661197627113 ) ) ;
#13520 = ORIENTED_EDGE ( 'NONE', *, *, #54538, .F. ) ;
#13521 = STYLED_ITEM ( 'NONE', ( #34784 ), #16860 ) ;
#13522 = EDGE_CURVE ( 'NONE', #46266, #19247, #977, .T. ) ;
#13523 = CARTESIAN_POINT ( 'NONE',  ( -15.55634918610411077, -46.66904755831208718, 0.000000000000000000 ) ) ;
#13524 = CARTESIAN_POINT ( 'NONE',  ( 150.2941978382489197, 53.52137138947627903, 61.55703088605018536 ) ) ;
#13525 = CARTESIAN_POINT ( 'NONE',  ( 15.78827728214693416, -170.0000000000000000, 3.170157082241545687 ) ) ;
#13526 = CARTESIAN_POINT ( 'NONE',  ( 563.4809901518626702, 190.0000000000000000, 57.79371821540657095 ) ) ;
#13527 = CIRCLE ( 'NONE', #52806, 242.4895526022646379 ) ;
#13528 = CARTESIAN_POINT ( 'NONE',  ( 6.375108774214766072E-14, 31.11269837220806167, 0.000000000000000000 ) ) ;
#13529 = B_SPLINE_CURVE_WITH_KNOTS ( 'NONE', 3,
 ( #59729, #34431, #44960, #17529 ),
 .UNSPECIFIED., .F., .F.,
 ( 4, 4 ),
 ( 9.900409499053008115E-07, 0.05658314289920116785 ),
 .UNSPECIFIED. ) ;
#13530 = ORIENTED_EDGE ( 'NONE', *, *, #30823, .F. ) ;
#13531 = CARTESIAN_POINT ( 'NONE',  ( -6.689127551062013843, -5.375634714784636614, -0.3173508448886639410 ) ) ;
#13532 = ORIENTED_EDGE ( 'NONE', *, *, #31587, .T. ) ;
#13533 = VERTEX_POINT ( 'NONE', #21498 ) ;
#13534 = CARTESIAN_POINT ( 'NONE',  ( 47.73902449248994628, 57.85799893277891215, 43.58025477438756212 ) ) ;
#13535 = CARTESIAN_POINT ( 'NONE',  ( 157.0316110297313514, 58.58403635656375030, 44.40946747225339664 ) ) ;
#13536 = CARTESIAN_POINT ( 'NONE',  ( 51.04336025769664076, 7.992588086412792059, 26.66469104408688651 ) ) ;
#13537 = ORIENTED_EDGE ( 'NONE', *, *, #18891, .F. ) ;
#13538 = CARTESIAN_POINT ( 'NONE',  ( -44.99999999999998579, 25.00000000000000000, 2.000000000000015543 ) ) ;
#13539 = CARTESIAN_POINT ( 'NONE',  ( -179.2177980985565284, 94.18084789436635162, 7.101110558428060493 ) ) ;
#13540 = CARTESIAN_POINT ( 'NONE',  ( -3.244108878396732010, 6.635632329121484041, 16.72956101399090301 ) ) ;
#13541 = CIRCLE ( 'NONE', #40490, 9.999999999999994671 ) ;
#13542 = DIRECTION ( 'NONE',  ( 0.000000000000000000, 0.000000000000000000, -1.000000000000000000 ) ) ;
#13543 = CARTESIAN_POINT ( 'NONE',  ( -86.15466590221103615, 26.40813842494318209, 38.41035032410803041 ) ) ;
#13544 = CARTESIAN_POINT ( 'NONE',  ( 151.3976820382521851, 53.07948349322499837, 94.99999999999866418 ) ) ;
#13545 = DIRECTION ( 'NONE',  ( -0.000000000000000000, 1.000000000000000000, -0.000000000000000000 ) ) ;
#13546 = EDGE_LOOP ( 'NONE', ( #31855, #65207, #43147, #59425 ) ) ;
#13547 = CARTESIAN_POINT ( 'NONE',  ( 117.4830770399668012, 32.37795270233550582, -41.39853099672338743 ) ) ;
#13548 = CARTESIAN_POINT ( 'NONE',  ( 10.55634918610400419, -15.55634918610406103, 0.000000000000000000 ) ) ;
#13549 = FACE_OUTER_BOUND ( 'NONE', #11550, .T. ) ;
#13550 = B_SPLINE_CURVE_WITH_KNOTS ( 'NONE', 3,
 ( #5015, #26482, #21204, #19827, #42651, #48942, #34806, #10981, #1476, #22237, #28202, #784, #22937, #33503, #43676, #59506, #38773, #37715, #16946, #32791 ),
 .UNSPECIFIED., .F., .F.,
 ( 4, 2, 2, 2, 2, 2, 2, 2, 2, 4 ),
 ( 0.000000000000000000, 0.001358410513504409783, 0.002037615770256615000, 0.002716821027008819566, 0.004075231540513249949, 0.005433642054017679898, 0.006792052567522109847, 0.008150463081026539797, 0.009508873594530970613, 0.01086728410803540143 ),
 .UNSPECIFIED. ) ;
#13551 = DIRECTION ( 'NONE',  ( -1.000000000000000000, 0.000000000000000000, 0.000000000000000000 ) ) ;
#13553 = ORIENTED_EDGE ( 'NONE', *, *, #69261, .T. ) ;
#13552 = CARTESIAN_POINT ( 'NONE',  ( 75.00000000000000000, 1.249999999999979350, 170.0000000000000000 ) ) ;
#13554 = CARTESIAN_POINT ( 'NONE',  ( 85.67138972405899722, 19.09593469918314312, -50.77549759938765561 ) ) ;
#13555 = VECTOR ( 'NONE', #23103, 1000.000000000000114 ) ;
#13556 = ORIENTED_EDGE ( 'NONE', *, *, #797, .F. ) ;
#13557 = CARTESIAN_POINT ( 'NONE',  ( -149.2910611247327779, 63.99625741915655652, 72.56537183036279259 ) ) ;
#13558 = CARTESIAN_POINT ( 'NONE',  ( 86.15454111412293514, 20.32174891186169319, 29.71208757247930521 ) ) ;
#13559 = DIRECTION ( 'NONE',  ( -0.000000000000000000, -0.000000000000000000, 1.000000000000000000 ) ) ;
#13560 = PLANE ( 'NONE',  #58601 ) ;
#13561 = CARTESIAN_POINT ( 'NONE',  ( -439.4229916354183842, 400.0000000000065370, -128.9497041420121093 ) ) ;
#13562 = DIRECTION ( 'NONE',  ( 1.000000000000000000, -0.000000000000000000, 0.000000000000000000 ) ) ;
#13563 = CARTESIAN_POINT ( 'NONE',  ( -174.7817412490652202, 90.52199442492060655, -22.69333526547698554 ) ) ;
#13564 = CARTESIAN_POINT ( 'NONE',  ( -31.90315521289063128, -56.64813493366051489, 170.0000000000000000 ) ) ;
#13565 = ORIENTED_EDGE ( 'NONE', *, *, #54238, .F. ) ;
#13566 = ORIENTED_EDGE ( 'NONE', *, *, #42878, .F. ) ;
#13567 = CARTESIAN_POINT ( 'NONE',  ( 106.6228877857910646, 27.24245963308690577, 70.54164431714124817 ) ) ;
#13568 = LINE ( 'NONE', #33988, #37976 ) ;
#13569 = CARTESIAN_POINT ( 'NONE',  ( -189.2739965869454295, 107.1373753350176372, 64.38768254793554036 ) ) ;
#13570 = CARTESIAN_POINT ( 'NONE',  ( -452.6627218934913230, 399.9999999999998863, 113.5502958579881749 ) ) ;
#13571 = DIRECTION ( 'NONE',  ( 1.000000000000000000, 1.850550996349095901E-16, 1.228197773518735191E-20 ) ) ;
#13572 = CARTESIAN_POINT ( 'NONE',  ( 164.8886903222556839, 63.65672212134877839, -71.60819778663672253 ) ) ;
#13573 = ORIENTED_EDGE ( 'NONE', *, *, #24510, .T. ) ;
#13574 = ORIENTED_EDGE ( 'NONE', *, *, #33002, .T. ) ;
#13575 = EDGE_CURVE ( 'NONE', #41022, #10664, #5662, .T. ) ;
#13576 = ORIENTED_EDGE ( 'NONE', *, *, #51775, .F. ) ;
#13577 = DIRECTION ( 'NONE',  ( -0.000000000000000000, -1.000000000000000000, -0.000000000000000000 ) ) ;
#13578 = CARTESIAN_POINT ( 'NONE',  ( 39.40195752203892710, -170.0000000000000000, 10.56928371549958889 ) ) ;
#13579 = CARTESIAN_POINT ( 'NONE',  ( 178.6969023688950244, 76.22585248861962270, -90.29539480279383667 ) ) ;
#13580 = CARTESIAN_POINT ( 'NONE',  ( 68.95451040317566083, 14.12887482153123919, -38.61394121317524508 ) ) ;
#13581 = DIRECTION ( 'NONE',  ( -0.000000000000000000, -1.000000000000000000, -0.000000000000000000 ) ) ;
#13582 = CARTESIAN_POINT ( 'NONE',  ( -56.96436614829621448, 16.24647150911285109, 30.56099534412708252 ) ) ;
#13583 = EDGE_CURVE ( 'NONE', #2845, #64522, #19355, .T. ) ;
#13584 = CARTESIAN_POINT ( 'NONE',  ( 133.8566784816069628, 41.42467568809809819, -9.178760341931967659 ) ) ;
#13585 = CARTESIAN_POINT ( 'NONE',  ( -4.174999999999999822, 5.112900386440199535E-16, -0.5776712190230133270 ) ) ;
#13586 = CARTESIAN_POINT ( 'NONE',  ( 32.38131036485454217, 7.599882848866447382, 93.82335863281235788 ) ) ;
#13587 =( GEOMETRIC_REPRESENTATION_CONTEXT ( 3 ) GLOBAL_UNCERTAINTY_ASSIGNED_CONTEXT ( ( #40235 ) ) GLOBAL_UNIT_ASSIGNED_CONTEXT ( ( #47079, #24609, #62924 ) ) REPRESENTATION_CONTEXT ( 'NONE', 'WORKASPACE' ) );
#13588 =( NAMED_UNIT ( * ) PLANE_ANGLE_UNIT ( ) SI_UNIT ( $, .RADIAN. ) );
#13589 = ORIENTED_EDGE ( 'NONE', *, *, #21971, .T. ) ;
#13590 = CARTESIAN_POINT ( 'NONE',  ( -0.7215816834507526867, 6.532459459468098473, -45.33604404609089755 ) ) ;
#13591 = DIRECTION ( 'NONE',  ( 0.000000000000000000, 1.000000000000000000, 0.000000000000000000 ) ) ;
#13592 = CARTESIAN_POINT ( 'NONE',  ( -189.2346268516247960, 107.0830361517164988, -41.89910121709165480 ) ) ;
#13593 = CARTESIAN_POINT ( 'NONE',  ( -143.2464978228198333, 59.04559547356109306, 15.51374128211022985 ) ) ;
#13594 = CARTESIAN_POINT ( 'NONE',  ( 16.27775141556967498, 7.523247835309955889, -23.67439350822211708 ) ) ;
#13595 = CARTESIAN_POINT ( 'NONE',  ( -104.5827168854524558, 33.96561401163047833, -76.51241882879068612 ) ) ;
#13596 = EDGE_CURVE ( 'NONE', #1198, #19781, #47131, .T. ) ;
#13597 = ORIENTED_EDGE ( 'NONE', *, *, #54935, .T. ) ;
#13598 = AXIS2_PLACEMENT_3D ( 'NONE', #21256, #26194, #15977 ) ;
#13599 = CARTESIAN_POINT ( 'NONE',  ( -24.85653282846401879, -170.0000000000000000, 94.99999999999866418 ) ) ;
#13600 = CARTESIAN_POINT ( 'NONE',  ( -38.16652041892308489, 11.81761816422916311, -46.16894994732523827 ) ) ;
#13601 = CYLINDRICAL_SURFACE ( 'NONE', #15479, 4.999999999999997335 ) ;
#13602 = CONTEXT_DEPENDENT_SHAPE_REPRESENTATION ( #60226, #14824 ) ;
#13603 = CARTESIAN_POINT ( 'NONE',  ( -165.9043865781291345, 79.43878925126232105, 89.93817603964164675 ) ) ;
#13604 = ORIENTED_EDGE ( 'NONE', *, *, #22162, .F. ) ;
#13605 = CARTESIAN_POINT ( 'NONE',  ( 126.3554864210861837, 38.22801630372151749, 10.39375937215169543 ) ) ;
#13606 = B_SPLINE_CURVE_WITH_KNOTS ( 'NONE', 3,
 ( #26366, #27381, #38289, #47806, #53414, #59730, #26022, #53761, #5583, #63658, #69265, #21091, #42535, #63988, #10515, #16490, #31984, #27036, #48467, #21761, #65384, #27733, #17890, #12611, #17172, #55158, #1359, #39004, #22813, #38645, #44257, #6982, #44961, #23864, #34072, #45306, #60788, #55513, #54451, #40037, #7340, #66790, #33726, #66446, #12264, #28796, #50245, #39345, #60448, #6280, #23171, #2066, #65738, #11907, #44617, #11541, #60085 ),
 .UNSPECIFIED., .F., .F.,
 ( 4, 2, 2, 2, 2, 2, 2, 2, 2, 2, 2, 2, 2, 2, 1, 2, 2, 2, 2, 2, 2, 2, 2, 2, 2, 2, 2, 2, 4 ),
 ( 0.000000000000000000, 0.001985873147602438497, 0.002978809721403657528, 0.003971746295204876993, 0.004964682869006096892, 0.005957619442807315056, 0.006950556016608534955, 0.007943492590409753987, 0.008936429164210973886, 0.009929365738012193784, 0.01092230231181341195, 0.01191523888561463011, 0.01390111203321707858, 0.01489404860701831583, 0.01588698518081955308, 0.01687992175462078859, 0.01787285832842202757, 0.01985873147602450206, 0.02085166804982573063, 0.02184460462362696268, 0.02283754119742819125, 0.02383047777122941982, 0.02581635091883191166, 0.02680928749263316452, 0.02780222406643441391, 0.02879516064023566677, 0.02978809721403691615, 0.03078103378783816901, 0.03177397036163941840 ),
 .UNSPECIFIED. ) ;
#13607 = CARTESIAN_POINT ( 'NONE',  ( -46.06722295615789875, 46.37372919877054755, 41.38025477438755928 ) ) ;
#13608 = DIRECTION ( 'NONE',  ( 0.000000000000000000, 0.000000000000000000, 1.000000000000000000 ) ) ;
#13609 = VERTEX_POINT ( 'NONE', #17981 ) ;
#13610 = CARTESIAN_POINT ( 'NONE',  ( 150.7605657748150065, 53.86013773008568961, 87.22787840158356687 ) ) ;
#13611 = ORIENTED_EDGE ( 'NONE', *, *, #42027, .F. ) ;
#13612 = CARTESIAN_POINT ( 'NONE',  ( 32.06997139192709767, 56.95813133885488355, 43.58025477438756212 ) ) ;
#13613 = CARTESIAN_POINT ( 'NONE',  ( 26.11269837220800127, -26.11269837220812562, 0.000000000000000000 ) ) ;
#13614 = CARTESIAN_POINT ( 'NONE',  ( -157.0079874970172682, 72.18249880494037996, 38.49446316589058625 ) ) ;
#13615 = CARTESIAN_POINT ( 'NONE',  ( -16.43619359402603664, -18.99971924381128474, 3.061616997868437868E-16 ) ) ;
#13616 = CYLINDRICAL_SURFACE ( 'NONE', #52974, 7.500000000000020428 ) ;
#13618 = ORIENTED_EDGE ( 'NONE', *, *, #45185, .F. ) ;
#13617 = DIRECTION ( 'NONE',  ( 0.000000000000000000, 0.000000000000000000, 1.000000000000000000 ) ) ;
#13619 = CARTESIAN_POINT ( 'NONE',  ( -0.6830060531215994546, 7.537854477244023244, -94.16412398650113857 ) ) ;
#13620 = ORIENTED_EDGE ( 'NONE', *, *, #24634, .T. ) ;
#13621 = ORIENTED_EDGE ( 'NONE', *, *, #27861, .T. ) ;
#13622 = CARTESIAN_POINT ( 'NONE',  ( 174.4978817191264397, 73.57770570413202904, 33.21040157506908486 ) ) ;
#13623 = CARTESIAN_POINT ( 'NONE',  ( 22.52576749827964520, 6.809805260274345962, -73.19476423806628418 ) ) ;
#13625 = ORIENTED_EDGE ( 'NONE', *, *, #61830, .T. ) ;
#13624 = DIRECTION ( 'NONE',  ( -1.000000000000000000, 0.000000000000000000, 0.000000000000000000 ) ) ;
#13626 = CARTESIAN_POINT ( 'NONE',  ( 445.3372781065086201, 177.8591479523844612, 78.55029585798806124 ) ) ;
#13627 = VECTOR ( 'NONE', #28297, 1000.000000000000114 ) ;
#13628 = CARTESIAN_POINT ( 'NONE',  ( -76.78104518372333587, 22.68568622761702613, -49.89015923587386681 ) ) ;
#13629 = ORIENTED_EDGE ( 'NONE', *, *, #33270, .F. ) ;
#13630 = AXIS2_PLACEMENT_3D ( 'NONE', #7906, #29703, #51165 ) ;
#13631 = ADVANCED_FACE ( 'NONE', ( #1808 ), #45396, .T. ) ;
#13632 = CARTESIAN_POINT ( 'NONE',  ( 212.0104729185451902, 118.7959000526603006, -68.97424183727284230 ) ) ;
#13633 = AXIS2_PLACEMENT_3D ( 'NONE', #54174, #738, #32406 ) ;
#13634 = AXIS2_PLACEMENT_3D ( 'NONE', #24918, #36852, #25618 ) ;
#13635 = ADVANCED_FACE ( 'NONE', ( #13396 ), #62265, .T. ) ;
#13636 = CARTESIAN_POINT ( 'NONE',  ( 133.8566784816069060, 42.60093787723652525, 44.51034083899536142 ) ) ;
#13637 = CARTESIAN_POINT ( 'NONE',  ( 117.4806398654733783, 33.50379325299404343, 35.07699718365589803 ) ) ;
#13638 = PLANE ( 'NONE',  #57238 ) ;
#13639 = DIRECTION ( 'NONE',  ( -1.387778780781445922E-16, 1.000000000000000000, 1.232595164407830946E-32 ) ) ;
#13640 = EDGE_LOOP ( 'NONE', ( #55151, #346, #49689, #9903 ) ) ;
#13641 = ORIENTED_EDGE ( 'NONE', *, *, #27798, .F. ) ;
#13642 = CARTESIAN_POINT ( 'NONE',  ( -148.0058283997321382, 64.22864592525513672, -22.81961389825241682 ) ) ;
#13643 = VECTOR ( 'NONE', #61248, 1000.000000000000114 ) ;
#13644 = DIRECTION ( 'NONE',  ( 0.000000000000000000, 0.000000000000000000, 1.000000000000000000 ) ) ;
#13645 = CARTESIAN_POINT ( 'NONE',  ( -56.92000000000000171, -26.09918303830819397, 30.00000000000000000 ) ) ;
#13646 = FACE_OUTER_BOUND ( 'NONE', #5556, .T. ) ;
#13647 = CARTESIAN_POINT ( 'NONE',  ( -144.9439644317224349, 60.40328483334189258, 32.26430146232742402 ) ) ;
#13648 = EDGE_CURVE ( 'NONE', #34548, #37698, #38722, .T. ) ;
#13649 = CARTESIAN_POINT ( 'NONE',  ( -133.3765738414514885, 51.62252165471728915, 65.54115532702775226 ) ) ;
#13650 = CARTESIAN_POINT ( 'NONE',  ( -165.7689197919844730, 79.30072199592272852, -67.54572964526467160 ) ) ;
#13651 = ORIENTED_EDGE ( 'NONE', *, *, #29773, .F. ) ;
#13652 = DIRECTION ( 'NONE',  ( -1.000000000000000000, 0.000000000000000000, 0.000000000000000000 ) ) ;
#13653 = EDGE_CURVE ( 'NONE', #39038, #68160, #26893, .T. ) ;
#13654 = EDGE_LOOP ( 'NONE', ( #14823, #29626, #23861, #51943 ) ) ;
#13655 = CARTESIAN_POINT ( 'NONE',  ( 38.42020198992005220, 8.283430712587444233, 29.96235999322596300 ) ) ;
#13656 = CARTESIAN_POINT ( 'NONE',  ( 55.65793654284612302, 50.28674377798304107, 170.0000000000000000 ) ) ;
#13657 = ORIENTED_EDGE ( 'NONE', *, *, #24309, .F. ) ;
#13658 = DIRECTION ( 'NONE',  ( 1.000000000000000000, 0.000000000000000000, 0.000000000000000000 ) ) ;
#13659 = B_SPLINE_CURVE_WITH_KNOTS ( 'NONE', 3,
 ( #26867, #41329, #36394, #9665, #57504, #20211, #15283, #36742, #9312, #31460, #21245, #20543, #31127, #26179, #68408, #47615, #63470, #25508, #58865, #20902, #63124, #42693, #41667, #57846, #15965, #52895, #62784, #15626, #14588, #53582, #42356, #68071, #63815, #37076, #36048, #52219 ),
 .UNSPECIFIED., .F., .F.,
 ( 4, 2, 2, 2, 2, 2, 2, 2, 2, 2, 2, 2, 2, 2, 2, 2, 2, 4 ),
 ( 0.000000000000000000, 0.001545474820159029039, 0.003090949640318058078, 0.004636424460477087985, 0.006181899280636116156, 0.007727374100795145195, 0.008500111510874661450, 0.009272848920954175969, 0.01081832374111321542, 0.01236379856127225139, 0.01390927338143128911, 0.01545474820159032682, 0.01700022302174936453, 0.01854569784190840051, 0.02009117266206743996, 0.02163664748222647594, 0.02318212230238551191, 0.02472759712254454789 ),
 .UNSPECIFIED. ) ;
#13660 = DIRECTION ( 'NONE',  ( -0.9839295885986295565, -0.1785568947986370392, 0.000000000000000000 ) ) ;
#13661 = DIRECTION ( 'NONE',  ( 0.000000000000000000, 0.000000000000000000, -1.000000000000000000 ) ) ;
#13662 = DIRECTION ( 'NONE',  ( 0.000000000000000000, 0.000000000000000000, 1.000000000000000000 ) ) ;
#13663 = CARTESIAN_POINT ( 'NONE',  ( 32.56927464314650678, 7.618924692399907883, 7.466848099861418397 ) ) ;
#13664 = CARTESIAN_POINT ( 'NONE',  ( -10.24974837193994404, 8.069704751038624835, -35.80395452523003996 ) ) ;
#13665 = ADVANCED_FACE ( 'NONE', ( #57691 ), #14768, .T. ) ;
#13666 = DIRECTION ( 'NONE',  ( 0.000000000000000000, 0.000000000000000000, -1.000000000000000000 ) ) ;
#13667 = ORIENTED_EDGE ( 'NONE', *, *, #15498, .F. ) ;
#13668 = CARTESIAN_POINT ( 'NONE',  ( -109.4756385662671221, 36.58892558929082384, -94.07530769078934441 ) ) ;
#13669 = ORIENTED_EDGE ( 'NONE', *, *, #26960, .T. ) ;
#13670 = CYLINDRICAL_SURFACE ( 'NONE', #57633, 22.00000000000000355 ) ;
#13671 = CARTESIAN_POINT ( 'NONE',  ( -39.55079474733624068, -51.59997227571039957, 170.0000000000000000 ) ) ;
#13672 = DIRECTION ( 'NONE',  ( 0.000000000000000000, -1.385458760688113094E-14, 1.000000000000000000 ) ) ;
#13673 = ORIENTED_EDGE ( 'NONE', *, *, #49690, .T. ) ;
#13674 = CARTESIAN_POINT ( 'NONE',  ( 432.4999999999999432, 207.5000000000000284, 0.000000000000000000 ) ) ;
#13675 = CARTESIAN_POINT ( 'NONE',  ( 153.4509883044095773, 55.84811350575044742, -76.80503978816277311 ) ) ;
#13676 = CARTESIAN_POINT ( 'NONE',  ( -33.13098007862451055, 9.875138601866705557, 45.02716274319689660 ) ) ;
#13677 = CARTESIAN_POINT ( 'NONE',  ( 134.3172730033263065, 41.70277427218488953, -36.02331093239567394 ) ) ;
#13678 = EDGE_CURVE ( 'NONE', #33970, #13204, #57343, .T. ) ;
#13679 = VERTEX_POINT ( 'NONE', #57000 ) ;
#13680 = VECTOR ( 'NONE', #20509, 1000.000000000000000 ) ;
#13681 = CARTESIAN_POINT ( 'NONE',  ( -156.0204364459164594, 71.27041535366184632, 68.79358406586271713 ) ) ;
#13682 = EDGE_CURVE ( 'NONE', #275, #63707, #43681, .T. ) ;
#13683 = ADVANCED_FACE ( 'NONE', ( #20738 ), #63660, .F. ) ;
#13684 = CARTESIAN_POINT ( 'NONE',  ( -121.1775535805057444, 43.46577565517550568, 43.97189950139811287 ) ) ;
#13685 = CARTESIAN_POINT ( 'NONE',  ( -60.97727891098336528, 16.35024395194892577, -47.34151352721814021 ) ) ;
#13686 = ORIENTED_EDGE ( 'NONE', *, *, #15787, .F. ) ;
#13687 = CARTESIAN_POINT ( 'NONE',  ( -179.8926034784145429, 96.58272071140103776, -72.29268138171191538 ) ) ;
#13688 = AXIS2_PLACEMENT_3D ( 'NONE', #49231, #1067, #65435 ) ;
#13689 = LINE ( 'NONE', #29515, #421 ) ;
#13690 = PRODUCT_DEFINITION_SHAPE ( 'NONE', 'NONE',  #69597 ) ;
#13691 = CARTESIAN_POINT ( 'NONE',  ( 110.2429982417149290, 28.88204397445231209, 29.61121420573730489 ) ) ;
#13692 = VECTOR ( 'NONE', #25426, 1000.000000000000000 ) ;
#13694 = AXIS2_PLACEMENT_3D ( 'NONE', #35133, #51325, #3139 ) ;
#13693 = CARTESIAN_POINT ( 'NONE',  ( 92.32928948494030408, 21.44473173578322545, -92.06573559034401910 ) ) ;
#13695 = LINE ( 'NONE', #51338, #5425 ) ;
#13696 = ORIENTED_EDGE ( 'NONE', *, *, #42477, .T. ) ;
#13697 = LINE ( 'NONE', #49932, #55890 ) ;
#13698 = CARTESIAN_POINT ( 'NONE',  ( 117.7447573007802788, 32.50990724960315958, -69.77678085006658648 ) ) ;
#13699 = CARTESIAN_POINT ( 'NONE',  ( 65.40032188136231639, 13.23841673691966747, 57.04257784809311715 ) ) ;
#13700 = CARTESIAN_POINT ( 'NONE',  ( 136.9822423813093337, 44.53121110416872597, 3.344055275432845420 ) ) ;
#13701 = CARTESIAN_POINT ( 'NONE',  ( 14.99999999999998579, 0.000000000000000000, -0.000000000000000000 ) ) ;
#13702 = AXIS2_PLACEMENT_3D ( 'NONE', #66154, #60846, #17230 ) ;
#13703 = ORIENTED_EDGE ( 'NONE', *, *, #37624, .F. ) ;
#13704 = CARTESIAN_POINT ( 'NONE',  ( 7.347880794884118356E-15, 70.00000000000000000, 60.00000000000000000 ) ) ;
#13705 = ORIENTED_EDGE ( 'NONE', *, *, #50896, .T. ) ;
#13706 = DIRECTION ( 'NONE',  ( 2.922263668027335568E-20, 1.000000000000000000, -5.551115123125781470E-17 ) ) ;
#13707 = CARTESIAN_POINT ( 'NONE',  ( 137.2430147073457931, 43.50693516253637227, 83.99996777949063187 ) ) ;
#13708 = ORIENTED_EDGE ( 'NONE', *, *, #25060, .F. ) ;
#13709 = CARTESIAN_POINT ( 'NONE',  ( -142.0685766576042113, 58.11789490499572963, -68.04818472065136348 ) ) ;
#13710 = LINE ( 'NONE', #63886, #21239 ) ;
#13711 = PLANE ( 'NONE',  #28295 ) ;
#13712 = CARTESIAN_POINT ( 'NONE',  ( 164.8886903222557407, 63.65672212134879260, -44.76364719617309618 ) ) ;
#13713 = VERTEX_POINT ( 'NONE', #10176 ) ;
#13714 = ADVANCED_FACE ( 'NONE', ( #65031 ), #64685, .T. ) ;
#13715 = CARTESIAN_POINT ( 'NONE',  ( -102.2801239173131052, 33.91021738430207222, 18.67452391595144334 ) ) ;
#13716 = CARTESIAN_POINT ( 'NONE',  ( 204.6977192012829789, -170.0000000000000000, 44.20772073876944575 ) ) ;
#13717 = EDGE_CURVE ( 'NONE', #17316, #18390, #43558, .T. ) ;
#13718 = DIRECTION ( 'NONE',  ( 0.000000000000000000, 0.000000000000000000, -1.000000000000000000 ) ) ;
#13719 = DIRECTION ( 'NONE',  ( 0.000000000000000000, 0.000000000000000000, 1.000000000000000000 ) ) ;
#13720 = CARTESIAN_POINT ( 'NONE',  ( -165.6393662153604964, 79.16886183052817216, 38.92739272313387033 ) ) ;
#13721 = CARTESIAN_POINT ( 'NONE',  ( -142.1450925953585340, 58.17784622801090677, -94.47787185721898595 ) ) ;
#13722 = DIRECTION ( 'NONE',  ( 0.000000000000000000, 1.000000000000000000, 0.000000000000000000 ) ) ;
#13723 = EDGE_LOOP ( 'NONE', ( #32213, #57682, #49015, #14936 ) ) ;
#13724 = CARTESIAN_POINT ( 'NONE',  ( 10.00000000000000178, -31.50328976398030534, -9.999999999999998224 ) ) ;
#13725 = CARTESIAN_POINT ( 'NONE',  ( -14.84903512415885452, 8.461292896365067762, 67.10196148585319520 ) ) ;
#13726 = ORIENTED_EDGE ( 'NONE', *, *, #2103, .F. ) ;
#13727 = VECTOR ( 'NONE', #55212, 1000.000000000000000 ) ;
#13728 = CARTESIAN_POINT ( 'NONE',  ( -154.6085044440278864, 69.98390342970671441, -47.81608844076072273 ) ) ;
#13729 = CARTESIAN_POINT ( 'NONE',  ( 211.5034924207028553, 118.0100795718635283, -13.81556118458025395 ) ) ;
#13730 = CIRCLE ( 'NONE', #3586, 5.000000000000004441 ) ;
#13731 = CARTESIAN_POINT ( 'NONE',  ( -4.731197926646205865, 7.716745361328039898, 30.77918364689588415 ) ) ;
#13732 = FACE_OUTER_BOUND ( 'NONE', #13654, .T. ) ;
#13733 = CARTESIAN_POINT ( 'NONE',  ( -51.77439426130688105, 13.82695438436704016, -62.81093775181126659 ) ) ;
#13734 = ADVANCED_FACE ( 'NONE', ( #37247 ), #48140, .F. ) ;
#13735 = CARTESIAN_POINT ( 'NONE',  ( 207.4696221732442893, 110.2206209205162111, -50.80684766909965333 ) ) ;
#13737 = CARTESIAN_POINT ( 'NONE',  ( -44.00727179482512241, -47.83680621839620528, 170.0000000000000000 ) ) ;
#13736 = AXIS2_PLACEMENT_3D ( 'NONE', #48445, #36896, #20713 ) ;
#13739 = ADVANCED_FACE ( 'NONE', ( #15803, #10516, #11908 ), #49525, .T. ) ;
#13738 = CARTESIAN_POINT ( 'NONE',  ( 110.7164744784863757, 29.10110206241301611, 17.76666361527367499 ) ) ;
#13740 = VERTEX_POINT ( 'NONE', #54452 ) ;
#13741 = CARTESIAN_POINT ( 'NONE',  ( -102.2801239173131194, 33.91021738430207222, -35.01457726497591239 ) ) ;
#13742 = ORIENTED_EDGE ( 'NONE', *, *, #31396, .T. ) ;
#13743 = CARTESIAN_POINT ( 'NONE',  ( 15.55634918610403261, 4.999999999999969802, 2.000000000000001776 ) ) ;
#13744 = ADVANCED_FACE ( 'NONE', ( #5584 ), #5919, .T. ) ;
#13745 = CARTESIAN_POINT ( 'NONE',  ( 41.09759788073306908, 9.651672055033841957, -8.965407513425770247 ) ) ;
#13746 = DIRECTION ( 'NONE',  ( 1.000000000000000000, 0.000000000000000000, 0.000000000000000000 ) ) ;
#13747 = CARTESIAN_POINT ( 'NONE',  ( -173.1211646369891071, 87.12891641440859303, 18.97714401617737678 ) ) ;
#13748 = CARTESIAN_POINT ( 'NONE',  ( -13.57610226747640425, 7.333588782202060230, 86.44604924231978771 ) ) ;
#13749 = CARTESIAN_POINT ( 'NONE',  ( -105.4487797565983982, 35.55724615608641415, -22.48385247276568677 ) ) ;
#13750 = DIRECTION ( 'NONE',  ( 0.000000000000000000, 0.000000000000000000, 1.000000000000000000 ) ) ;
#13751 = CARTESIAN_POINT ( 'NONE',  ( -165.9992860119574232, 79.53569239468046703, 62.79718458295194239 ) ) ;
#13752 = EDGE_LOOP ( 'NONE', ( #53113, #24876, #68609, #43593 ) ) ;
#13753 = ORIENTED_EDGE ( 'NONE', *, *, #50004, .F. ) ;
#13754 = CARTESIAN_POINT ( 'NONE',  ( 444.9999999999999432, -35.00000000000000000, -2.000000000000000000 ) ) ;
#13755 = CARTESIAN_POINT ( 'NONE',  ( 188.9999999999999432, 225.0000000000000000, 72.99999999999998579 ) ) ;
#13756 = CARTESIAN_POINT ( 'NONE',  ( 174.9042454172879673, 72.57746269938724026, -12.60028719114147400 ) ) ;
#13757 = CARTESIAN_POINT ( 'NONE',  ( 103.0004140566503281, 26.76634862952790428, 65.96999840838908824 ) ) ;
#13758 = DIRECTION ( 'NONE',  ( -0.000000000000000000, -0.000000000000000000, -1.000000000000000000 ) ) ;
#13759 = DIRECTION ( 'NONE',  ( 1.000000000000000000, 0.000000000000000000, -0.000000000000000000 ) ) ;
#13760 = EDGE_LOOP ( 'NONE', ( #4452, #14809, #29639, #56992 ) ) ;
#13761 = ADVANCED_FACE ( 'NONE', ( #54811 ), #65386, .F. ) ;
#13762 = EDGE_CURVE ( 'NONE', #16778, #8019, #38291, .T. ) ;
#13763 = DIRECTION ( 'NONE',  ( -1.000000000000000000, 0.000000000000000000, 0.000000000000000000 ) ) ;
#13764 = CARTESIAN_POINT ( 'NONE',  ( 22.90619343622340054, 7.840927939412482672, -45.43282700353950077 ) ) ;
#13765 = CARTESIAN_POINT ( 'NONE',  ( 8.337549025192450003, 7.382630697225773808, 63.37153782633733812 ) ) ;
#13766 = PLANE ( 'NONE',  #15016 ) ;
#13767 = FACE_BOUND ( 'NONE', #550, .T. ) ;
#13768 = EDGE_CURVE ( 'NONE', #40885, #66752, #11205, .T. ) ;
#13769 = EDGE_LOOP ( 'NONE', ( #14270, #12142 ) ) ;
#13770 = ORIENTED_EDGE ( 'NONE', *, *, #31594, .T. ) ;
#13771 = LINE ( 'NONE', #40503, #32390 ) ;
#13772 = CARTESIAN_POINT ( 'NONE',  ( -7.329206686002009974E-14, -41.66904755831212270, 2.000000000000001776 ) ) ;
#13773 = VECTOR ( 'NONE', #44763, 1000.000000000000000 ) ;
#13774 = DIRECTION ( 'NONE',  ( 2.298858655265451588E-16, 9.825793442286241754E-17, 1.000000000000000000 ) ) ;
#13775 = CARTESIAN_POINT ( 'NONE',  ( -173.1211646369891355, -170.0000000000000000, 57.66624519710472185 ) ) ;
#13776 = CARTESIAN_POINT ( 'NONE',  ( 13.52497250360456782, 6.438709070458922490, 84.04600024306211026 ) ) ;
#13777 = CARTESIAN_POINT ( 'NONE',  ( 82.94943325692331371, 18.19803534719806137, -76.70580516979920560 ) ) ;
#13778 = VECTOR ( 'NONE', #2406, 1000.000000000000000 ) ;
#13779 = EDGE_LOOP ( 'NONE', ( #39660, #49194, #20199, #56429 ) ) ;
#13780 = CARTESIAN_POINT ( 'NONE',  ( 44.99999999999999289, -20.00000000000000355, 2.000000000000015543 ) ) ;
#13781 = CARTESIAN_POINT ( 'NONE',  ( -6.689127551062009402, -5.375634714784637502, -9.182649155111338501 ) ) ;
#13782 = VERTEX_POINT ( 'NONE', #6282 ) ;
#13783 = CIRCLE ( 'NONE', #16031, 75.31295361348099959 ) ;
#13784 = FACE_OUTER_BOUND ( 'NONE', #31737, .T. ) ;
#13785 = ORIENTED_EDGE ( 'NONE', *, *, #7224, .T. ) ;
#13786 = CARTESIAN_POINT ( 'NONE',  ( -80.54757501605354264, 23.04700348514567665, -62.19583100815920318 ) ) ;
#13787 = CARTESIAN_POINT ( 'NONE',  ( 31.11269837220812562, 31.11269837220800483, 85.00100000000000477 ) ) ;
#13788 = VECTOR ( 'NONE', #1128, 1000.000000000000000 ) ;
#13789 = CARTESIAN_POINT ( 'NONE',  ( 94.06699947028482711, 23.17027898120150198, -71.16360367612234938 ) ) ;
#13790 = VERTEX_POINT ( 'NONE', #27734 ) ;
#13791 = VERTEX_POINT ( 'NONE', #54097 ) ;
#13792 = CARTESIAN_POINT ( 'NONE',  ( 46.65974587859240330, 10.48396258569371398, 62.30449875318643649 ) ) ;
#13793 = CARTESIAN_POINT ( 'NONE',  ( -15.55634918610408945, -31.11269837220804035, 85.00100000000000477 ) ) ;
#13794 = CARTESIAN_POINT ( 'NONE',  ( 103.0004140566503281, 26.76634862952790428, 12.28089722746173429 ) ) ;
#13795 = ORIENTED_EDGE ( 'NONE', *, *, #49680, .F. ) ;
#13796 = DIRECTION ( 'NONE',  ( -1.000000000000000000, 0.000000000000000000, 0.000000000000000000 ) ) ;
#13797 = EDGE_CURVE ( 'NONE', #53534, #37383, #27382, .T. ) ;
#13798 = CARTESIAN_POINT ( 'NONE',  ( 177.7964363391244831, 76.75162026635257462, -77.32570004121048157 ) ) ;
#13799 = CARTESIAN_POINT ( 'NONE',  ( 7.484861546145031852, 64.56761454192836425, 40.00000000000003553 ) ) ;
#13800 = CARTESIAN_POINT ( 'NONE',  ( 113.4493678088378630, 30.39339414805074213, -9.781423810587101642 ) ) ;
#13801 = CARTESIAN_POINT ( 'NONE',  ( 79.22872707466396491, 18.07970189365808977, -42.07899737201626778 ) ) ;
#13802 = DIRECTION ( 'NONE',  ( -0.3513748240813304724, -0.9362348706397417564, 0.000000000000000000 ) ) ;
#13803 = EDGE_LOOP ( 'NONE', ( #55434, #8020, #7369, #49703, #48341 ) ) ;
#13804 = ORIENTED_EDGE ( 'NONE', *, *, #27232, .T. ) ;
#13805 = CARTESIAN_POINT ( 'NONE',  ( 86.62931800182293784, 19.42108912189596381, -77.66611478937542756 ) ) ;
#13806 = CARTESIAN_POINT ( 'NONE',  ( -78.66644367742111399, -170.0000000000000000, 57.26275173013680586 ) ) ;
#13807 = CYLINDRICAL_SURFACE ( 'NONE', #45813, 5.000000000000004441 ) ;
#13808 = CARTESIAN_POINT ( 'NONE',  ( -188.6739852773920063, 108.2139733222100375, -16.97215699203637129 ) ) ;
#13809 = CARTESIAN_POINT ( 'NONE',  ( 127.6144785300460711, 37.78099129859916161, 6.000583388021733633 ) ) ;
#13810 = DIRECTION ( 'NONE',  ( 0.000000000000000000, -1.000000000000000000, 0.000000000000000000 ) ) ;
#13811 = ADVANCED_FACE ( 'NONE', ( #665 ), #37595, .F. ) ;
#13812 = CARTESIAN_POINT ( 'NONE',  ( 212.1393014306632381, 118.9967099399321881, 89.43627726685924983 ) ) ;
#13813 = LINE ( 'NONE', #52143, #673 ) ;
#13814 = PLANE ( 'NONE',  #39888 ) ;
#13815 = CARTESIAN_POINT ( 'NONE',  ( -8.314575874103544706, 6.922894809783090686, 30.11558103944717857 ) ) ;
#13816 = ORIENTED_EDGE ( 'NONE', *, *, #38377, .F. ) ;
#13817 = AXIS2_PLACEMENT_3D ( 'NONE', #55099, #1647, #38230 ) ;
#13818 = CARTESIAN_POINT ( 'NONE',  ( 8.683910719548897816, 7.383368463746303512, -18.59074450809671930 ) ) ;
#13819 = ORIENTED_EDGE ( 'NONE', *, *, #42060, .F. ) ;
#13820 = ADVANCED_FACE ( 'NONE', ( #1013 ), #22114, .T. ) ;
#13821 = CARTESIAN_POINT ( 'NONE',  ( -102.2801239173131194, -170.0000000000000000, -42.51457726497592660 ) ) ;
#13822 = ORIENTED_EDGE ( 'NONE', *, *, #50107, .T. ) ;
#13823 = EDGE_CURVE ( 'NONE', #41104, #30932, #38646, .T. ) ;
#13824 = DIRECTION ( 'NONE',  ( 0.000000000000000000, 0.000000000000000000, 1.000000000000000000 ) ) ;
#13825 = AXIS2_PLACEMENT_3D ( 'NONE', #28893, #55259, #54196 ) ;
#13826 = DIRECTION ( 'NONE',  ( -0.000000000000000000, -0.000000000000000000, -1.000000000000000000 ) ) ;
#13827 = CARTESIAN_POINT ( 'NONE',  ( -36.19950032668960205, 11.44450118435070429, 85.60097597857388507 ) ) ;
#13828 = CARTESIAN_POINT ( 'NONE',  ( 157.4703587214989398, -170.0000000000000000, -89.81328548006499091 ) ) ;
#13829 = CARTESIAN_POINT ( 'NONE',  ( 37.46254810722764717, 8.164772623042706456, -50.38115373914292405 ) ) ;
#13830 = AXIS2_PLACEMENT_3D ( 'NONE', #48385, #55427, #44883 ) ;
#13831 = DIRECTION ( 'NONE',  ( 0.000000000000000000, 0.000000000000000000, 1.000000000000000000 ) ) ;
#13832 = PLANE ( 'NONE',  #4509 ) ;
#13833 = CARTESIAN_POINT ( 'NONE',  ( 44.99999999999995737, 25.00000000000000000, 1.999999999999984457 ) ) ;
#13834 = ORIENTED_EDGE ( 'NONE', *, *, #6424, .F. ) ;
#13835 = ORIENTED_EDGE ( 'NONE', *, *, #36362, .T. ) ;
#13836 = VECTOR ( 'NONE', #48250, 1000.000000000000114 ) ;
#13837 = CARTESIAN_POINT ( 'NONE',  ( 185.8199718667679861, 85.00425737502088452, 84.67356966130316209 ) ) ;
#13838 = DIRECTION ( 'NONE',  ( 1.000000000000000000, 0.000000000000000000, 0.000000000000000000 ) ) ;
#13839 = CARTESIAN_POINT ( 'NONE',  ( 133.8566784816069344, -170.0000000000000000, -51.02331093239568816 ) ) ;
#13840 = CARTESIAN_POINT ( 'NONE',  ( -25.35398647985413945, 8.671412257862213480, -74.05290484057726985 ) ) ;
#13841 = VECTOR ( 'NONE', #37518, 1000.000000000000000 ) ;
#13842 = DIRECTION ( 'NONE',  ( 0.7071067811865475727, 5.551115123125781470E-17, -0.7071067811865474617 ) ) ;
#13843 = VERTEX_POINT ( 'NONE', #16143 ) ;
#13844 = CARTESIAN_POINT ( 'NONE',  ( 209.3223706822284100, 0.000000000000000000, 31.44247402469554942 ) ) ;
#13845 = CARTESIAN_POINT ( 'NONE',  ( -56.72676045871359207, 16.18052435693491375, -76.87568460535000270 ) ) ;
#13846 = CARTESIAN_POINT ( 'NONE',  ( 178.1999009735082211, 75.73911533785327777, -63.64278916692260424 ) ) ;
#13847 = CARTESIAN_POINT ( 'NONE',  ( -177.1100086896682910, 168.8027595498802214, 281.0165308706135647 ) ) ;
#13848 = CARTESIAN_POINT ( 'NONE',  ( 278.3885044869534227, -21.48423713950020897, 4.736025848076669931 ) ) ;
#13849 = DIRECTION ( 'NONE',  ( -0.000000000000000000, -0.000000000000000000, 1.000000000000000000 ) ) ;
#13850 = CARTESIAN_POINT ( 'NONE',  ( -23.93933407965395688, 9.495050561681670942, 65.05660416612819574 ) ) ;
#13851 = CARTESIAN_POINT ( 'NONE',  ( -64.83840629396345889, -4.580509716060184644, 40.00000000000003553 ) ) ;
#13852 = ADVANCED_FACE ( 'NONE', ( #59046 ), #32335, .T. ) ;
#13853 = CARTESIAN_POINT ( 'NONE',  ( -15.55634918610403439, 2.818925648462311528E-14, 2.000000000000001776 ) ) ;
#13854 = CARTESIAN_POINT ( 'NONE',  ( -4.513903087372272971, 6.697902023160579255, 57.72633437538576118 ) ) ;
#13855 = ORIENTED_EDGE ( 'NONE', *, *, #9200, .T. ) ;
#13856 = CARTESIAN_POINT ( 'NONE',  ( 209.3223706822284100, 18.00000000000002842, 31.44247402469554942 ) ) ;
#13857 = CARTESIAN_POINT ( 'NONE',  ( 157.0357419681844533, 58.58786672900118475, 56.26341910979446936 ) ) ;
#13858 = CARTESIAN_POINT ( 'NONE',  ( -108.6944271866238978, 37.30738480893075604, -65.44042506789568847 ) ) ;
#13859 = CARTESIAN_POINT ( 'NONE',  ( -5.000000000000000000, 0.000000000000000000, 0.000000000000000000 ) ) ;
#13860 = FACE_OUTER_BOUND ( 'NONE', #31882, .T. ) ;
#13861 = LINE ( 'NONE', #35323, #60317 ) ;
#13862 = ORIENTED_EDGE ( 'NONE', *, *, #36875, .T. ) ;
#13863 = DIRECTION ( 'NONE',  ( 0.000000000000000000, 0.000000000000000000, -1.000000000000000000 ) ) ;
#13864 = ORIENTED_EDGE ( 'NONE', *, *, #18055, .F. ) ;
#13865 = EDGE_LOOP ( 'NONE', ( #57816, #11038, #18027, #22306 ) ) ;
#13866 = MECHANICAL_DESIGN_GEOMETRIC_PRESENTATION_REPRESENTATION (  '', ( #34118 ), #8253 ) ;
#13867 = CARTESIAN_POINT ( 'NONE',  ( 180.6710448012268841, 78.18844465372403363, -51.22505766587963905 ) ) ;
#13868 = CARTESIAN_POINT ( 'NONE',  ( 150.2941978382489481, 53.52137138947628614, 34.71248029558645953 ) ) ;
#13869 = DIRECTION ( 'NONE',  ( -0.000000000000000000, 1.000000000000000000, -0.000000000000000000 ) ) ;
#13870 = ORIENTED_EDGE ( 'NONE', *, *, #2613, .T. ) ;
#13871 = CARTESIAN_POINT ( 'NONE',  ( 151.3976820382521851, 54.32583990172415156, 94.99999999999866418 ) ) ;
#13872 = CARTESIAN_POINT ( 'NONE',  ( -180.6213815675304488, 95.88446356933840775, 11.16758809461633462 ) ) ;
#13873 = DIRECTION ( 'NONE',  ( -0.04486483035050447404, -0.9989930665413151445, 0.000000000000000000 ) ) ;
#13874 = DIRECTION ( 'NONE',  ( 0.8584487936018655452, 0.5128992774059070170, 0.000000000000000000 ) ) ;
#13875 = CARTESIAN_POINT ( 'NONE',  ( -83.15209219203883606, 25.16621997697722435, 43.94856979754528226 ) ) ;
#13876 = CARTESIAN_POINT ( 'NONE',  ( -24.60892750534350171, 9.584951112520229799, -19.08067319542340812 ) ) ;
#13877 = PRODUCT_DEFINITION ( 'UNKNOWN', '', #14187, #37353 ) ;
#13878 = CARTESIAN_POINT ( 'NONE',  ( -15.47041015649555185, -73.39774458108232125, 170.0000000000000000 ) ) ;
#13880 = ADVANCED_FACE ( 'NONE', ( #304 ), #59395, .T. ) ;
#13879 = VECTOR ( 'NONE', #44061, 1000.000000000000000 ) ;
#13881 = EDGE_CURVE ( 'NONE', #4944, #25496, #66247, .T. ) ;
#13882 = ORIENTED_EDGE ( 'NONE', *, *, #57267, .T. ) ;
#13883 = VECTOR ( 'NONE', #45085, 999.9999999999998863 ) ;
#13884 = LINE ( 'NONE', #51183, #35679 ) ;
#13885 = EDGE_CURVE ( 'NONE', #64675, #48379, #23173, .T. ) ;
#13886 = VECTOR ( 'NONE', #11961, 1000.000000000000114 ) ;
#13887 = DIRECTION ( 'NONE',  ( 0.6234898018587318180, 0.7818314824680311359, 0.000000000000000000 ) ) ;
#13888 = LINE ( 'NONE', #8275, #7973 ) ;
#13889 = DIRECTION ( 'NONE',  ( -0.000000000000000000, 0.000000000000000000, -1.000000000000000000 ) ) ;
#13891 = EDGE_LOOP ( 'NONE', ( #69246, #28459, #17873, #46797 ) ) ;
#13890 = CARTESIAN_POINT ( 'NONE',  ( -15.55634918610405748, -10.55634918610400597, 85.00100000000000477 ) ) ;
#13892 = CARTESIAN_POINT ( 'NONE',  ( 79.22946426532584496, 17.02750615740070828, -44.56886393397318358 ) ) ;
#13893 = ORIENTED_EDGE ( 'NONE', *, *, #40169, .F. ) ;
#13894 = AXIS2_PLACEMENT_3D ( 'NONE', #1733, #54118, #27055 ) ;
#13895 = ORIENTED_EDGE ( 'NONE', *, *, #17565, .T. ) ;
#13896 = LINE ( 'NONE', #45210, #25641 ) ;
#13897 = CARTESIAN_POINT ( 'NONE',  ( 79.33384730094452664, 18.11203072455028007, 35.45442786235279442 ) ) ;
#13898 = DIRECTION ( 'NONE',  ( 1.000000000000000000, 0.000000000000000000, 0.000000000000000000 ) ) ;
#13899 = CARTESIAN_POINT ( 'NONE',  ( -137.3060924980642596, 138.4631249211268482, 10.00000000000000000 ) ) ;
#13900 = CARTESIAN_POINT ( 'NONE',  ( -122.3745688183166180, 44.21964839958059912, 71.60445237168489996 ) ) ;
#13901 = CARTESIAN_POINT ( 'NONE',  ( -82.32006615997345023, 24.83050031643764655, -22.33869602845198798 ) ) ;
#13902 = CARTESIAN_POINT ( 'NONE',  ( -177.5288247523078837, 93.72924674643516596, -9.281560969338585210 ) ) ;
#13903 = CARTESIAN_POINT ( 'NONE',  ( 39.77028211725738771, 51.87520073220943573, 3.125053320693569132E-16 ) ) ;
#13904 = ORIENTED_EDGE ( 'NONE', *, *, #65793, .F. ) ;
#13906 = EDGE_CURVE ( 'NONE', #31701, #59178, #51295, .T. ) ;
#13905 =( REPRESENTATION_RELATIONSHIP ('NONE','NONE', #40274, #22184 ) REPRESENTATION_RELATIONSHIP_WITH_TRANSFORMATION ( #31723 )SHAPE_REPRESENTATION_RELATIONSHIP( ) );
#13907 = ORIENTED_EDGE ( 'NONE', *, *, #50211, .T. ) ;
#13908 = ADVANCED_FACE ( 'NONE', ( #29138 ), #29479, .T. ) ;
#13909 = DIRECTION ( 'NONE',  ( -1.000000000000000000, 0.000000000000000000, 0.000000000000000000 ) ) ;
#13910 = DIRECTION ( 'NONE',  ( -0.000000000000000000, 1.000000000000000000, -0.000000000000000000 ) ) ;
#13911 = CARTESIAN_POINT ( 'NONE',  ( 160.9069879467680551, 60.37290772564307417, 57.07157262504325956 ) ) ;
#13912 = CARTESIAN_POINT ( 'NONE',  ( -189.7334103489409927, 107.7745063523401399, 62.57085666808671931 ) ) ;
#13913 = PLANE ( 'NONE',  #57 ) ;
#13914 = CARTESIAN_POINT ( 'NONE',  ( 18.66025561752211104, 6.609375019058817635, 30.57350750057610256 ) ) ;
#13915 = CARTESIAN_POINT ( 'NONE',  ( 164.9697211531229755, 63.72502658717164792, -70.76554158249184923 ) ) ;
#13916 = ORIENTED_EDGE ( 'NONE', *, *, #43957, .F. ) ;
#13917 = ORIENTED_EDGE ( 'NONE', *, *, #56299, .F. ) ;
#13918 = EDGE_LOOP ( 'NONE', ( #29003, #10892, #68043, #19610 ) ) ;
#13919 = CIRCLE ( 'NONE', #29629, 2.999999999999999112 ) ;
#13920 = CARTESIAN_POINT ( 'NONE',  ( -73.37368996857509273, 20.37564829273156164, 86.28413825297953110 ) ) ;
#13921 = CARTESIAN_POINT ( 'NONE',  ( -81.01337222286377937, 23.22902179892323460, 57.62334405355243661 ) ) ;
#13922 = CARTESIAN_POINT ( 'NONE',  ( 67.93926590385567010, 13.86859831467923421, -37.54205066259513046 ) ) ;
#13923 = CARTESIAN_POINT ( 'NONE',  ( -75.31295361348102801, 9.223176757708264319E-15, 2.500000000000030198 ) ) ;
#13924 = CARTESIAN_POINT ( 'NONE',  ( -61.10880364359508832, 17.43879918625642489, 33.38610393800483678 ) ) ;
#13925 = AXIS2_PLACEMENT_3D ( 'NONE', #67663, #3627, #68681 ) ;
#13926 = CARTESIAN_POINT ( 'NONE',  ( -32.41898580403140784, 10.77423026598438227, -62.20981738725323140 ) ) ;
#13927 = AXIS2_PLACEMENT_3D ( 'NONE', #54921, #65496, #7456 ) ;
#13928 = CARTESIAN_POINT ( 'NONE',  ( 55.57634120535662703, 12.09544293553732608, 38.29713233239909442 ) ) ;
#13929 = CARTESIAN_POINT ( 'NONE',  ( 35.91764385665408099, 7.981776510761975807, 84.45325133309545151 ) ) ;
#13930 =( NAMED_UNIT ( * ) PLANE_ANGLE_UNIT ( ) SI_UNIT ( $, .RADIAN. ) );
#13931 = ORIENTED_EDGE ( 'NONE', *, *, #3986, .F. ) ;
#13932 = DIRECTION ( 'NONE',  ( 0.000000000000000000, 0.000000000000000000, 1.000000000000000000 ) ) ;
#13933 = FACE_OUTER_BOUND ( 'NONE', #11688, .T. ) ;
#13934 = CARTESIAN_POINT ( 'NONE',  ( -118.9649285217355725, 42.09781191014328527, 8.393151206171708623 ) ) ;
#13935 = LINE ( 'NONE', #36782, #34286 ) ;
#13936 = CIRCLE ( 'NONE', #50995, 74.95140232871122521 ) ;
#13937 = CARTESIAN_POINT ( 'NONE',  ( 18.20314211955701467, 7.596739727129572017, -23.29199594580876820 ) ) ;
#13938 = CARTESIAN_POINT ( 'NONE',  ( -7.329206686002009974E-14, -46.66904755831211560, 0.000000000000000000 ) ) ;
#13939 = AXIS2_PLACEMENT_3D ( 'NONE', #16626, #59877, #60588 ) ;
#13940 = VECTOR ( 'NONE', #19667, 1000.000000000000000 ) ;
#13941 = ORIENTED_EDGE ( 'NONE', *, *, #5483, .F. ) ;
#13942 = B_SPLINE_CURVE_WITH_KNOTS ( 'NONE', 3,
 ( #55476, #22775, #44926, #50554, #28397, #66753, #39311, #44218, #55838, #50207, #60755, #12576, #13278, #2033, #33345, #34036, #65344, #2372, #55123, #23487 ),
 .UNSPECIFIED., .F., .F.,
 ( 4, 2, 2, 2, 2, 2, 2, 2, 2, 4 ),
 ( 0.01088281063028401045, 0.01226892151836797562, 0.01365503240645193905, 0.01504114329453590422, 0.01642725418261986939, 0.01781336507070383282, 0.01919947595878779972, 0.02058558684687176316, 0.02127864229091375528, 0.02197169773495574741 ),
 .UNSPECIFIED. ) ;
#13944 = VECTOR ( 'NONE', #32785, 1000.000000000000000 ) ;
#13943 = SHAPE_DEFINITION_REPRESENTATION ( #42230, #45625 ) ;
#13945 = DIRECTION ( 'NONE',  ( -0.9009688679024218105, 0.4338837391175525693, 0.000000000000000000 ) ) ;
#13946 = CARTESIAN_POINT ( 'NONE',  ( -36.37229078872274357, 11.47648211215765812, -48.48744179093426965 ) ) ;
#13947 = DIRECTION ( 'NONE',  ( -0.000000000000000000, -1.000000000000000000, -0.000000000000000000 ) ) ;
#13948 = DIRECTION ( 'NONE',  ( 4.463998536185623432E-17, -2.459865942542999442E-16, 1.000000000000000000 ) ) ;
#13949 = ORIENTED_EDGE ( 'NONE', *, *, #32634, .F. ) ;
#13950 = VERTEX_POINT ( 'NONE', #12265 ) ;
#13951 = ADVANCED_BREP_SHAPE_REPRESENTATION ( '', ( #64527, #66832 ), #47807 ) ;
#13952 = CARTESIAN_POINT ( 'NONE',  ( -29.51060362117876323, 9.282716514427253429, -23.22459071689376486 ) ) ;
#13953 = CARTESIAN_POINT ( 'NONE',  ( -125.8938041572051389, 47.69968343338780414, -61.75825448869760237 ) ) ;
#13954 = ORIENTED_EDGE ( 'NONE', *, *, #49945, .T. ) ;
#13955 = CARTESIAN_POINT ( 'NONE',  ( 164.7561380852247055, 64.86195321300263572, 92.41705344553244572 ) ) ;
#13956 = ORIENTED_EDGE ( 'NONE', *, *, #22879, .T. ) ;
#13957 = CARTESIAN_POINT ( 'NONE',  ( 126.6464677212869248, 38.39096133771044350, -72.49914021808577047 ) ) ;
#13958 = CARTESIAN_POINT ( 'NONE',  ( 132.9485794245231318, 40.87843215479636427, 44.46890670783304955 ) ) ;
#13959 = CARTESIAN_POINT ( 'NONE',  ( -18.24318075359480318, 17.27206262134385284, 3.061616997868437868E-16 ) ) ;
#13961 = EDGE_CURVE ( 'NONE', #18376, #21875, #28435, .T. ) ;
#13960 = FACE_OUTER_BOUND ( 'NONE', #51892, .T. ) ;
#13962 = CARTESIAN_POINT ( 'NONE',  ( -2.374459999240554620, 25.00999262126967437, 3.061616997868437868E-16 ) ) ;
#13964 = ORIENTED_EDGE ( 'NONE', *, *, #48199, .T. ) ;
#13963 = LINE ( 'NONE', #8353, #1630 ) ;
#13965 = CARTESIAN_POINT ( 'NONE',  ( 56.66775172211441003, 11.28938863449062779, 41.31488029608967594 ) ) ;
#13966 = EDGE_CURVE ( 'NONE', #62805, #65715, #40039, .T. ) ;
#13967 = ORIENTED_EDGE ( 'NONE', *, *, #63163, .T. ) ;
#13968 = VERTEX_POINT ( 'NONE', #60789 ) ;
#13969 = CARTESIAN_POINT ( 'NONE',  ( -165.6215009671261100, 80.58889799860440917, 11.79125241431325399 ) ) ;
#13970 = VECTOR ( 'NONE', #41325, 1000.000000000000000 ) ;
#13971 = ADVANCED_FACE ( 'NONE', ( #8383 ), #56208, .T. ) ;
#13972 = CARTESIAN_POINT ( 'NONE',  ( -32.50312470669472731, 10.78887528550998276, -89.07914025037321437 ) ) ;
#13973 = AXIS2_PLACEMENT_3D ( 'NONE', #65322, #11149, #33325 ) ;
#13975 = VERTEX_POINT ( 'NONE', #61498 ) ;
#13974 = CARTESIAN_POINT ( 'NONE',  ( -132.0870433264402948, 51.94057326482882786, 69.20208566340080836 ) ) ;
#13976 = CARTESIAN_POINT ( 'NONE',  ( -5.066666666666671759, 8.000000000000000000, -11.86666666666666536 ) ) ;
#13977 = EDGE_CURVE ( 'NONE', #25778, #55030, #12612, .T. ) ;
#13978 = CARTESIAN_POINT ( 'NONE',  ( -73.10086105983762650, 21.34631349770503306, -37.56410186751649860 ) ) ;
#13979 = AXIS2_PLACEMENT_3D ( 'NONE', #5608, #47479, #52756 ) ;
#13980 = ORIENTED_EDGE ( 'NONE', *, *, #51176, .F. ) ;
#13981 = CARTESIAN_POINT ( 'NONE',  ( 15.68296563925494702, 63.09411298019766434, 170.0000000000000000 ) ) ;
#13982 = VECTOR ( 'NONE', #42213, 1000.000000000000000 ) ;
#13983 = VECTOR ( 'NONE', #1379, 1000.000000000000000 ) ;
#13984 = CARTESIAN_POINT ( 'NONE',  ( -173.1211646369891355, -170.0000000000000000, 11.47714401617735902 ) ) ;
#13985 = LINE ( 'NONE', #35443, #67376 ) ;
#13986 = VECTOR ( 'NONE', #6693, 1000.000000000000000 ) ;
#13987 = FACE_OUTER_BOUND ( 'NONE', #47331, .T. ) ;
#13988 = CARTESIAN_POINT ( 'NONE',  ( 67.55199883153193241, 14.80832170058781472, -76.05753081593569220 ) ) ;
#13989 = EDGE_CURVE ( 'NONE', #55679, #49789, #56284, .T. ) ;
#13990 = ORIENTED_EDGE ( 'NONE', *, *, #27366, .T. ) ;
#13991 = ORIENTED_EDGE ( 'NONE', *, *, #25374, .F. ) ;
#13992 = CARTESIAN_POINT ( 'NONE',  ( -143.8634661037141029, 60.82480701605699380, -20.43370834467151198 ) ) ;
#13993 = LINE ( 'NONE', #56911, #43533 ) ;
#13994 = DIRECTION ( 'NONE',  ( 0.000000000000000000, 1.000000000000000000, -0.000000000000000000 ) ) ;
#13995 = CARTESIAN_POINT ( 'NONE',  ( -54.62534944479597954, 14.56729055894799529, -88.91457369577481984 ) ) ;
#13996 = CARTESIAN_POINT ( 'NONE',  ( 26.11269837220803325, -10.55634918610409656, 0.000000000000000000 ) ) ;
#13997 = CARTESIAN_POINT ( 'NONE',  ( 100.0000000000000284, 0.000000000000000000, 0.000000000000000000 ) ) ;
#13998 = CARTESIAN_POINT ( 'NONE',  ( 0.4969600502617471105, 4.995646404165273502, -7.347286611336972584 ) ) ;
#13999 = DIRECTION ( 'NONE',  ( 0.000000000000000000, 0.000000000000000000, -1.000000000000000000 ) ) ;
#14000 = CARTESIAN_POINT ( 'NONE',  ( -166.5704851812740799, 80.12110537694672985, -72.71914147894192126 ) ) ;
#14001 = ORIENTED_EDGE ( 'NONE', *, *, #63614, .T. ) ;
#14002 = LINE ( 'NONE', #35106, #51257 ) ;
#14003 = VERTEX_POINT ( 'NONE', #63226 ) ;
#14004 = LINE ( 'NONE', #25264, #36379 ) ;
#14005 = CARTESIAN_POINT ( 'NONE',  ( 80.73462811483979351, 18.54763808182591944, 59.39265946625696557 ) ) ;
#14006 = ORIENTED_EDGE ( 'NONE', *, *, #50811, .F. ) ;
#14007 = FACE_OUTER_BOUND ( 'NONE', #11255, .T. ) ;
#14008 = CARTESIAN_POINT ( 'NONE',  ( -52.73319225379862019, -53.34578647582125654, 170.0000000000000000 ) ) ;
#14009 = FACE_OUTER_BOUND ( 'NONE', #755, .T. ) ;
#14010 = DIRECTION ( 'NONE',  ( 0.4738686624729966379, 0.8805955318567391110, 0.000000000000000000 ) ) ;
#14011 = CARTESIAN_POINT ( 'NONE',  ( 31.95008798096002423, 7.556925044648910905, 11.55179525732833845 ) ) ;
#14012 = DIRECTION ( 'NONE',  ( 0.000000000000000000, 0.000000000000000000, 1.000000000000000000 ) ) ;
#14013 = CARTESIAN_POINT ( 'NONE',  ( -65.36598343705435354, 0.000000000000000000, 41.38025477438755928 ) ) ;
#14014 = VERTEX_POINT ( 'NONE', #14682 ) ;
#14015 = CARTESIAN_POINT ( 'NONE',  ( -149.5074843970971017, 65.50121172469319220, 45.72082123989907387 ) ) ;
#14016 = VERTEX_POINT ( 'NONE', #19976 ) ;
#14017 = LINE ( 'NONE', #67491, #47413 ) ;
#14018 = CARTESIAN_POINT ( 'NONE',  ( -59.57462349605614804, 16.98779896904798647, 58.65824683570725284 ) ) ;
#14019 = CARTESIAN_POINT ( 'NONE',  ( -29.51060362117876679, 9.282716514427262311, 3.619959873569910336 ) ) ;
#14020 = EDGE_LOOP ( 'NONE', ( #44092, #12820, #26767, #29878 ) ) ;
#14021 = LINE ( 'NONE', #28823, #23274 ) ;
#14022 = CARTESIAN_POINT ( 'NONE',  ( -13.78709718204648560, 7.352743657744184702, -74.33944143250060677 ) ) ;
#14023 = DIRECTION ( 'NONE',  ( 0.000000000000000000, 0.000000000000000000, -1.000000000000000000 ) ) ;
#14024 = CARTESIAN_POINT ( 'NONE',  ( -25.48237668717800375, 8.689083390666786144, 69.14452889623510146 ) ) ;
#14025 = AXIS2_PLACEMENT_3D ( 'NONE', #14933, #69434, #47969 ) ;
#14026 = EDGE_LOOP ( 'NONE', ( #13835, #11606, #62804, #16611 ) ) ;
#14027 = DIRECTION ( 'NONE',  ( -0.3965763696460822829, 0.8752426702110749357, 0.2769069361358097447 ) ) ;
#14028 = DIRECTION ( 'NONE',  ( -0.7071067811865475727, -2.220446049250312341E-16, 0.7071067811865474617 ) ) ;
#14029 = DIRECTION ( 'NONE',  ( -0.000000000000000000, -0.000000000000000000, 1.000000000000000000 ) ) ;
#14030 = ORIENTED_EDGE ( 'NONE', *, *, #49798, .F. ) ;
#14032 = CARTESIAN_POINT ( 'NONE',  ( -173.9617926765114362, 89.58633395456780590, -61.59193146985943201 ) ) ;
#14031 = VECTOR ( 'NONE', #18489, 1000.000000000000000 ) ;
#14033 = CIRCLE ( 'NONE', #38729, 5.000000000000004441 ) ;
#14034 = ADVANCED_FACE ( 'NONE', ( #10100 ), #36492, .T. ) ;
#14035 = FACE_OUTER_BOUND ( 'NONE', #64389, .T. ) ;
#14036 = AXIS2_PLACEMENT_3D ( 'NONE', #50870, #38944, #49464 ) ;
#14037 = CARTESIAN_POINT ( 'NONE',  ( 117.6865880453675999, 32.48051379280605033, 36.05596251868298907 ) ) ;
#14038 = VECTOR ( 'NONE', #9296, 1000.000000000000000 ) ;
#14039 = CARTESIAN_POINT ( 'NONE',  ( 89.74347354996881165, 20.50579948213362869, -90.14040706678140680 ) ) ;
#14040 = AXIS2_PLACEMENT_3D ( 'NONE', #50141, #60341, #29378 ) ;
#14041 = DIRECTION ( 'NONE',  ( 1.000000000000000000, 0.000000000000000000, 0.000000000000000000 ) ) ;
#14042 = ORIENTED_EDGE ( 'NONE', *, *, #43838, .F. ) ;
#14043 = CARTESIAN_POINT ( 'NONE',  ( 201.6034029841262338, 102.1956603101140928, 43.55317564153742182 ) ) ;
#14044 = CARTESIAN_POINT ( 'NONE',  ( 115.0692128464502701, 31.17922615202199310, -64.50543960138530508 ) ) ;
#14045 = CARTESIAN_POINT ( 'NONE',  ( 69.08240197259640070, 14.16210831900843203, 59.74101951860149740 ) ) ;
#14046 = CARTESIAN_POINT ( 'NONE',  ( 140.7888851157410102, 46.97220912571250295, 13.04025809958710624 ) ) ;
#14047 = CARTESIAN_POINT ( 'NONE',  ( -452.6627218934913799, 399.9999999999953957, 113.5502958579925803 ) ) ;
#14048 = ORIENTED_EDGE ( 'NONE', *, *, #50300, .F. ) ;
#14049 = CARTESIAN_POINT ( 'NONE',  ( 164.9706294237033717, 65.04392654036658428, -17.05375542338060413 ) ) ;
#14050 = EDGE_CURVE ( 'NONE', #28268, #27257, #59622, .T. ) ;
#14051 = ORIENTED_EDGE ( 'NONE', *, *, #61615, .T. ) ;
#14052 = DIRECTION ( 'NONE',  ( 1.000000000000000000, 0.000000000000000000, 0.000000000000000000 ) ) ;
#14053 = CARTESIAN_POINT ( 'NONE',  ( 130.0022568700022703, 39.14528604308903681, 84.25756070950254184 ) ) ;
#14055 = ORIENTED_EDGE ( 'NONE', *, *, #66030, .T. ) ;
#14054 = CARTESIAN_POINT ( 'NONE',  ( 40.13282190615316836, 1.842283050316774879E-12, -9.999999999999998224 ) ) ;
#14056 = CARTESIAN_POINT ( 'NONE',  ( -149.0732005398558613, 63.81212100765655748, -61.66682328262454860 ) ) ;
#14057 = EDGE_CURVE ( 'NONE', #40816, #25434, #41220, .T. ) ;
#14058 = CARTESIAN_POINT ( 'NONE',  ( -35.00000000000002842, -35.00000000000000000, 380.0000000000000000 ) ) ;
#14059 = CARTESIAN_POINT ( 'NONE',  ( 164.7250737226289630, 63.51898362052163804, -41.70171562401918663 ) ) ;
#14060 = VERTEX_POINT ( 'NONE', #225 ) ;
#14061 = CARTESIAN_POINT ( 'NONE',  ( -3.364862276288897558, 74.92447999059858432, 0.000000000000000000 ) ) ;
#14062 = CARTESIAN_POINT ( 'NONE',  ( 56.33018609834994095, 12.24748093153179518, 94.41788745877084921 ) ) ;
#14063 = FACE_OUTER_BOUND ( 'NONE', #36751, .T. ) ;
#14064 = CIRCLE ( 'NONE', #8450, 91.99999999999997158 ) ;
#14065 = CARTESIAN_POINT ( 'NONE',  ( 86.14890207173843351, 20.31981596387580424, -8.977013608448027426 ) ) ;
#14066 = DIRECTION ( 'NONE',  ( -1.000000000000000000, 0.000000000000000000, 0.000000000000000000 ) ) ;
#14067 = DIRECTION ( 'NONE',  ( 0.000000000000000000, 0.000000000000000000, 1.000000000000000000 ) ) ;
#14068 = CARTESIAN_POINT ( 'NONE',  ( 181.0840389613909736, 80.03940679743415387, 44.30859410551141764 ) ) ;
#14069 = ADVANCED_FACE ( 'NONE', ( #21338 ), #48744, .T. ) ;
#14070 = EDGE_LOOP ( 'NONE', ( #29464, #33859, #68811, #12520 ) ) ;
#14071 = CARTESIAN_POINT ( 'NONE',  ( -97.86516199987804043, 31.71158167298307617, 58.78184745139680700 ) ) ;
#14072 = DIRECTION ( 'NONE',  ( -0.000000000000000000, 1.000000000000000000, -0.000000000000000000 ) ) ;
#14073 = EDGE_LOOP ( 'NONE', ( #54119, #66193, #13895, #11051 ) ) ;
#14074 = VECTOR ( 'NONE', #20124, 1000.000000000000000 ) ;
#14075 = EDGE_CURVE ( 'NONE', #50425, #20755, #16062, .T. ) ;
#14076 = EDGE_CURVE ( 'NONE', #43093, #19218, #48063, .T. ) ;
#14077 = CARTESIAN_POINT ( 'NONE',  ( 150.5538013146980347, 53.70974888488127164, -13.86729835050963899 ) ) ;
#14078 = DIRECTION ( 'NONE',  ( 1.387778780781445922E-16, -1.000000000000000000, -3.469446951953615421E-17 ) ) ;
#14079 = CIRCLE ( 'NONE', #11860, 65.00000000000000000 ) ;
#14080 = CONICAL_SURFACE ( 'NONE', #62385, 8.000000000000001776, 1.047197551196595855 ) ;
#14081 = CARTESIAN_POINT ( 'NONE',  ( 102.7414208686707724, 26.65627265923299660, 37.60061438686749113 ) ) ;
#14082 = CARTESIAN_POINT ( 'NONE',  ( -4.506365319453810692, 7.705038994660847074, 30.88546273271729348 ) ) ;
#14083 = CARTESIAN_POINT ( 'NONE',  ( 55.82071269177104256, 11.11819622756448034, 88.85841515383880562 ) ) ;
#14084 = CARTESIAN_POINT ( 'NONE',  ( -50.14771795543004629, 13.42081263859818385, -75.25552575325329485 ) ) ;
#14085 = CARTESIAN_POINT ( 'NONE',  ( 0.000000000000000000, 0.000000000000000000, 40.00000000000003553 ) ) ;
#14086 = AXIS2_PLACEMENT_3D ( 'NONE', #58182, #48630, #21241 ) ;
#14087 = FACE_OUTER_BOUND ( 'NONE', #3242, .T. ) ;
#14088 = CARTESIAN_POINT ( 'NONE',  ( -62.15324028806259093, 16.70091357159900980, 13.43818584318690057 ) ) ;
#14089 = ORIENTED_EDGE ( 'NONE', *, *, #68529, .T. ) ;
#14090 = LINE ( 'NONE', #52413, #14981 ) ;
#14091 = ORIENTED_EDGE ( 'NONE', *, *, #12365, .T. ) ;
#14092 = CARTESIAN_POINT ( 'NONE',  ( 102.8518012651273779, 25.61025413220827929, -68.96863170923236908 ) ) ;
#14093 = DIRECTION ( 'NONE',  ( 0.000000000000000000, 0.000000000000000000, -1.000000000000000000 ) ) ;
#14094 = CARTESIAN_POINT ( 'NONE',  ( 42.49453823366106064, 8.831814337191476127, 71.09543012908832793 ) ) ;
#14095 = LINE ( 'NONE', #46096, #55862 ) ;
#14096 = CARTESIAN_POINT ( 'NONE',  ( -8.157890479254499283, 6.912699202480759197, 83.80498378616138666 ) ) ;
#14097 = CARTESIAN_POINT ( 'NONE',  ( -107.7886332494339712, 36.81249801143974310, -10.55694427585111050 ) ) ;
#14098 = VERTEX_POINT ( 'NONE', #26282 ) ;
#14099 = CARTESIAN_POINT ( 'NONE',  ( 429.8372781065087338, 395.0000000000001137, -123.9497041420121235 ) ) ;
#14100 = DIRECTION ( 'NONE',  ( -0.6246950475544236214, 7.650307904307285654E-17, 0.7808688094430308313 ) ) ;
#14101 = EDGE_LOOP ( 'NONE', ( #13131, #46819 ) ) ;
#14102 = VERTEX_POINT ( 'NONE', #37172 ) ;
#14103 = CARTESIAN_POINT ( 'NONE',  ( -155.7433525314458791, 69.65452735858369238, 42.39591026950624553 ) ) ;
#14104 = CARTESIAN_POINT ( 'NONE',  ( 55.65793654284683356, -50.28674377798225237, 170.0000000000000000 ) ) ;
#14105 = CARTESIAN_POINT ( 'NONE',  ( 179.0096185093688064, 76.53352131383245194, -24.10098174011748640 ) ) ;
#14106 = CARTESIAN_POINT ( 'NONE',  ( 107.0555969502564153, 28.53646637607231540, 57.15036769607191758 ) ) ;
#14107 = CARTESIAN_POINT ( 'NONE',  ( 0.000000000000000000, 0.000000000000000000, 25.70156211871649887 ) ) ;
#14108 = CARTESIAN_POINT ( 'NONE',  ( 55.51528220483959331, 12.08323518953685749, -16.13771739302386621 ) ) ;
#14109 = ORIENTED_EDGE ( 'NONE', *, *, #1761, .F. ) ;
#14110 = CARTESIAN_POINT ( 'NONE',  ( 107.2614272668149056, 28.62909081796205513, -36.53649460854888531 ) ) ;
#14111 = VERTEX_POINT ( 'NONE', #22034 ) ;
#14112 = CARTESIAN_POINT ( 'NONE',  ( 210.1633650091869470, 114.1507944623966893, 4.721410748252139911 ) ) ;
#14113 = CARTESIAN_POINT ( 'NONE',  ( 8.763528846667103522, 7.383598436776579454, 66.99810038742778318 ) ) ;
#14114 = CARTESIAN_POINT ( 'NONE',  ( 208.9507214515059843, 112.3605999017434982, 30.51409441703008696 ) ) ;
#14115 = EDGE_CURVE ( 'NONE', #35105, #67632, #27743, .T. ) ;
#14116 = FACE_BOUND ( 'NONE', #33499, .T. ) ;
#14117 = ADVANCED_FACE ( 'NONE', ( #33302 ), #38213, .F. ) ;
#14118 = VECTOR ( 'NONE', #61047, 1000.000000000000000 ) ;
#14119 = ORIENTED_EDGE ( 'NONE', *, *, #12232, .F. ) ;
#14120 = ORIENTED_EDGE ( 'NONE', *, *, #49118, .T. ) ;
#14121 = FACE_OUTER_BOUND ( 'NONE', #15384, .T. ) ;
#14122 = CARTESIAN_POINT ( 'NONE',  ( -123.1629650876958948, 45.91644518770717553, 84.79916741339407338 ) ) ;
#14123 = AXIS2_PLACEMENT_3D ( 'NONE', #30356, #24044, #61324 ) ;
#14124 = DIRECTION ( 'NONE',  ( 0.000000000000000000, 0.000000000000000000, 1.000000000000000000 ) ) ;
#14125 = DIRECTION ( 'NONE',  ( 1.000000000000000000, 0.000000000000000000, 0.000000000000000000 ) ) ;
#14126 = CARTESIAN_POINT ( 'NONE',  ( 8.970976835706142793, 6.378128542324178696, 88.06027136665343846 ) ) ;
#14127 = CARTESIAN_POINT ( 'NONE',  ( 79.22946426532585917, 17.02750615740070828, -71.41341452443687388 ) ) ;
#14128 = AXIS2_PLACEMENT_3D ( 'NONE', #62118, #62475, #46636 ) ;
#14129 = VECTOR ( 'NONE', #56423, 1000.000000000000000 ) ;
#14130 = VERTEX_POINT ( 'NONE', #42785 ) ;
#14132 = EDGE_CURVE ( 'NONE', #68707, #66593, #17090, .T. ) ;
#14131 = FACE_BOUND ( 'NONE', #22026, .T. ) ;
#14133 = VECTOR ( 'NONE', #118, 1000.000000000000000 ) ;
#14134 = CARTESIAN_POINT ( 'NONE',  ( 198.8732368717152212, 100.3103976497390732, -39.09420075645709858 ) ) ;
#14135 = ORIENTED_EDGE ( 'NONE', *, *, #37560, .T. ) ;
#14136 = EDGE_CURVE ( 'NONE', #49232, #40260, #32255, .T. ) ;
#14137 = FACE_BOUND ( 'NONE', #11954, .T. ) ;
#14138 = ORIENTED_EDGE ( 'NONE', *, *, #7943, .T. ) ;
#14139 = CARTESIAN_POINT ( 'NONE',  ( -85.75947274862029701, 25.15128705015480293, -71.94837500685306964 ) ) ;
#14140 = DIRECTION ( 'NONE',  ( -0.9639628606958550172, 0.2660368455666687892, 0.000000000000000000 ) ) ;
#14141 = EDGE_LOOP ( 'NONE', ( #60507, #29407 ) ) ;
#14142 = EDGE_CURVE ( 'NONE', #61903, #12845, #24711, .T. ) ;
#14143 = ORIENTED_EDGE ( 'NONE', *, *, #17060, .T. ) ;
#14144 = CARTESIAN_POINT ( 'NONE',  ( 46.89016064832839703, 10.52130577388959409, 63.77019485676617450 ) ) ;
#14145 = ADVANCED_FACE ( 'NONE', ( #22381 ), #16411, .F. ) ;
#14146 = LINE ( 'NONE', #57396, #10000 ) ;
#14147 = CARTESIAN_POINT ( 'NONE',  ( 102.7938674513919040, 26.67851209377772292, 11.27790700381929945 ) ) ;
#14148 = ORIENTED_EDGE ( 'NONE', *, *, #42769, .F. ) ;
#14149 = CARTESIAN_POINT ( 'NONE',  ( -28.92901790436172149, 9.192688694475796396, 84.33077190568265280 ) ) ;
#14150 = PLANE ( 'NONE',  #20788 ) ;
#14151 = CARTESIAN_POINT ( 'NONE',  ( 4.606779575614314837, -24.69646479044436305, 3.061616997868437868E-16 ) ) ;
#14152 = CARTESIAN_POINT ( 'NONE',  ( 109.3079614081140249, 28.45126415661782460, -35.96632621749219538 ) ) ;
#14153 = EDGE_CURVE ( 'NONE', #65974, #32844, #12687, .T. ) ;
#14154 = CARTESIAN_POINT ( 'NONE',  ( 163.5430354047457229, 62.53125887746119105, 94.99999999999866418 ) ) ;
#14155 = DIRECTION ( 'NONE',  ( 1.000000000000000000, 0.000000000000000000, 0.000000000000000000 ) ) ;
#14156 = ORIENTED_EDGE ( 'NONE', *, *, #46473, .F. ) ;
#14157 = ADVANCED_FACE ( 'NONE', ( #64603 ), #5846, .F. ) ;
#14158 = EDGE_CURVE ( 'NONE', #68142, #39369, #28716, .T. ) ;
#14159 = EDGE_CURVE ( 'NONE', #16864, #32664, #25286, .T. ) ;
#14160 = ORIENTED_EDGE ( 'NONE', *, *, #45668, .T. ) ;
#14161 = CARTESIAN_POINT ( 'NONE',  ( 43.35980717318837918, 8.957244490220908517, 16.94469360157332360 ) ) ;
#14162 = PLANE ( 'NONE',  #46178 ) ;
#14163 = DIRECTION ( 'NONE',  ( 0.000000000000000000, -0.000000000000000000, -1.000000000000000000 ) ) ;
#14164 = DIRECTION ( 'NONE',  ( -0.5508969814520944253, -0.8345732537213078617, 0.000000000000000000 ) ) ;
#14165 = CARTESIAN_POINT ( 'NONE',  ( 128.0848616812662897, 38.04676222636084049, 14.98112062868012906 ) ) ;
#14166 = CARTESIAN_POINT ( 'NONE',  ( -442.6627218934912662, 394.9999999999998295, 99.85872701201111568 ) ) ;
#14167 = DIRECTION ( 'NONE',  ( 0.7041338076821838099, -0.7100673072878298520, 0.000000000000000000 ) ) ;
#14168 = CARTESIAN_POINT ( 'NONE',  ( 212.1976655298228138, 119.0878071902807562, 36.52985908372631485 ) ) ;
#14169 = CARTESIAN_POINT ( 'NONE',  ( -74.79002408692173276, 20.88280597089421775, -63.03483985874790108 ) ) ;
#14170 = CARTESIAN_POINT ( 'NONE',  ( -108.6909373351217596, 36.15835109565443162, 34.09471970242879735 ) ) ;
#14171 = ORIENTED_EDGE ( 'NONE', *, *, #11040, .T. ) ;
#14172 = CIRCLE ( 'NONE', #7454, 24.99999999999985434 ) ;
#14173 = DIRECTION ( 'NONE',  ( 0.000000000000000000, 0.000000000000000000, 1.000000000000000000 ) ) ;
#14174 = VERTEX_POINT ( 'NONE', #17447 ) ;
#14175 = CARTESIAN_POINT ( 'NONE',  ( 197.1974290009105175, 96.59277840252782710, -17.30540446041513292 ) ) ;
#14176 = ORIENTED_EDGE ( 'NONE', *, *, #12144, .T. ) ;
#14177 = DIRECTION ( 'NONE',  ( 0.000000000000000000, -0.1086713087885527035, -0.9940777367219240102 ) ) ;
#14178 = VECTOR ( 'NONE', #27314, 1000.000000000000114 ) ;
#14179 = CARTESIAN_POINT ( 'NONE',  ( 186.2575601542430661, 85.47765906955508797, -65.13421257721934410 ) ) ;
#14180 = CARTESIAN_POINT ( 'NONE',  ( -143.8756912989387047, 60.83492035645719653, 70.02464342104502748 ) ) ;
#14181 = CARTESIAN_POINT ( 'NONE',  ( -96.76159256735191150, 30.06445763698411611, -37.41197554230570432 ) ) ;
#14182 = CIRCLE ( 'NONE', #38888, 65.36598343705435354 ) ;
#14183 = VECTOR ( 'NONE', #352, 1000.000000000000114 ) ;
#14184 = CARTESIAN_POINT ( 'NONE',  ( 37.47081272996200596, 8.166145978397521432, -35.86855199365803060 ) ) ;
#14185 = CARTESIAN_POINT ( 'NONE',  ( -105.8879439778144587, 34.65133284149109727, 4.582014221861286707 ) ) ;
#14186 = CARTESIAN_POINT ( 'NONE',  ( 86.62931800182293784, -170.0000000000000000, 10.36753698201563267 ) ) ;
#14187 = PRODUCT_DEFINITION_FORMATION_WITH_SPECIFIED_SOURCE ( 'ANY', '', #36615, .NOT_KNOWN. ) ;
#14188 = FACE_OUTER_BOUND ( 'NONE', #36364, .T. ) ;
#14189 = EDGE_LOOP ( 'NONE', ( #68269, #54237, #67546, #12368 ) ) ;
#14190 = ORIENTED_EDGE ( 'NONE', *, *, #62229, .F. ) ;
#14191 = AXIS2_PLACEMENT_3D ( 'NONE', #51102, #46154, #19081 ) ;
#14192 = B_SPLINE_CURVE_WITH_KNOTS ( 'NONE', 3,
 ( #62648, #14456, #52080, #25368 ),
 .UNSPECIFIED., .F., .F.,
 ( 4, 4 ),
 ( 0.1259919275528360583, 0.1829744153748752988 ),
 .UNSPECIFIED. ) ;
#14193 = CARTESIAN_POINT ( 'NONE',  ( 187.5460976208452735, 86.88588274757240981, 86.67476712161497687 ) ) ;
#14194 = AXIS2_PLACEMENT_3D ( 'NONE', #21011, #30879, #42456 ) ;
#14195 = CARTESIAN_POINT ( 'NONE',  ( -24.39249304643357519, -60.24953346690487166, 170.0000000000000000 ) ) ;
#14196 = CARTESIAN_POINT ( 'NONE',  ( -30.94753041835916108, 9.510749728915508072, -62.16174795566552547 ) ) ;
#14197 = UNCERTAINTY_MEASURE_WITH_UNIT (LENGTH_MEASURE( 1.000000000000000082E-05 ), #36592, 'distance_accuracy_value', 'NONE');
#14198 = PLANE ( 'NONE',  #21656 ) ;
#14199 = CARTESIAN_POINT ( 'NONE',  ( 281.6145892210130341, 21.48294702482179730, -4.743341903180106733 ) ) ;
#14200 = CARTESIAN_POINT ( 'NONE',  ( 34.76618902119740540, 54.93755186520760958, 43.58025477438756923 ) ) ;
#14201 = CARTESIAN_POINT ( 'NONE',  ( 173.9288990958749537, 71.66475105971930759, -68.24753224134477136 ) ) ;
#14202 = CARTESIAN_POINT ( 'NONE',  ( 275.1608565259479633, -21.96391085485757699, -1.300312621757654608 ) ) ;
#14203 = DIRECTION ( 'NONE',  ( -1.000000000000000000, 0.000000000000000000, 0.000000000000000000 ) ) ;
#14204 = CARTESIAN_POINT ( 'NONE',  ( -169.8791831685529701, 83.59058982490282119, 18.25486782800532382 ) ) ;
#14205 = CARTESIAN_POINT ( 'NONE',  ( 32.06997139192793611, -56.95813133885440038, 3.125053320693577513E-16 ) ) ;
#14206 = B_SPLINE_CURVE_WITH_KNOTS ( 'NONE', 3,
 ( #5951, #18874, #37977, #43930, #694, #16858, #65411, #38315, #59761, #11575, #33050, #54486, #6311, #17202, #25883, #58226, #41370, #30814, #57884, #4082, #63170, #24512, #19204, #63507, #62117, #62823, #30129, #19915, #62474, #9703, #51580, #31498, #56857, #14290, #14964, #40664, #35397, #8675, #68441, #31169, #36430, #36090, #67413, #20247, #3387, #67760 ),
 .UNSPECIFIED., .F., .F.,
 ( 4, 2, 2, 2, 2, 2, 2, 2, 2, 2, 2, 2, 2, 2, 2, 2, 2, 2, 2, 2, 2, 2, 4 ),
 ( 3.538155541877297313E-17, 0.001572224531395696864, 0.003144449062791358600, 0.004716673594187020119, 0.006288898125582681638, 0.007861122656978343157, 0.009433347188374003808, 0.01021945945407182199, 0.01100557171976964017, 0.01179168398546745836, 0.01257779625116527654, 0.01415002078256091464, 0.01493613304825873976, 0.01572224531395656488, 0.01650835757965439174, 0.01729446984535221513, 0.01886669437674783414, 0.01965280664244563671, 0.02043891890814343928, 0.02201114343953904443, 0.02358336797093465304, 0.02436948023663245907, 0.02515559250233026858 ),
 .UNSPECIFIED. ) ;
#14207 = CARTESIAN_POINT ( 'NONE',  ( -53.13004807512039207, 14.17398740785108302, 71.92754858008906638 ) ) ;
#14208 = EDGE_CURVE ( 'NONE', #47971, #67731, #33992, .T. ) ;
#14209 = CARTESIAN_POINT ( 'NONE',  ( -100.6125620134474019, 31.94146452012412141, -88.87928813972597197 ) ) ;
#14210 = VERTEX_POINT ( 'NONE', #6899 ) ;
#14211 = CARTESIAN_POINT ( 'NONE',  ( -29.87147652227455552, 100.0000000000000000, 133.5802547743875550 ) ) ;
#14212 = DIRECTION ( 'NONE',  ( 0.000000000000000000, 1.000000000000000000, 0.000000000000000000 ) ) ;
#14213 = CARTESIAN_POINT ( 'NONE',  ( -102.7494334820056565, 34.14986869751099618, -61.85912785543958137 ) ) ;
#14214 = DIRECTION ( 'NONE',  ( 0.000000000000000000, 1.000000000000000000, 0.000000000000000000 ) ) ;
#14215 = DIRECTION ( 'NONE',  ( 0.000000000000000000, 0.000000000000000000, 1.000000000000000000 ) ) ;
#14216 = DIRECTION ( 'NONE',  ( -0.9009688679024155933, -0.4338837391175656699, 0.000000000000000000 ) ) ;
#14217 = ORIENTED_EDGE ( 'NONE', *, *, #57690, .T. ) ;
#14219 = EDGE_CURVE ( 'NONE', #24929, #53581, #28355, .T. ) ;
#14218 = CARTESIAN_POINT ( 'NONE',  ( 0.000000000000000000, 0.000000000000000000, 0.000000000000000000 ) ) ;
#14220 = DIRECTION ( 'NONE',  ( -0.000000000000000000, -0.000000000000000000, -1.000000000000000000 ) ) ;
#14221 = ORIENTED_EDGE ( 'NONE', *, *, #63975, .T. ) ;
#14222 = AXIS2_PLACEMENT_3D ( 'NONE', #16141, #37593, #65029 ) ;
#14223 = ORIENTED_EDGE ( 'NONE', *, *, #42258, .T. ) ;
#14224 = CARTESIAN_POINT ( 'NONE',  ( 8.000000000000007105, 249.8719672152120381, 94.99999999999866418 ) ) ;
#14225 = CARTESIAN_POINT ( 'NONE',  ( 24.39800339187844003, 60.26242556095705538, 43.58025477438756923 ) ) ;
#14226 = EDGE_CURVE ( 'NONE', #6690, #3913, #50854, .T. ) ;
#14227 = DIRECTION ( 'NONE',  ( 0.000000000000000000, 1.000000000000000000, 0.000000000000000000 ) ) ;
#14228 = ORIENTED_EDGE ( 'NONE', *, *, #35915, .F. ) ;
#14229 = DIRECTION ( 'NONE',  ( -0.000000000000000000, 1.000000000000000000, -0.000000000000000000 ) ) ;
#14230 = EDGE_CURVE ( 'NONE', #56059, #46924, #17815, .T. ) ;
#14231 = VECTOR ( 'NONE', #40312, 1000.000000000000000 ) ;
#14232 = DIRECTION ( 'NONE',  ( 0.000000000000000000, 0.000000000000000000, 1.000000000000000000 ) ) ;
#14233 = CARTESIAN_POINT ( 'NONE',  ( -7.336760511143403996, 6.859209474528211281, 3.271030448983516248 ) ) ;
#14234 = CARTESIAN_POINT ( 'NONE',  ( -20.63749999999999929, 0.000000000000000000, 0.000000000000000000 ) ) ;
#14235 = CARTESIAN_POINT ( 'NONE',  ( 19.40210665709608406, -63.75862921693536833, 34.48241795236665297 ) ) ;
#14236 = VECTOR ( 'NONE', #29270, 1000.000000000000000 ) ;
#14237 = CARTESIAN_POINT ( 'NONE',  ( 151.9464045465396111, 53.48030587346669762, 85.51384040717854873 ) ) ;
#14238 = CARTESIAN_POINT ( 'NONE',  ( 139.1353280997809065, 44.70436000187870462, 15.49914358619959209 ) ) ;
#14239 = SURFACE_STYLE_FILL_AREA ( #43929 ) ;
#14240 = EDGE_LOOP ( 'NONE', ( #7824, #57240, #62325, #42880 ) ) ;
#14241 = DIRECTION ( 'NONE',  ( -0.000000000000000000, -0.000000000000000000, -1.000000000000000000 ) ) ;
#14242 = AXIS2_PLACEMENT_3D ( 'NONE', #32917, #64938, #16046 ) ;
#14243 = DIRECTION ( 'NONE',  ( 1.000000000000000000, 0.000000000000000000, 0.000000000000000000 ) ) ;
#14244 = DIRECTION ( 'NONE',  ( -1.000000000000000000, -0.000000000000000000, -0.000000000000000000 ) ) ;
#14245 = CARTESIAN_POINT ( 'NONE',  ( -125.0000000000000000, 1.530808498934191561E-14, 10.00000000000000000 ) ) ;
#14247 = ORIENTED_EDGE ( 'NONE', *, *, #40703, .F. ) ;
#14246 = CARTESIAN_POINT ( 'NONE',  ( -118.3982140490518020, 41.75260250602053702, 91.38396685080842019 ) ) ;
#14248 = LINE ( 'NONE', #9660, #66765 ) ;
#14249 = ORIENTED_EDGE ( 'NONE', *, *, #22782, .T. ) ;
#14250 = EDGE_CURVE ( 'NONE', #69029, #13412, #55079, .T. ) ;
#14251 = ORIENTED_EDGE ( 'NONE', *, *, #68387, .T. ) ;
#14252 = DIRECTION ( 'NONE',  ( 0.000000000000000000, 0.000000000000000000, 1.000000000000000000 ) ) ;
#14253 = PLANE ( 'NONE',  #16535 ) ;
#14254 = CARTESIAN_POINT ( 'NONE',  ( 199.7278513351970730, 99.76879341361772902, -65.03439541865878937 ) ) ;
#14255 = EDGE_CURVE ( 'NONE', #19842, #40675, #7260, .T. ) ;
#14256 = CARTESIAN_POINT ( 'NONE',  ( -31.43908319763709969, 10.61114334766716105, 45.21645440618919309 ) ) ;
#14257 = CARTESIAN_POINT ( 'NONE',  ( -118.4622862908118748, 41.79153065058245886, 66.01100761066821576 ) ) ;
#14258 = PLANE ( 'NONE',  #28801 ) ;
#14259 = CARTESIAN_POINT ( 'NONE',  ( 16.27765348919937338, 6.516472002017812848, -23.67439350822213129 ) ) ;
#14260 = CARTESIAN_POINT ( 'NONE',  ( 26.11269837220809364, 20.55634918610396866, 0.000000000000000000 ) ) ;
#14261 = ORIENTED_EDGE ( 'NONE', *, *, #50212, .T. ) ;
#14262 = ORIENTED_EDGE ( 'NONE', *, *, #52512, .F. ) ;
#14263 = CARTESIAN_POINT ( 'NONE',  ( -109.6752351740181695, 37.84903014964773860, 12.45126650322635165 ) ) ;
#14264 = CARTESIAN_POINT ( 'NONE',  ( 107.2672065034543181, 27.52931006625851396, 57.06728851299916272 ) ) ;
#14265 = CARTESIAN_POINT ( 'NONE',  ( 164.3702714028688376, 63.22112480708619131, 66.70566855636806736 ) ) ;
#14266 = CARTESIAN_POINT ( 'NONE',  ( -189.2826425734428426, 107.1493800926105848, 66.14067199168205491 ) ) ;
#14267 = DIRECTION ( 'NONE',  ( 1.387778780781445429E-16, -1.000000000000000000, -3.081487911019577365E-33 ) ) ;
#14268 = DIRECTION ( 'NONE',  ( -1.000000000000000000, 0.000000000000000000, 0.000000000000000000 ) ) ;
#14269 = CARTESIAN_POINT ( 'NONE',  ( -142.6736406357357794, 59.87555372585265445, 94.99999999999866418 ) ) ;
#14270 = ORIENTED_EDGE ( 'NONE', *, *, #52494, .F. ) ;
#14271 = PRODUCT_DEFINITION_SHAPE ( 'NONE', 'NONE',  #3950 ) ;
#14272 = EDGE_LOOP ( 'NONE', ( #39321, #60455 ) ) ;
#14273 = ORIENTED_EDGE ( 'NONE', *, *, #22782, .F. ) ;
#14274 = AXIS2_PLACEMENT_3D ( 'NONE', #26722, #27050, #42210 ) ;
#14275 = CARTESIAN_POINT ( 'NONE',  ( -152.2873556200145231, 67.91256772393731467, -22.43757778285992899 ) ) ;
#14276 = DIRECTION ( 'NONE',  ( -1.000000000000000000, 0.000000000000000000, 0.000000000000000000 ) ) ;
#14277 = CARTESIAN_POINT ( 'NONE',  ( -78.66644367742111399, -170.0000000000000000, -15.77090004125421352 ) ) ;
#14278 = CARTESIAN_POINT ( 'NONE',  ( 108.7020975237396812, -21.46299323290192618, 4.831387770023936490 ) ) ;
#14279 = TOROIDAL_SURFACE ( 'NONE', #47940, 5.400000000000001243, 0.4000000000000000222 ) ;
#14280 = CARTESIAN_POINT ( 'NONE',  ( -60.95805269991217301, 17.39401718769329364, 33.18720258285724611 ) ) ;
#14281 = CARTESIAN_POINT ( 'NONE',  ( -36.00304714721389132, 11.40794940913600186, -63.69002027861343862 ) ) ;
#14282 = VECTOR ( 'NONE', #44130, 1000.000000000000000 ) ;
#14283 = PLANE ( 'NONE',  #3138 ) ;
#14284 = CARTESIAN_POINT ( 'NONE',  ( 9.290502160020464473, 6.379616279862541539, -19.92800821493562680 ) ) ;
#14285 = VERTEX_POINT ( 'NONE', #60714 ) ;
#14286 = CARTESIAN_POINT ( 'NONE',  ( -2.174378755909798233, 6.588636630831477881, -37.96269615286738031 ) ) ;
#14287 = CARTESIAN_POINT ( 'NONE',  ( 188.5837490358996433, 86.53279111916958755, 63.34238295915565686 ) ) ;
#14288 = CARTESIAN_POINT ( 'NONE',  ( -118.6288898061518324, 41.89286798341290563, 9.393189492624903991 ) ) ;
#14289 = CARTESIAN_POINT ( 'NONE',  ( -37.04655464516766727, -53.85410457537912521, 41.38025477438755928 ) ) ;
#14290 = CARTESIAN_POINT ( 'NONE',  ( 128.9253503890652723, 38.52561778336674081, -22.33494626306552178 ) ) ;
#14292 = EDGE_CURVE ( 'NONE', #24611, #28268, #42812, .T. ) ;
#14291 = CARTESIAN_POINT ( 'NONE',  ( 23.03546163277113124, 7.848986635155159597, -14.22797331585904779 ) ) ;
#14293 = CARTESIAN_POINT ( 'NONE',  ( 9.837735240994033958, 7.389327806910500840, 6.098290571077138900 ) ) ;
#14294 = VECTOR ( 'NONE', #31128, 1000.000000000000114 ) ;
#14295 = EDGE_CURVE ( 'NONE', #46683, #43624, #67606, .T. ) ;
#14296 = ORIENTED_EDGE ( 'NONE', *, *, #14910, .T. ) ;
#14297 = APPLICATION_PROTOCOL_DEFINITION ( 'draft international standard', 'automotive_design', 1998, #45341 ) ;
#14298 = CARTESIAN_POINT ( 'NONE',  ( 126.3681350380370958, 38.23508791628619008, -43.03070144732701152 ) ) ;
#14299 = CARTESIAN_POINT ( 'NONE',  ( -125.8938041572051105, 46.49392987655494380, -34.91370389823391918 ) ) ;
#14300 = CARTESIAN_POINT ( 'NONE',  ( -173.1211646369891355, -170.0000000000000000, -42.21195716474999671 ) ) ;
#14301 = CONTEXT_DEPENDENT_SHAPE_REPRESENTATION ( #36403, #59 ) ;
#14302 = DIRECTION ( 'NONE',  ( 1.000000000000000000, 0.000000000000000000, 0.000000000000000000 ) ) ;
#14303 = ORIENTED_EDGE ( 'NONE', *, *, #34401, .F. ) ;
#14304 = VERTEX_POINT ( 'NONE', #25177 ) ;
#14306 = EDGE_CURVE ( 'NONE', #40455, #34795, #30104, .T. ) ;
#14305 = DIRECTION ( 'NONE',  ( 0.000000000000000000, 1.000000000000000000, 0.000000000000000000 ) ) ;
#14307 = FACE_OUTER_BOUND ( 'NONE', #55309, .T. ) ;
#14308 = ORIENTED_EDGE ( 'NONE', *, *, #40169, .T. ) ;
#14309 = ADVANCED_FACE ( 'NONE', ( #45928 ), #8650, .F. ) ;
#14310 = CARTESIAN_POINT ( 'NONE',  ( 152.9555868970377617, 55.47759417304577312, 84.60090716898641006 ) ) ;
#14311 = ORIENTED_EDGE ( 'NONE', *, *, #35292, .T. ) ;
#14312 = CARTESIAN_POINT ( 'NONE',  ( -62.54086041493278714, 17.86944394914988621, 11.46389630284894245 ) ) ;
#14313 = DIRECTION ( 'NONE',  ( 0.000000000000000000, 1.000000000000000000, 0.000000000000000000 ) ) ;
#14314 = EDGE_CURVE ( 'NONE', #48274, #56852, #63145, .T. ) ;
#14315 = CARTESIAN_POINT ( 'NONE',  ( -155.1204242627070471, 70.44799358128194910, 33.24034032259653060 ) ) ;
#14316 = CARTESIAN_POINT ( 'NONE',  ( -97.49219489034500441, 30.41416107059313134, 32.22565006754435757 ) ) ;
#14317 = FACE_OUTER_BOUND ( 'NONE', #22640, .T. ) ;
#14319 = ORIENTED_EDGE ( 'NONE', *, *, #19805, .T. ) ;
#14318 = LINE ( 'NONE', #40350, #65662 ) ;
#14320 = VECTOR ( 'NONE', #62307, 1000.000000000000000 ) ;
#14321 = DIRECTION ( 'NONE',  ( 0.000000000000000000, 0.000000000000000000, 1.000000000000000000 ) ) ;
#14322 = ORIENTED_EDGE ( 'NONE', *, *, #20983, .F. ) ;
#14323 = ORIENTED_EDGE ( 'NONE', *, *, #33180, .F. ) ;
#14324 = VECTOR ( 'NONE', #43839, 1000.000000000000000 ) ;
#14325 = CARTESIAN_POINT ( 'NONE',  ( 174.4912080999798434, 73.57140295268871455, 40.39465835065680466 ) ) ;
#14326 = APPLICATION_CONTEXT ( 'automotive_design' ) ;
#14327 = CARTESIAN_POINT ( 'NONE',  ( -33.53989818724163996, 10.96657222678981647, -89.29382644890102938 ) ) ;
#14328 = AXIS2_PLACEMENT_3D ( 'NONE', #2958, #24757, #35306 ) ;
#14330 = VERTEX_POINT ( 'NONE', #68424 ) ;
#14329 = CARTESIAN_POINT ( 'NONE',  ( -127.6894679065405427, 48.89973668460850575, 72.26033685317716504 ) ) ;
#14331 = CARTESIAN_POINT ( 'NONE',  ( -102.0448918136529528, 33.79000532939934942, 84.20608419455113847 ) ) ;
#14332 = FACE_BOUND ( 'NONE', #37301, .T. ) ;
#14333 = STYLED_ITEM ( 'NONE', ( #11981 ), #63157 ) ;
#14334 = ORIENTED_EDGE ( 'NONE', *, *, #2460, .F. ) ;
#14335 = VECTOR ( 'NONE', #58347, 1000.000000000000000 ) ;
#14336 = CARTESIAN_POINT ( 'NONE',  ( -59.57733000654211253, 15.94108165424593082, -21.87290956083888460 ) ) ;
#14337 = EDGE_CURVE ( 'NONE', #26154, #23331, #24490, .T. ) ;
#14338 = VECTOR ( 'NONE', #31714, 1000.000000000000000 ) ;
#14339 = CARTESIAN_POINT ( 'NONE',  ( 137.4031600461560458, 44.79620770172218158, 30.39764953766911404 ) ) ;
#14340 = CARTESIAN_POINT ( 'NONE',  ( 117.0069443446175512, 33.26475960880694061, 40.36144550428178945 ) ) ;
#14341 = CARTESIAN_POINT ( 'NONE',  ( -102.2801239173131052, 32.78103895658058065, 3.674523915951417141 ) ) ;
#14342 = CARTESIAN_POINT ( 'NONE',  ( -99.98930671699734773, 31.63190627461932891, -76.51612866312223105 ) ) ;
#14343 = EDGE_LOOP ( 'NONE', ( #60324, #60855 ) ) ;
#14344 = EDGE_LOOP ( 'NONE', ( #5344, #38261, #67796, #52453 ) ) ;
#14345 = CARTESIAN_POINT ( 'NONE',  ( -143.4048679855201271, 60.45763799613828837, -11.10110644613702213 ) ) ;
#14346 = CARTESIAN_POINT ( 'NONE',  ( 15.55634918610409656, 31.11269837220803325, 0.000000000000000000 ) ) ;
#14347 = CARTESIAN_POINT ( 'NONE',  ( 46.66904755831207297, -10.55634918610412853, 85.00100000000000477 ) ) ;
#14348 = DIRECTION ( 'NONE',  ( 1.000000000000000000, -0.000000000000000000, -0.000000000000000000 ) ) ;
#14349 = CARTESIAN_POINT ( 'NONE',  ( -35.00000000000000000, 225.0000000000000000, 2.000000000000000000 ) ) ;
#14350 = FACE_OUTER_BOUND ( 'NONE', #10905, .T. ) ;
#14351 = CARTESIAN_POINT ( 'NONE',  ( -148.4259959918497600, 63.26767374754761875, 45.64561139210511698 ) ) ;
#14352 = DIRECTION ( 'NONE',  ( 0.000000000000000000, -0.7071067811865474617, -0.7071067811865474617 ) ) ;
#14353 = CARTESIAN_POINT ( 'NONE',  ( 208.9507214515059843, 112.3605999017434982, 57.35864500749378436 ) ) ;
#14354 = VERTEX_POINT ( 'NONE', #4061 ) ;
#14355 = CARTESIAN_POINT ( 'NONE',  ( -103.2164890789475464, 34.39030697009942372, 45.47519882833343985 ) ) ;
#14356 = ORIENTED_EDGE ( 'NONE', *, *, #31094, .F. ) ;
#14357 = CARTESIAN_POINT ( 'NONE',  ( -38.93922791710217979, 10.94334660650242341, 10.62999269609350073 ) ) ;
#14358 = FILL_AREA_STYLE_COLOUR ( '', #9409 ) ;
#14359 = ORIENTED_EDGE ( 'NONE', *, *, #29460, .F. ) ;
#14360 = CARTESIAN_POINT ( 'NONE',  ( -82.70370746070747714, 23.90061571611317959, -89.98019051878993935 ) ) ;
#14361 = FACE_OUTER_BOUND ( 'NONE', #53255, .T. ) ;
#14362 = DIRECTION ( 'NONE',  ( 1.000000000000000000, 1.387778780781445429E-16, 0.000000000000000000 ) ) ;
#14363 = CARTESIAN_POINT ( 'NONE',  ( -58.33959211651037435, 29.48226216511319464, 6.377659838150142091E-18 ) ) ;
#14364 = CARTESIAN_POINT ( 'NONE',  ( 35.44781468922823109, 7.928097401423682911, 4.191639090875672657 ) ) ;
#14365 = CYLINDRICAL_SURFACE ( 'NONE', #8656, 7.500000000000013323 ) ;
#14366 = CARTESIAN_POINT ( 'NONE',  ( -38.93938005333175312, 11.96888249046460473, -15.73295882571353133 ) ) ;
#14367 = ADVANCED_FACE ( 'NONE', ( #41349 ), #36067, .T. ) ;
#14368 = ORIENTED_EDGE ( 'NONE', *, *, #10921, .T. ) ;
#14369 = VECTOR ( 'NONE', #37830, 1000.000000000000000 ) ;
#14370 = CARTESIAN_POINT ( 'NONE',  ( -55.05276343752910151, -170.0000000000000000, -96.40542517938723677 ) ) ;
#14371 = VERTEX_POINT ( 'NONE', #9330 ) ;
#14372 = CARTESIAN_POINT ( 'NONE',  ( -53.31111153860250340, -37.18770477615797176, 40.00000000000003553 ) ) ;
#14373 = CARTESIAN_POINT ( 'NONE',  ( -24.40147488398712383, 5.437648709335531905, 0.000000000000000000 ) ) ;
#14374 = CARTESIAN_POINT ( 'NONE',  ( -23.93965512371324422, 8.480096402797093091, 10.36685825010890660 ) ) ;
#14375 = VERTEX_POINT ( 'NONE', #52238 ) ;
#14376 = FACE_OUTER_BOUND ( 'NONE', #2514, .T. ) ;
#14378 = ADVANCED_FACE ( 'NONE', ( #9683 ), #14947, .T. ) ;
#14377 = CARTESIAN_POINT ( 'NONE',  ( -59.62510596525322626, 15.95520351401966863, -90.45643964509370960 ) ) ;
#14379 = CARTESIAN_POINT ( 'NONE',  ( -101.3602137809054398, 32.31558061113913283, -23.12788902119873313 ) ) ;
#14380 = AXIS2_PLACEMENT_3D ( 'NONE', #24758, #63424, #57113 ) ;
#14381 = CARTESIAN_POINT ( 'NONE',  ( 155.7167524447090727, 57.56687707799952136, -36.31862843462141655 ) ) ;
#14382 = EDGE_CURVE ( 'NONE', #55222, #42236, #31474, .T. ) ;
#14383 = AXIS2_PLACEMENT_3D ( 'NONE', #44916, #18536, #46292 ) ;
#14384 = ORIENTED_EDGE ( 'NONE', *, *, #14057, .T. ) ;
#14385 = ADVANCED_FACE ( 'NONE', ( #41684 ), #25865, .T. ) ;
#14386 = CARTESIAN_POINT ( 'NONE',  ( 848.0071894358292184, 1011.991584617518470, 794.0068267248692564 ) ) ;
#14387 = CARTESIAN_POINT ( 'NONE',  ( 0.000000000000000000, 70.00000000000000000, -30.00000000000000000 ) ) ;
#14388 = CARTESIAN_POINT ( 'NONE',  ( 173.8576514579035290, 72.97529922124007840, -14.85231137013811598 ) ) ;
#14389 = CARTESIAN_POINT ( 'NONE',  ( -123.6699087229882252, 45.04696784753414818, 30.95361604618596019 ) ) ;
#14390 = VECTOR ( 'NONE', #20986, 1000.000000000000000 ) ;
#14391 = FACE_OUTER_BOUND ( 'NONE', #17908, .T. ) ;
#14392 = ORIENTED_EDGE ( 'NONE', *, *, #32938, .T. ) ;
#14393 = CARTESIAN_POINT ( 'NONE',  ( -173.1211646369891355, 88.63826465341151106, -76.55650775521370122 ) ) ;
#14394 = CARTESIAN_POINT ( 'NONE',  ( 131.4581049088925511, 41.16307974347478904, 83.58612097971699484 ) ) ;
#14395 = CARTESIAN_POINT ( 'NONE',  ( 110.7164744784864325, 29.10110206241302677, 44.61121420573734753 ) ) ;
#14396 = SURFACE_STYLE_USAGE ( .BOTH. , #56599 ) ;
#14397 = EDGE_CURVE ( 'NONE', #13226, #23841, #58417, .T. ) ;
#14398 = DIRECTION ( 'NONE',  ( -1.000000000000000000, 0.000000000000000000, 0.000000000000000000 ) ) ;
#14399 = ORIENTED_EDGE ( 'NONE', *, *, #62080, .F. ) ;
#14400 = CARTESIAN_POINT ( 'NONE',  ( 200.4600337307566349, 100.7087439352121265, 42.91312774902829830 ) ) ;
#14401 = CARTESIAN_POINT ( 'NONE',  ( 110.7114632166112216, 29.09878355652111637, -77.76698815611742077 ) ) ;
#14402 = CARTESIAN_POINT ( 'NONE',  ( 181.9411407973025234, 80.91291802046384873, 44.30859410551142474 ) ) ;
#14403 = CARTESIAN_POINT ( 'NONE',  ( 137.4031600461560458, 44.79620770172221000, 3.553098947205445501 ) ) ;
#14404 = CARTESIAN_POINT ( 'NONE',  ( -49.42000000000000171, -36.09918303830819752, 15.41169613715280562 ) ) ;
#14405 = ORIENTED_EDGE ( 'NONE', *, *, #18927, .F. ) ;
#14406 = CARTESIAN_POINT ( 'NONE',  ( 164.0073343966822392, 64.23003864582454980, -13.09387731840895164 ) ) ;
#14407 = EDGE_LOOP ( 'NONE', ( #51640, #26692, #12402, #5887 ) ) ;
#14408 = CARTESIAN_POINT ( 'NONE',  ( 70.41705859591012029, 15.55317472777717747, 62.92014748638126775 ) ) ;
#14409 = CARTESIAN_POINT ( 'NONE',  ( 127.5859662773347054, 37.76488191276836659, 86.57016596594176860 ) ) ;
#14411 = ORIENTED_EDGE ( 'NONE', *, *, #62422, .F. ) ;
#14410 = LINE ( 'NONE', #19329, #47763 ) ;
#14412 = CARTESIAN_POINT ( 'NONE',  ( 161.7031777507226593, 62.31724004902780223, -37.41578519910148515 ) ) ;
#14413 = CARTESIAN_POINT ( 'NONE',  ( -4.999999999999999112, 6.123233995736765296E-16, 3.469446951953614189E-15 ) ) ;
#14414 = CARTESIAN_POINT ( 'NONE',  ( 160.5141379054753941, 60.05651755415394888, -36.75489487743244865 ) ) ;
#14415 = ORIENTED_EDGE ( 'NONE', *, *, #50724, .T. ) ;
#14416 = CARTESIAN_POINT ( 'NONE',  ( -94.83794676023109105, 30.26879337035744655, 12.23732165643094838 ) ) ;
#14417 = LINE ( 'NONE', #29901, #51494 ) ;
#14418 = AXIS2_PLACEMENT_3D ( 'NONE', #1483, #15925, #37371 ) ;
#14419 = CARTESIAN_POINT ( 'NONE',  ( 150.4748268795259776, 53.65235499498208327, -94.57192694735240934 ) ) ;
#14420 = CARTESIAN_POINT ( 'NONE',  ( 80.73462811483977930, 18.54763808182591944, -21.14099230513408401 ) ) ;
#14421 = LINE ( 'NONE', #41152, #59452 ) ;
#14422 = CARTESIAN_POINT ( 'NONE',  ( 152.2940756559018780, 53.73566983921582363, 58.32125015338372265 ) ) ;
#14423 = CARTESIAN_POINT ( 'NONE',  ( 181.0840389613909736, -170.0000000000000000, 17.46404351504774510 ) ) ;
#14424 = EDGE_LOOP ( 'NONE', ( #9158, #4578 ) ) ;
#14425 = FACE_OUTER_BOUND ( 'NONE', #44279, .T. ) ;
#14426 = CARTESIAN_POINT ( 'NONE',  ( -11.57950265606958062, 8.174070387114795722, 70.95759044635187252 ) ) ;
#14427 = B_SPLINE_CURVE_WITH_KNOTS ( 'NONE', 3,
 ( #28647, #17751, #39206, #5781, #49027, #3300, #40244, #29337, #8587, #7549, #56411, #2608, #24067, #50451, #14202, #30036, #57116, #29008, #50789, #39892, #61688, #56073, #29682, #7890, #13513, #51499, #8929, #34968, #61349, #45511, #13848, #24761, #66995, #46194, #23718, #61000 ),
 .UNSPECIFIED., .F., .F.,
 ( 4, 2, 2, 2, 2, 2, 2, 2, 2, 2, 2, 2, 2, 2, 2, 2, 2, 4 ),
 ( 0.02352539391595311752, 0.02450549414544721943, 0.02548559437494132135, 0.02646569460443541980, 0.02744579483392952171, 0.02842589506342362016, 0.02940599529291772207, 0.03038609552241182052, 0.03136619575190591896, 0.03234629598140002088, 0.03332639621089411586, 0.03430649644038821777, 0.03528659666988231969, 0.03626669689937642160, 0.03724679712887052352, 0.03773684724361749815, 0.03822689735836447278, 0.03920699758785825551 ),
 .UNSPECIFIED. ) ;
#14428 = ORIENTED_EDGE ( 'NONE', *, *, #53094, .T. ) ;
#14429 = CARTESIAN_POINT ( 'NONE',  ( 154.4617654203035784, 56.60942201271838314, -23.66421568052971836 ) ) ;
#14430 = AXIS2_PLACEMENT_3D ( 'NONE', #16488, #59392, #10513 ) ;
#14431 = CARTESIAN_POINT ( 'NONE',  ( -55.38707628885372714, 14.77122047090632506, 84.00730630929061249 ) ) ;
#14432 = VECTOR ( 'NONE', #65043, 1000.000000000000000 ) ;
#14433 = CARTESIAN_POINT ( 'NONE',  ( 104.3759779378692514, 27.35691041569131343, 41.80980636896079972 ) ) ;
#14434 = EDGE_CURVE ( 'NONE', #51018, #67247, #22479, .T. ) ;
#14435 = DIRECTION ( 'NONE',  ( 0.000000000000000000, 0.000000000000000000, 1.000000000000000000 ) ) ;
#14436 = LINE ( 'NONE', #35886, #7869 ) ;
#14437 = CARTESIAN_POINT ( 'NONE',  ( 188.2091813586561670, 87.61952156613880049, 12.32265291410417341 ) ) ;
#14438 = CARTESIAN_POINT ( 'NONE',  ( 209.6877167158271220, 113.4449353909247549, -38.22188785752970830 ) ) ;
#14439 = CARTESIAN_POINT ( 'NONE',  ( 173.6020601204681952, 71.36108012062129546, 10.56114396026872271 ) ) ;
#14440 = ORIENTED_EDGE ( 'NONE', *, *, #25257, .F. ) ;
#14441 = DIRECTION ( 'NONE',  ( -0.000000000000000000, 1.000000000000000000, -0.000000000000000000 ) ) ;
#14442 = EDGE_LOOP ( 'NONE', ( #46737, #17190 ) ) ;
#14443 = CARTESIAN_POINT ( 'NONE',  ( 104.3805245147141534, 26.26278144139197934, -74.97124564213564213 ) ) ;
#14444 = CARTESIAN_POINT ( 'NONE',  ( 43.14669449386823175, 9.942681284149132992, -9.758692608636117427 ) ) ;
#14445 = CARTESIAN_POINT ( 'NONE',  ( 29.69502258243350923, 57.82046033912877903, 170.0000000000000000 ) ) ;
#14446 = DIRECTION ( 'NONE',  ( 0.000000000000000000, 0.000000000000000000, -1.000000000000000000 ) ) ;
#14447 = CARTESIAN_POINT ( 'NONE',  ( 53.32245423372562243, 37.19594572654712294, 43.58025477438756923 ) ) ;
#14448 = CARTESIAN_POINT ( 'NONE',  ( -108.6944271866239404, 37.30738480893076314, -11.75132388696829899 ) ) ;
#14449 = VERTEX_POINT ( 'NONE', #42029 ) ;
#14450 = CARTESIAN_POINT ( 'NONE',  ( -73.79615177260654946, 20.52570924097573624, 70.48734656626530182 ) ) ;
#14451 = CARTESIAN_POINT ( 'NONE',  ( -55.05276343752910151, -170.0000000000000000, 30.31732777293113301 ) ) ;
#14452 = ORIENTED_EDGE ( 'NONE', *, *, #25350, .F. ) ;
#14453 = EDGE_LOOP ( 'NONE', ( #67858, #69247, #37240, #68009 ) ) ;
#14455 = EDGE_CURVE ( 'NONE', #57503, #50950, #63489, .T. ) ;
#14454 = CARTESIAN_POINT ( 'NONE',  ( -153.7005182577089215, 67.81869626254723471, 44.45584362651335653 ) ) ;
#14456 = CARTESIAN_POINT ( 'NONE',  ( -36.60035679358400529, 11.39778710981509668, 13.32819397642333392 ) ) ;
#14457 = CARTESIAN_POINT ( 'NONE',  ( 177.7889574972181777, 75.33777460203558007, -23.63291069985390536 ) ) ;
#14458 = LINE ( 'NONE', #52431, #10308 ) ;
#14459 = DIRECTION ( 'NONE',  ( 0.000000000000000000, 0.000000000000000000, -1.000000000000000000 ) ) ;
#14460 = EDGE_CURVE ( 'NONE', #67324, #31650, #30258, .T. ) ;
#14461 = ORIENTED_EDGE ( 'NONE', *, *, #51380, .F. ) ;
#14462 = CARTESIAN_POINT ( 'NONE',  ( -51.33022649596136233, 5.874856473938592671, 26.66469104408688295 ) ) ;
#14463 = ORIENTED_EDGE ( 'NONE', *, *, #21033, .F. ) ;
#14464 = CARTESIAN_POINT ( 'NONE',  ( 18.88468164817598804, 7.626722602998420975, -49.85434746371562653 ) ) ;
#14465 = CARTESIAN_POINT ( 'NONE',  ( 8.288696687633802185, 7.382586467017838494, 63.85837421632901822 ) ) ;
#14466 = CARTESIAN_POINT ( 'NONE',  ( 211.1200456646897123, 115.5868795682033578, 40.59128962156992770 ) ) ;
#14467 = FACE_BOUND ( 'NONE', #50394, .T. ) ;
#14468 = EDGE_CURVE ( 'NONE', #16629, #67458, #11048, .T. ) ;
#14469 = VERTEX_POINT ( 'NONE', #497 ) ;
#14470 = AXIS2_PLACEMENT_3D ( 'NONE', #16708, #1584, #59964 ) ;
#14471 = ORIENTED_EDGE ( 'NONE', *, *, #18798, .F. ) ;
#14472 = CARTESIAN_POINT ( 'NONE',  ( 110.3299582524531957, -21.42428528562853174, -5.000000000000005329 ) ) ;
#14473 = CARTESIAN_POINT ( 'NONE',  ( -133.2252929082529249, 52.75117980926378891, 93.42566031637895207 ) ) ;
#14474 = CARTESIAN_POINT ( 'NONE',  ( -166.9982296371934751, 80.56207291422406058, -19.70677099263670584 ) ) ;
#14475 = DIRECTION ( 'NONE',  ( 0.000000000000000000, 0.000000000000000000, 1.000000000000000000 ) ) ;
#14476 = CARTESIAN_POINT ( 'NONE',  ( 9.608296193479125336, 6.381315205148816894, 86.90354082819708026 ) ) ;
#14477 = CARTESIAN_POINT ( 'NONE',  ( 79.93126905972555107, 17.24332478304276250, -73.54974159810120682 ) ) ;
#14478 = CIRCLE ( 'NONE', #21293, 2.999999999999999112 ) ;
#14479 = VERTEX_POINT ( 'NONE', #21949 ) ;
#14480 = DIRECTION ( 'NONE',  ( 0.000000000000000000, 0.000000000000000000, -1.000000000000000000 ) ) ;
#14481 = CARTESIAN_POINT ( 'NONE',  ( -100.4466073551322722, 31.85873123265079698, 57.57636481214915847 ) ) ;
#14482 = ORIENTED_EDGE ( 'NONE', *, *, #68300, .F. ) ;
#14483 = DIRECTION ( 'NONE',  ( -0.000000000000000000, 1.000000000000000000, -0.000000000000000000 ) ) ;
#14484 = ORIENTED_EDGE ( 'NONE', *, *, #57557, .T. ) ;
#14485 = DIRECTION ( 'NONE',  ( -0.000000000000000000, 1.000000000000000000, -0.000000000000000000 ) ) ;
#14486 = ORIENTED_EDGE ( 'NONE', *, *, #33150, .F. ) ;
#14487 = VERTEX_POINT ( 'NONE', #42373 ) ;
#14488 = CARTESIAN_POINT ( 'NONE',  ( 39.40195752203892710, 9.424259417798131366, 56.75838489642694640 ) ) ;
#14489 = CARTESIAN_POINT ( 'NONE',  ( -109.6829043543429236, 37.85329552808669717, -95.00000000000133582 ) ) ;
#14490 = CARTESIAN_POINT ( 'NONE',  ( 104.3759779378692372, 27.35691041569131343, 14.96525577849715027 ) ) ;
#14491 = VERTEX_POINT ( 'NONE', #69091 ) ;
#14492 = CARTESIAN_POINT ( 'NONE',  ( -32.73509123563383127, 9.807531206076880892, 84.01140421885408216 ) ) ;
#14493 = CARTESIAN_POINT ( 'NONE',  ( 174.4912080999798434, 73.57140295268874297, -66.98354401119793522 ) ) ;
#14494 = DIRECTION ( 'NONE',  ( -0.000000000000000000, -0.000000000000000000, -1.000000000000000000 ) ) ;
#14495 = CARTESIAN_POINT ( 'NONE',  ( 102.8066580714141054, 25.59117171226999332, -44.43077199080595108 ) ) ;
#14496 = DIRECTION ( 'NONE',  ( 1.000000000000000000, 0.000000000000000000, -0.000000000000000000 ) ) ;
#14497 = CARTESIAN_POINT ( 'NONE',  ( -5.000000000000000888, 0.000000000000000000, -9.474599999999998801 ) ) ;
#14498 = ORIENTED_EDGE ( 'NONE', *, *, #16820, .T. ) ;
#14499 = EDGE_LOOP ( 'NONE', ( #28303, #35429 ) ) ;
#14500 = DIRECTION ( 'NONE',  ( -1.000000000000000000, 0.000000000000000000, 0.000000000000000000 ) ) ;
#14501 = CARTESIAN_POINT ( 'NONE',  ( -78.66644367742109978, 23.39876645725288284, -76.96000122218160300 ) ) ;
#14502 = CARTESIAN_POINT ( 'NONE',  ( 173.6737675136087375, 72.80308721038093722, 8.769662785337226651 ) ) ;
#14503 = FACE_OUTER_BOUND ( 'NONE', #42414, .T. ) ;
#14504 = ADVANCED_FACE ( 'NONE', ( #20920 ), #64168, .F. ) ;
#14505 = DIRECTION ( 'NONE',  ( 0.9009688679024218105, -0.4338837391175525693, 0.000000000000000000 ) ) ;
#14506 = CARTESIAN_POINT ( 'NONE',  ( 133.8566784816069344, 41.42467568809808398, -89.71241211332301191 ) ) ;
#14507 = CARTESIAN_POINT ( 'NONE',  ( 34.16438717774036604, 7.785979658506379408, -91.43666240146571056 ) ) ;
#14508 = CARTESIAN_POINT ( 'NONE',  ( -85.35521056349260505, 24.98314685266450752, 94.99999999999866418 ) ) ;
#14509 = CARTESIAN_POINT ( 'NONE',  ( 206.2957331585308509, 110.2946564621823029, 29.33458522330292340 ) ) ;
#14510 = CARTESIAN_POINT ( 'NONE',  ( -86.16504208171677703, 26.41251233979376067, 64.23306810451259707 ) ) ;
#14511 = CARTESIAN_POINT ( 'NONE',  ( -104.1244073710070239, 33.72720758483609416, 45.30355529039214701 ) ) ;
#14513 = ORIENTED_EDGE ( 'NONE', *, *, #60126, .T. ) ;
#14512 = ADVANCED_FACE ( 'NONE', ( #10025 ), #1144, .T. ) ;
#14514 = CARTESIAN_POINT ( 'NONE',  ( 0.000000000000000000, 0.000000000000000000, 0.000000000000000000 ) ) ;
#14515 = ORIENTED_EDGE ( 'NONE', *, *, #36287, .F. ) ;
#14516 = CARTESIAN_POINT ( 'NONE',  ( 197.9847015768255005, 97.56951352050452897, -13.62497584703676168 ) ) ;
#14517 = ORIENTED_EDGE ( 'NONE', *, *, #45734, .F. ) ;
#14518 = AXIS2_PLACEMENT_3D ( 'NONE', #43230, #33752, #40104 ) ;
#14519 = CYLINDRICAL_SURFACE ( 'NONE', #44443, 7.500000000000013323 ) ;
#14520 = DIRECTION ( 'NONE',  ( -0.5407162030609372616, -0.6444004775717706579, -0.5407162030609377057 ) ) ;
#14521 = CARTESIAN_POINT ( 'NONE',  ( 8.942470798084380945, -23.47701018505899739, 3.061616997868437868E-16 ) ) ;
#14522 = CARTESIAN_POINT ( 'NONE',  ( 65.35403040894466642, -1.250000000000021760, 41.38025477438755928 ) ) ;
#14524 = CARTESIAN_POINT ( 'NONE',  ( -84.49322488516129681, 0.000000000000000000, 43.58025477438756212 ) ) ;
#14523 = CIRCLE ( 'NONE', #25733, 10.00000000000000178 ) ;
#14525 = DIRECTION ( 'NONE',  ( 0.000000000000000000, 0.000000000000000000, 1.000000000000000000 ) ) ;
#14526 = CARTESIAN_POINT ( 'NONE',  ( 199.9741262455892752, 100.0845158163269133, 84.56275067836362780 ) ) ;
#14527 = CARTESIAN_POINT ( 'NONE',  ( 11.20486344102687504, 7.403248964808832433, -37.06203751448568795 ) ) ;
#14528 = LINE ( 'NONE', #53863, #17187 ) ;
#14529 = ORIENTED_EDGE ( 'NONE', *, *, #13906, .F. ) ;
#14530 = EDGE_CURVE ( 'NONE', #69123, #47461, #42711, .T. ) ;
#14531 = ORIENTED_EDGE ( 'NONE', *, *, #48902, .T. ) ;
#14532 = ADVANCED_FACE ( 'NONE', ( #43048 ), #32854, .F. ) ;
#14533 = DIRECTION ( 'NONE',  ( 0.000000000000000000, 0.000000000000000000, 1.000000000000000000 ) ) ;
#14534 = FILL_AREA_STYLE_COLOUR ( '', #456 ) ;
#14535 = DIRECTION ( 'NONE',  ( -0.8090169943749506709, 0.5877852522924686962, 0.000000000000000000 ) ) ;
#14536 = EDGE_CURVE ( 'NONE', #11118, #69500, #38126, .T. ) ;
#14537 = CIRCLE ( 'NONE', #4445, 5.000000000000004441 ) ;
#14538 = CARTESIAN_POINT ( 'NONE',  ( 14.08699529666006178, 6.452200550165255954, 17.97873554617772029 ) ) ;
#14539 = CARTESIAN_POINT ( 'NONE',  ( 46.51679720856117228, 10.46086439153924630, -72.38759062435165959 ) ) ;
#14540 = VERTEX_POINT ( 'NONE', #44811 ) ;
#14541 = CARTESIAN_POINT ( 'NONE',  ( 186.2575601542430377, 85.47765906955505955, -11.44511139629197061 ) ) ;
#14542 = CARTESIAN_POINT ( 'NONE',  ( 179.0096185093687495, 76.53352131383243773, -77.79008292104482791 ) ) ;
#14543 = CARTESIAN_POINT ( 'NONE',  ( -180.0175713311536470, 95.14770835574078944, -45.17381040195942177 ) ) ;
#14544 = CARTESIAN_POINT ( 'NONE',  ( 87.59061758233886508, 19.75077892934018919, -9.023281811036417466 ) ) ;
#14545 = CARTESIAN_POINT ( 'NONE',  ( -25.49247221749737591, 9.706368398275744269, 69.15791252073658768 ) ) ;
#14546 = CARTESIAN_POINT ( 'NONE',  ( 105.3198800741404284, 21.92942769035742501, 1.767193244627911719 ) ) ;
#14547 = CARTESIAN_POINT ( 'NONE',  ( -48.57297291660695748, 13.03920345822338156, 60.85288077998132650 ) ) ;
#14548 = ADVANCED_FACE ( 'NONE', ( #50770 ), #54995, .F. ) ;
#14549 = VERTEX_POINT ( 'NONE', #59920 ) ;
#14550 = CARTESIAN_POINT ( 'NONE',  ( -55.05276343752909440, 14.68156374112638929, 57.16187836339483397 ) ) ;
#14551 = DIRECTION ( 'NONE',  ( -1.000000000000000000, 0.000000000000000000, 0.000000000000000000 ) ) ;
#14552 = CARTESIAN_POINT ( 'NONE',  ( -108.6622665321722963, 37.28993738537008795, -73.30661870913355926 ) ) ;
#14553 = CARTESIAN_POINT ( 'NONE',  ( -48.32993240732253781, 12.98137013984324994, -39.35435737847355853 ) ) ;
#14554 = EDGE_CURVE ( 'NONE', #41180, #40156, #33216, .T. ) ;
#14555 = DIRECTION ( 'NONE',  ( 0.000000000000000000, 0.000000000000000000, 1.000000000000000000 ) ) ;
#14556 = ADVANCED_FACE ( 'NONE', ( #56056 ), #38841, .F. ) ;
#14557 = CARTESIAN_POINT ( 'NONE',  ( -20.63749999999999574, 0.000000000000000000, 0.000000000000000000 ) ) ;
#14558 = EDGE_CURVE ( 'NONE', #22538, #40260, #28097, .T. ) ;
#14559 = VERTEX_POINT ( 'NONE', #39528 ) ;
#14560 = CARTESIAN_POINT ( 'NONE',  ( -422.6627218934914936, 399.9999999999998863, -146.4497041420118251 ) ) ;
#14561 = CARTESIAN_POINT ( 'NONE',  ( 26.69682282325795697, -59.27986298182186431, 170.0000000000000000 ) ) ;
#14562 = ORIENTED_EDGE ( 'NONE', *, *, #64384, .T. ) ;
#14563 = ORIENTED_EDGE ( 'NONE', *, *, #51628, .F. ) ;
#14564 = FACE_OUTER_BOUND ( 'NONE', #16300, .T. ) ;
#14565 = LINE ( 'NONE', #69047, #37760 ) ;
#14566 = CARTESIAN_POINT ( 'NONE',  ( 134.2360421295532831, 42.83129061307084839, -89.71241211332299770 ) ) ;
#14567 = ORIENTED_EDGE ( 'NONE', *, *, #47164, .F. ) ;
#14568 = DIRECTION ( 'NONE',  ( 0.000000000000000000, -0.000000000000000000, -1.000000000000000000 ) ) ;
#14569 = VECTOR ( 'NONE', #468, 1000.000000000000000 ) ;
#14570 = FACE_OUTER_BOUND ( 'NONE', #65985, .T. ) ;
#14571 = CARTESIAN_POINT ( 'NONE',  ( 1.500000000000013545, 3.000000000000030198, -1.500000000000014211 ) ) ;
#14572 = DIRECTION ( 'NONE',  ( -3.081487911019579554E-32, -1.000000000000000000, -3.469446951953612956E-17 ) ) ;
#14573 = CARTESIAN_POINT ( 'NONE',  ( 21.96921518829288900, -71.65937688154161833, 41.38025477438755928 ) ) ;
#14574 = CARTESIAN_POINT ( 'NONE',  ( 150.1343759737873995, 52.16508607228156791, 88.99384000258469030 ) ) ;
#14575 = DIRECTION ( 'NONE',  ( -0.000000000000000000, 1.000000000000000000, -0.000000000000000000 ) ) ;
#14576 = ORIENTED_EDGE ( 'NONE', *, *, #11489, .T. ) ;
#14577 = CARTESIAN_POINT ( 'NONE',  ( 105.2529848321548513, 27.73895015262024444, -22.18228092862218048 ) ) ;
#14578 = CARTESIAN_POINT ( 'NONE',  ( 10.83046137699561129, 6.392429922561258415, 70.00811123621038234 ) ) ;
#14579 = CARTESIAN_POINT ( 'NONE',  ( -25.48750459758502629, 9.705678256319565378, 33.12635188977065326 ) ) ;
#14580 = CARTESIAN_POINT ( 'NONE',  ( 197.3064269725219333, 98.33232022113057269, 38.02162036052619243 ) ) ;
#14581 = CARTESIAN_POINT ( 'NONE',  ( -81.69214136958434835, 24.57917239217752936, 84.71714431126503086 ) ) ;
#14583 = ORIENTED_EDGE ( 'NONE', *, *, #67449, .T. ) ;
#14582 = CARTESIAN_POINT ( 'NONE',  ( 15.55634918610396511, -46.66904755831214402, 85.00100000000000477 ) ) ;
#14584 = CARTESIAN_POINT ( 'NONE',  ( 69.83260694998128315, 15.39825517924928810, 40.44980415152751618 ) ) ;
#14585 = ORIENTED_EDGE ( 'NONE', *, *, #10790, .T. ) ;
#14586 = AXIS2_PLACEMENT_3D ( 'NONE', #63739, #5335, #54186 ) ;
#14587 = ORIENTED_EDGE ( 'NONE', *, *, #66674, .F. ) ;
#14588 = CARTESIAN_POINT ( 'NONE',  ( 114.6797682035588934, 32.10876583290004760, -76.33282036865305997 ) ) ;
#14589 = CARTESIAN_POINT ( 'NONE',  ( 110.2429982417149574, 29.99119854320845846, -89.61153874658103291 ) ) ;
#14590 = CARTESIAN_POINT ( 'NONE',  ( 200.4559562755963498, 100.7034888016685414, -76.87303439381707904 ) ) ;
#14591 = DIRECTION ( 'NONE',  ( 0.000000000000000000, 0.000000000000000000, 1.000000000000000000 ) ) ;
#14592 = DIRECTION ( 'NONE',  ( 2.921639538487254261E-16, 1.134144525784205431E-35, 1.000000000000000000 ) ) ;
#14593 = PLANE ( 'NONE',  #30912 ) ;
#14594 = LINE ( 'NONE', #57510, #7296 ) ;
#14595 = EDGE_CURVE ( 'NONE', #48145, #2888, #33908, .T. ) ;
#14596 = CARTESIAN_POINT ( 'NONE',  ( -48.23389383802711450, 13.99288361739331776, 34.68448182751232167 ) ) ;
#14597 = ORIENTED_EDGE ( 'NONE', *, *, #67351, .F. ) ;
#14598 = ORIENTED_EDGE ( 'NONE', *, *, #7821, .F. ) ;
#14599 = DIRECTION ( 'NONE',  ( 1.000000000000000000, 0.000000000000000000, 0.000000000000000000 ) ) ;
#14600 = CARTESIAN_POINT ( 'NONE',  ( -81.01931326044683601, 24.31309346877659650, -35.49007369283990698 ) ) ;
#14601 = CARTESIAN_POINT ( 'NONE',  ( 114.5373975997477771, 30.91911807405818635, 84.61738033458334485 ) ) ;
#14602 = CARTESIAN_POINT ( 'NONE',  ( -189.5329886872043801, 107.4958891766011249, 63.13570540318301738 ) ) ;
#14603 = B_SPLINE_CURVE_WITH_KNOTS ( 'NONE', 3,
 ( #46934, #3674, #68061, #30765, #42002, #52210, #19160, #9653, #3337, #30413, #14578, #4027, #36038, #4374, #25499, #51864, #47270, #20201, #25152, #41657, #63461, #67710, #63114, #31116, #14914, #46580, #19863, #36384, #15272, #57837, #40614, #25838, #24796, #41318, #62774, #19507, #67369, #68722, #52884, #20533, #36734, #58178, #8627 ),
 .UNSPECIFIED., .F., .F.,
 ( 4, 2, 2, 2, 2, 2, 2, 2, 1, 2, 2, 2, 2, 2, 2, 2, 2, 2, 2, 2, 2, 4 ),
 ( 3.469446951953614189E-18, 0.001465684626643306123, 0.002198526939964957558, 0.002931369253286608776, 0.004397053879929927259, 0.005862738506573245308, 0.007328423133216562489, 0.008061265446538238427, 0.008794107759859915233, 0.009526950073181592038, 0.01025979238650326711, 0.01172547701314661898, 0.01319116163978997260, 0.01465684626643334355, 0.01538968857975502903, 0.01612253089307671278, 0.01758821551972006986, 0.01905390014636342347, 0.01978674245968510895, 0.02051958477300678749, 0.02198526939965015498, 0.02345095402629352246 ),
 .UNSPECIFIED. ) ;
#14604 = CARTESIAN_POINT ( 'NONE',  ( 183.1865184929771715, 80.75677158533829925, -50.92751890011346916 ) ) ;
#14605 = CARTESIAN_POINT ( 'NONE',  ( 164.9709596662455624, 63.72607097915129515, -70.20507495433403733 ) ) ;
#14606 = ORIENTED_EDGE ( 'NONE', *, *, #14455, .F. ) ;
#14607 = EDGE_CURVE ( 'NONE', #5602, #7572, #49712, .T. ) ;
#14608 = ORIENTED_EDGE ( 'NONE', *, *, #44447, .T. ) ;
#14609 = EDGE_CURVE ( 'NONE', #41760, #32688, #5597, .T. ) ;
#14610 = ORIENTED_EDGE ( 'NONE', *, *, #50038, .F. ) ;
#14611 = EDGE_CURVE ( 'NONE', #27023, #51958, #18079, .T. ) ;
#14612 = DIRECTION ( 'NONE',  ( 1.000000000000000000, 0.000000000000000000, 0.000000000000000000 ) ) ;
#14613 = CARTESIAN_POINT ( 'NONE',  ( 86.62931800182293784, 19.42108912189597447, -23.97701360844805407 ) ) ;
#14614 = DIRECTION ( 'NONE',  ( 0.000000000000000000, 0.000000000000000000, -1.000000000000000000 ) ) ;
#14615 = CARTESIAN_POINT ( 'NONE',  ( 108.2349883415519258, -21.49634503089637150, 4.680941717099545762 ) ) ;
#14616 = EDGE_CURVE ( 'NONE', #44628, #27271, #2591, .T. ) ;
#14617 = DIRECTION ( 'NONE',  ( -0.000000000000000000, 1.000000000000000000, -0.000000000000000000 ) ) ;
#14618 = CARTESIAN_POINT ( 'NONE',  ( -156.4841188516942623, 70.33041971808549420, -18.23474518811625344 ) ) ;
#14619 = AXIS2_PLACEMENT_3D ( 'NONE', #18368, #50719, #19059 ) ;
#14620 = CARTESIAN_POINT ( 'NONE',  ( 31.90184941268614693, 7.552181687745345151, 64.01634121766176122 ) ) ;
#14621 = CARTESIAN_POINT ( 'NONE',  ( 46.83265140856891406, 9.492621673067191068, 89.88835326161378703 ) ) ;
#14622 = ORIENTED_EDGE ( 'NONE', *, *, #37702, .T. ) ;
#14623 = CARTESIAN_POINT ( 'NONE',  ( -4.725257700476002576, 6.708862164351561574, -36.08442693939512935 ) ) ;
#14624 = CARTESIAN_POINT ( 'NONE',  ( 188.2133404574782674, 86.12414067617878288, 65.99936258389180921 ) ) ;
#14625 = CARTESIAN_POINT ( 'NONE',  ( -34.96012151086515019, 55.23134702900888016, 6.377659838150195247E-18 ) ) ;
#14626 = CARTESIAN_POINT ( 'NONE',  ( 417.3372781065086201, 399.9999999999998863, 113.5502958579881891 ) ) ;
#14627 = DIRECTION ( 'NONE',  ( 0.000000000000000000, 0.000000000000000000, 1.000000000000000000 ) ) ;
#14628 = CARTESIAN_POINT ( 'NONE',  ( 21.75198946226450758, 7.772524967554916842, -20.74856676359930674 ) ) ;
#14629 = CARTESIAN_POINT ( 'NONE',  ( 9.275903038161096958, 7.385619229189520851, 14.42232764313656901 ) ) ;
#14630 = ORIENTED_EDGE ( 'NONE', *, *, #6516, .F. ) ;
#14631 = CARTESIAN_POINT ( 'NONE',  ( 188.0141161196705752, 85.90515114331881819, 12.84600617614940887 ) ) ;
#14632 = APPLICATION_PROTOCOL_DEFINITION ( 'draft international standard', 'automotive_design', 1998, #30970 ) ;
#14633 = CIRCLE ( 'NONE', #4540, 5.000000000000004441 ) ;
#14634 = CARTESIAN_POINT ( 'NONE',  ( 128.0540543950622236, 39.18660671946769725, -38.74486588045738245 ) ) ;
#14635 = CARTESIAN_POINT ( 'NONE',  ( -129.3963145237381411, 48.84337839101542755, -35.77770630875843949 ) ) ;
#14636 = EDGE_CURVE ( 'NONE', #22148, #7019, #12449, .T. ) ;
#14637 = CARTESIAN_POINT ( 'NONE',  ( -108.6622665321722963, 37.28993738537006664, -46.46206811866990449 ) ) ;
#14638 = EDGE_CURVE ( 'NONE', #8669, #15703, #2254, .T. ) ;
#14639 = CARTESIAN_POINT ( 'NONE',  ( 185.7267155939802024, 84.90388481853123892, -49.62006233998373261 ) ) ;
#14640 = VERTEX_POINT ( 'NONE', #29322 ) ;
#14641 = VERTEX_POINT ( 'NONE', #28266 ) ;
#14642 = EDGE_CURVE ( 'NONE', #47023, #56594, #45490, .T. ) ;
#14643 = CARTESIAN_POINT ( 'NONE',  ( -26.88245755577923291, 8.887394979218511182, -21.95019337430851536 ) ) ;
#14644 = DIRECTION ( 'NONE',  ( 0.000000000000000000, 0.000000000000000000, 1.000000000000000000 ) ) ;
#14645 = ORIENTED_EDGE ( 'NONE', *, *, #59771, .F. ) ;
#14646 = CARTESIAN_POINT ( 'NONE',  ( 150.9996123609081167, 54.03443948832624955, 94.40777087719918370 ) ) ;
#14647 = ORIENTED_EDGE ( 'NONE', *, *, #37476, .T. ) ;
#14648 = CARTESIAN_POINT ( 'NONE',  ( 126.3681350380371242, 38.23508791628619718, -69.87525203779068761 ) ) ;
#14649 = FACE_OUTER_BOUND ( 'NONE', #6527, .T. ) ;
#14650 = LINE ( 'NONE', #26928, #11710 ) ;
#14651 = VECTOR ( 'NONE', #24922, 1000.000000000000000 ) ;
#14652 = CARTESIAN_POINT ( 'NONE',  ( -95.52163045714283385, 29.47808868198299592, 34.75761988864483953 ) ) ;
#14653 = CARTESIAN_POINT ( 'NONE',  ( -27.41072500102445275, 43.79450017564173692, 26.66469104408688295 ) ) ;
#14655 = EDGE_LOOP ( 'NONE', ( #49700, #27053, #24923, #65784 ) ) ;
#14654 = DIRECTION ( 'NONE',  ( -0.000000000000000000, -0.000000000000000000, -1.000000000000000000 ) ) ;
#14656 = B_SPLINE_CURVE_WITH_KNOTS ( 'NONE', 3,
 ( #43195, #16479, #33007, #32661, #6620, #66084, #6970, #38631, #17875, #27722, #11892, #65726, #17515, #49160, #38992, #39333, #28418, #54798, #60436, #7328, #17157, #43889, #33372, #60776, #28068, #37933, #33715, #27369, #999, #65372, #48809, #59379, #12252, #55145, #650, #23156, #54087, #49871, #5907, #28783, #1698, #65019, #16815, #44605 ),
 .UNSPECIFIED., .F., .F.,
 ( 4, 2, 2, 2, 2, 2, 2, 2, 2, 2, 2, 2, 2, 2, 2, 2, 2, 2, 2, 2, 2, 4 ),
 ( 6.938893903907228378E-18, 0.001476829494128812335, 0.002215244241193225008, 0.002953658988257637247, 0.004430488482386464762, 0.005907317976515292710, 0.007384147470644119790, 0.008122562217708531596, 0.008860976964772943401, 0.01033780645890176528, 0.01181463595303058715, 0.01255305070009499549, 0.01329146544715940383, 0.01476829494128822744, 0.01550670968835264618, 0.01624512443541706666, 0.01772195392954591109, 0.01919878342367475552, 0.01993719817073917946, 0.02067561291780359994, 0.02215244241193246172, 0.02362927190606132349 ),
 .UNSPECIFIED. ) ;
#14657 = CARTESIAN_POINT ( 'NONE',  ( -44.00727179482576901, 47.83680621839559421, 170.0000000000000000 ) ) ;
#14658 = ORIENTED_EDGE ( 'NONE', *, *, #21073, .F. ) ;
#14659 = ORIENTED_EDGE ( 'NONE', *, *, #68405, .T. ) ;
#14660 = CARTESIAN_POINT ( 'NONE',  ( -166.0012244511291328, 80.97916541034754800, 9.102247628649013933 ) ) ;
#14661 = CARTESIAN_POINT ( 'NONE',  ( -146.5309471467636229, 62.99917515507670629, -35.42503834684312380 ) ) ;
#14663 = VERTEX_POINT ( 'NONE', #65572 ) ;
#14662 = CARTESIAN_POINT ( 'NONE',  ( -133.3944793432480651, 52.87251459353622352, 65.21942218520352696 ) ) ;
#14664 = CARTESIAN_POINT ( 'NONE',  ( 1.118033988749894458, 0.000000000000000000, 23.50000000000000000 ) ) ;
#14665 = CARTESIAN_POINT ( 'NONE',  ( 5.007715329123879543E-16, -9.237604307034043671, -9.500000000000000000 ) ) ;
#14666 = ORIENTED_EDGE ( 'NONE', *, *, #29701, .F. ) ;
#14667 = CARTESIAN_POINT ( 'NONE',  ( -60.66241560458681192, 16.25736033771446998, -20.87440278488216094 ) ) ;
#14668 = CARTESIAN_POINT ( 'NONE',  ( -132.9126122820978821, 52.52752252041126724, -71.91483001303755884 ) ) ;
#14669 = ADVANCED_FACE ( 'NONE', ( #50082 ), #54650, .F. ) ;
#14670 = DIRECTION ( 'NONE',  ( -0.000000000000000000, -0.000000000000000000, -1.000000000000000000 ) ) ;
#14671 = CARTESIAN_POINT ( 'NONE',  ( 0.000000000000000000, 0.000000000000000000, -10.00000000000000000 ) ) ;
#14672 = CARTESIAN_POINT ( 'NONE',  ( 69.36287815987336103, 15.27486453472190497, -74.06810378652023985 ) ) ;
#14673 = VERTEX_POINT ( 'NONE', #1542 ) ;
#14674 = ORIENTED_EDGE ( 'NONE', *, *, #61464, .T. ) ;
#14675 = CARTESIAN_POINT ( 'NONE',  ( 116.4569059613810680, 31.86445263670867334, 94.99999999999866418 ) ) ;
#14676 = CARTESIAN_POINT ( 'NONE',  ( -450.6627218934913230, 217.8591479523843475, -111.4497041420117966 ) ) ;
#14677 = DIRECTION ( 'NONE',  ( -0.8118923937861950435, -0.5838071093367415143, 0.000000000000000000 ) ) ;
#14678 = CARTESIAN_POINT ( 'NONE',  ( -51.75347637701212733, 13.82167660501363393, -89.66666266855726519 ) ) ;
#14679 = VECTOR ( 'NONE', #66485, 1000.000000000000000 ) ;
#14680 = CARTESIAN_POINT ( 'NONE',  ( -71.17846906053300415, 20.67346400882179225, 37.42370288375377640 ) ) ;
#14681 = CARTESIAN_POINT ( 'NONE',  ( 445.3372781065086201, 217.8591479523844612, 78.55029585798806124 ) ) ;
#14682 = CARTESIAN_POINT ( 'NONE',  ( 30.12852347772543027, 58.62603998952763362, 133.5802547743875550 ) ) ;
#14683 = LINE ( 'NONE', #15382, #60932 ) ;
#14684 = CARTESIAN_POINT ( 'NONE',  ( 210.1633650091868901, 114.1507944623966608, 58.41051192917949209 ) ) ;
#14685 = EDGE_CURVE ( 'NONE', #65795, #26373, #34852, .T. ) ;
#14686 = ORIENTED_EDGE ( 'NONE', *, *, #13114, .F. ) ;
#14688 = CARTESIAN_POINT ( 'NONE',  ( -109.7643866341847172, 37.89854104106754562, 37.46775542559241501 ) ) ;
#14687 = VECTOR ( 'NONE', #35115, 1000.000000000000000 ) ;
#14689 = ORIENTED_EDGE ( 'NONE', *, *, #25375, .T. ) ;
#14690 = CARTESIAN_POINT ( 'NONE',  ( -178.3015291115128207, 93.08500010736474906, -90.45828512500401075 ) ) ;
#14691 = LINE ( 'NONE', #41086, #41990 ) ;
#14692 = ADVANCED_FACE ( 'NONE', ( #23366 ), #20224, .T. ) ;
#14693 = CARTESIAN_POINT ( 'NONE',  ( -125.0000000000000000, 1.530808498934191561E-14, 5.000000000000000000 ) ) ;
#14694 = CARTESIAN_POINT ( 'NONE',  ( -190.6985136298602015, 109.1272424661243434, -64.50448789838189612 ) ) ;
#14695 = CARTESIAN_POINT ( 'NONE',  ( 34.45972925205165183, 8.830088223935245395, 4.906826754313283523 ) ) ;
#14696 = EDGE_CURVE ( 'NONE', #47003, #39145, #58755, .T. ) ;
#14697 = CARTESIAN_POINT ( 'NONE',  ( -447.6627218934912662, 369.9999999999998295, 113.5502958579880328 ) ) ;
#14698 = CARTESIAN_POINT ( 'NONE',  ( 31.99894129856763314, 7.561773404408294930, 9.342126976674117955 ) ) ;
#14699 = CARTESIAN_POINT ( 'NONE',  ( -12.39770133248888229, 8.241491894828989473, -48.88360719805099563 ) ) ;
#14700 = CIRCLE ( 'NONE', #38239, 5.000000000000004441 ) ;
#14701 = LINE ( 'NONE', #51989, #40508 ) ;
#14702 = EDGE_CURVE ( 'NONE', #46372, #35681, #34952, .T. ) ;
#14703 = ORIENTED_EDGE ( 'NONE', *, *, #39776, .T. ) ;
#14704 = CARTESIAN_POINT ( 'NONE',  ( -122.6790374842361757, 45.60652803413277923, -89.31330210188735919 ) ) ;
#14705 = ORIENTED_EDGE ( 'NONE', *, *, #6319, .T. ) ;
#14706 = LINE ( 'NONE', #2774, #68755 ) ;
#14707 = FILL_AREA_STYLE ('',( #4838 ) ) ;
#14708 = DIRECTION ( 'NONE',  ( -0.000000000000000000, 0.000000000000000000, -1.000000000000000000 ) ) ;
#14709 = DIRECTION ( 'NONE',  ( -0.000000000000000000, -1.000000000000000000, -0.000000000000000000 ) ) ;
#14710 = LINE ( 'NONE', #67846, #24282 ) ;
#14711 = CARTESIAN_POINT ( 'NONE',  ( -97.85576954355160240, 30.58918648956190367, -9.594846923323533616 ) ) ;
#14712 = B_SPLINE_CURVE_WITH_KNOTS ( 'NONE', 3,
 ( #67703, #14233, #18124, #39576, #35693, #35340, #8615, #56437, #2636, #61027, #50477, #56799, #45891, #24100, #29714, #51522, #12854, #18813, #23747, #34308, #55754, #45194, #66670, #3327, #18470, #7915, #39918, #61374, #51174, #45539, #13199, #34664, #29365, #50819, #61716, #13540, #34995, #2991, #24450, #68389, #20880, #25140, #63800, #41989, #26505 ),
 .UNSPECIFIED., .F., .F.,
 ( 4, 2, 2, 1, 2, 2, 2, 2, 2, 2, 2, 2, 2, 2, 2, 2, 2, 2, 2, 2, 2, 2, 4 ),
 ( 0.02348395315094740227, 0.02495010856601298163, 0.02568318627354576958, 0.02641626398107856100, 0.02714934168861135241, 0.02788241939614414036, 0.02934857481120972666, 0.03008165251874251461, 0.03081473022627530950, 0.03228088564134089233, 0.03301396334887368722, 0.03374704105640647517, 0.03521319647147206494, 0.03667935188653764778, 0.03741242959407044266, 0.03814550730160323755, 0.03961166271666881344, 0.04107781813173440322, 0.04254397354679998605, 0.04327705125433277400, 0.04401012896186556889, 0.04547628437693115172, 0.04694243979199673455 ),
 .UNSPECIFIED. ) ;
#14713 = CARTESIAN_POINT ( 'NONE',  ( 150.4722669492348643, 53.65054032737663903, -46.33541081562344033 ) ) ;
#14714 = VERTEX_POINT ( 'NONE', #29666 ) ;
#14715 = DIRECTION ( 'NONE',  ( 0.9998063756620100273, 0.01967768242440602611, -8.868226791111877285E-15 ) ) ;
#14716 = FACE_OUTER_BOUND ( 'NONE', #37553, .T. ) ;
#14717 = CARTESIAN_POINT ( 'NONE',  ( 178.1888264190354505, 77.13727704498029425, -9.948467367157029173 ) ) ;
#14718 = CARTESIAN_POINT ( 'NONE',  ( -102.2801239173131052, 33.91021738430207222, 72.36362509687883460 ) ) ;
#14719 = FACE_OUTER_BOUND ( 'NONE', #15340, .T. ) ;
#14720 = VERTEX_POINT ( 'NONE', #40915 ) ;
#14721 = CARTESIAN_POINT ( 'NONE',  ( -175.1895962157337010, 90.99110972060690017, -76.27797459989902507 ) ) ;
#14722 = CARTESIAN_POINT ( 'NONE',  ( -0.3249717932738303561, 6.518578686837484426, -15.58535181265489022 ) ) ;
#14723 = EDGE_CURVE ( 'NONE', #35609, #27646, #37092, .T. ) ;
#14724 = CARTESIAN_POINT ( 'NONE',  ( 112.1012908502484606, 29.75117929736499889, 29.84123205385900590 ) ) ;
#14725 = CARTESIAN_POINT ( 'NONE',  ( -67.57266509268116295, -32.54128043381741975, 43.58025477438756212 ) ) ;
#14726 = EDGE_LOOP ( 'NONE', ( #44020, #2351 ) ) ;
#14727 = CARTESIAN_POINT ( 'NONE',  ( 197.1980152960109933, 96.59350208824299955, 37.04504252498942662 ) ) ;
#14728 = CARTESIAN_POINT ( 'NONE',  ( 115.0454575488273576, 31.16784721673998249, -76.03284390000987969 ) ) ;
#14729 = DIRECTION ( 'NONE',  ( 0.000000000000000000, 0.000000000000000000, 1.000000000000000000 ) ) ;
#14730 = CARTESIAN_POINT ( 'NONE',  ( 187.0314709137215345, 84.83273891797912825, -92.84016220200550151 ) ) ;
#14731 = CARTESIAN_POINT ( 'NONE',  ( 4.174999999999999822, 0.000000000000000000, -0.5776712190230133270 ) ) ;
#14732 = AXIS2_PLACEMENT_3D ( 'NONE', #38682, #34111, #7380 ) ;
#14733 = VECTOR ( 'NONE', #50808, 1000.000000000000000 ) ;
#14734 = EDGE_LOOP ( 'NONE', ( #19199, #31051, #17911, #33153 ) ) ;
#14735 = DIRECTION ( 'NONE',  ( -0.000000000000000000, -0.000000000000000000, 1.000000000000000000 ) ) ;
#14736 = AXIS2_PLACEMENT_3D ( 'NONE', #51853, #19493, #68048 ) ;
#14737 = VECTOR ( 'NONE', #49017, 1000.000000000000114 ) ;
#14738 = ORIENTED_EDGE ( 'NONE', *, *, #18028, .F. ) ;
#14739 = CARTESIAN_POINT ( 'NONE',  ( -105.8768181937898873, 34.64545164169051361, -35.91624400628371916 ) ) ;
#14740 = CARTESIAN_POINT ( 'NONE',  ( 140.8375554551808477, 45.80242115643797973, 93.46421066599228311 ) ) ;
#14742 = ORIENTED_EDGE ( 'NONE', *, *, #65215, .T. ) ;
#14741 = CARTESIAN_POINT ( 'NONE',  ( 151.1827182658834090, 54.16800928478853194, 5.944559561786584290 ) ) ;
#14743 = FACE_BOUND ( 'NONE', #26083, .T. ) ;
#14744 = AXIS2_PLACEMENT_3D ( 'NONE', #51554, #67390, #3019 ) ;
#14745 = CARTESIAN_POINT ( 'NONE',  ( 46.66904755831212981, 15.55634918610394379, 85.00100000000000477 ) ) ;
#14746 = B_SPLINE_CURVE_WITH_KNOTS ( 'NONE', 3,
 ( #41774, #69522, #58623, #63913, #15727, #42789, #53692, #37176, #20309, #37520, #4145, #10438, #68504, #10786, #63230, #58972, #32259, #36496, #57947, #5512, #21686, #9767, #31229, #43137, #64607, #52660, #20655, #16416, #25944, #47376, #52322, #68831, #42115, #63572, #38563, #38217, #54380, #32937 ),
 .UNSPECIFIED., .F., .F.,
 ( 4, 2, 2, 2, 2, 2, 2, 2, 2, 2, 2, 2, 2, 2, 2, 2, 2, 2, 4 ),
 ( 1.561251128379126385E-17, 0.001559859933532253048, 0.003119719867064490483, 0.004679579800596727485, 0.006239439734128965354, 0.007799299667661202355, 0.008579229634427315218, 0.009359159601193428948, 0.01091901953472565120, 0.01169894950149175800, 0.01247887946825786652, 0.01403873940179008704, 0.01559859933532230583, 0.01715845926885452288, 0.01871831920238674341, 0.02027817913591895699, 0.02183803906945117751, 0.02339789900298339109, 0.02495775893651561161 ),
 .UNSPECIFIED. ) ;
#14747 = CARTESIAN_POINT ( 'NONE',  ( 29.69502258243432635, -57.82046033912835270, 170.0000000000000000 ) ) ;
#14748 = ADVANCED_FACE ( 'NONE', ( #8217, #8570 ), #13832, .T. ) ;
#14749 = VERTEX_POINT ( 'NONE', #18770 ) ;
#14750 = DIRECTION ( 'NONE',  ( 0.000000000000000000, 0.000000000000000000, 1.000000000000000000 ) ) ;
#14751 = ADVANCED_FACE ( 'NONE', ( #13493 ), #30018, .F. ) ;
#14752 = EDGE_CURVE ( 'NONE', #9108, #66548, #3289, .T. ) ;
#14753 = CARTESIAN_POINT ( 'NONE',  ( -447.6627218934913230, 399.9999999999997726, 83.55029585798818914 ) ) ;
#14754 = VERTEX_POINT ( 'NONE', #19811 ) ;
#14755 = CARTESIAN_POINT ( 'NONE',  ( 139.6203063421347395, 45.01495791936840618, 59.03001518722842889 ) ) ;
#14756 = EDGE_CURVE ( 'NONE', #22171, #66403, #33784, .T. ) ;
#14757 = CARTESIAN_POINT ( 'NONE',  ( 444.4083459183740956, 365.0000000000001137, -143.5207719538773006 ) ) ;
#14758 = DIRECTION ( 'NONE',  ( -1.000000000000000000, 0.000000000000000000, 0.000000000000000000 ) ) ;
#14759 = CARTESIAN_POINT ( 'NONE',  ( 88.52077179907878701, 21.14145351760140557, 44.47362131126318729 ) ) ;
#14760 = VERTEX_POINT ( 'NONE', #54112 ) ;
#14761 = CARTESIAN_POINT ( 'NONE',  ( 39.40195752203891999, 9.424259417798145577, 18.06928371549960133 ) ) ;
#14762 = EDGE_LOOP ( 'NONE', ( #54071, #67113, #43671, #2566 ) ) ;
#14763 = CARTESIAN_POINT ( 'NONE',  ( 150.2941978382489197, 53.52137138947625061, -18.97662088534088198 ) ) ;
#14764 = CARTESIAN_POINT ( 'NONE',  ( -4.999999999999936939, 31.11269837220806167, 85.00100000000000477 ) ) ;
#14765 = CARTESIAN_POINT ( 'NONE',  ( 197.6319840686292082, -170.0000000000000000, -95.00000000000133582 ) ) ;
#14766 = CARTESIAN_POINT ( 'NONE',  ( -152.2964402771109462, 66.58174574061955298, -62.19164853688251071 ) ) ;
#14767 = CARTESIAN_POINT ( 'NONE',  ( 59.84823624668899811, 11.96014623718603964, 84.19572422589860139 ) ) ;
#14768 = PLANE ( 'NONE',  #7834 ) ;
#14769 = CARTESIAN_POINT ( 'NONE',  ( 212.0739503583954217, 117.0412199804969617, -45.22451888985740709 ) ) ;
#14770 = CARTESIAN_POINT ( 'NONE',  ( 176.4367926094705581, 74.03315361639849357, 4.072456122556812552 ) ) ;
#14771 = ORIENTED_EDGE ( 'NONE', *, *, #36287, .T. ) ;
#14772 = CARTESIAN_POINT ( 'NONE',  ( 24.34427655538949509, 5.688250960946272805, 0.000000000000000000 ) ) ;
#14773 = ORIENTED_EDGE ( 'NONE', *, *, #56797, .F. ) ;
#14774 = CARTESIAN_POINT ( 'NONE',  ( -76.33235143960693847, 22.51916353135074189, 71.89429839980979864 ) ) ;
#14775 = EDGE_CURVE ( 'NONE', #17657, #20172, #10917, .T. ) ;
#14776 = CARTESIAN_POINT ( 'NONE',  ( 63.01563776193091826, 12.67277567978498709, -62.56524142263340593 ) ) ;
#14777 = EDGE_CURVE ( 'NONE', #63181, #41760, #33036, .T. ) ;
#14778 = LINE ( 'NONE', #25358, #171 ) ;
#14779 = CARTESIAN_POINT ( 'NONE',  ( 99.71998884745383407, 190.0000000000000000, 7.478223336038896996 ) ) ;
#14780 = CARTESIAN_POINT ( 'NONE',  ( 17.72748965151693668, 7.577488030789625739, 44.76384774945338307 ) ) ;
#14781 = CARTESIAN_POINT ( 'NONE',  ( -104.1225399044495816, 34.86084180570100699, -22.94399755735298996 ) ) ;
#14782 = VERTEX_POINT ( 'NONE', #54826 ) ;
#14783 = AXIS2_PLACEMENT_3D ( 'NONE', #53813, #49582, #27094 ) ;
#14784 = CARTESIAN_POINT ( 'NONE',  ( -15.47041015649658391, 73.39774458108210808, 133.5802547743875550 ) ) ;
#14785 = CARTESIAN_POINT ( 'NONE',  ( 197.6319840686292082, 97.13072366387987699, -95.00000000000133582 ) ) ;
#14786 = ORIENTED_EDGE ( 'NONE', *, *, #69567, .T. ) ;
#14787 = ORIENTED_EDGE ( 'NONE', *, *, #4617, .T. ) ;
#14788 = CARTESIAN_POINT ( 'NONE',  ( -8.000000000000000000, -0.7805016046291012310, 1.011357339021634605E-15 ) ) ;
#14789 = CARTESIAN_POINT ( 'NONE',  ( 0.000000000000000000, 0.000000000000000000, 41.38025477438755928 ) ) ;
#14791 = CARTESIAN_POINT ( 'NONE',  ( 177.0024338932394130, 74.57605685449964028, -10.57210100736196878 ) ) ;
#14790 = AXIS2_PLACEMENT_3D ( 'NONE', #30257, #24641, #63650 ) ;
#14792 = SURFACE_STYLE_FILL_AREA ( #62650 ) ;
#14793 = CARTESIAN_POINT ( 'NONE',  ( -143.7151964745329451, 59.41799441280381444, 6.605001292783195588 ) ) ;
#14794 = VECTOR ( 'NONE', #8478, 999.9999999999998863 ) ;
#14795 = VERTEX_POINT ( 'NONE', #6298 ) ;
#14796 = CARTESIAN_POINT ( 'NONE',  ( -2.116120943112232755, 74.98056102853672655, 43.58025477438756212 ) ) ;
#14797 = ORIENTED_EDGE ( 'NONE', *, *, #15378, .F. ) ;
#14798 = CARTESIAN_POINT ( 'NONE',  ( 210.9747454890631388, 115.3673079504855536, 13.97618168240338399 ) ) ;
#14799 = CARTESIAN_POINT ( 'NONE',  ( 11.20486344102687504, 7.403248964808828880, 70.31616484736908035 ) ) ;
#14800 = FACE_BOUND ( 'NONE', #38343, .T. ) ;
#14801 = ORIENTED_EDGE ( 'NONE', *, *, #6009, .T. ) ;
#14802 = ORIENTED_EDGE ( 'NONE', *, *, #60674, .F. ) ;
#14803 = DIRECTION ( 'NONE',  ( -0.000000000000000000, 1.000000000000000000, -0.000000000000000000 ) ) ;
#14804 = CARTESIAN_POINT ( 'NONE',  ( -118.3864719359396389, 42.92356051160688679, 91.74072687414530947 ) ) ;
#14805 = CARTESIAN_POINT ( 'NONE',  ( -166.2028657618941452, 79.74389853943294781, -12.45684997849616771 ) ) ;
#14806 = FACE_OUTER_BOUND ( 'NONE', #35230, .T. ) ;
#14807 = CARTESIAN_POINT ( 'NONE',  ( 22.57231971038877205, 6.812631029037583552, 94.41881611565530363 ) ) ;
#14808 = CARTESIAN_POINT ( 'NONE',  ( 23.28635475458051118, 7.864714260171793647, 91.57214863357140189 ) ) ;
#14809 = ORIENTED_EDGE ( 'NONE', *, *, #48676, .T. ) ;
#14810 = DIRECTION ( 'NONE',  ( -0.000000000000000000, 1.000000000000000000, -0.000000000000000000 ) ) ;
#14811 = CARTESIAN_POINT ( 'NONE',  ( -96.43148989374459745, 29.90755650959363976, 69.58523154106214292 ) ) ;
#14812 = ORIENTED_EDGE ( 'NONE', *, *, #29371, .T. ) ;
#14813 = CARTESIAN_POINT ( 'NONE',  ( -84.54326985437106146, 24.64760594531652771, 15.75942825447480189 ) ) ;
#14814 = ORIENTED_EDGE ( 'NONE', *, *, #16853, .F. ) ;
#14815 = CARTESIAN_POINT ( 'NONE',  ( -31.43908319763709969, 10.61114334766717171, -62.16174795566551836 ) ) ;
#14816 = ORIENTED_EDGE ( 'NONE', *, *, #13505, .T. ) ;
#14817 = AXIS2_PLACEMENT_3D ( 'NONE', #9037, #51934, #2718 ) ;
#14818 = ORIENTED_EDGE ( 'NONE', *, *, #20575, .T. ) ;
#14819 = CARTESIAN_POINT ( 'NONE',  ( 15.78827728214693416, 6.500811158483284835, -50.51894409868581448 ) ) ;
#14820 = DIRECTION ( 'NONE',  ( -0.6579387259397028176, -0.7530714660036196273, 5.102127870520020458E-18 ) ) ;
#14821 = CARTESIAN_POINT ( 'NONE',  ( 132.0582325211145474, 40.34869848118185587, 71.15012554800902933 ) ) ;
#14822 = VECTOR ( 'NONE', #60512, 1000.000000000000000 ) ;
#14823 = ORIENTED_EDGE ( 'NONE', *, *, #45127, .F. ) ;
#14824 = PRODUCT_DEFINITION_SHAPE ( 'NONE', 'NONE',  #69629 ) ;
#14825 = EDGE_CURVE ( 'NONE', #13533, #26941, #38304, .T. ) ;
#14826 = VECTOR ( 'NONE', #47529, 1000.000000000000000 ) ;
#14827 = AXIS2_PLACEMENT_3D ( 'NONE', #34032, #29103, #66407 ) ;
#14828 = CARTESIAN_POINT ( 'NONE',  ( -28.33384212282240000, 9.102119872907532994, 84.57104976863398349 ) ) ;
#14829 = CARTESIAN_POINT ( 'NONE',  ( 179.4074606910091347, 78.34362448405028090, -63.20884701633242031 ) ) ;
#14830 = EDGE_CURVE ( 'NONE', #10200, #16148, #22129, .T. ) ;
#14831 = CARTESIAN_POINT ( 'NONE',  ( -31.43908319763710679, -170.0000000000000000, 18.37190381572551701 ) ) ;
#14832 = CARTESIAN_POINT ( 'NONE',  ( 104.7034219878852213, 26.40210929103716708, -48.50262205611462463 ) ) ;
#14833 = AXIS2_PLACEMENT_3D ( 'NONE', #48532, #14820, #36294 ) ;
#14834 = CARTESIAN_POINT ( 'NONE',  ( 80.16761386260783695, 18.37011649821943138, -47.16167432286557215 ) ) ;
#14835 = CARTESIAN_POINT ( 'NONE',  ( -149.5074843970970733, 65.50121172469317798, -61.65738112195564469 ) ) ;
#14836 = EDGE_LOOP ( 'NONE', ( #57828, #66420, #40388, #21025, #22944 ) ) ;
#14837 = EDGE_CURVE ( 'NONE', #3230, #19006, #4655, .T. ) ;
#14838 = CLOSED_SHELL ( 'NONE', ( #11485, #21512, #53202, #27130, #13811, #16297 ) ) ;
#14839 = FACE_OUTER_BOUND ( 'NONE', #54551, .T. ) ;
#14840 = CARTESIAN_POINT ( 'NONE',  ( -86.11230725916328765, 26.39026888680168526, -70.49370428031920710 ) ) ;
#14841 = CARTESIAN_POINT ( 'NONE',  ( -1.000266010268695327, 6.542200531770547833, -93.38246921637555431 ) ) ;
#14842 = FACE_OUTER_BOUND ( 'NONE', #32364, .T. ) ;
#14843 = DIRECTION ( 'NONE',  ( 1.000000000000000000, 0.000000000000000000, 0.000000000000000000 ) ) ;
#14844 = CARTESIAN_POINT ( 'NONE',  ( 126.6395826915640015, 37.23416510613628816, 8.108414546062657990 ) ) ;
#14845 = CARTESIAN_POINT ( 'NONE',  ( 32.12337157895397866, 7.574134358465434147, -95.00000000000133582 ) ) ;
#14846 = CARTESIAN_POINT ( 'NONE',  ( 0.000000000000000000, 26.99999999999999645, 0.000000000000000000 ) ) ;
#14847 = B_SPLINE_CURVE_WITH_KNOTS ( 'NONE', 3,
 ( #24766, #3305, #62395, #12831, #45869, #18445, #29689, #13854, #51155, #35315, #67682, #51504, #39900, #19130, #56776, #34974, #55733, #8594, #56080, #46550, #34287, #40249, #19474, #18789, #30381, #2967, #23724, #24428, #30043, #51833, #50457, #62038, #40934, #61695, #29016, #3645, #68031, #39556, #61007, #2278, #13177, #34645, #7896, #29343, #50797 ),
 .UNSPECIFIED., .F., .F.,
 ( 4, 2, 2, 1, 2, 2, 2, 2, 2, 2, 2, 2, 2, 2, 2, 2, 2, 2, 2, 2, 2, 2, 4 ),
 ( 0.02348395315094738839, 0.02495010856601294694, 0.02568318627354572795, 0.02641626398107850549, 0.02714934168861128302, 0.02788241939614406056, 0.02934857481120962258, 0.03008165251874240706, 0.03081473022627519501, 0.03228088564134074662, 0.03301396334887353456, 0.03374704105640634333, 0.03521319647147195392, 0.03667935188653756451, 0.03741242959407034552, 0.03814550730160313347, 0.03961166271666874406, 0.04107781813173435465, 0.04254397354679996524, 0.04327705125433275318, 0.04401012896186554807, 0.04547628437693113090, 0.04694243979199672068 ),
 .UNSPECIFIED. ) ;
#14848 = CARTESIAN_POINT ( 'NONE',  ( 208.9585401441656245, 114.1617785893844257, 42.89634414365027482 ) ) ;
#14849 = CARTESIAN_POINT ( 'NONE',  ( -74.17694007417655655, 20.66176641130876845, -63.43242567744339055 ) ) ;
#14850 = CARTESIAN_POINT ( 'NONE',  ( -109.5142642360664098, 36.61018064014776741, 35.97134868343648861 ) ) ;
#14851 = ORIENTED_EDGE ( 'NONE', *, *, #42638, .F. ) ;
#14852 = CONTEXT_DEPENDENT_SHAPE_REPRESENTATION ( #65582, #24368 ) ;
#14853 = CARTESIAN_POINT ( 'NONE',  ( -57.24869976356938395, 16.32563047877252416, 84.32812304263042336 ) ) ;
#14854 = ORIENTED_EDGE ( 'NONE', *, *, #33936, .F. ) ;
#14855 = PLANE ( 'NONE',  #29532 ) ;
#14856 = ORIENTED_EDGE ( 'NONE', *, *, #65352, .F. ) ;
#14857 = EDGE_CURVE ( 'NONE', #57612, #4893, #15216, .T. ) ;
#14858 = CARTESIAN_POINT ( 'NONE',  ( 0.000000000000000000, 190.0000000000000000, 2.000000000000000000 ) ) ;
#14859 = DIRECTION ( 'NONE',  ( -1.000000000000000000, 0.000000000000000000, 0.000000000000000000 ) ) ;
#14860 = DIRECTION ( 'NONE',  ( 1.387778780781445676E-16, -1.000000000000000000, -4.294171409582122931E-32 ) ) ;
#14861 = FACE_OUTER_BOUND ( 'NONE', #12926, .T. ) ;
#14862 = CARTESIAN_POINT ( 'NONE',  ( 139.6326990672751265, 46.22017155708125813, -48.31381116572497803 ) ) ;
#14863 = CARTESIAN_POINT ( 'NONE',  ( 206.0459564151325083, 109.9423578521132328, -90.10578531043864814 ) ) ;
#14864 = CARTESIAN_POINT ( 'NONE',  ( 46.66904755831210139, -9.150666335777657423E-14, 0.000000000000000000 ) ) ;
#14865 = PLANE ( 'NONE',  #58902 ) ;
#14866 = LINE ( 'NONE', #15907, #32968 ) ;
#14867 = ORIENTED_EDGE ( 'NONE', *, *, #43178, .T. ) ;
#14868 = ORIENTED_EDGE ( 'NONE', *, *, #12499, .F. ) ;
#14869 = CARTESIAN_POINT ( 'NONE',  ( 179.2582403890615979, 78.19797385420241653, 83.21752769010527118 ) ) ;
#14870 = SURFACE_STYLE_FILL_AREA ( #35991 ) ;
#14871 = CARTESIAN_POINT ( 'NONE',  ( -30.95355748062275936, 9.511738996772322707, -77.16174795566556099 ) ) ;
#14872 = UNCERTAINTY_MEASURE_WITH_UNIT (LENGTH_MEASURE( 1.000000000000000082E-05 ), #5288, 'distance_accuracy_value', 'NONE');
#14873 = CIRCLE ( 'NONE', #32802, 65.36598343705435354 ) ;
#14874 = CARTESIAN_POINT ( 'NONE',  ( 26.11269837220800127, -31.11269837220812562, 85.00100000000000477 ) ) ;
#14875 = CARTESIAN_POINT ( 'NONE',  ( -7.825402957745087207, 7.899365992529248537, -62.26262132240749736 ) ) ;
#14876 = LINE ( 'NONE', #36696, #13274 ) ;
#14877 = CARTESIAN_POINT ( 'NONE',  ( 173.6020601204681952, 71.36108012062130967, -69.97250781112231266 ) ) ;
#14878 = AXIS2_PLACEMENT_3D ( 'NONE', #10511, #5244, #48134 ) ;
#14879 = CARTESIAN_POINT ( 'NONE',  ( 0.000000000000000000, 0.000000000000000000, 41.38025477438755928 ) ) ;
#14880 = CARTESIAN_POINT ( 'NONE',  ( -30.00000000000000355, -30.00000000000000355, 12.00000000000000000 ) ) ;
#14881 = CARTESIAN_POINT ( 'NONE',  ( -29.03891846981456126, 10.22741474064058487, 57.43857379582767209 ) ) ;
#14882 = LINE ( 'NONE', #35663, #57635 ) ;
#14883 = CARTESIAN_POINT ( 'NONE',  ( -47.95468448182523247, 12.89252559348046212, 67.09685781612688515 ) ) ;
#14884 = VECTOR ( 'NONE', #9438, 1000.000000000000000 ) ;
#14885 = EDGE_LOOP ( 'NONE', ( #58747, #65893 ) ) ;
#14886 = DIRECTION ( 'NONE',  ( -5.096990367256705246E-18, 2.289061013374613071E-19, -1.000000000000000000 ) ) ;
#14887 = CYLINDRICAL_SURFACE ( 'NONE', #6948, 4.999999999999997335 ) ;
#14888 = B_SPLINE_CURVE_WITH_KNOTS ( 'NONE', 3,
 ( #43489, #21346, #10789, #64964 ),
 .UNSPECIFIED., .F., .F.,
 ( 4, 4 ),
 ( 0.1259919275528357807, 0.1829744153748745217 ),
 .UNSPECIFIED. ) ;
#14889 = DIRECTION ( 'NONE',  ( 0.000000000000000000, 0.000000000000000000, 1.000000000000000000 ) ) ;
#14890 = CARTESIAN_POINT ( 'NONE',  ( -109.4995148930278077, 37.75156937139181679, -71.45788426471575860 ) ) ;
#14891 = CARTESIAN_POINT ( 'NONE',  ( 7.484861546145031852, 64.56761454192836425, 170.0000000000000000 ) ) ;
#14892 = CARTESIAN_POINT ( 'NONE',  ( 133.8566784816069060, 42.60093787723652525, 44.51034083899536142 ) ) ;
#14893 = PLANE ( 'NONE',  #15375 ) ;
#14894 = EDGE_CURVE ( 'NONE', #8769, #20715, #32623, .T. ) ;
#14895 = VERTEX_POINT ( 'NONE', #69011 ) ;
#14896 = CYLINDRICAL_SURFACE ( 'NONE', #30297, 7.500000000000013323 ) ;
#14897 = CARTESIAN_POINT ( 'NONE',  ( -61.86403937395562735, 16.61416349803656445, 67.81112795023058482 ) ) ;
#14898 = ORIENTED_EDGE ( 'NONE', *, *, #58658, .F. ) ;
#14899 = ORIENTED_EDGE ( 'NONE', *, *, #67508, .F. ) ;
#14900 = CARTESIAN_POINT ( 'NONE',  ( 46.88995144419296679, 10.52126979626132197, 90.56259000874159426 ) ) ;
#14901 = CARTESIAN_POINT ( 'NONE',  ( -175.1920326508033270, 89.46239303019292777, -76.27753814462546700 ) ) ;
#14902 = CARTESIAN_POINT ( 'NONE',  ( 55.46196446482129261, -34.59309596431295830, 41.38025477438755928 ) ) ;
#14903 = EDGE_LOOP ( 'NONE', ( #20656, #40521, #54008, #48187 ) ) ;
#14904 = DIRECTION ( 'NONE',  ( -0.000000000000000000, 1.000000000000000000, -0.000000000000000000 ) ) ;
#14905 = DIRECTION ( 'NONE',  ( -1.000000000000000000, 0.000000000000000000, 0.000000000000000000 ) ) ;
#14906 = CARTESIAN_POINT ( 'NONE',  ( 55.57634120535661992, 12.09544293553729943, -42.23651943899194805 ) ) ;
#14907 = CARTESIAN_POINT ( 'NONE',  ( 16.83496171716143408, -55.85776949775602418, 27.58472315868180402 ) ) ;
#14908 = CARTESIAN_POINT ( 'NONE',  ( 9.737557066527559257, 188.0000000000000000, 2.275957463600584596 ) ) ;
#14909 = CARTESIAN_POINT ( 'NONE',  ( 93.33480479917541572, 21.81892021443993812, 40.60918334494109416 ) ) ;
#14910 = EDGE_CURVE ( 'NONE', #46954, #37858, #33741, .T. ) ;
#14911 = ORIENTED_EDGE ( 'NONE', *, *, #48872, .T. ) ;
#14912 = EDGE_CURVE ( 'NONE', #29587, #20616, #57038, .T. ) ;
#14913 = CARTESIAN_POINT ( 'NONE',  ( -15.55634918610408945, -31.11269837220804035, 0.000000000000000000 ) ) ;
#14914 = CARTESIAN_POINT ( 'NONE',  ( 8.528421445032394743, 6.376778749352037146, 62.41374088788820274 ) ) ;
#14915 = CARTESIAN_POINT ( 'NONE',  ( -25.07901552294942960, 9.649193085547780768, 41.69897551811279612 ) ) ;
#14916 = CARTESIAN_POINT ( 'NONE',  ( 197.6329787101073805, 98.74106466892202150, 34.17182954918762050 ) ) ;
#14917 = PLANE ( 'NONE',  #17390 ) ;
#14919 = ORIENTED_EDGE ( 'NONE', *, *, #45838, .T. ) ;
#14918 = CARTESIAN_POINT ( 'NONE',  ( 8.942470798084043437, 23.47701018505912174, 0.000000000000000000 ) ) ;
#14920 = DIRECTION ( 'NONE',  ( -0.6910626489868580968, -0.7227948638273978821, 0.000000000000000000 ) ) ;
#14921 = EDGE_LOOP ( 'NONE', ( #29253, #33052, #2062, #64200 ) ) ;
#14922 = CIRCLE ( 'NONE', #23920, 65.00000000000000000 ) ;
#14923 = ADVANCED_FACE ( 'NONE', ( #23189 ), #62197, .F. ) ;
#14924 = ORIENTED_EDGE ( 'NONE', *, *, #63378, .T. ) ;
#14925 = AXIS2_PLACEMENT_3D ( 'NONE', #580, #32930, #5843 ) ;
#14926 =( LENGTH_UNIT ( ) NAMED_UNIT ( * ) SI_UNIT ( .MILLI., .METRE. ) );
#14927 = CARTESIAN_POINT ( 'NONE',  ( 61.91366885787816443, -28.42865614898931881, 41.38025477438755928 ) ) ;
#14928 = CARTESIAN_POINT ( 'NONE',  ( 197.3707490726349363, 96.80690576410100334, -69.03806240719120524 ) ) ;
#14929 = CARTESIAN_POINT ( 'NONE',  ( -38.93938005333174601, 11.96888249046459940, 64.80069294567751115 ) ) ;
#14930 = AXIS2_PLACEMENT_3D ( 'NONE', #47917, #32103, #25462 ) ;
#14931 = CARTESIAN_POINT ( 'NONE',  ( -118.6288898061518466, 41.89286798341290563, 63.08229067355227215 ) ) ;
#14932 = CARTESIAN_POINT ( 'NONE',  ( -82.93126516400697312, 25.07709093823493518, -21.94504152255926144 ) ) ;
#14933 = CARTESIAN_POINT ( 'NONE',  ( -196.7348448768811409, -170.0000000000000000, -15.26653320754434162 ) ) ;
#14934 = VECTOR ( 'NONE', #19472, 1000.000000000000000 ) ;
#14935 = DIRECTION ( 'NONE',  ( 0.000000000000000000, -1.000000000000000000, 0.000000000000000000 ) ) ;
#14936 = ORIENTED_EDGE ( 'NONE', *, *, #1490, .F. ) ;
#14937 = EDGE_LOOP ( 'NONE', ( #40297, #12748, #25724, #2583 ) ) ;
#14938 = EDGE_CURVE ( 'NONE', #57624, #60956, #12630, .T. ) ;
#14939 = CARTESIAN_POINT ( 'NONE',  ( -17.50000000000002842, -18.06806526123148160, 380.0000000000000000 ) ) ;
#14940 = CARTESIAN_POINT ( 'NONE',  ( -86.16504208171676282, 26.41251233979373936, -43.14513425734210017 ) ) ;
#14941 = AXIS2_PLACEMENT_3D ( 'NONE', #17722, #6467, #34251 ) ;
#14942 = CARTESIAN_POINT ( 'NONE',  ( 106.3034350612047518, 27.10143568295973182, 84.40989449007727785 ) ) ;
#14944 = EDGE_CURVE ( 'NONE', #31811, #12136, #2313, .T. ) ;
#14943 = DIRECTION ( 'NONE',  ( 0.000000000000000000, 0.000000000000000000, 1.000000000000000000 ) ) ;
#14945 = ADVANCED_FACE ( 'NONE', ( #44635 ), #2423, .F. ) ;
#14946 = CARTESIAN_POINT ( 'NONE',  ( 0.000000000000000000, 0.000000000000000000, 0.000000000000000000 ) ) ;
#14947 = PLANE ( 'NONE',  #43799 ) ;
#14948 = CARTESIAN_POINT ( 'NONE',  ( 164.8942204024298803, 63.66138186734712434, -69.36631708222795112 ) ) ;
#14949 = ORIENTED_EDGE ( 'NONE', *, *, #16038, .T. ) ;
#14950 = VERTEX_POINT ( 'NONE', #17906 ) ;
#14951 = VERTEX_POINT ( 'NONE', #13330 ) ;
#14952 = LINE ( 'NONE', #36416, #57759 ) ;
#14953 = CARTESIAN_POINT ( 'NONE',  ( -86.10361028793438720, 25.29528064050658287, 63.76107057542620993 ) ) ;
#14954 = CARTESIAN_POINT ( 'NONE',  ( 105.2224576781852363, 26.62754899994121516, -91.52473545953954215 ) ) ;
#14955 = CARTESIAN_POINT ( 'NONE',  ( -35.17296606710973350, 11.25626711331310403, -76.18484644730783373 ) ) ;
#14956 = CARTESIAN_POINT ( 'NONE',  ( -26.69131247781221106, -59.26697088777007849, 170.0000000000000000 ) ) ;
#14957 = CARTESIAN_POINT ( 'NONE',  ( 32.28603806442400526, 7.590310383548732887, 61.83839758995276981 ) ) ;
#14958 = CARTESIAN_POINT ( 'NONE',  ( 46.40453471432315524, 9.423871119279747077, 93.80938164509879584 ) ) ;
#14959 =( NAMED_UNIT ( * ) PLANE_ANGLE_UNIT ( ) SI_UNIT ( $, .RADIAN. ) );
#14960 = CARTESIAN_POINT ( 'NONE',  ( 17.72748965151693668, 7.577488030789625739, 17.91929715898970699 ) ) ;
#14961 = CARTESIAN_POINT ( 'NONE',  ( 185.1647878987786555, 82.82967084668430857, 57.34492923270315856 ) ) ;
#14962 = DIRECTION ( 'NONE',  ( -0.000000000000000000, -0.000000000000000000, -1.000000000000000000 ) ) ;
#14963 = CYLINDRICAL_SURFACE ( 'NONE', #24196, 5.000000000000004441 ) ;
#14964 = CARTESIAN_POINT ( 'NONE',  ( 129.1137093889808796, 38.63348691920625555, -22.49364613101846899 ) ) ;
#14965 = CARTESIAN_POINT ( 'NONE',  ( 21.43750346857337874, 7.754771113113081427, -11.21701564101427451 ) ) ;
#14966 = CARTESIAN_POINT ( 'NONE',  ( 198.2545923567585078, 97.90679023593570207, 59.70290751491250347 ) ) ;
#14967 = MECHANICAL_DESIGN_GEOMETRIC_PRESENTATION_REPRESENTATION (  '', ( #11587 ), #58787 ) ;
#14968 = ORIENTED_EDGE ( 'NONE', *, *, #13583, .F. ) ;
#14970 = CARTESIAN_POINT ( 'NONE',  ( 188.5645326065591405, 86.51153908883291876, 9.344684421083345072 ) ) ;
#14969 = AXIS2_PLACEMENT_3D ( 'NONE', #38747, #16584, #44355 ) ;
#14971 = APPLICATION_PROTOCOL_DEFINITION ( 'draft international standard', 'automotive_design', 1998, #9390 ) ;
#14972 = CARTESIAN_POINT ( 'NONE',  ( 173.6020601204682237, 71.36108012062136652, 37.40569455073241301 ) ) ;
#14973 = DIRECTION ( 'NONE',  ( -0.000000000000000000, 0.000000000000000000, 1.000000000000000000 ) ) ;
#14974 = CARTESIAN_POINT ( 'NONE',  ( -106.6711220790662935, 36.20923238211248929, -48.59962218315158822 ) ) ;
#14975 = ITEM_DEFINED_TRANSFORMATION ( 'NONE', 'NONE', #50136,  #66832 ) ;
#14976 = CARTESIAN_POINT ( 'NONE',  ( 187.5165082312810512, 86.85340440641662951, -47.59062793446263839 ) ) ;
#14977 = ORIENTED_EDGE ( 'NONE', *, *, #34495, .T. ) ;
#14978 = VECTOR ( 'NONE', #24229, 1000.000000000000000 ) ;
#14979 = EDGE_CURVE ( 'NONE', #5170, #3478, #14700, .T. ) ;
#14980 = ORIENTED_EDGE ( 'NONE', *, *, #48905, .T. ) ;
#14981 = VECTOR ( 'NONE', #3529, 1000.000000000000114 ) ;
#14982 = CARTESIAN_POINT ( 'NONE',  ( -24.39249304643438521, 60.24953346690454481, 170.0000000000000000 ) ) ;
#14983 = AXIS2_PLACEMENT_3D ( 'NONE', #49648, #53877, #21533 ) ;
#14984 = CARTESIAN_POINT ( 'NONE',  ( 173.8971638285193819, 71.63521281801094176, 92.67731212905682980 ) ) ;
#14985 = VERTEX_POINT ( 'NONE', #45325 ) ;
#14986 = EDGE_CURVE ( 'NONE', #2052, #925, #18948, .T. ) ;
#14987 = AXIS2_PLACEMENT_3D ( 'NONE', #620, #60405, #60043 ) ;
#14988 = CARTESIAN_POINT ( 'NONE',  ( 116.6457744947906860, 31.95847117670279403, 60.04196747368758480 ) ) ;
#14989 = ORIENTED_EDGE ( 'NONE', *, *, #7235, .T. ) ;
#14990 = CARTESIAN_POINT ( 'NONE',  ( 44.98017923036987042, -25.41829121023151927, 26.66469066592268433 ) ) ;
#14991 = DIRECTION ( 'NONE',  ( -0.000000000000000000, -0.000000000000000000, 1.000000000000000000 ) ) ;
#14992 = CARTESIAN_POINT ( 'NONE',  ( 10.55634918610396511, -41.66904755831214402, 85.00100000000000477 ) ) ;
#14993 = AXIS2_PLACEMENT_3D ( 'NONE', #62, #15218, #42966 ) ;
#14994 = PLANE ( 'NONE',  #56190 ) ;
#14995 = DIRECTION ( 'NONE',  ( 1.000000000000000000, 0.000000000000000000, 0.000000000000000000 ) ) ;
#14997 = ORIENTED_EDGE ( 'NONE', *, *, #45127, .T. ) ;
#14996 = CYLINDRICAL_SURFACE ( 'NONE', #6135, 60.00000000000000000 ) ;
#14998 = ADVANCED_FACE ( 'NONE', ( #61511, #8398, #60802 ), #50261, .F. ) ;
#14999 = DIRECTION ( 'NONE',  ( 0.000000000000000000, 1.000000000000000000, 0.000000000000000000 ) ) ;
#15000 = ORIENTED_EDGE ( 'NONE', *, *, #33678, .T. ) ;
#15002 = ORIENTED_EDGE ( 'NONE', *, *, #23735, .F. ) ;
#15001 = ADVANCED_FACE ( 'NONE', ( #12984 ), #35471, .T. ) ;
#15003 = SHAPE_REPRESENTATION ( 'cover', ( #66832 ), #17430 ) ;
#15004 = DIRECTION ( 'NONE',  ( 0.000000000000000000, -1.000000000000000000, 0.000000000000000000 ) ) ;
#15005 = B_SPLINE_CURVE_WITH_KNOTS ( 'NONE', 3,
 ( #14489, #57062, #40189, #25407, #67965, #20113, #29977, #34916, #61640, #8176, #52118, #35945, #46838, #61294, #7835, #13117, #13456, #29283, #45809, #56355, #8874, #51090, #40524, #2904 ),
 .UNSPECIFIED., .F., .F.,
 ( 4, 2, 2, 2, 2, 2, 2, 2, 2, 2, 2, 4 ),
 ( 0.000000000000000000, 0.001412135740307523526, 0.002118203610461290385, 0.002824271480615057027, 0.004236407220922555616, 0.005648542961230055073, 0.007060678701537554530, 0.007766746571691303391, 0.008472814441845052252, 0.009884950182152539566, 0.01059101805230627281, 0.01129708592246000433 ),
 .UNSPECIFIED. ) ;
#15006 = DIRECTION ( 'NONE',  ( -2.086468734323010064E-16, 1.377265952997520258E-16, 1.000000000000000000 ) ) ;
#15007 = CARTESIAN_POINT ( 'NONE',  ( -177.5271152834791337, 92.16916858125016176, -9.280385424022256302 ) ) ;
#15008 = EDGE_CURVE ( 'NONE', #32748, #33778, #9670, .T. ) ;
#15010 = VERTEX_POINT ( 'NONE', #49900 ) ;
#15009 = DIRECTION ( 'NONE',  ( -1.261617073437677999E-16, -0.000000000000000000, -1.000000000000000000 ) ) ;
#15011 = LINE ( 'NONE', #31883, #31948 ) ;
#15012 = DIRECTION ( 'NONE',  ( 0.000000000000000000, 0.000000000000000000, 1.000000000000000000 ) ) ;
#15013 = ORIENTED_EDGE ( 'NONE', *, *, #51063, .T. ) ;
#15014 = CARTESIAN_POINT ( 'NONE',  ( -62.45176220516621868, 16.79101814080733490, -14.61954841212545553 ) ) ;
#15015 = CARTESIAN_POINT ( 'NONE',  ( -132.0738857626834317, 51.93126104279143362, -73.51499412664540500 ) ) ;
#15017 = DIRECTION ( 'NONE',  ( -0.9362348706397417564, 0.3513748240813305279, 0.000000000000000000 ) ) ;
#15016 = AXIS2_PLACEMENT_3D ( 'NONE', #40496, #66561, #61266 ) ;
#15018 = LINE ( 'NONE', #36481, #51616 ) ;
#15019 = CARTESIAN_POINT ( 'NONE',  ( 69.72789637502503979, 15.37065610545702121, -73.42043340095284520 ) ) ;
#15020 = VERTEX_POINT ( 'NONE', #61163 ) ;
#15021 = ORIENTED_EDGE ( 'NONE', *, *, #7407, .T. ) ;
#15022 = VERTEX_POINT ( 'NONE', #34451 ) ;
#15023 = VECTOR ( 'NONE', #12195, 1000.000000000000000 ) ;
#15024 = CARTESIAN_POINT ( 'NONE',  ( 183.3913492984168840, 80.96922346472079823, -77.70910907680601554 ) ) ;
#15025 = DIRECTION ( 'NONE',  ( 0.000000000000000000, 0.000000000000000000, 1.000000000000000000 ) ) ;
#15027 = EDGE_CURVE ( 'NONE', #37023, #19968, #14701, .T. ) ;
#15026 = CARTESIAN_POINT ( 'NONE',  ( -2.914335439641035288E-14, 0.000000000000000000, -104.9999999999999858 ) ) ;
#15028 = EDGE_CURVE ( 'NONE', #41430, #67865, #57622, .T. ) ;
#15029 = EDGE_CURVE ( 'NONE', #51895, #35337, #62898, .T. ) ;
#15030 = AXIS2_PLACEMENT_3D ( 'NONE', #30448, #9691, #14276 ) ;
#15031 = CARTESIAN_POINT ( 'NONE',  ( 102.7446498997619955, 26.65764321315729646, -70.80359580029494282 ) ) ;
#15032 = CARTESIAN_POINT ( 'NONE',  ( -74.18622060908361959, 21.73430079572373685, 31.88400080372565171 ) ) ;
#15033 = CARTESIAN_POINT ( 'NONE',  ( 79.14242532928582818, 17.00090225993928073, 37.72179837095220734 ) ) ;
#15034 = EDGE_CURVE ( 'NONE', #46531, #67474, #67486, .T. ) ;
#15035 = CARTESIAN_POINT ( 'NONE',  ( -146.1142527948576628, 61.35394402951022386, 44.91319804243705960 ) ) ;
#15036 = AXIS2_PLACEMENT_3D ( 'NONE', #940, #10788, #42792 ) ;
#15037 = CARTESIAN_POINT ( 'NONE',  ( -121.2119672714299412, 44.67540322905995964, 43.99914708956819709 ) ) ;
#15038 = CARTESIAN_POINT ( 'NONE',  ( -166.9982296371934751, 80.56207291422407479, -73.39587217356408644 ) ) ;
#15039 = VERTEX_POINT ( 'NONE', #25274 ) ;
#15041 = CYLINDRICAL_SURFACE ( 'NONE', #43389, 7.500000000000013323 ) ;
#15040 = VECTOR ( 'NONE', #4679, 1000.000000000000000 ) ;
#15042 = ORIENTED_EDGE ( 'NONE', *, *, #54768, .T. ) ;
#15043 = CARTESIAN_POINT ( 'NONE',  ( -176.2094613402388177, 90.62878080648660273, -89.01962546083346695 ) ) ;
#15044 = VECTOR ( 'NONE', #57995, 1000.000000000000000 ) ;
#15045 = SURFACE_SIDE_STYLE ('',( #25949 ) ) ;
#15046 = DIRECTION ( 'NONE',  ( 0.000000000000000000, 0.000000000000000000, 1.000000000000000000 ) ) ;
#15047 = DIRECTION ( 'NONE',  ( 0.000000000000000000, 0.000000000000000000, 1.000000000000000000 ) ) ;
#15048 = CARTESIAN_POINT ( 'NONE',  ( 33.93974911725171495, 8.773765372885565128, 5.423990806426351341 ) ) ;
#15049 = DIRECTION ( 'NONE',  ( 0.000000000000000000, 0.000000000000000000, 1.000000000000000000 ) ) ;
#15050 = CARTESIAN_POINT ( 'NONE',  ( 33.75639351246964992, 7.742023566824295600, 5.607121423256566040 ) ) ;
#15051 = CARTESIAN_POINT ( 'NONE',  ( -14.84452950307166752, 8.460866451887707029, -45.57178442109233174 ) ) ;
#15052 = CIRCLE ( 'NONE', #42009, 245.3095347406802773 ) ;
#15053 = CARTESIAN_POINT ( 'NONE',  ( -37.05762690088740641, 11.60527003175541516, -20.94685073097974026 ) ) ;
#15054 = ORIENTED_EDGE ( 'NONE', *, *, #14611, .F. ) ;
#15055 = CARTESIAN_POINT ( 'NONE',  ( -118.5482723061148675, 43.02244411383185252, -94.50929498175072752 ) ) ;
#15056 = ORIENTED_EDGE ( 'NONE', *, *, #64905, .F. ) ;
#15057 = DIRECTION ( 'NONE',  ( 1.000000000000000000, 0.000000000000000000, -0.000000000000000000 ) ) ;
#15058 = CARTESIAN_POINT ( 'NONE',  ( 15.29912143387263335, 7.491799981865498559, -77.36349468914950478 ) ) ;
#15059 = CARTESIAN_POINT ( 'NONE',  ( -25.35398647985413945, 8.671412257862217032, 6.480746930813777951 ) ) ;
#15060 = CARTESIAN_POINT ( 'NONE',  ( 18.19409201603430404, 72.94804796678661774, 73.58025477438755502 ) ) ;
#15061 = CARTESIAN_POINT ( 'NONE',  ( -15.26524495591508490, 7.490231452641284093, -70.74238069447982014 ) ) ;
#15062 = LINE ( 'NONE', #36173, #16470 ) ;
#15063 = CARTESIAN_POINT ( 'NONE',  ( 157.0316110297313799, 58.58403635656377162, -36.12418429913763163 ) ) ;
#15064 = ORIENTED_EDGE ( 'NONE', *, *, #62023, .F. ) ;
#15065 = DIRECTION ( 'NONE',  ( 0.9108602745606090290, 0.4127148655274870404, -6.944224005554473694E-15 ) ) ;
#15066 = CARTESIAN_POINT ( 'NONE',  ( -154.7826623253030220, 70.14150242829514070, 59.72844556814614947 ) ) ;
#15067 = CARTESIAN_POINT ( 'NONE',  ( 175.8947993867357411, 74.90689716047907609, -22.31635991957287146 ) ) ;
#15068 = LINE ( 'NONE', #36525, #59287 ) ;
#15069 = CARTESIAN_POINT ( 'NONE',  ( -127.6881387055492354, 48.89937523111241546, -49.69948083571843256 ) ) ;
#15070 = ORIENTED_EDGE ( 'NONE', *, *, #7117, .F. ) ;
#15071 = CARTESIAN_POINT ( 'NONE',  ( -180.5954680880247452, 97.44843622358467883, -69.69668263771576733 ) ) ;
#15072 = CARTESIAN_POINT ( 'NONE',  ( 93.09528872995974780, 21.72934119836187961, 67.88888913272387526 ) ) ;
#15073 = CARTESIAN_POINT ( 'NONE',  ( 114.6632852039171269, 30.98120524556723865, 31.04740591163416852 ) ) ;
#15074 = CARTESIAN_POINT ( 'NONE',  ( 6.800000000000000711, 0.000000000000000000, -5.400000000000001243 ) ) ;
#15075 = EDGE_CURVE ( 'NONE', #34467, #29783, #63241, .T. ) ;
#15076 = AXIS2_PLACEMENT_3D ( 'NONE', #6615, #38983, #60430 ) ;
#15077 = CARTESIAN_POINT ( 'NONE',  ( 140.4897729434290738, 45.57634363643753517, 40.54951988003531937 ) ) ;
#15078 = ORIENTED_EDGE ( 'NONE', *, *, #65215, .F. ) ;
#15079 = CARTESIAN_POINT ( 'NONE',  ( 141.9165763529819344, -52.00000000000000711, 129.0000000000000000 ) ) ;
#15080 = CARTESIAN_POINT ( 'NONE',  ( 112.1164716692773453, 29.75790342121400656, -62.98934640487257042 ) ) ;
#15081 = AXIS2_PLACEMENT_3D ( 'NONE', #32942, #5854, #1289 ) ;
#15082 = CARTESIAN_POINT ( 'NONE',  ( 184.5867277229703518, 83.68414666546578928, 43.44420243020122996 ) ) ;
#15083 = CARTESIAN_POINT ( 'NONE',  ( 163.5944155533006210, 63.88379440759435823, 5.727933679616943330 ) ) ;
#15084 = CARTESIAN_POINT ( 'NONE',  ( -1.224646799147352468E-15, 0.000000000000000000, 0.000000000000000000 ) ) ;
#15085 = VECTOR ( 'NONE', #7368, 1000.000000000000000 ) ;
#15086 = ORIENTED_EDGE ( 'NONE', *, *, #8274, .T. ) ;
#15087 = VECTOR ( 'NONE', #42298, 1000.000000000000000 ) ;
#15088 = EDGE_CURVE ( 'NONE', #40950, #48132, #25622, .T. ) ;
#15089 = LINE ( 'NONE', #5217, #60939 ) ;
#15090 = CIRCLE ( 'NONE', #54379, 242.4895526022646379 ) ;
#15091 = ORIENTED_EDGE ( 'NONE', *, *, #10824, .F. ) ;
#15092 = CARTESIAN_POINT ( 'NONE',  ( -77.72491324796693846, 21.96482567905605876, -23.22677241843959450 ) ) ;
#15093 = CARTESIAN_POINT ( 'NONE',  ( 140.9234142684720723, 45.85831937333605168, 88.16266470440997693 ) ) ;
#15094 = AXIS2_PLACEMENT_3D ( 'NONE', #56100, #30402, #67361 ) ;
#15095 = EDGE_CURVE ( 'NONE', #29084, #48132, #51294, .T. ) ;
#15096 = CARTESIAN_POINT ( 'NONE',  ( -62.49130718206701829, 16.80297926264070796, 36.82688365366426808 ) ) ;
#15097 = EDGE_CURVE ( 'NONE', #18335, #62679, #43853, .T. ) ;
#15099 = ORIENTED_EDGE ( 'NONE', *, *, #24886, .T. ) ;
#15098 = CARTESIAN_POINT ( 'NONE',  ( 156.5993887774280608, 58.24868799840906775, 2.612442410024496731 ) ) ;
#15100 = DIRECTION ( 'NONE',  ( 0.000000000000000000, -0.000000000000000000, 1.000000000000000000 ) ) ;
#15101 = CARTESIAN_POINT ( 'NONE',  ( -7.825402957745083654, 6.891034867348163395, -23.57352014148015584 ) ) ;
#15102 = DIRECTION ( 'NONE',  ( -0.000000000000000000, -0.000000000000000000, -1.000000000000000000 ) ) ;
#15103 = ORIENTED_EDGE ( 'NONE', *, *, #30928, .F. ) ;
#15104 = CARTESIAN_POINT ( 'NONE',  ( 32.67633866439968671, -58.08495054655669065, 34.48241823991042310 ) ) ;
#15105 = CARTESIAN_POINT ( 'NONE',  ( 30.12852347772543027, -74.98256102853682137, 73.58025477438755502 ) ) ;
#15106 = ORIENTED_EDGE ( 'NONE', *, *, #10089, .F. ) ;
#15107 = CARTESIAN_POINT ( 'NONE',  ( 135.4423125506059193, 42.39015362494584593, 56.52087882447440137 ) ) ;
#15108 = CARTESIAN_POINT ( 'NONE',  ( 31.11269837220803325, -15.55634918610409656, 0.000000000000000000 ) ) ;
#15109 = DIRECTION ( 'NONE',  ( -0.000000000000000000, 1.000000000000000000, -0.000000000000000000 ) ) ;
#15110 = LINE ( 'NONE', #35875, #47314 ) ;
#15111 = ORIENTED_EDGE ( 'NONE', *, *, #53344, .F. ) ;
#15112 = LINE ( 'NONE', #4216, #6175 ) ;
#15113 = ORIENTED_EDGE ( 'NONE', *, *, #14723, .F. ) ;
#15115 = EDGE_CURVE ( 'NONE', #10179, #10310, #45319, .T. ) ;
#15114 = LINE ( 'NONE', #20733, #68796 ) ;
#15116 = CARTESIAN_POINT ( 'NONE',  ( 207.8398359204632868, 112.5208221429021336, -23.79464188816103487 ) ) ;
#15117 = LINE ( 'NONE', #14765, #64990 ) ;
#15118 = CARTESIAN_POINT ( 'NONE',  ( -7.336630171688589108, 7.867399454768209566, 30.11558103944719633 ) ) ;
#15119 = CARTESIAN_POINT ( 'NONE',  ( 56.83144462367863525, 11.32279212915456768, 86.74568550056409322 ) ) ;
#15120 = EDGE_CURVE ( 'NONE', #64668, #56478, #21696, .T. ) ;
#15121 = CARTESIAN_POINT ( 'NONE',  ( 182.7686108735401262, 81.77235358504610474, 2.643295075472624323 ) ) ;
#15122 = CARTESIAN_POINT ( 'NONE',  ( 207.4867844023104340, 110.2451255333963900, -36.85174997040083156 ) ) ;
#15123 = CARTESIAN_POINT ( 'NONE',  ( -13.60872002018478355, 65.24114715245431739, 34.48241795236666718 ) ) ;
#15124 = VERTEX_POINT ( 'NONE', #595 ) ;
#15125 = AXIS2_PLACEMENT_3D ( 'NONE', #13984, #34419, #61813 ) ;
#15126 = LINE ( 'NONE', #31641, #41953 ) ;
#15127 = VERTEX_POINT ( 'NONE', #54034 ) ;
#15128 = CARTESIAN_POINT ( 'NONE',  ( -77.02112161466367013, 22.77583432622785153, 72.08387616735952008 ) ) ;
#15129 = CARTESIAN_POINT ( 'NONE',  ( 56.66775172211443845, 11.28938863449062069, -66.06332206576500710 ) ) ;
#15130 = FILL_AREA_STYLE_COLOUR ( '', #32726 ) ;
#15131 = LINE ( 'NONE', #25006, #64837 ) ;
#15132 = CARTESIAN_POINT ( 'NONE',  ( -10.38456464615029518, 7.071067413477805985, 84.24719785865121935 ) ) ;
#15133 = CARTESIAN_POINT ( 'NONE',  ( -104.1393288135077171, 34.86912007524087898, -8.388960353306918805 ) ) ;
#15134 = VECTOR ( 'NONE', #16262, 1000.000000000000000 ) ;
#15135 = ORIENTED_EDGE ( 'NONE', *, *, #31067, .F. ) ;
#15136 = CARTESIAN_POINT ( 'NONE',  ( -75.43044859198180063, 21.11535168543635876, 71.53302750611915428 ) ) ;
#15137 = LINE ( 'NONE', #21437, #39752 ) ;
#15138 = VERTEX_POINT ( 'NONE', #946 ) ;
#15139 = VECTOR ( 'NONE', #24152, 1000.000000000000000 ) ;
#15140 = EDGE_LOOP ( 'NONE', ( #58398, #500, #43053, #26877, #16134 ) ) ;
#15141 = CIRCLE ( 'NONE', #33114, 24.99999999999985434 ) ;
#15142 = CARTESIAN_POINT ( 'NONE',  ( 18.62350602913453557, 70.00000000000000000, 23.51946052065799364 ) ) ;
#15143 = CARTESIAN_POINT ( 'NONE',  ( 58.48209831743722731, 11.66636741727081983, -37.22615017468061893 ) ) ;
#15144 = CARTESIAN_POINT ( 'NONE',  ( 174.9053416555736646, 72.57849647436442808, -21.16220004635683694 ) ) ;
#15145 =( LENGTH_UNIT ( ) NAMED_UNIT ( * ) SI_UNIT ( .MILLI., .METRE. ) );
#15146 = CIRCLE ( 'NONE', #60014, 243.4957430088094839 ) ;
#15147 = CARTESIAN_POINT ( 'NONE',  ( -147.3641864666714696, 62.38213854487951693, 4.175494494443603877 ) ) ;
#15148 = B_SPLINE_CURVE_WITH_KNOTS ( 'NONE', 3,
 ( #48691, #21983, #33601, #28305, #66659, #11418, #6510, #49403, #23042, #39566, #18109, #59957, #65610, #7207, #17766, #54325, #22338, #43776 ),
 .UNSPECIFIED., .F., .F.,
 ( 4, 2, 2, 2, 2, 2, 2, 2, 4 ),
 ( 0.01172246177653528745, 0.01320773491327431257, 0.01469300805001333941, 0.01617828118675236626, 0.01766355432349139137, 0.01914882746023041649, 0.02063410059696944160, 0.02211937373370847018, 0.02360464687044749529 ),
 .UNSPECIFIED. ) ;
#15149 = ORIENTED_EDGE ( 'NONE', *, *, #45418, .T. ) ;
#15150 = CARTESIAN_POINT ( 'NONE',  ( -133.3220917939969752, 52.82057604964900577, 39.18959366347132089 ) ) ;
#15151 = ORIENTED_EDGE ( 'NONE', *, *, #30050, .T. ) ;
#15152 = CARTESIAN_POINT ( 'NONE',  ( 211.5175447467295839, 116.1901475271413631, 12.99830586765888185 ) ) ;
#15153 = CARTESIAN_POINT ( 'NONE',  ( -142.0070007485041401, 59.34878529741516928, 37.95131792514063562 ) ) ;
#15154 = CARTESIAN_POINT ( 'NONE',  ( 212.0850679406003678, 117.0583048437722198, 38.04715775346591045 ) ) ;
#15155 = CARTESIAN_POINT ( 'NONE',  ( -44.99999999999998579, -25.00000000000000000, 1.999999999999984457 ) ) ;
#15156 = ADVANCED_FACE ( 'NONE', ( #27316 ), #15798, .T. ) ;
#15157 = EDGE_CURVE ( 'NONE', #33686, #37117, #10449, .T. ) ;
#15158 = ORIENTED_EDGE ( 'NONE', *, *, #34494, .T. ) ;
#15159 = ORIENTED_EDGE ( 'NONE', *, *, #31755, .T. ) ;
#15160 = CARTESIAN_POINT ( 'NONE',  ( 114.9999364138626703, -21.99998554860538391, -0.3278620034596400612 ) ) ;
#15161 = CARTESIAN_POINT ( 'NONE',  ( -126.5321066302584825, 48.12358255329873913, 84.33085040477796213 ) ) ;
#15162 = CARTESIAN_POINT ( 'NONE',  ( -165.6210506643949145, 79.15024150453838558, -15.06613721450044885 ) ) ;
#15163 = DIRECTION ( 'NONE',  ( -0.000000000000000000, 1.000000000000000000, -0.000000000000000000 ) ) ;
#15164 = CARTESIAN_POINT ( 'NONE',  ( 64.94794467308301478, 13.12874966082101835, 44.57620359267861687 ) ) ;
#15165 = CARTESIAN_POINT ( 'NONE',  ( 14.48805533322835792, 7.468382295965534823, 83.78772674431218093 ) ) ;
#15166 = ORIENTED_EDGE ( 'NONE', *, *, #7656, .T. ) ;
#15167 = LINE ( 'NONE', #22085, #22444 ) ;
#15168 = CARTESIAN_POINT ( 'NONE',  ( -97.88309373898363219, 30.60238467438961862, 58.76896769614690896 ) ) ;
#15169 = VERTEX_POINT ( 'NONE', #43146 ) ;
#15170 = CARTESIAN_POINT ( 'NONE',  ( -84.96580414052107244, 24.82184094495580595, 15.15151241668911730 ) ) ;
#15171 = VERTEX_POINT ( 'NONE', #69533 ) ;
#15172 = CIRCLE ( 'NONE', #65745, 2.999999999999999112 ) ;
#15173 = ADVANCED_FACE ( 'NONE', ( #17461 ), #65316, .T. ) ;
#15174 = ORIENTED_EDGE ( 'NONE', *, *, #7996, .F. ) ;
#15175 = EDGE_CURVE ( 'NONE', #44661, #30106, #38452, .T. ) ;
#15176 = VECTOR ( 'NONE', #34068, 1000.000000000000114 ) ;
#15177 = ORIENTED_EDGE ( 'NONE', *, *, #61875, .F. ) ;
#15178 = CARTESIAN_POINT ( 'NONE',  ( 12.69192874957004413, 6.421326776602847453, -49.85437527733665775 ) ) ;
#15179 = CARTESIAN_POINT ( 'NONE',  ( -179.2177980985565000, 94.18084789436636584, 60.79021173935545619 ) ) ;
#15180 = EDGE_CURVE ( 'NONE', #57004, #9808, #53700, .T. ) ;
#15181 = CARTESIAN_POINT ( 'NONE',  ( 126.3541873520044021, 37.07520218256171773, 63.35537632752008363 ) ) ;
#15182 = AXIS2_PLACEMENT_3D ( 'NONE', #18067, #13142, #34606 ) ;
#15183 = CIRCLE ( 'NONE', #2835, 65.00000000000000000 ) ;
#15184 = ORIENTED_EDGE ( 'NONE', *, *, #61694, .F. ) ;
#15185 = CARTESIAN_POINT ( 'NONE',  ( -33.04857881320337754, 9.860948377235466467, 84.07333317060516720 ) ) ;
#15186 = CARTESIAN_POINT ( 'NONE',  ( 154.4550750032601343, 55.34393534448155805, 43.78048194385345937 ) ) ;
#15187 = AXIS2_PLACEMENT_3D ( 'NONE', #6533, #50832, #24112 ) ;
#15188 = DIRECTION ( 'NONE',  ( -0.000000000000000000, 1.000000000000000000, -0.000000000000000000 ) ) ;
#15189 = CARTESIAN_POINT ( 'NONE',  ( 102.8518012651273494, 25.61025413220827573, -42.12408111876868588 ) ) ;
#15190 = CARTESIAN_POINT ( 'NONE',  ( -28.35330809568272059, 9.105138953156457049, 44.55656940449198089 ) ) ;
#15191 = CARTESIAN_POINT ( 'NONE',  ( -143.7133518487516994, 60.70463114991427034, -64.38850710249009524 ) ) ;
#15192 = ORIENTED_EDGE ( 'NONE', *, *, #46964, .T. ) ;
#15193 = CYLINDRICAL_SURFACE ( 'NONE', #11795, 4.999999999999997335 ) ;
#15194 = CARTESIAN_POINT ( 'NONE',  ( -80.54915509118112027, 24.12810583352862537, -76.72378030112859904 ) ) ;
#15195 = CARTESIAN_POINT ( 'NONE',  ( 173.8623159076319666, 72.97967239795019623, 7.919453758277684940 ) ) ;
#15196 = CARTESIAN_POINT ( 'NONE',  ( -452.6627218934914367, 399.9999999999998863, -146.4497041420118251 ) ) ;
#15197 = FACE_BOUND ( 'NONE', #25741, .T. ) ;
#15198 = CARTESIAN_POINT ( 'NONE',  ( 132.0440382699654833, 40.34028297386453943, 2.873803673234553990 ) ) ;
#15199 = CARTESIAN_POINT ( 'NONE',  ( -156.9910258076866114, 70.79617246506499839, 10.80262140621922384 ) ) ;
#15200 = CARTESIAN_POINT ( 'NONE',  ( 197.2746525007791547, 98.29263840007783415, 91.49113674313775846 ) ) ;
#15201 = CARTESIAN_POINT ( 'NONE',  ( 208.5936709733498446, 113.6229123546138169, 30.28492877757630453 ) ) ;
#15202 = CARTESIAN_POINT ( 'NONE',  ( 163.7464701930790056, 62.69993100427431898, 5.927907296324478992 ) ) ;
#15203 = DIRECTION ( 'NONE',  ( -0.000000000000000000, -0.000000000000000000, -1.000000000000000000 ) ) ;
#15204 = VERTEX_POINT ( 'NONE', #238 ) ;
#15205 = DIRECTION ( 'NONE',  ( 0.000000000000000000, 0.000000000000000000, 1.000000000000000000 ) ) ;
#15206 = ORIENTED_EDGE ( 'NONE', *, *, #28604, .T. ) ;
#15207 = DIRECTION ( 'NONE',  ( -0.000000000000000000, -0.000000000000000000, -1.000000000000000000 ) ) ;
#15208 = ORIENTED_EDGE ( 'NONE', *, *, #53745, .F. ) ;
#15209 = FACE_OUTER_BOUND ( 'NONE', #56149, .T. ) ;
#15210 = CARTESIAN_POINT ( 'NONE',  ( -5.066666666666664653, 0.000000000000000000, 43.13333333333333286 ) ) ;
#15211 = CARTESIAN_POINT ( 'NONE',  ( -170.2856292770789537, 85.50720222068223109, 31.36520312212658723 ) ) ;
#15212 = LINE ( 'NONE', #52828, #51280 ) ;
#15213 = CARTESIAN_POINT ( 'NONE',  ( 134.3182571105338639, 42.88121222759019702, -36.02331093239565973 ) ) ;
#15214 = LINE ( 'NONE', #36678, #58015 ) ;
#15215 = B_SPLINE_CURVE_WITH_KNOTS ( 'NONE', 3,
 ( #54303, #1212, #65588, #5098, #37799, #865, #512, #48324, #53618, #33233, #38860, #157, #27237, #12122, #60301, #21963, #43410, #69457, #49381, #42726, #33585, #6492, #64181, #48670, #47993, #22664, #59936, #5779, #16688, #21277, #11396, #6125, #58898, #64887, #64533, #32521, #16343, #32187, #59246, #59580, #38493, #15994, #43061, #10713 ),
 .UNSPECIFIED., .F., .F.,
 ( 4, 2, 2, 2, 2, 2, 2, 2, 2, 2, 2, 2, 2, 2, 2, 2, 2, 2, 2, 2, 2, 4 ),
 ( 1.387778780781445676E-17, 0.003433139681083760119, 0.004291424601354644312, 0.005149709521625528072, 0.006866279362167280846, 0.007724564282438147259, 0.008582849202709011069, 0.009441134122979876614, 0.01029941904325074216, 0.01201598888379252009, 0.01373255872433429801, 0.01459084364460518611, 0.01544912856487607768, 0.01630741348514696751, 0.01716569840541785907, 0.01888226824595965608, 0.02059883808650145309, 0.02145712300677238282, 0.02231540792704331602, 0.02403197776758509915, 0.02574854760812688229, 0.02746511744866866542 ),
 .UNSPECIFIED. ) ;
#15216 = LINE ( 'NONE', #47550, #1193 ) ;
#15217 = LINE ( 'NONE', #52505, #21746 ) ;
#15218 = DIRECTION ( 'NONE',  ( -0.000000000000000000, 1.000000000000000000, -0.000000000000000000 ) ) ;
#15219 = ORIENTED_EDGE ( 'NONE', *, *, #23035, .T. ) ;
#15220 = ORIENTED_EDGE ( 'NONE', *, *, #25957, .F. ) ;
#15221 = VECTOR ( 'NONE', #8095, 1000.000000000000000 ) ;
#15222 = CARTESIAN_POINT ( 'NONE',  ( 180.6785550066271924, 79.62522105737480160, 82.98728187965927816 ) ) ;
#15223 =( NAMED_UNIT ( * ) PLANE_ANGLE_UNIT ( ) SI_UNIT ( $, .RADIAN. ) );
#15224 = CARTESIAN_POINT ( 'NONE',  ( 126.6904219525097659, 38.41566710102375737, -95.00000000000133582 ) ) ;
#15225 = AXIS2_PLACEMENT_3D ( 'NONE', #47973, #21941, #20558 ) ;
#15226 = CARTESIAN_POINT ( 'NONE',  ( 69.68177367721197868, -20.52767805628086961, 3.061616997868437868E-16 ) ) ;
#15227 = ADVANCED_FACE ( 'NONE', ( #6570 ), #1294, .T. ) ;
#15228 = CARTESIAN_POINT ( 'NONE',  ( 92.20490818459940385, 22.47175429302964034, 15.40764561472821015 ) ) ;
#15229 = VECTOR ( 'NONE', #49456, 1000.000000000000000 ) ;
#15230 = AXIS2_PLACEMENT_3D ( 'NONE', #40506, #46471, #68291 ) ;
#15231 = DIRECTION ( 'NONE',  ( -0.000000000000000000, 1.000000000000000000, -0.000000000000000000 ) ) ;
#15232 = CARTESIAN_POINT ( 'NONE',  ( -4.164416015345870470, 64.86646004871185767, 170.0000000000000000 ) ) ;
#15233 = CARTESIAN_POINT ( 'NONE',  ( 0.08224679563972019103, -7.710515798486379246, -2.644994884459114459 ) ) ;
#15234 = CARTESIAN_POINT ( 'NONE',  ( 93.33480479917550099, 21.81892021443992746, -13.07991783598629532 ) ) ;
#15235 = FACE_OUTER_BOUND ( 'NONE', #3424, .T. ) ;
#15236 = PLANE ( 'NONE',  #49769 ) ;
#15237 = AXIS2_PLACEMENT_3D ( 'NONE', #36871, #63940, #51667 ) ;
#15238 = CARTESIAN_POINT ( 'NONE',  ( 0.000000000000000000, 0.000000000000000000, 2.000000000000000000 ) ) ;
#15239 = AXIS2_PLACEMENT_3D ( 'NONE', #14582, #3003, #30769 ) ;
#15240 = EDGE_CURVE ( 'NONE', #12534, #25214, #38225, .T. ) ;
#15241 = VECTOR ( 'NONE', #27545, 1000.000000000000000 ) ;
#15242 = EDGE_CURVE ( 'NONE', #67479, #11433, #59666, .T. ) ;
#15243 =( REPRESENTATION_RELATIONSHIP ('NONE','NONE', #40274, #50551 ) REPRESENTATION_RELATIONSHIP_WITH_TRANSFORMATION ( #11161 )SHAPE_REPRESENTATION_RELATIONSHIP( ) );
#15244 = VERTEX_POINT ( 'NONE', #32268 ) ;
#15245 = CARTESIAN_POINT ( 'NONE',  ( 126.8114659053430842, 38.48351437375814754, 7.542840871000518810 ) ) ;
#15246 = DIRECTION ( 'NONE',  ( -1.387778780781446169E-16, 1.000000000000000000, 3.469446951953615421E-17 ) ) ;
#15247 = EDGE_CURVE ( 'NONE', #23032, #53816, #42801, .T. ) ;
#15248 = CARTESIAN_POINT ( 'NONE',  ( 157.0316110297313230, 58.58403635656375741, 71.25401806271707983 ) ) ;
#15249 = CARTESIAN_POINT ( 'NONE',  ( 63.01563776193091826, -170.0000000000000000, 37.31296093922129131 ) ) ;
#15250 = DIRECTION ( 'NONE',  ( -0.000000000000000000, 1.000000000000000000, -0.000000000000000000 ) ) ;
#15251 = CARTESIAN_POINT ( 'NONE',  ( -439.4229916354182706, 400.0000000000065370, -123.9497041420119530 ) ) ;
#15252 = ORIENTED_EDGE ( 'NONE', *, *, #34475, .F. ) ;
#15253 = CARTESIAN_POINT ( 'NONE',  ( 157.4703587214989113, 58.92748579479259519, -62.96873488960130771 ) ) ;
#15254 = CARTESIAN_POINT ( 'NONE',  ( -62.48965350618344416, 16.80247907725181733, 65.66443840238910923 ) ) ;
#15255 = EDGE_LOOP ( 'NONE', ( #31860, #60299, #4403, #51256 ) ) ;
#15256 = ORIENTED_EDGE ( 'NONE', *, *, #58508, .F. ) ;
#15257 = CARTESIAN_POINT ( 'NONE',  ( 46.69842531913727157, 10.49021410897251272, 92.86971545278713336 ) ) ;
#15258 = CARTESIAN_POINT ( 'NONE',  ( -180.6209440844958181, 95.88392769199010957, -68.73652789255280027 ) ) ;
#15259 = DIRECTION ( 'NONE',  ( 0.000000000000000000, -1.000000000000000000, 0.000000000000000000 ) ) ;
#15260 = EDGE_CURVE ( 'NONE', #30857, #41100, #32602, .T. ) ;
#15261 = ORIENTED_EDGE ( 'NONE', *, *, #6578, .T. ) ;
#15262 = DIRECTION ( 'NONE',  ( 0.5407162030609374836, -0.6444004775717707689, -0.5407162030609372616 ) ) ;
#15263 = CARTESIAN_POINT ( 'NONE',  ( 230.9999999999999432, 190.0000000000000000, 380.0000000000000000 ) ) ;
#15264 = CARTESIAN_POINT ( 'NONE',  ( 32.09567473596477782, 7.571373529017940029, -14.56364366973223845 ) ) ;
#15265 = CARTESIAN_POINT ( 'NONE',  ( -17.50000000000002842, 207.5000000000000284, -2.000000000000000000 ) ) ;
#15266 = CARTESIAN_POINT ( 'NONE',  ( 164.9797987607189214, 63.73352393706674235, 90.52080388245950360 ) ) ;
#15267 = CARTESIAN_POINT ( 'NONE',  ( 93.61951000632932107, 21.92572933971849025, 34.48277232936159464 ) ) ;
#15268 = PRODUCT_DEFINITION_SHAPE ( 'NONE', 'NONE',  #16010 ) ;
#15269 = EDGE_LOOP ( 'NONE', ( #5409, #23940, #8810, #19099 ) ) ;
#15270 =( NAMED_UNIT ( * ) SI_UNIT ( $, .STERADIAN. ) SOLID_ANGLE_UNIT ( ) );
#15271 = AXIS2_PLACEMENT_3D ( 'NONE', #34163, #66874, #44706 ) ;
#15272 = CARTESIAN_POINT ( 'NONE',  ( 9.290502160020466249, 6.379616279862541539, 60.60564355645543344 ) ) ;
#15273 = DIRECTION ( 'NONE',  ( -0.000000000000000000, 1.000000000000000000, -0.000000000000000000 ) ) ;
#15274 = CARTESIAN_POINT ( 'NONE',  ( 203.9203998321607969, 106.9845510704142413, 44.17774257179522124 ) ) ;
#15275 = CARTESIAN_POINT ( 'NONE',  ( 79.26746824650808776, 17.03912548276234773, 89.42829496025042602 ) ) ;
#15276 = AXIS2_PLACEMENT_3D ( 'NONE', #47728, #58290, #37183 ) ;
#15278 = ORIENTED_EDGE ( 'NONE', *, *, #12813, .F. ) ;
#15277 = CYLINDRICAL_SURFACE ( 'NONE', #14086, 7.500000000000020428 ) ;
#15279 = ORIENTED_EDGE ( 'NONE', *, *, #15029, .F. ) ;
#15280 = VECTOR ( 'NONE', #39291, 1000.000000000000000 ) ;
#15281 = AXIS2_PLACEMENT_3D ( 'NONE', #68874, #16109, #20351 ) ;
#15282 = ORIENTED_EDGE ( 'NONE', *, *, #48100, .F. ) ;
#15283 = CARTESIAN_POINT ( 'NONE',  ( 113.8626313173126334, 31.71036178495293711, -63.68104293568552521 ) ) ;
#15284 = DIRECTION ( 'NONE',  ( 0.000000000000000000, 1.000000000000000000, 0.000000000000000000 ) ) ;
#15285 = CARTESIAN_POINT ( 'NONE',  ( 204.6977192012829789, 106.3443248447423599, -78.17048162308530834 ) ) ;
#15286 = AXIS2_PLACEMENT_3D ( 'NONE', #16090, #253, #49473 ) ;
#15288 = DIRECTION ( 'NONE',  ( -0.000000000000000000, 1.000000000000000000, -0.000000000000000000 ) ) ;
#15287 = VECTOR ( 'NONE', #41238, 1000.000000000000114 ) ;
#15289 = CARTESIAN_POINT ( 'NONE',  ( 0.000000000000000000, 6.000000000000000000, -20.00000000000000000 ) ) ;
#15290 = CARTESIAN_POINT ( 'NONE',  ( 151.1873096904021736, 52.92629247302097184, -66.36498583336128831 ) ) ;
#15291 = DIRECTION ( 'NONE',  ( -0.000000000000000000, -0.000000000000000000, 1.000000000000000000 ) ) ;
#15292 = AXIS2_PLACEMENT_3D ( 'NONE', #11289, #9929, #32760 ) ;
#15293 = CARTESIAN_POINT ( 'NONE',  ( -30.60309003827974550, 68.41902945196812880, 41.38025477438755928 ) ) ;
#15294 = ORIENTED_EDGE ( 'NONE', *, *, #47825, .F. ) ;
#15295 = ORIENTED_EDGE ( 'NONE', *, *, #55834, .T. ) ;
#15296 = B_SPLINE_CURVE_WITH_KNOTS ( 'NONE', 3,
 ( #58472, #31415, #63426, #15233, #37362, #26134, #36003, #36698 ),
 .UNSPECIFIED., .F., .F.,
 ( 4, 2, 2, 4 ),
 ( 0.004673709593152144438, 0.005837709341827637330, 0.007001709090503131089, 0.009329708587854116872 ),
 .UNSPECIFIED. ) ;
#15297 = DIRECTION ( 'NONE',  ( -0.000000000000000000, -1.000000000000000000, -0.000000000000000000 ) ) ;
#15298 = CARTESIAN_POINT ( 'NONE',  ( -85.75002235020433261, 26.23806300442547723, -40.13818612277900399 ) ) ;
#15299 = CARTESIAN_POINT ( 'NONE',  ( 160.9241720448058857, 60.38677655937334521, 70.42760667945063346 ) ) ;
#15300 = CARTESIAN_POINT ( 'NONE',  ( 116.0822834687217409, 32.80169113915576418, -11.84535301537962937 ) ) ;
#15301 = EDGE_CURVE ( 'NONE', #454, #2243, #40314, .T. ) ;
#15302 = CARTESIAN_POINT ( 'NONE',  ( 184.3994103300443328, 82.02159554764422467, -36.98265584704628139 ) ) ;
#15303 = CARTESIAN_POINT ( 'NONE',  ( 447.3372781065085064, 400.0000000000037517, 113.5502958579882034 ) ) ;
#15304 = CARTESIAN_POINT ( 'NONE',  ( -151.7334413882332456, 67.42499880430109727, 84.72756373490047110 ) ) ;
#15305 = ORIENTED_EDGE ( 'NONE', *, *, #37282, .F. ) ;
#15306 = ORIENTED_EDGE ( 'NONE', *, *, #62917, .T. ) ;
#15307 = VERTEX_POINT ( 'NONE', #60726 ) ;
#15308 = FILL_AREA_STYLE_COLOUR ( '', #55488 ) ;
#15309 = CARTESIAN_POINT ( 'NONE',  ( 90.78038362056545907, 21.94937144186732425, -90.75119527580173440 ) ) ;
#15310 = CARTESIAN_POINT ( 'NONE',  ( -15.55634918610405748, -15.55634918610400774, 85.00100000000000477 ) ) ;
#15311 = CARTESIAN_POINT ( 'NONE',  ( -33.38294402636583413, 10.93918551420888363, -62.40138409474297987 ) ) ;
#15312 = CARTESIAN_POINT ( 'NONE',  ( 201.9822477997853412, 104.3642793804899753, 56.54934032291012613 ) ) ;
#15313 = CARTESIAN_POINT ( 'NONE',  ( 33.44527180510248598, 7.709232309484707280, 59.67497009447234291 ) ) ;
#15314 = CARTESIAN_POINT ( 'NONE',  ( 60.40479419793764038, 24.00543350795394915, 170.0000000000000000 ) ) ;
#15315 =( NAMED_UNIT ( * ) SI_UNIT ( $, .STERADIAN. ) SOLID_ANGLE_UNIT ( ) );
#15316 = CARTESIAN_POINT ( 'NONE',  ( 0.000000000000000000, 200.0000000000000000, -10.00000000000000000 ) ) ;
#15317 = FACE_OUTER_BOUND ( 'NONE', #29296, .T. ) ;
#15318 = CARTESIAN_POINT ( 'NONE',  ( -120.4816138481824908, 43.03185659245511374, 6.060518139089774436 ) ) ;
#15319 = CARTESIAN_POINT ( 'NONE',  ( 98.48662049252135375, -156.6058287036421461, 10.00000000000000000 ) ) ;
#15320 = CARTESIAN_POINT ( 'NONE',  ( -447.6627218934914936, 392.9289321881341266, -141.4497041420118251 ) ) ;
#15321 = LINE ( 'NONE', #36784, #61328 ) ;
#15322 = DIRECTION ( 'NONE',  ( -1.000000000000000000, 0.000000000000000000, 0.000000000000000000 ) ) ;
#15323 = EDGE_CURVE ( 'NONE', #8527, #32748, #18866, .T. ) ;
#15324 = VECTOR ( 'NONE', #27825, 1000.000000000000000 ) ;
#15325 = ORIENTED_EDGE ( 'NONE', *, *, #17731, .T. ) ;
#15326 = VECTOR ( 'NONE', #66032, 1000.000000000000000 ) ;
#15327 = CARTESIAN_POINT ( 'NONE',  ( 188.5662303205146770, 86.51341602961787203, 10.56255491576774830 ) ) ;
#15328 = APPLICATION_PROTOCOL_DEFINITION ( 'draft international standard', 'automotive_design', 1998, #55716 ) ;
#15329 = ADVANCED_FACE ( 'NONE', ( #7629 ), #29081, .T. ) ;
#15330 = CARTESIAN_POINT ( 'NONE',  ( 174.9053416555736646, 72.57849647436445650, 32.52690113457052234 ) ) ;
#15331 = DIRECTION ( 'NONE',  ( -0.000000000000000000, -0.000000000000000000, -1.000000000000000000 ) ) ;
#15332 = PLANE ( 'NONE',  #55953 ) ;
#15333 = CARTESIAN_POINT ( 'NONE',  ( -36.11269837220809364, -15.55634918610397754, 0.000000000000000000 ) ) ;
#15334 = ORIENTED_EDGE ( 'NONE', *, *, #26061, .F. ) ;
#15335 = VECTOR ( 'NONE', #18788, 1000.000000000000000 ) ;
#15336 = EDGE_CURVE ( 'NONE', #12092, #11928, #55552, .T. ) ;
#15337 = ORIENTED_EDGE ( 'NONE', *, *, #54278, .T. ) ;
#15338 = CARTESIAN_POINT ( 'NONE',  ( 35.54014968547571129, -66.04466488925490353, 0.000000000000000000 ) ) ;
#15339 = CARTESIAN_POINT ( 'NONE',  ( 199.7291770695761102, 101.4092159658447230, 15.48654468859881561 ) ) ;
#15340 = EDGE_LOOP ( 'NONE', ( #65390, #64020, #51418, #38157 ) ) ;
#15341 = VECTOR ( 'NONE', #13409, 1000.000000000000000 ) ;
#15342 = CARTESIAN_POINT ( 'NONE',  ( 117.4696399285658970, 32.37118663718648293, 61.88302862921270275 ) ) ;
#15343 = EDGE_CURVE ( 'NONE', #63326, #34523, #33664, .T. ) ;
#15344 = ORIENTED_EDGE ( 'NONE', *, *, #50688, .F. ) ;
#15345 = CARTESIAN_POINT ( 'NONE',  ( 427.4999999999999432, -18.06806526123148160, 378.0000000000000000 ) ) ;
#15346 = CARTESIAN_POINT ( 'NONE',  ( 0.000000000000000000, 0.000000000000000000, 40.00000000000003553 ) ) ;
#15347 = DIRECTION ( 'NONE',  ( -1.000000000000000000, -0.000000000000000000, -0.000000000000000000 ) ) ;
#15348 = EDGE_CURVE ( 'NONE', #57527, #13467, #45240, .T. ) ;
#15349 = CARTESIAN_POINT ( 'NONE',  ( 26.99999999999999289, 26.99999999999999645, 0.000000000000000000 ) ) ;
#15350 = CARTESIAN_POINT ( 'NONE',  ( 93.70675391435746349, 21.95852801827565060, -45.81628112151712173 ) ) ;
#15352 = ORIENTED_EDGE ( 'NONE', *, *, #22534, .F. ) ;
#15351 = CARTESIAN_POINT ( 'NONE',  ( 75.00000000000000000, 0.000000000000000000, 43.58025477438756212 ) ) ;
#15353 = LINE ( 'NONE', #69145, #48548 ) ;
#15354 = VERTEX_POINT ( 'NONE', #49815 ) ;
#15355 = ORIENTED_EDGE ( 'NONE', *, *, #4297, .F. ) ;
#15356 = CARTESIAN_POINT ( 'NONE',  ( -118.3960663196801306, 41.75130200162922023, -16.13710083091054059 ) ) ;
#15357 = CARTESIAN_POINT ( 'NONE',  ( 39.40195752203892710, 8.409560354027400209, 29.91383430596324899 ) ) ;
#15358 = CARTESIAN_POINT ( 'NONE',  ( -179.2262621278718200, 94.19039042964669761, -10.98208730704558533 ) ) ;
#15360 = ORIENTED_EDGE ( 'NONE', *, *, #20391, .F. ) ;
#15359 = CARTESIAN_POINT ( 'NONE',  ( -143.2464978228199470, 59.04559547356110016, -38.17535989881711345 ) ) ;
#15361 = CARTESIAN_POINT ( 'NONE',  ( -108.1267491639865028, 36.99658152819874601, 86.96702877733119408 ) ) ;
#15362 = DIRECTION ( 'NONE',  ( -0.000000000000000000, -0.000000000000000000, -1.000000000000000000 ) ) ;
#15363 = ORIENTED_EDGE ( 'NONE', *, *, #61745, .F. ) ;
#15364 = DIRECTION ( 'NONE',  ( 0.000000000000000000, 0.000000000000000000, -1.000000000000000000 ) ) ;
#15365 = CARTESIAN_POINT ( 'NONE',  ( -133.3316503378478046, 52.82738260200862612, -70.36155835367432587 ) ) ;
#15366 = CARTESIAN_POINT ( 'NONE',  ( 55.76286625948333864, 11.10663164471739606, -95.00000000000133582 ) ) ;
#15367 = CARTESIAN_POINT ( 'NONE',  ( -95.86612279493098754, 29.64021615886203520, 15.06998184580957201 ) ) ;
#15368 = CARTESIAN_POINT ( 'NONE',  ( -95.19652294162980866, 29.32558722310179888, -66.84180561699812984 ) ) ;
#15369 = VERTEX_POINT ( 'NONE', #50526 ) ;
#15370 = ORIENTED_EDGE ( 'NONE', *, *, #36931, .T. ) ;
#15371 = AXIS2_PLACEMENT_3D ( 'NONE', #21361, #10121, #4840 ) ;
#15372 = CARTESIAN_POINT ( 'NONE',  ( 181.5127080940606845, 79.03904173130082711, -63.06960825634329382 ) ) ;
#15373 = CARTESIAN_POINT ( 'NONE',  ( -173.1211646369891071, 87.12891641440859303, -34.71195716474998960 ) ) ;
#15374 = DIRECTION ( 'NONE',  ( -0.000000000000000000, -1.000000000000000000, -0.000000000000000000 ) ) ;
#15375 = AXIS2_PLACEMENT_3D ( 'NONE', #46911, #40592, #41295 ) ;
#15376 = CARTESIAN_POINT ( 'NONE',  ( 109.3047140914111708, 29.55674059952507804, -62.81089258595097391 ) ) ;
#15377 = CARTESIAN_POINT ( 'NONE',  ( -71.97658551692140350, 20.95070248419150971, 34.51833332167712598 ) ) ;
#15378 = EDGE_CURVE ( 'NONE', #67017, #20457, #66721, .T. ) ;
#15379 = CARTESIAN_POINT ( 'NONE',  ( 79.53408731553405175, 17.12082763744058767, 39.69320813087158228 ) ) ;
#15380 = AXIS2_PLACEMENT_3D ( 'NONE', #56932, #35116, #46017 ) ;
#15381 = CARTESIAN_POINT ( 'NONE',  ( 69.35866309798979046, 15.27376159675663203, -39.21109914877717273 ) ) ;
#15382 = CARTESIAN_POINT ( 'NONE',  ( 181.0840389613909736, -170.0000000000000000, -89.91415884680696990 ) ) ;
#15383 = LINE ( 'NONE', #48065, #25106 ) ;
#15384 = EDGE_LOOP ( 'NONE', ( #22541, #26204, #62690, #34851 ) ) ;
#15385 = CYLINDRICAL_SURFACE ( 'NONE', #22063, 7.500000000000013323 ) ;
#15386 = ORIENTED_EDGE ( 'NONE', *, *, #12875, .F. ) ;
#15387 = EDGE_CURVE ( 'NONE', #19256, #46466, #30421, .T. ) ;
#15389 = AXIS2_PLACEMENT_3D ( 'NONE', #53397, #47786, #69248 ) ;
#15388 = DIRECTION ( 'NONE',  ( 0.000000000000000000, 1.000000000000000000, 0.000000000000000000 ) ) ;
#15390 = CARTESIAN_POINT ( 'NONE',  ( 79.13041963748371188, 18.04952109592811738, 63.53642847383714098 ) ) ;
#15391 = CARTESIAN_POINT ( 'NONE',  ( -79.51308867657013479, 22.64556585543077105, -88.84041300975997046 ) ) ;
#15392 = LINE ( 'NONE', #21017, #21946 ) ;
#15393 = CARTESIAN_POINT ( 'NONE',  ( -173.1211646369891071, 87.12891641440859303, 45.82169460664104577 ) ) ;
#15394 = DIRECTION ( 'NONE',  ( -0.000000000000000000, -0.000000000000000000, -1.000000000000000000 ) ) ;
#15395 = LINE ( 'NONE', #44096, #62596 ) ;
#15396 = CARTESIAN_POINT ( 'NONE',  ( -95.86163447241558799, 30.75089131639700213, -73.27107820499439583 ) ) ;
#15397 = CARTESIAN_POINT ( 'NONE',  ( -38.80621516088655198, 11.94263260276895267, -14.50409165160439606 ) ) ;
#15398 = ORIENTED_EDGE ( 'NONE', *, *, #54962, .T. ) ;
#15399 = DIRECTION ( 'NONE',  ( -2.213730317917169031E-18, 4.596858371395784539E-18, -1.000000000000000000 ) ) ;
#15400 = VERTEX_POINT ( 'NONE', #13584 ) ;
#15401 = DIRECTION ( 'NONE',  ( -1.000000000000000000, 0.000000000000000000, -0.000000000000000000 ) ) ;
#15402 = CARTESIAN_POINT ( 'NONE',  ( 0.000000000000000000, 0.000000000000000000, 170.0000000000000000 ) ) ;
#15403 = CARTESIAN_POINT ( 'NONE',  ( -30.47069031368414826, 9.433993659086572947, 3.418604320433936472 ) ) ;
#15404 = EDGE_CURVE ( 'NONE', #51157, #64323, #56487, .T. ) ;
#15405 = DIRECTION ( 'NONE',  ( -1.000000000000000000, -0.000000000000000000, -0.000000000000000000 ) ) ;
#15406 = CARTESIAN_POINT ( 'NONE',  ( -13.78293860383720038, 7.352367295275509029, -65.17994511467486518 ) ) ;
#15407 = LINE ( 'NONE', #58306, #4086 ) ;
#15408 = ADVANCED_FACE ( 'NONE', ( #25191 ), #46973, .T. ) ;
#15409 = CARTESIAN_POINT ( 'NONE',  ( 150.9128604434957595, 53.97103482421771048, -47.30234765383832496 ) ) ;
#15410 = EDGE_CURVE ( 'NONE', #3016, #67765, #57876, .T. ) ;
#15411 = ORIENTED_EDGE ( 'NONE', *, *, #12389, .F. ) ;
#15412 = CARTESIAN_POINT ( 'NONE',  ( 647.4701170695277597, 829.1028891121204651, 657.5068267248701659 ) ) ;
#15413 = EDGE_CURVE ( 'NONE', #56653, #35195, #19550, .T. ) ;
#15414 = CARTESIAN_POINT ( 'NONE',  ( 141.0229350107040887, 47.12561858623062960, -95.00000000000133582 ) ) ;
#15415 = CARTESIAN_POINT ( 'NONE',  ( 174.2538192999569731, 73.34752463892030505, -19.99058039971637513 ) ) ;
#15416 = CARTESIAN_POINT ( 'NONE',  ( 309.8720357909272707, 18.00000000000002842, 256.6193948016162381 ) ) ;
#15417 = CARTESIAN_POINT ( 'NONE',  ( 0.4969600502617522730, 8.860760056385746708, 0.6527133886630306359 ) ) ;
#15418 = VERTEX_POINT ( 'NONE', #36772 ) ;
#15419 = LINE ( 'NONE', #37554, #43458 ) ;
#15420 = CARTESIAN_POINT ( 'NONE',  ( -1.728570918131775436, 6.570609986804681668, -20.44832033284899353 ) ) ;
#15421 = CIRCLE ( 'NONE', #37907, 5.000000000000004441 ) ;
#15422 = FILL_AREA_STYLE_COLOUR ( '', #12261 ) ;
#15423 = CARTESIAN_POINT ( 'NONE',  ( -142.4971084705952649, 58.45403049551539709, 89.22328903718332072 ) ) ;
#15424 = VECTOR ( 'NONE', #2083, 1000.000000000000000 ) ;
#15425 = CARTESIAN_POINT ( 'NONE',  ( -15.47041015649555185, -73.39774458108232125, 170.0000000000000000 ) ) ;
#15426 = EDGE_CURVE ( 'NONE', #38200, #26520, #10792, .T. ) ;
#15427 = EDGE_LOOP ( 'NONE', ( #674, #62289, #24114, #9722 ) ) ;
#15428 = CARTESIAN_POINT ( 'NONE',  ( -42.02161712141799654, -26.09918303830819042, 30.00000000000000000 ) ) ;
#15429 = CARTESIAN_POINT ( 'NONE',  ( 84.74089592029042706, 19.84571403269346135, 3.105186560012996200 ) ) ;
#15430 = AXIS2_PLACEMENT_3D ( 'NONE', #9261, #4340, #45860 ) ;
#15431 = CARTESIAN_POINT ( 'NONE',  ( 63.01563776193091826, -170.0000000000000000, -16.37614024170606797 ) ) ;
#15432 = CARTESIAN_POINT ( 'NONE',  ( 155.2992895652388086, 57.24699634758580657, 29.71672381646145311 ) ) ;
#15433 = CARTESIAN_POINT ( 'NONE',  ( -101.3537077702550562, 33.43904726487055967, 45.47600929637822986 ) ) ;
#15434 = EDGE_CURVE ( 'NONE', #3067, #41100, #68762, .T. ) ;
#15435 = EDGE_CURVE ( 'NONE', #28106, #59106, #20574, .T. ) ;
#15436 = ADVANCED_FACE ( 'NONE', ( #30803 ), #42038, .T. ) ;
#15437 = AXIS2_PLACEMENT_3D ( 'NONE', #3850, #41133, #46749 ) ;
#15438 = ORIENTED_EDGE ( 'NONE', *, *, #26708, .T. ) ;
#15439 = VECTOR ( 'NONE', #64755, 1000.000000000000000 ) ;
#15440 = CARTESIAN_POINT ( 'NONE',  ( 173.6024011093110744, 72.73634049052006390, 63.05001675959219654 ) ) ;
#15441 = ORIENTED_EDGE ( 'NONE', *, *, #11098, .T. ) ;
#15442 = AXIS2_PLACEMENT_3D ( 'NONE', #6459, #5059, #17347 ) ;
#15443 = CARTESIAN_POINT ( 'NONE',  ( -71.43874587651173158, 19.69883891272894516, -17.78934971970884149 ) ) ;
#15444 = CARTESIAN_POINT ( 'NONE',  ( -15.55634918610411077, -46.66904755831208718, 85.00100000000000477 ) ) ;
#15445 = CARTESIAN_POINT ( 'NONE',  ( -60.13226458141418362, 16.10241298991027037, 43.34078196804391325 ) ) ;
#15447 = ORIENTED_EDGE ( 'NONE', *, *, #43574, .T. ) ;
#15446 = DIRECTION ( 'NONE',  ( -0.000000000000000000, 1.000000000000000000, -0.000000000000000000 ) ) ;
#15448 = CARTESIAN_POINT ( 'NONE',  ( -179.8996803435689174, 95.00451760716445904, 41.54311889901401145 ) ) ;
#15449 = DIRECTION ( 'NONE',  ( 1.000000000000000000, 0.000000000000000000, 0.000000000000000000 ) ) ;
#15450 = FACE_OUTER_BOUND ( 'NONE', #24221, .T. ) ;
#15451 = ORIENTED_EDGE ( 'NONE', *, *, #17630, .F. ) ;
#15452 = PLANE ( 'NONE',  #6399 ) ;
#15453 = B_SPLINE_CURVE_WITH_KNOTS ( 'NONE', 3,
 ( #52127, #3260, #20121, #46153, #57405, #41572, #25065, #51786, #19422, #18739, #8540, #66946, #61647, #25415, #56365, #14834, #9224, #36302, #35263, #57756, #9572, #52473, #40199, #3597, #13465, #8187, #13801, #34923, #29632, #51101, #2910, #24373, #45817, #67296, #19080, #40532, #40881, #61984, #56721, #29987, #46495, #67628, #67978, #62343 ),
 .UNSPECIFIED., .F., .F.,
 ( 4, 2, 2, 2, 2, 2, 2, 2, 2, 2, 2, 2, 2, 2, 2, 2, 2, 2, 2, 2, 2, 4 ),
 ( 0.02416815208377489851, 0.02567033257376874489, 0.02642142281876567328, 0.02717251306376259820, 0.02867469355375640988, 0.02942578379875333480, 0.03017687404375025625, 0.03167905453374411651, 0.03318123502373797329, 0.03393232526873489474, 0.03468341551373183007, 0.03618559600372571461, 0.03693668624872264300, 0.03768777649371957139, 0.03918995698371341430, 0.04069213747370725720, 0.04219431796370110010, 0.04369649845369494301, 0.04444758869869186446, 0.04519867894368878591, 0.04670085943368267045, 0.04820303992367655499 ),
 .UNSPECIFIED. ) ;
#15454 = LINE ( 'NONE', #42177, #35460 ) ;
#15455 = CARTESIAN_POINT ( 'NONE',  ( 141.2470358420065679, 46.06959063280891087, 65.16002587109025512 ) ) ;
#15456 = CARTESIAN_POINT ( 'NONE',  ( 21.27121078971613244, 61.42097029141973508, 40.00000000000003553 ) ) ;
#15457 = CARTESIAN_POINT ( 'NONE',  ( 155.2910738464913436, 55.97560547655807994, 56.56338629075234081 ) ) ;
#15458 = CARTESIAN_POINT ( 'NONE',  ( 94.02499804464929412, 23.15433260743126453, 38.48408892620923183 ) ) ;
#15459 = ORIENTED_EDGE ( 'NONE', *, *, #1674, .T. ) ;
#15460 = CARTESIAN_POINT ( 'NONE',  ( 259.4165763529819060, -27.00000000000000355, 128.9999999999999716 ) ) ;
#15461 = VERTEX_POINT ( 'NONE', #64882 ) ;
#15462 = CARTESIAN_POINT ( 'NONE',  ( 149.9714610887121466, 53.28792066194168342, -17.08704249943660969 ) ) ;
#15463 = CARTESIAN_POINT ( 'NONE',  ( 209.6642862813004911, 115.2127693334914085, -22.61907644621658164 ) ) ;
#15464 = DIRECTION ( 'NONE',  ( 0.000000000000000000, 0.000000000000000000, 1.000000000000000000 ) ) ;
#15465 = LINE ( 'NONE', #43204, #5219 ) ;
#15466 = AXIS2_PLACEMENT_3D ( 'NONE', #59966, #12852, #23745 ) ;
#15467 = CARTESIAN_POINT ( 'NONE',  ( 69.85706361178125690, 14.36422398738209161, 87.91050011282558785 ) ) ;
#15468 = CARTESIAN_POINT ( 'NONE',  ( -84.49322488516129681, 0.000000000000000000, 43.58025477438756212 ) ) ;
#15469 = DIRECTION ( 'NONE',  ( 0.000000000000000000, 0.000000000000000000, -1.000000000000000000 ) ) ;
#15470 = FACE_OUTER_BOUND ( 'NONE', #32745, .T. ) ;
#15471 = ORIENTED_EDGE ( 'NONE', *, *, #37409, .F. ) ;
#15472 = CIRCLE ( 'NONE', #33452, 10.00000000000000000 ) ;
#15473 = EDGE_CURVE ( 'NONE', #36451, #30352, #42383, .T. ) ;
#15474 = DIRECTION ( 'NONE',  ( 1.000000000000000000, 0.000000000000000000, 0.000000000000000000 ) ) ;
#15475 = EDGE_LOOP ( 'NONE', ( #45403, #65208, #16648, #4174 ) ) ;
#15476 = SURFACE_STYLE_USAGE ( .BOTH. , #52740 ) ;
#15477 = CARTESIAN_POINT ( 'NONE',  ( 206.6955592216990567, 109.1214665502617720, -77.91101188158484092 ) ) ;
#15478 = CARTESIAN_POINT ( 'NONE',  ( 43.14565945994674223, 9.942782559600559011, -22.77872216780330916 ) ) ;
#15479 = AXIS2_PLACEMENT_3D ( 'NONE', #23477, #13947, #7647 ) ;
#15480 = DIRECTION ( 'NONE',  ( 1.000000000000000000, -0.000000000000000000, -0.000000000000000000 ) ) ;
#15481 = DIRECTION ( 'NONE',  ( 1.000000000000000000, 0.000000000000000000, 0.000000000000000000 ) ) ;
#15482 =( GEOMETRIC_REPRESENTATION_CONTEXT ( 3 ) GLOBAL_UNCERTAINTY_ASSIGNED_CONTEXT ( ( #44465 ) ) GLOBAL_UNIT_ASSIGNED_CONTEXT ( ( #3673, #46579, #15270 ) ) REPRESENTATION_CONTEXT ( 'NONE', 'WORKASPACE' ) );
#15483 = DIRECTION ( 'NONE',  ( 1.000000000000000000, 0.000000000000000000, 0.000000000000000000 ) ) ;
#15484 = ORIENTED_EDGE ( 'NONE', *, *, #9879, .T. ) ;
#15485 = CARTESIAN_POINT ( 'NONE',  ( -75.43953471071002070, 21.11829282998123958, 57.97565906622840970 ) ) ;
#15486 = CARTESIAN_POINT ( 'NONE',  ( -3.566018980795016002, -51.54211481249757298, 26.66469104408689006 ) ) ;
#15487 = ORIENTED_EDGE ( 'NONE', *, *, #23985, .T. ) ;
#15488 = EDGE_LOOP ( 'NONE', ( #19512, #10711, #1129, #53974 ) ) ;
#15489 = EDGE_CURVE ( 'NONE', #39831, #35076, #21959, .T. ) ;
#15490 = ADVANCED_FACE ( 'NONE', ( #31829 ), #16339, .T. ) ;
#15491 = CARTESIAN_POINT ( 'NONE',  ( -155.5978531700835674, 69.52241200678679434, 42.60492188881196540 ) ) ;
#15492 = DIRECTION ( 'NONE',  ( 0.000000000000000000, 1.000000000000000000, 0.000000000000000000 ) ) ;
#15493 = CARTESIAN_POINT ( 'NONE',  ( 2.905661822261151883E-14, 20.55634918610402906, 0.000000000000000000 ) ) ;
#15494 = EDGE_CURVE ( 'NONE', #1914, #37583, #24276, .T. ) ;
#15495 = DIRECTION ( 'NONE',  ( 0.000000000000000000, 0.000000000000000000, 1.000000000000000000 ) ) ;
#15496 = CIRCLE ( 'NONE', #48004, 5.000000000000004441 ) ;
#15497 = CARTESIAN_POINT ( 'NONE',  ( 0.000000000000000000, 0.000000000000000000, 41.38025477438755928 ) ) ;
#15498 = EDGE_CURVE ( 'NONE', #21309, #25475, #15654, .T. ) ;
#15499 = ORIENTED_EDGE ( 'NONE', *, *, #30895, .F. ) ;
#15500 = EDGE_CURVE ( 'NONE', #7966, #63543, #5439, .T. ) ;
#15501 = CARTESIAN_POINT ( 'NONE',  ( -133.3923804760466112, 52.87100816290224969, 37.55266435330955233 ) ) ;
#15502 = ORIENTED_EDGE ( 'NONE', *, *, #41580, .F. ) ;
#15503 = CARTESIAN_POINT ( 'NONE',  ( 33.93974911725171495, 8.773765372885575786, -21.42055978403731942 ) ) ;
#15504 = CARTESIAN_POINT ( 'NONE',  ( 185.4510914867138354, 84.60702097455163084, -91.30541823130347723 ) ) ;
#15505 = CARTESIAN_POINT ( 'NONE',  ( 56.19211641164837090, 11.19288081156168424, 61.03486635809458960 ) ) ;
#15506 = CARTESIAN_POINT ( 'NONE',  ( -2.177337698256115672, 7.595833446947581002, 69.41885401754487361 ) ) ;
#15507 = CARTESIAN_POINT ( 'NONE',  ( 15.78827728214693416, 7.507518794609588042, 3.170157082241545687 ) ) ;
#15508 = VERTEX_POINT ( 'NONE', #34629 ) ;
#15509 = EDGE_LOOP ( 'NONE', ( #32307, #42326, #26888, #23575 ) ) ;
#15510 = CARTESIAN_POINT ( 'NONE',  ( -15.55634918610405748, -15.55634918610400774, 85.00100000000000477 ) ) ;
#15511 = DIRECTION ( 'NONE',  ( -0.5128992774058949156, -0.8584487936018728726, 0.000000000000000000 ) ) ;
#15512 = DIRECTION ( 'NONE',  ( -0.000000000000000000, 1.000000000000000000, -0.000000000000000000 ) ) ;
#15513 = FACE_OUTER_BOUND ( 'NONE', #53265, .T. ) ;
#15514 = CARTESIAN_POINT ( 'NONE',  ( 70.11438327604406595, 14.43198353181102789, 39.74598324287578066 ) ) ;
#15515 = EDGE_CURVE ( 'NONE', #59605, #42064, #38856, .T. ) ;
#15516 = CARTESIAN_POINT ( 'NONE',  ( 8.467009815279766372, 7.382848975951745274, 92.86400164404348345 ) ) ;
#15517 = EDGE_LOOP ( 'NONE', ( #27573, #40788, #27224, #60473 ) ) ;
#15518 = EDGE_CURVE ( 'NONE', #629, #37519, #41512, .T. ) ;
#15519 = DIRECTION ( 'NONE',  ( 1.850169831522831466E-16, -1.000000000000000000, 5.551115123125781470E-17 ) ) ;
#15520 = CARTESIAN_POINT ( 'NONE',  ( -96.76159256735193992, 30.06445763698413032, 69.96622681954906398 ) ) ;
#15521 = VERTEX_POINT ( 'NONE', #22660 ) ;
#15523 = CARTESIAN_POINT ( 'NONE',  ( -1.734723475976807094E-15, 9.237604307034022355, -0.7145311798163346273 ) ) ;
#15522 = AXIS2_PLACEMENT_3D ( 'NONE', #19120, #61686, #65951 ) ;
#15524 = ORIENTED_EDGE ( 'NONE', *, *, #17794, .T. ) ;
#15525 = ORIENTED_EDGE ( 'NONE', *, *, #56633, .F. ) ;
#15526 = ORIENTED_EDGE ( 'NONE', *, *, #46454, .F. ) ;
#15527 = CARTESIAN_POINT ( 'NONE',  ( -118.5151419614604578, 43.00218563933589166, 12.64493271249231654 ) ) ;
#15528 = CARTESIAN_POINT ( 'NONE',  ( -178.7458319892714087, 93.61502008198024782, 70.13378254355463071 ) ) ;
#15529 = VECTOR ( 'NONE', #17071, 1000.000000000000000 ) ;
#15530 = CARTESIAN_POINT ( 'NONE',  ( 19.75784582661441391, 6.660183274347841298, 17.03828975487343556 ) ) ;
#15531 = EDGE_LOOP ( 'NONE', ( #14463, #46753, #45833, #65304 ) ) ;
#15532 = CARTESIAN_POINT ( 'NONE',  ( -33.66596729176688996, 9.967356680381493916, 84.23666802118060559 ) ) ;
#15533 = CIRCLE ( 'NONE', #919, 243.4957430088094839 ) ;
#15534 = CARTESIAN_POINT ( 'NONE',  ( 150.0433793199863146, 52.09973307442955814, 35.82920141195970842 ) ) ;
#15535 = LINE ( 'NONE', #52798, #3345 ) ;
#15536 = CARTESIAN_POINT ( 'NONE',  ( 103.5588133492864955, 25.91050225236391569, -46.86172722952704817 ) ) ;
#15537 = B_SPLINE_CURVE_WITH_KNOTS ( 'NONE', 3,
 ( #52329, #51983, #57952, #47382, #9773, #4153 ),
 .UNSPECIFIED., .F., .F.,
 ( 4, 2, 4 ),
 ( 0.03218936187311347008, 0.06469833704501400107, 0.09720731221691453205 ),
 .UNSPECIFIED. ) ;
#15538 = CARTESIAN_POINT ( 'NONE',  ( -29.49620345460275317, 9.280093073089041411, 44.97709496270313423 ) ) ;
#15539 = CARTESIAN_POINT ( 'NONE',  ( 0.000000000000000000, 0.000000000000000000, 7.000000000000000000 ) ) ;
#15540 = ORIENTED_EDGE ( 'NONE', *, *, #60899, .F. ) ;
#15541 = DIRECTION ( 'NONE',  ( -0.000000000000000000, -0.000000000000000000, 1.000000000000000000 ) ) ;
#15542 = CARTESIAN_POINT ( 'NONE',  ( -3.319543390096040714, 7.321065037175420898, -9.483111142572234087 ) ) ;
#15543 = CARTESIAN_POINT ( 'NONE',  ( -25.00000000000000000, 65.13282190615278466, -5.000000000000000000 ) ) ;
#15544 = CARTESIAN_POINT ( 'NONE',  ( -118.7011544766493500, 43.11604763363183679, -40.27239875278853987 ) ) ;
#15545 = CARTESIAN_POINT ( 'NONE',  ( -78.66644367742111399, 23.39876645725285798, 18.57365054920947500 ) ) ;
#15546 = LINE ( 'NONE', #38031, #21353 ) ;
#15547 = CARTESIAN_POINT ( 'NONE',  ( -156.6819053601226415, 70.51177710383655040, 13.63498518674871107 ) ) ;
#15548 = CARTESIAN_POINT ( 'NONE',  ( -122.3994536713185255, 45.42826354555017332, -62.61790137560624459 ) ) ;
#15549 = EDGE_CURVE ( 'NONE', #23937, #16594, #28639, .T. ) ;
#15550 = FACE_OUTER_BOUND ( 'NONE', #14070, .T. ) ;
#15551 = CARTESIAN_POINT ( 'NONE',  ( -86.10360257264196093, 26.38663017581290404, 65.76492460684757191 ) ) ;
#15552 = CARTESIAN_POINT ( 'NONE',  ( -105.8768181937898873, 34.64545164169051361, 44.61740776510733042 ) ) ;
#15553 = EDGE_LOOP ( 'NONE', ( #22920, #27993, #45447, #2675, #2827, #58539, #43391, #13034, #69482 ) ) ;
#15554 = EDGE_CURVE ( 'NONE', #56212, #66914, #6829, .T. ) ;
#15555 = ITEM_DEFINED_TRANSFORMATION ( 'NONE', 'NONE', #20856,  #66832 ) ;
#15556 = CARTESIAN_POINT ( 'NONE',  ( -61.76967730161514680, 17.63609381203634641, 88.10797299145480110 ) ) ;
#15557 = ORIENTED_EDGE ( 'NONE', *, *, #67271, .F. ) ;
#15558 = LINE ( 'NONE', #10958, #32899 ) ;
#15559 = ORIENTED_EDGE ( 'NONE', *, *, #29174, .F. ) ;
#15560 = CARTESIAN_POINT ( 'NONE',  ( 15.78827728214693771, 7.507518794609575608, -62.36349468914946925 ) ) ;
#15561 = DIRECTION ( 'NONE',  ( 1.000000000000000000, 0.000000000000000000, 0.000000000000000000 ) ) ;
#15562 = FACE_OUTER_BOUND ( 'NONE', #51519, .T. ) ;
#15563 = CARTESIAN_POINT ( 'NONE',  ( 110.0000000000000284, 21.42428528562853529, -5.000000000000004441 ) ) ;
#15564 = DIRECTION ( 'NONE',  ( -0.000000000000000000, -0.000000000000000000, 1.000000000000000000 ) ) ;
#15565 = CARTESIAN_POINT ( 'NONE',  ( -49.12372073857198984, 14.20664392157176081, -74.18029338664986483 ) ) ;
#15566 = DIRECTION ( 'NONE',  ( 1.000000000000000000, 0.000000000000000000, 0.000000000000000000 ) ) ;
#15567 = CARTESIAN_POINT ( 'NONE',  ( -11.97857120004195330, -31.20571949911692045, 6.893342933292192498 ) ) ;
#15568 = ORIENTED_EDGE ( 'NONE', *, *, #53429, .F. ) ;
#15569 = ORIENTED_EDGE ( 'NONE', *, *, #5320, .T. ) ;
#15570 = EDGE_CURVE ( 'NONE', #8876, #17506, #29318, .T. ) ;
#15571 = VECTOR ( 'NONE', #64812, 1000.000000000000000 ) ;
#15572 = CARTESIAN_POINT ( 'NONE',  ( 8.000000000000007105, 249.8719672152120381, 94.99999999999866418 ) ) ;
#15573 = SURFACE_STYLE_FILL_AREA ( #63765 ) ;
#15574 = DIRECTION ( 'NONE',  ( 0.9909497617679351444, -0.1342332658176522420, -2.292031753669949326E-16 ) ) ;
#15575 = EDGE_CURVE ( 'NONE', #7569, #26944, #16833, .T. ) ;
#15576 = AXIS2_PLACEMENT_3D ( 'NONE', #22426, #27344, #60411 ) ;
#15577 = ADVANCED_FACE ( 'NONE', ( #1923 ), #45153, .F. ) ;
#15578 = PRODUCT_DEFINITION_CONTEXT ( 'detailed design', #55716, 'design' ) ;
#15579 = DIRECTION ( 'NONE',  ( -0.000000000000000000, -0.000000000000000000, -1.000000000000000000 ) ) ;
#15580 = EDGE_CURVE ( 'NONE', #66935, #45299, #49408, .T. ) ;
#15581 = VECTOR ( 'NONE', #57340, 1000.000000000000000 ) ;
#15582 = CARTESIAN_POINT ( 'NONE',  ( 281.3030933484816956, 21.46146164524276045, 4.838392277045652001 ) ) ;
#15583 = LINE ( 'NONE', #14200, #2030 ) ;
#15584 = CARTESIAN_POINT ( 'NONE',  ( 208.0306608271318112, 112.7988899307265456, 3.141066733790039311 ) ) ;
#15585 = CYLINDRICAL_SURFACE ( 'NONE', #14930, 5.000000000000000000 ) ;
#15586 = CARTESIAN_POINT ( 'NONE',  ( 90.30166390191402570, 20.70652093100729374, -23.03453807668526565 ) ) ;
#15587 = CARTESIAN_POINT ( 'NONE',  ( 204.6977192012829789, 106.3443248447423599, -24.48138044215792419 ) ) ;
#15588 = FACE_OUTER_BOUND ( 'NONE', #24203, .T. ) ;
#15589 = CARTESIAN_POINT ( 'NONE',  ( 3.000000000000006217, 2.877919977996280320E-15, 23.50000000000000000 ) ) ;
#15590 = ORIENTED_EDGE ( 'NONE', *, *, #35893, .T. ) ;
#15591 = DIRECTION ( 'NONE',  ( -1.000000000000000000, 0.000000000000000000, -0.000000000000000000 ) ) ;
#15592 = CARTESIAN_POINT ( 'NONE',  ( 9.737557066527559257, 200.0000000000000000, 2.275957463600584596 ) ) ;
#15593 = CYLINDRICAL_SURFACE ( 'NONE', #28496, 7.500000000000013323 ) ;
#15594 = FACE_OUTER_BOUND ( 'NONE', #29501, .T. ) ;
#15595 = CARTESIAN_POINT ( 'NONE',  ( 437.3372781065085633, 400.0000000000000568, -136.4497041420118251 ) ) ;
#15596 = CARTESIAN_POINT ( 'NONE',  ( -10.07362276049133953, 8.056690395595460075, 84.14207705956837913 ) ) ;
#15597 = EDGE_LOOP ( 'NONE', ( #26924, #53780, #22293, #10301 ) ) ;
#15598 = ADVANCED_FACE ( 'NONE', ( #32492 ), #32835, .F. ) ;
#15599 = CARTESIAN_POINT ( 'NONE',  ( 0.4988340113715861723, 3.871605243926953044, 7.999999999999998224 ) ) ;
#15600 = DIRECTION ( 'NONE',  ( 1.000000000000000000, 0.000000000000000000, 0.000000000000000000 ) ) ;
#15601 = VERTEX_POINT ( 'NONE', #60267 ) ;
#15602 = VERTEX_POINT ( 'NONE', #26868 ) ;
#15603 = CARTESIAN_POINT ( 'NONE',  ( 36.21632519057887833, 9.028958671447663065, 84.28089839341768652 ) ) ;
#15604 = CARTESIAN_POINT ( 'NONE',  ( -179.5082312244189211, 94.53075638132055758, -72.99655709447104357 ) ) ;
#15605 = CYLINDRICAL_SURFACE ( 'NONE', #68446, 7.500000000000020428 ) ;
#15606 = EDGE_LOOP ( 'NONE', ( #7757, #50618, #65105 ) ) ;
#15607 = CARTESIAN_POINT ( 'NONE',  ( 15.78827728214693416, -170.0000000000000000, -43.01894409868580027 ) ) ;
#15608 = CARTESIAN_POINT ( 'NONE',  ( 157.4703587214989398, -170.0000000000000000, -70.46873488960132192 ) ) ;
#15609 = CARTESIAN_POINT ( 'NONE',  ( -5.879983509979045841, 7.779504553499513975, 3.511211028316594707 ) ) ;
#15610 = CARTESIAN_POINT ( 'NONE',  ( 178.1965488566140436, 77.14488558164484289, -50.66031209579180228 ) ) ;
#15611 = DIRECTION ( 'NONE',  ( 0.000000000000000000, 0.000000000000000000, 1.000000000000000000 ) ) ;
#15612 = FACE_OUTER_BOUND ( 'NONE', #10998, .T. ) ;
#15613 = ORIENTED_EDGE ( 'NONE', *, *, #45094, .T. ) ;
#15614 = CARTESIAN_POINT ( 'NONE',  ( 103.0124792097646349, 26.77148435100179569, -18.63633658775954061 ) ) ;
#15615 = FACE_OUTER_BOUND ( 'NONE', #35056, .T. ) ;
#15616 = CARTESIAN_POINT ( 'NONE',  ( 9.837735240994037511, 7.389327806910500840, 32.94284116154079811 ) ) ;
#15617 = CARTESIAN_POINT ( 'NONE',  ( 197.6341357773624452, 98.74251867088338486, 39.24647996897417102 ) ) ;
#15618 = AXIS2_PLACEMENT_3D ( 'NONE', #45972, #51939, #19231 ) ;
#15619 = CYLINDRICAL_SURFACE ( 'NONE', #33224, 7.500000000000013323 ) ;
#15621 = ORIENTED_EDGE ( 'NONE', *, *, #47260, .T. ) ;
#15620 = LINE ( 'NONE', #64146, #23073 ) ;
#15622 = VERTEX_POINT ( 'NONE', #38819 ) ;
#15623 = PRESENTATION_LAYER_ASSIGNMENT (  '', '', ( #40332 ) ) ;
#15625 = ORIENTED_EDGE ( 'NONE', *, *, #55396, .T. ) ;
#15624 = EDGE_CURVE ( 'NONE', #47669, #47023, #17518, .T. ) ;
#15626 = CARTESIAN_POINT ( 'NONE',  ( 115.0606351894211485, 32.29586232625066344, -76.03609025758434825 ) ) ;
#15627 = FACE_OUTER_BOUND ( 'NONE', #15427, .T. ) ;
#15628 = DIRECTION ( 'NONE',  ( 1.000000000000000000, 0.000000000000000000, -0.000000000000000000 ) ) ;
#15629 = CARTESIAN_POINT ( 'NONE',  ( -31.11269837220812207, -26.11269837220801193, 85.00100000000000477 ) ) ;
#15630 = EDGE_CURVE ( 'NONE', #39142, #42011, #24380, .T. ) ;
#15631 = CARTESIAN_POINT ( 'NONE',  ( -15.32495246574475090, 8.506829480038508251, -16.57547917308654206 ) ) ;
#15632 = CARTESIAN_POINT ( 'NONE',  ( 60.82895951008336510, 30.68107831874607072, 170.0000000000000000 ) ) ;
#15633 = CARTESIAN_POINT ( 'NONE',  ( 157.4703587214989113, 57.65129005721576760, -77.96873488960135035 ) ) ;
#15634 = ADVANCED_FACE ( 'NONE', ( #1891 ), #12432, .F. ) ;
#15635 = CARTESIAN_POINT ( 'NONE',  ( -156.7487895666416478, 70.57327586518564999, -44.28588653070858783 ) ) ;
#15636 = VERTEX_POINT ( 'NONE', #8545 ) ;
#15637 = ORIENTED_EDGE ( 'NONE', *, *, #44198, .T. ) ;
#15638 = CARTESIAN_POINT ( 'NONE',  ( 70.45451534980408326, 15.56315969138428379, -17.36384710539488552 ) ) ;
#15639 = ADVANCED_FACE ( 'NONE', ( #45471 ), #19086, .F. ) ;
#15640 = CARTESIAN_POINT ( 'NONE',  ( -62.41990535723909517, 17.83270318706536983, -95.00000000000133582 ) ) ;
#15641 = CARTESIAN_POINT ( 'NONE',  ( 109.6602010289487055, 28.61221948077516686, 83.29575177580451850 ) ) ;
#15642 = CARTESIAN_POINT ( 'NONE',  ( -156.4797890011541881, 71.69341087347116570, 8.599111263860363508 ) ) ;
#15643 = CARTESIAN_POINT ( 'NONE',  ( 188.5662303205147055, 86.51341602961788624, -43.12654626515958967 ) ) ;
#15644 = CARTESIAN_POINT ( 'NONE',  ( 21.44031696305385637, 6.747195267824410259, 42.46889706688644850 ) ) ;
#15645 = CARTESIAN_POINT ( 'NONE',  ( -156.5226901298209725, 71.73305092143021966, 89.25176612992051162 ) ) ;
#15646 = VERTEX_POINT ( 'NONE', #40205 ) ;
#15647 = ORIENTED_EDGE ( 'NONE', *, *, #25925, .T. ) ;
#15648 = ORIENTED_EDGE ( 'NONE', *, *, #3031, .F. ) ;
#15649 =( NAMED_UNIT ( * ) PLANE_ANGLE_UNIT ( ) SI_UNIT ( $, .RADIAN. ) );
#15650 = CARTESIAN_POINT ( 'NONE',  ( 92.56307064175635446, 22.60487289243135223, -92.40539893235690272 ) ) ;
#15651 = EDGE_CURVE ( 'NONE', #772, #4364, #61653, .T. ) ;
#15652 = DIRECTION ( 'NONE',  ( 0.000000000000000000, 0.000000000000000000, 1.000000000000000000 ) ) ;
#15653 = EDGE_CURVE ( 'NONE', #66979, #59078, #16641, .T. ) ;
#15654 = LINE ( 'NONE', #64528, #19166 ) ;
#15655 = CIRCLE ( 'NONE', #39266, 25.12245591505646303 ) ;
#15656 = CARTESIAN_POINT ( 'NONE',  ( 112.3013380801406385, 400.0000000000077307, 96.05029585798746439 ) ) ;
#15657 = ORIENTED_EDGE ( 'NONE', *, *, #30028, .F. ) ;
#15658 = CARTESIAN_POINT ( 'NONE',  ( 185.5457097283154440, 84.70846743303872017, 69.69978301039404300 ) ) ;
#15659 = CARTESIAN_POINT ( 'NONE',  ( 12.03194517566456057, 6.409266703743584870, -9.664381073535908584 ) ) ;
#15660 = B_SPLINE_CURVE_WITH_KNOTS ( 'NONE', 3,
 ( #17266, #44713, #66191, #16919, #38383, #66533, #7073, #49619, #49268, #38740, #1450, #59824, #60184, #17984, #1102, #54190, #22553, #12003, #33477, #22904, #44350, #34168, #28531, #65833, #60539, #17629, #12353, #49980, #38035, #33810, #60881, #12703, #55606, #7436, #50339, #59479, #11290, #56649, #13738, #8118 ),
 .UNSPECIFIED., .F., .F.,
 ( 4, 2, 2, 2, 2, 2, 2, 2, 2, 2, 2, 2, 2, 2, 2, 2, 2, 2, 2, 4 ),
 ( 0.02454308262169001276, 0.02608670964102879908, 0.02685852315069820612, 0.02763033666036761662, 0.02917396367970642723, 0.02994577718937583427, 0.03071759069904523784, 0.03226121771838406926, 0.03303303122805349018, 0.03380484473772291804, 0.03534847175706176681, 0.03689209877640062252, 0.03843572579573947129, 0.03997935281507832006, 0.04152297983441717577, 0.04306660685375602454, 0.04461023387309488719, 0.04615386089243374984, 0.04769748791177261249, 0.04924111493111147514 ),
 .UNSPECIFIED. ) ;
#15661 = DIRECTION ( 'NONE',  ( -0.000000000000000000, -1.000000000000000000, -0.000000000000000000 ) ) ;
#15662 = CARTESIAN_POINT ( 'NONE',  ( 182.5617509987553433, 80.11195108039726165, 56.29705353328592565 ) ) ;
#15663 = DIRECTION ( 'NONE',  ( 0.000000000000000000, -1.000000000000000000, 0.000000000000000000 ) ) ;
#15664 = CARTESIAN_POINT ( 'NONE',  ( -79.14678386417813272, 22.50468917936073154, -35.11545063171787717 ) ) ;
#15665 = CARTESIAN_POINT ( 'NONE',  ( 18.21423326326596381, 6.590134686181386314, 71.47284841903351094 ) ) ;
#15666 = DIRECTION ( 'NONE',  ( -0.3090169943749582759, 0.9510565162951499785, 0.000000000000000000 ) ) ;
#15667 = CARTESIAN_POINT ( 'NONE',  ( 69.36122620657974380, 15.27447566922079858, 94.99999999999866418 ) ) ;
#15668 = AXIS2_PLACEMENT_3D ( 'NONE', #63807, #32479, #53912 ) ;
#15669 = ORIENTED_EDGE ( 'NONE', *, *, #14397, .F. ) ;
#15670 = DIRECTION ( 'NONE',  ( 0.000000000000000000, 0.000000000000000000, 1.000000000000000000 ) ) ;
#15671 = APPLICATION_PROTOCOL_DEFINITION ( 'draft international standard', 'automotive_design', 1998, #17920 ) ;
#15672 = CARTESIAN_POINT ( 'NONE',  ( 0.000000000000000000, 0.000000000000000000, 170.0000000000000000 ) ) ;
#15673 = FACE_OUTER_BOUND ( 'NONE', #47950, .T. ) ;
#15674 = CARTESIAN_POINT ( 'NONE',  ( -108.0902552660050731, 36.97681740369924341, -47.28325963604802951 ) ) ;
#15675 = VECTOR ( 'NONE', #41384, 1000.000000000000000 ) ;
#15676 = CARTESIAN_POINT ( 'NONE',  ( -1.118033988749894458, 0.000000000000000000, -21.50000000000000000 ) ) ;
#15677 = ORIENTED_EDGE ( 'NONE', *, *, #18261, .T. ) ;
#15678 = EDGE_LOOP ( 'NONE', ( #19362, #4626 ) ) ;
#15679 = CARTESIAN_POINT ( 'NONE',  ( -30.94753041835916818, 9.510749728915508072, -8.472646774738157305 ) ) ;
#15680 = CARTESIAN_POINT ( 'NONE',  ( 174.4089829827045435, 72.11302376861458185, 93.92229883193532203 ) ) ;
#15681 = ORIENTED_EDGE ( 'NONE', *, *, #51043, .F. ) ;
#15682 = CARTESIAN_POINT ( 'NONE',  ( -31.43908319763710679, -170.0000000000000000, 10.87190381572550280 ) ) ;
#15683 = ORIENTED_EDGE ( 'NONE', *, *, #15630, .T. ) ;
#15684 = CARTESIAN_POINT ( 'NONE',  ( 130.3035708464390154, 40.48418876551454559, -63.74550792924027576 ) ) ;
#15685 = DIRECTION ( 'NONE',  ( -1.000000000000000000, 0.000000000000000000, 0.000000000000000000 ) ) ;
#15686 = B_SPLINE_CURVE_WITH_KNOTS ( 'NONE', 3,
 ( #19663, #29879, #67866, #62927, #14043, #51340, #14400, #19315, #4523, #3836, #9809, #24612, #30923, #25307, #68210, #20020, #41474, #52696, #14727, #56603, #68546, #36542, #68871, #57651, #67516, #20695, #46046, #42156, #40770, #9462, #20348, #56963, #52367, #4183, #25652, #30230, #3485, #41817 ),
 .UNSPECIFIED., .F., .F.,
 ( 4, 2, 2, 2, 2, 2, 2, 2, 2, 2, 2, 2, 2, 2, 2, 2, 2, 2, 4 ),
 ( 0.000000000000000000, 0.003908178031105456751, 0.005862267046658146095, 0.007816356062210835440, 0.009770445077763523917, 0.01172453409331621413, 0.01270157860109255230, 0.01367862310886889046, 0.01465566761664522863, 0.01563271212442156680, 0.01660975663219790843, 0.01758680113997424660, 0.01954089015552693681, 0.02051793466330329579, 0.02149497917107965825, 0.02344906818663237622, 0.02540315720218510112, 0.02735724621773782256, 0.03126542424884323074 ),
 .UNSPECIFIED. ) ;
#15687 = CARTESIAN_POINT ( 'NONE',  ( -24.85653282846401879, 8.603185326828743484, 94.99999999999866418 ) ) ;
#15688 = VECTOR ( 'NONE', #1429, 1000.000000000000000 ) ;
#15689 = CARTESIAN_POINT ( 'NONE',  ( 163.6501672645067345, 62.62019911992669563, -93.05832839351816688 ) ) ;
#15690 = CARTESIAN_POINT ( 'NONE',  ( 90.30166390191405412, 20.70652093100728663, -49.87908866714894884 ) ) ;
#15692 = ORIENTED_EDGE ( 'NONE', *, *, #52767, .T. ) ;
#15691 = FACE_OUTER_BOUND ( 'NONE', #46295, .T. ) ;
#15693 = ORIENTED_EDGE ( 'NONE', *, *, #31734, .F. ) ;
#15694 = ORIENTED_EDGE ( 'NONE', *, *, #53873, .T. ) ;
#15695 = CARTESIAN_POINT ( 'NONE',  ( -118.4553071845215015, 41.78724769484927037, -16.66711030142431937 ) ) ;
#15696 = CARTESIAN_POINT ( 'NONE',  ( 74.62299871641508275, -5.461138973197949831, 170.0000000000000000 ) ) ;
#15697 = CARTESIAN_POINT ( 'NONE',  ( -177.5259994307673423, 92.16784265327252967, -21.45548079138242059 ) ) ;
#15698 = CARTESIAN_POINT ( 'NONE',  ( -169.8972248494843029, 85.08697738648014308, -62.26996028157370944 ) ) ;
#15700 = ORIENTED_EDGE ( 'NONE', *, *, #53146, .T. ) ;
#15699 = CARTESIAN_POINT ( 'NONE',  ( -145.3279998500303805, 60.71393190715793509, -48.54482469514504572 ) ) ;
#15701 = CARTESIAN_POINT ( 'NONE',  ( -109.4616842129796339, 37.73062014485820015, 89.52162112396747773 ) ) ;
#15702 = VECTOR ( 'NONE', #66791, 1000.000000000000000 ) ;
#15703 = VERTEX_POINT ( 'NONE', #33890 ) ;
#15704 = CARTESIAN_POINT ( 'NONE',  ( -128.9786047358386156, 48.55852351614669971, 44.96012683757445672 ) ) ;
#15705 = CARTESIAN_POINT ( 'NONE',  ( -125.8938041572051389, -170.0000000000000000, -96.10280507916131398 ) ) ;
#15706 = EDGE_CURVE ( 'NONE', #20401, #36151, #51107, .T. ) ;
#15707 = CARTESIAN_POINT ( 'NONE',  ( 86.15410276028863734, 19.25894675708890702, -23.97701360844807184 ) ) ;
#15708 = CARTESIAN_POINT ( 'NONE',  ( -130.2071229607962835, 50.62285182196875866, -63.10483451847541403 ) ) ;
#15709 = DIRECTION ( 'NONE',  ( 0.9839295885986321100, -0.1785568947986229116, 0.000000000000000000 ) ) ;
#15710 = EDGE_CURVE ( 'NONE', #63707, #275, #23408, .T. ) ;
#15711 = DIRECTION ( 'NONE',  ( 0.000000000000000000, 0.000000000000000000, -1.000000000000000000 ) ) ;
#15712 = CARTESIAN_POINT ( 'NONE',  ( -94.78109144324895396, 29.13179392050638228, -69.64435539242961681 ) ) ;
#15713 = ORIENTED_EDGE ( 'NONE', *, *, #6455, .T. ) ;
#15714 = ORIENTED_EDGE ( 'NONE', *, *, #5238, .T. ) ;
#15715 = EDGE_CURVE ( 'NONE', #53047, #58120, #68650, .T. ) ;
#15716 = CARTESIAN_POINT ( 'NONE',  ( 0.000000000000000000, 0.000000000000000000, -0.002000000000002000178 ) ) ;
#15717 = CARTESIAN_POINT ( 'NONE',  ( -172.7116702014380110, 86.67317892691259829, -34.71195716474999671 ) ) ;
#15718 = CARTESIAN_POINT ( 'NONE',  ( -31.11269837220804035, 15.55634918610408945, 85.00100000000000477 ) ) ;
#15719 = CONICAL_SURFACE ( 'NONE', #32590, 5.000000000000000888, 0.9599310885968810325 ) ;
#15720 = CARTESIAN_POINT ( 'NONE',  ( 442.3372781065085064, 390.0000000000001137, -146.4497041420117966 ) ) ;
#15721 = CARTESIAN_POINT ( 'NONE',  ( -76.32456871438918711, 22.51591205926308348, 30.77704971272454770 ) ) ;
#15722 = CARTESIAN_POINT ( 'NONE',  ( -71.97171223898807568, 20.94894057408426491, -66.04217098637484185 ) ) ;
#15723 = CARTESIAN_POINT ( 'NONE',  ( 66.73431804020511038, 14.60294556126670784, -49.73844288260944069 ) ) ;
#15724 = CARTESIAN_POINT ( 'NONE',  ( 46.89016064832838993, 10.52130577388959409, -43.60800750508858670 ) ) ;
#15725 = DIRECTION ( 'NONE',  ( 1.000000000000000000, 0.000000000000000000, -0.000000000000000000 ) ) ;
#15726 = ORIENTED_EDGE ( 'NONE', *, *, #40483, .T. ) ;
#15727 = CARTESIAN_POINT ( 'NONE',  ( -104.5730787903383288, 33.96058035148152499, -8.513426699022396349 ) ) ;
#15728 = EDGE_LOOP ( 'NONE', ( #11026, #2337, #6739, #25003 ) ) ;
#15729 = CARTESIAN_POINT ( 'NONE',  ( -31.43908319763709969, 9.591432048623765638, 3.371903815725488585 ) ) ;
#15730 = CARTESIAN_POINT ( 'NONE',  ( 56.74421265833604622, -32.44697398030825042, 43.58025477438756212 ) ) ;
#15731 = CARTESIAN_POINT ( 'NONE',  ( -85.34581468285759343, 24.97911134307621950, -92.86422577895648089 ) ) ;
#15732 = EDGE_CURVE ( 'NONE', #23369, #55648, #43546, .T. ) ;
#15733 = CARTESIAN_POINT ( 'NONE',  ( 151.6192474229129630, 53.24103268919208176, -21.47852014988733060 ) ) ;
#15734 = CYLINDRICAL_SURFACE ( 'NONE', #55698, 7.500000000000020428 ) ;
#15735 = CARTESIAN_POINT ( 'NONE',  ( 38.91493890549796220, 8.346224043800610559, -77.46436805589146957 ) ) ;
#15736 = CARTESIAN_POINT ( 'NONE',  ( -35.00000000000002842, 225.0000000000000000, -2.000000000000000000 ) ) ;
#15737 = CIRCLE ( 'NONE', #8972, 65.00000000000000000 ) ;
#15738 = DIRECTION ( 'NONE',  ( -0.000000000000000000, 1.000000000000000000, -0.000000000000000000 ) ) ;
#15739 = VERTEX_POINT ( 'NONE', #15543 ) ;
#15740 = CARTESIAN_POINT ( 'NONE',  ( 444.9999999999999432, -35.00000000000000000, 0.000000000000000000 ) ) ;
#15741 = ORIENTED_EDGE ( 'NONE', *, *, #29471, .F. ) ;
#15742 = CARTESIAN_POINT ( 'NONE',  ( 62.05396267233467711, 13.48332220860127428, 56.70355666220334712 ) ) ;
#15743 = CARTESIAN_POINT ( 'NONE',  ( 10.15118267943871722, 7.391905976536037315, -74.81668340143906448 ) ) ;
#15744 = CARTESIAN_POINT ( 'NONE',  ( 31.11269837220806522, -6.375108774214766072E-14, 85.00100000000000477 ) ) ;
#15745 = DIRECTION ( 'NONE',  ( -0.000000000000000000, -0.000000000000000000, -1.000000000000000000 ) ) ;
#15746 = CARTESIAN_POINT ( 'NONE',  ( -1.319107422865893442, 6.554467368239795810, 33.85272720924916712 ) ) ;
#15747 = CARTESIAN_POINT ( 'NONE',  ( 230.9999999999999432, -35.00000000000000000, -2.000000000000000000 ) ) ;
#15748 = CARTESIAN_POINT ( 'NONE',  ( 10.55634918610406281, 20.55634918610400064, 0.000000000000000000 ) ) ;
#15749 =( REPRESENTATION_RELATIONSHIP ('NONE','NONE', #40274, #64096 ) REPRESENTATION_RELATIONSHIP_WITH_TRANSFORMATION ( #61101 )SHAPE_REPRESENTATION_RELATIONSHIP( ) );
#15750 = ORIENTED_EDGE ( 'NONE', *, *, #13596, .T. ) ;
#15751 = DIRECTION ( 'NONE',  ( 0.3957342950827489325, 2.220446049250313081E-16, 0.9183650514339923854 ) ) ;
#15752 = AXIS2_PLACEMENT_3D ( 'NONE', #44450, #11738, #65937 ) ;
#15753 = LINE ( 'NONE', #37900, #22818 ) ;
#15754 = CARTESIAN_POINT ( 'NONE',  ( 437.3372781065085633, 395.0000000000001137, -136.4497041420117966 ) ) ;
#15755 = B_SPLINE_CURVE_WITH_KNOTS ( 'NONE', 3,
 ( #65122, #49979, #12352, #33115, #22903, #39097 ),
 .UNSPECIFIED., .F., .F.,
 ( 4, 2, 4 ),
 ( 1.095770181115536239E-06, 0.03239442681617710901, 0.06478775786217311206 ),
 .UNSPECIFIED. ) ;
#15756 = CARTESIAN_POINT ( 'NONE',  ( -190.6985136298601731, 109.1272424661242582, 60.81597207375692449 ) ) ;
#15757 = CONTEXT_DEPENDENT_SHAPE_REPRESENTATION ( #30550, #38927 ) ;
#15758 = CARTESIAN_POINT ( 'NONE',  ( -180.2534575077006593, 95.43481063389138797, 94.35782419044186042 ) ) ;
#15759 = ORIENTED_EDGE ( 'NONE', *, *, #9367, .F. ) ;
#15760 = FACE_OUTER_BOUND ( 'NONE', #48289, .T. ) ;
#15761 = CARTESIAN_POINT ( 'NONE',  ( 93.33480479917547257, 21.81892021443992746, 67.45373393540474183 ) ) ;
#15762 = SURFACE_STYLE_USAGE ( .BOTH. , #27000 ) ;
#15763 = CARTESIAN_POINT ( 'NONE',  ( 0.000000000000000000, 0.000000000000000000, 41.38025477438755928 ) ) ;
#15764 = CARTESIAN_POINT ( 'NONE',  ( 140.0614732283738135, 45.29930344725072899, 32.78982767501074136 ) ) ;
#15765 = ORIENTED_EDGE ( 'NONE', *, *, #39188, .F. ) ;
#15766 = CARTESIAN_POINT ( 'NONE',  ( 0.000000000000000000, -6.928203230275503444, 4.000000000000010658 ) ) ;
#15767 = DIRECTION ( 'NONE',  ( -0.000000000000000000, 1.000000000000000000, -0.000000000000000000 ) ) ;
#15768 = CARTESIAN_POINT ( 'NONE',  ( 160.2883311361769927, 61.16711613734478448, 17.01903432654508563 ) ) ;
#15769 = DIRECTION ( 'NONE',  ( -1.000000000000000000, -0.000000000000000000, -1.334402673828313339E-16 ) ) ;
#15770 = AXIS2_PLACEMENT_3D ( 'NONE', #62506, #25224, #68794 ) ;
#15771 = ORIENTED_EDGE ( 'NONE', *, *, #61774, .T. ) ;
#15772 = EDGE_CURVE ( 'NONE', #1617, #58260, #62349, .T. ) ;
#15773 = CARTESIAN_POINT ( 'NONE',  ( 179.4227152810058499, 78.36166152262364903, 56.32724963102304372 ) ) ;
#15774 = ORIENTED_EDGE ( 'NONE', *, *, #66795, .T. ) ;
#15775 = EDGE_CURVE ( 'NONE', #44335, #54364, #3503, .T. ) ;
#15776 = CARTESIAN_POINT ( 'NONE',  ( -105.4556185321791446, 34.42302275449793569, -35.70349811333863244 ) ) ;
#15777 = CARTESIAN_POINT ( 'NONE',  ( 66.29961816943398389, 13.45804302849873757, -76.82535056491491332 ) ) ;
#15778 = CARTESIAN_POINT ( 'NONE',  ( -58.33245019990697955, 15.58496056636070293, 44.57971224376340302 ) ) ;
#15780 = ORIENTED_EDGE ( 'NONE', *, *, #4611, .F. ) ;
#15779 = FACE_OUTER_BOUND ( 'NONE', #52724, .T. ) ;
#15781 = CARTESIAN_POINT ( 'NONE',  ( -177.5271152834790769, 92.16916858125013334, 44.40871575690508166 ) ) ;
#15782 = VECTOR ( 'NONE', #34771, 1000.000000000000000 ) ;
#15783 = DIRECTION ( 'NONE',  ( 0.000000000000000000, 0.000000000000000000, -1.000000000000000000 ) ) ;
#15784 = CARTESIAN_POINT ( 'NONE',  ( 112.1009898303695422, 30.86414810229296890, -36.14121760344119849 ) ) ;
#15785 = VERTEX_POINT ( 'NONE', #42272 ) ;
#15786 = DIRECTION ( 'NONE',  ( -0.000000000000000000, 0.000000000000000000, -1.000000000000000000 ) ) ;
#15787 = EDGE_CURVE ( 'NONE', #39050, #16169, #60783, .T. ) ;
#15788 = ADVANCED_FACE ( 'NONE', ( #63735 ), #14162, .T. ) ;
#15789 = B_SPLINE_CURVE_WITH_KNOTS ( 'NONE', 3,
 ( #54310, #64894, #43764, #873, #11764, #69465, #26905, #32878, #33241, #16694, #22673, #53626, #521, #1220, #6134, #49388, #21284, #6499, #42733, #48331, #27594, #65235, #21624, #165, #43069, #38500, #21970, #59254, #17030, #27946, #5451, #10720, #59944, #54671, #53958, #64190, #16001, #64541, #37450, #32194, #16351, #37807, #43418 ),
 .UNSPECIFIED., .F., .F.,
 ( 4, 2, 2, 2, 2, 2, 2, 2, 1, 2, 2, 2, 2, 2, 2, 2, 2, 2, 2, 2, 2, 4 ),
 ( 0.000000000000000000, 0.001465684626643354044, 0.002198526939965028681, 0.002931369253286704186, 0.004397053879930075578, 0.005862738506573445668, 0.007328423133216816626, 0.008061265446538484758, 0.008794107759860152890, 0.009526950073181819287, 0.01025979238650348742, 0.01172547701314682368, 0.01319116163979015995, 0.01465684626643349621, 0.01538968857975516261, 0.01612253089307683074, 0.01758821551972016353, 0.01905390014636349980, 0.01978674245968516446, 0.02051958477300683259, 0.02198526939965016885, 0.02345095402629350165 ),
 .UNSPECIFIED. ) ;
#15790 = CARTESIAN_POINT ( 'NONE',  ( 136.9934874058118055, 43.35050367224291534, 70.68308355397081755 ) ) ;
#15791 = CYLINDRICAL_SURFACE ( 'NONE', #20159, 7.500000000000027534 ) ;
#15792 = CARTESIAN_POINT ( 'NONE',  ( -38.15923928782687824, 10.79140400702259228, -66.32252006240803155 ) ) ;
#15793 = EDGE_LOOP ( 'NONE', ( #51754, #1004, #68092, #37952, #54329, #20871, #8846, #23753, #53326 ) ) ;
#15794 = DIRECTION ( 'NONE',  ( 0.000000000000000000, 0.000000000000000000, -1.000000000000000000 ) ) ;
#15795 = ORIENTED_EDGE ( 'NONE', *, *, #63925, .T. ) ;
#15796 = ORIENTED_EDGE ( 'NONE', *, *, #12558, .T. ) ;
#15797 = EDGE_CURVE ( 'NONE', #21823, #47361, #20891, .T. ) ;
#15798 = CONICAL_SURFACE ( 'NONE', #48355, 65.00000000000000000, 0.7853981633974497223 ) ;
#15799 = CARTESIAN_POINT ( 'NONE',  ( -62.54987051470499182, 16.82069887634177974, 91.89306705351904725 ) ) ;
#15800 = DIRECTION ( 'NONE',  ( -1.000000000000000000, 0.000000000000000000, 0.000000000000000000 ) ) ;
#15801 = CARTESIAN_POINT ( 'NONE',  ( 6.000000000000000000, 0.000000000000000000, 5.000000000000000000 ) ) ;
#15802 = CARTESIAN_POINT ( 'NONE',  ( 69.71296738434152473, 14.32639855680324459, 87.60999871946472695 ) ) ;
#15803 = FACE_BOUND ( 'NONE', #45179, .T. ) ;
#15804 = CARTESIAN_POINT ( 'NONE',  ( 41.66904755831210849, 4.999999999999909406, 85.00100000000000477 ) ) ;
#15805 = CARTESIAN_POINT ( 'NONE',  ( 30.58844157136472575, 28.38418561969873721, 13.79046412417415191 ) ) ;
#15806 = ORIENTED_EDGE ( 'NONE', *, *, #48705, .T. ) ;
#15807 = CARTESIAN_POINT ( 'NONE',  ( -50.92620509423088038, 55.07344309828769724, 170.0000000000000000 ) ) ;
#15808 = EDGE_LOOP ( 'NONE', ( #11170, #41906 ) ) ;
#15809 = PRESENTATION_STYLE_ASSIGNMENT (( #15476 ) ) ;
#15810 = CARTESIAN_POINT ( 'NONE',  ( 187.5272808203427530, 85.37192123373903030, 32.93173814286044632 ) ) ;
#15811 = EDGE_CURVE ( 'NONE', #29891, #47734, #21843, .T. ) ;
#15812 = CARTESIAN_POINT ( 'NONE',  ( 61.10129719786245772, 12.23677173834305520, -62.80958882113672814 ) ) ;
#15813 = CARTESIAN_POINT ( 'NONE',  ( -71.17819443284076897, 19.60909329639482834, 11.56462333534533471 ) ) ;
#15814 = CARTESIAN_POINT ( 'NONE',  ( -38.29761368137835120, 10.81775503710270669, -93.35085947631458225 ) ) ;
#15815 = CARTESIAN_POINT ( 'NONE',  ( 19.75315861330098244, 7.667327050329334703, 31.14372870632146828 ) ) ;
#15816 = CARTESIAN_POINT ( 'NONE',  ( -149.5074843970971301, -170.0000000000000000, -49.81283053149198992 ) ) ;
#15817 = EDGE_CURVE ( 'NONE', #25239, #58815, #28160, .T. ) ;
#15818 = EDGE_CURVE ( 'NONE', #12220, #48080, #37326, .T. ) ;
#15819 = CARTESIAN_POINT ( 'NONE',  ( 164.4761273435911164, 64.62485394454748189, -73.19840926013584692 ) ) ;
#15820 = ORIENTED_EDGE ( 'NONE', *, *, #38902, .F. ) ;
#15821 = CARTESIAN_POINT ( 'NONE',  ( -75.01314391403413140, 20.96328762434826487, 58.19466124245714411 ) ) ;
#15822 = DIRECTION ( 'NONE',  ( 0.000000000000000000, 1.000000000000000000, -0.000000000000000000 ) ) ;
#15823 = ORIENTED_EDGE ( 'NONE', *, *, #23621, .F. ) ;
#15824 = ORIENTED_EDGE ( 'NONE', *, *, #44122, .T. ) ;
#15825 = CARTESIAN_POINT ( 'NONE',  ( -27.70115495247213744, 10.02455692117576369, -63.14125139223980909 ) ) ;
#15826 = DIRECTION ( 'NONE',  ( 0.000000000000000000, 0.000000000000000000, 1.000000000000000000 ) ) ;
#15827 = FACE_OUTER_BOUND ( 'NONE', #27928, .T. ) ;
#15828 = LINE ( 'NONE', #58723, #40646 ) ;
#15829 = CARTESIAN_POINT ( 'NONE',  ( -36.11269837220812207, -26.11269837220801193, 2.000000000000001776 ) ) ;
#15830 = EDGE_LOOP ( 'NONE', ( #44729, #21382, #46045, #41071 ) ) ;
#15831 = AXIS2_PLACEMENT_3D ( 'NONE', #19106, #13831, #18417 ) ;
#15832 = ORIENTED_EDGE ( 'NONE', *, *, #37546, .T. ) ;
#15833 = CARTESIAN_POINT ( 'NONE',  ( -132.9227230387960503, 52.53474289881227577, 40.74974517129221852 ) ) ;
#15834 = ORIENTED_EDGE ( 'NONE', *, *, #34487, .F. ) ;
#15835 = CARTESIAN_POINT ( 'NONE',  ( 206.7099580236348970, 109.1417833474364301, 17.09981171093966168 ) ) ;
#15836 = CARTESIAN_POINT ( 'NONE',  ( -143.8634661037141313, 60.82480701605702222, 33.25539283625584375 ) ) ;
#15837 = AXIS2_PLACEMENT_3D ( 'NONE', #19221, #50895, #46998 ) ;
#15838 = CARTESIAN_POINT ( 'NONE',  ( 55.51547041749725508, 11.05727559334826893, 63.91534904839117814 ) ) ;
#15839 = LINE ( 'NONE', #64363, #26189 ) ;
#15840 = VECTOR ( 'NONE', #44939, 1000.000000000000000 ) ;
#15841 = LINE ( 'NONE', #22159, #59706 ) ;
#15842 = EDGE_LOOP ( 'NONE', ( #39117, #14051, #28964, #9589 ) ) ;
#15843 = ORIENTED_EDGE ( 'NONE', *, *, #5071, .T. ) ;
#15844 = DIRECTION ( 'NONE',  ( 1.000000000000000000, 0.000000000000000000, 0.000000000000000000 ) ) ;
#15845 = DIRECTION ( 'NONE',  ( -0.000000000000000000, -0.000000000000000000, -1.000000000000000000 ) ) ;
#15846 = CARTESIAN_POINT ( 'NONE',  ( -167.1540252468942356, 80.72321878831101571, -19.91812675169417801 ) ) ;
#15847 = CARTESIAN_POINT ( 'NONE',  ( 139.2921620648437795, 44.80435067172499686, -75.55868156767934352 ) ) ;
#15848 = CARTESIAN_POINT ( 'NONE',  ( 63.50528314073025626, 12.78634332146812724, 44.81296093922130552 ) ) ;
#15849 = AXIS2_PLACEMENT_3D ( 'NONE', #21494, #11996, #10943 ) ;
#15850 = CARTESIAN_POINT ( 'NONE',  ( 21.57321902410670234, 7.762142431058419945, 86.38521836418507860 ) ) ;
#15851 = ORIENTED_EDGE ( 'NONE', *, *, #18261, .F. ) ;
#15852 = EDGE_CURVE ( 'NONE', #52541, #48379, #34375, .T. ) ;
#15853 = CARTESIAN_POINT ( 'NONE',  ( -95.61819996182570947, 29.52346081122274768, 68.31800957063339297 ) ) ;
#15854 = ORIENTED_EDGE ( 'NONE', *, *, #19129, .F. ) ;
#15855 = CARTESIAN_POINT ( 'NONE',  ( -76.32962633615589709, 21.44528079176260604, 30.78751738144537953 ) ) ;
#15856 = VERTEX_POINT ( 'NONE', #32752 ) ;
#15857 = EDGE_CURVE ( 'NONE', #42885, #31341, #64412, .T. ) ;
#15858 = ORIENTED_EDGE ( 'NONE', *, *, #5245, .T. ) ;
#15859 = CARTESIAN_POINT ( 'NONE',  ( -120.4666325602656087, 44.20829586446609483, 6.092936465464075191 ) ) ;
#15860 = CARTESIAN_POINT ( 'NONE',  ( -179.5082312244188643, 94.53075638132052916, 61.22619585784733687 ) ) ;
#15861 = CARTESIAN_POINT ( 'NONE',  ( 127.4953815656694758, 37.71366486045447175, 67.85928618946456936 ) ) ;
#15862 = ORIENTED_EDGE ( 'NONE', *, *, #27065, .F. ) ;
#15863 = ADVANCED_FACE ( 'NONE', ( #11282 ), #48908, .T. ) ;
#15864 = EDGE_CURVE ( 'NONE', #41137, #51945, #48213, .T. ) ;
#15865 = DIRECTION ( 'NONE',  ( -0.000000000000000000, -0.000000000000000000, -1.000000000000000000 ) ) ;
#15866 = PLANE ( 'NONE',  #44385 ) ;
#15867 = CARTESIAN_POINT ( 'NONE',  ( -52.73319225379940178, 53.34578647582053179, 43.58025477438756923 ) ) ;
#15868 = DIRECTION ( 'NONE',  ( 1.000000000000000000, 0.000000000000000000, -0.000000000000000000 ) ) ;
#15869 = DIRECTION ( 'NONE',  ( 1.000000000000000000, 0.000000000000000000, -0.000000000000000000 ) ) ;
#15870 = ADVANCED_FACE ( 'NONE', ( #54892 ), #6004, .F. ) ;
#15871 = CARTESIAN_POINT ( 'NONE',  ( -27.70005010046228477, 9.007417901453015574, 44.22257959986427522 ) ) ;
#15872 = CARTESIAN_POINT ( 'NONE',  ( -4.337405327940998312, -24.62086340933521456, 0.000000000000000000 ) ) ;
#15873 = VERTEX_POINT ( 'NONE', #42942 ) ;
#15874 = VECTOR ( 'NONE', #39729, 1000.000000000000000 ) ;
#15875 = FACE_BOUND ( 'NONE', #43616, .T. ) ;
#15876 = LINE ( 'NONE', #4974, #14074 ) ;
#15877 = CARTESIAN_POINT ( 'NONE',  ( 42.49453823366108196, 8.831814337191470798, 17.40632894816096865 ) ) ;
#15879 = CARTESIAN_POINT ( 'NONE',  ( -147.7895256390024485, 64.04409735547015714, -8.113308455688843068 ) ) ;
#15878 = CONICAL_SURFACE ( 'NONE', #43987, 8.000000000000001776, 1.047197551196595855 ) ;
#15880 = CARTESIAN_POINT ( 'NONE',  ( -119.9771613955296772, 43.90337778233485011, -47.02966473605362552 ) ) ;
#15881 = CARTESIAN_POINT ( 'NONE',  ( -80.54915509118110606, 24.12810583352862892, 3.809871470262444770 ) ) ;
#15882 = FACE_OUTER_BOUND ( 'NONE', #32888, .T. ) ;
#15883 = CARTESIAN_POINT ( 'NONE',  ( -154.7934364910360046, 68.79594655117533364, 16.70251692308080038 ) ) ;
#15884 = CARTESIAN_POINT ( 'NONE',  ( 198.5545530549422608, 99.90438832179273732, 94.71449343778881769 ) ) ;
#15886 = CARTESIAN_POINT ( 'NONE',  ( 69.08240197259638649, 14.16210831900842138, 6.051918337674103476 ) ) ;
#15885 = AXIS2_PLACEMENT_3D ( 'NONE', #59987, #23074, #11447 ) ;
#15887 = AXIS2_PLACEMENT_3D ( 'NONE', #16677, #23008, #38848 ) ;
#15888 = CARTESIAN_POINT ( 'NONE',  ( -17.90772993695114934, 72.84144224619130625, 133.5802547743875550 ) ) ;
#15889 = CARTESIAN_POINT ( 'NONE',  ( 92.53033045403536505, 22.59263332688195902, -21.13235829536132471 ) ) ;
#15890 = VERTEX_POINT ( 'NONE', #38028 ) ;
#15891 = CARTESIAN_POINT ( 'NONE',  ( -38.80621516088655198, 11.94263260276894023, 12.34045893885926226 ) ) ;
#15892 = ORIENTED_EDGE ( 'NONE', *, *, #16335, .T. ) ;
#15893 = CARTESIAN_POINT ( 'NONE',  ( 31.11269837220809364, 15.55634918610396866, 2.000000000000001776 ) ) ;
#15894 = ORIENTED_EDGE ( 'NONE', *, *, #52263, .T. ) ;
#15895 = B_SPLINE_CURVE_WITH_KNOTS ( 'NONE', 3,
 ( #37386, #5720, #63448, #15257, #47935, #20873, #41642, #32466, #14900, #10655, #4361, #26156, #63098, #9982, #53898, #41984, #69407, #27178, #42332, #58840, #36366, #52538, #68710, #21225, #26844, #4693, #43000, #63795, #20519, #32123, #26500, #37052, #15603, #59181, #42671, #9640, #58490, #57824, #5390, #31434, #64126, #53558, #10311, #52866, #47250, #47587, #48611, #31100, #25822, #36718, #48271, #11004, #69046, #58166 ),
 .UNSPECIFIED., .F., .F.,
 ( 4, 2, 2, 2, 2, 2, 2, 2, 2, 2, 2, 2, 2, 2, 2, 2, 2, 2, 2, 2, 2, 2, 2, 2, 2, 2, 4 ),
 ( 0.000000000000000000, 0.001981879248976703162, 0.002972818873465054527, 0.003963758497953406325, 0.004954698122441758557, 0.005945637746930109054, 0.006936577371418461285, 0.007927516995906812650, 0.009909396244883470276, 0.01189127549386012617, 0.01288221511834845671, 0.01387315474283678553, 0.01486409436732511434, 0.01585503399181344142, 0.01684597361630177023, 0.01783691324079009558, 0.01981879248976678443, 0.02080973211425513406, 0.02180067173874348369, 0.02279161136323183678, 0.02378255098772018641, 0.02477349061220853951, 0.02576443023669689261, 0.02774630948567364044, 0.02972818873465039174, 0.03071912835913878301, 0.03171006798362717427 ),
 .UNSPECIFIED. ) ;
#15896 = CARTESIAN_POINT ( 'NONE',  ( 20.74185656603722450, 7.717159106492279541, -75.51655753953751571 ) ) ;
#15897 = FACE_OUTER_BOUND ( 'NONE', #37275, .T. ) ;
#15898 = CARTESIAN_POINT ( 'NONE',  ( -145.5195986658808351, 62.16746116576784686, 58.70931206985594031 ) ) ;
#15899 = DIRECTION ( 'NONE',  ( 0.000000000000000000, 0.000000000000000000, 1.000000000000000000 ) ) ;
#15900 = AXIS2_PLACEMENT_3D ( 'NONE', #41262, #26461, #68341 ) ;
#15901 = EDGE_CURVE ( 'NONE', #6977, #38689, #707, .T. ) ;
#15902 = EDGE_CURVE ( 'NONE', #44118, #33190, #62005, .T. ) ;
#15903 = CARTESIAN_POINT ( 'NONE',  ( 133.8566784816069060, 42.60093787723652525, -36.02331093239566684 ) ) ;
#15904 = CARTESIAN_POINT ( 'NONE',  ( 209.2335797101723358, 114.5704254651986957, -91.52982707713782418 ) ) ;
#15905 = LINE ( 'NONE', #18859, #18458 ) ;
#15906 = EDGE_CURVE ( 'NONE', #33777, #54626, #35975, .T. ) ;
#15907 = CARTESIAN_POINT ( 'NONE',  ( -6.000000000000000000, 23.07878402833891229, 9.999999999999998224 ) ) ;
#15908 = VERTEX_POINT ( 'NONE', #46332 ) ;
#15909 = ORIENTED_EDGE ( 'NONE', *, *, #2302, .T. ) ;
#15910 = CARTESIAN_POINT ( 'NONE',  ( 69.50572373348796873, 14.27208627753790360, -39.42976292691626128 ) ) ;
#15911 = CARTESIAN_POINT ( 'NONE',  ( 173.5812904811884607, 72.71661333629877788, 90.47055245242088972 ) ) ;
#15912 = CARTESIAN_POINT ( 'NONE',  ( 133.8566784816069344, -170.0000000000000000, -62.86786152285933582 ) ) ;
#15913 = CARTESIAN_POINT ( 'NONE',  ( 66.17193415285930769, 14.46328737281204901, -90.10321091663050197 ) ) ;
#15914 = VERTEX_POINT ( 'NONE', #67466 ) ;
#15915 = CARTESIAN_POINT ( 'NONE',  ( 60.58000000000000540, -36.09918303830819752, 15.41169613715280562 ) ) ;
#15916 = CARTESIAN_POINT ( 'NONE',  ( 184.3966782763552033, 83.48172388049826509, -23.62389823460853222 ) ) ;
#15917 = CARTESIAN_POINT ( 'NONE',  ( 207.2640160519426900, 111.6867652229576322, 2.812936537257378244 ) ) ;
#15918 = SHAPE_REPRESENTATION_RELATIONSHIP ( 'NONE' , 'NONE' ,  #46431, #483 ) ;
#15919 = CARTESIAN_POINT ( 'NONE',  ( -173.9548930713591233, 88.06040582145364226, -49.67720558674120923 ) ) ;
#15920 = DIRECTION ( 'NONE',  ( 1.000000000000000000, 0.000000000000000000, 0.000000000000000000 ) ) ;
#15921 = CARTESIAN_POINT ( 'NONE',  ( 206.2980740120524672, 108.5619562183279783, -24.31977854252603422 ) ) ;
#15922 = FACE_OUTER_BOUND ( 'NONE', #61727, .T. ) ;
#15923 = CARTESIAN_POINT ( 'NONE',  ( 164.0073343966822677, 64.23003864582459244, 67.43977445298207840 ) ) ;
#15924 = EDGE_LOOP ( 'NONE', ( #27771, #58045 ) ) ;
#15925 = DIRECTION ( 'NONE',  ( 0.000000000000000000, 0.000000000000000000, -1.000000000000000000 ) ) ;
#15926 = CARTESIAN_POINT ( 'NONE',  ( 6.800000000000000711, 0.000000000000000000, 0.000000000000000000 ) ) ;
#15927 = AXIS2_PLACEMENT_3D ( 'NONE', #68696, #15246, #41972 ) ;
#15928 = CARTESIAN_POINT ( 'NONE',  ( 153.8224167330182865, 56.12711234192241250, 70.31123550504270270 ) ) ;
#15929 = DIRECTION ( 'NONE',  ( 0.000000000000000000, 0.000000000000000000, 1.000000000000000000 ) ) ;
#15930 = CARTESIAN_POINT ( 'NONE',  ( 151.1607415860635228, 52.90668588398087024, 5.978490512986149419 ) ) ;
#15931 = CARTESIAN_POINT ( 'NONE',  ( -4.667841011628368619, 7.713338668255913966, 84.49383781058769216 ) ) ;
#15932 = AXIS2_PLACEMENT_3D ( 'NONE', #16552, #54876, #1781 ) ;
#15933 = ORIENTED_EDGE ( 'NONE', *, *, #55086, .F. ) ;
#15934 = DIRECTION ( 'NONE',  ( -0.000000000000000000, 1.000000000000000000, -0.000000000000000000 ) ) ;
#15935 = CYLINDRICAL_SURFACE ( 'NONE', #4630, 7.500000000000013323 ) ;
#15936 = ORIENTED_EDGE ( 'NONE', *, *, #65270, .F. ) ;
#15937 = CIRCLE ( 'NONE', #12587, 242.4895526022646379 ) ;
#15938 = VECTOR ( 'NONE', #6661, 1000.000000000000000 ) ;
#15939 = EDGE_LOOP ( 'NONE', ( #1048, #19635, #15854, #49583 ) ) ;
#15940 = ADVANCED_FACE ( 'NONE', ( #67809 ), #22578, .T. ) ;
#15941 = CARTESIAN_POINT ( 'NONE',  ( 41.66904755831208007, -15.55634918610412853, 0.000000000000000000 ) ) ;
#15942 = FACE_OUTER_BOUND ( 'NONE', #5480, .T. ) ;
#15943 = CARTESIAN_POINT ( 'NONE',  ( 437.3372781065084496, 395.0000000000043201, 103.5502958579839259 ) ) ;
#15944 = ORIENTED_EDGE ( 'NONE', *, *, #57210, .F. ) ;
#15945 = AXIS2_PLACEMENT_3D ( 'NONE', #21071, #16124, #68228 ) ;
#15946 = CARTESIAN_POINT ( 'NONE',  ( -62.45356936877015386, 16.79156452995239945, -70.80215903815181377 ) ) ;
#15947 = CLOSED_SHELL ( 'NONE', ( #32652, #33942, #58809, #14998, #32048, #67428, #50501, #38188, #4847, #4322, #43169, #65687, #64587, #40447, #23137, #4868, #26968, #20171, #36132, #26544, #66069, #55190 ) ) ;
#15948 = CARTESIAN_POINT ( 'NONE',  ( 34.45500533947588906, 7.817363290423887001, -10.61686954642301117 ) ) ;
#15949 = CARTESIAN_POINT ( 'NONE',  ( 177.0110682437508558, 75.98481089748386808, -50.03885341334632386 ) ) ;
#15950 = CARTESIAN_POINT ( 'NONE',  ( -150.3831389294225573, 66.25266777263973950, -76.60930139824938578 ) ) ;
#15951 = LINE ( 'NONE', #31786, #46616 ) ;
#15952 = EDGE_CURVE ( 'NONE', #69210, #68800, #27088, .T. ) ;
#15953 = EDGE_LOOP ( 'NONE', ( #28406, #25946, #47626, #2459 ) ) ;
#15954 = DIRECTION ( 'NONE',  ( 0.6234898018587318180, 0.7818314824680311359, 0.000000000000000000 ) ) ;
#15955 = CARTESIAN_POINT ( 'NONE',  ( -173.1211646369891355, -170.0000000000000000, -69.05650775521368701 ) ) ;
#15956 = EDGE_CURVE ( 'NONE', #5435, #20075, #51966, .T. ) ;
#15957 = CARTESIAN_POINT ( 'NONE',  ( 9.280894575734581764, 7.385644305345140381, 33.75376781634191303 ) ) ;
#15958 = CARTESIAN_POINT ( 'NONE',  ( 197.2199163281728431, 98.22431253015352581, 36.04431904461028324 ) ) ;
#15959 = ADVANCED_FACE ( 'NONE', ( #24212 ), #53985, .T. ) ;
#15960 = CARTESIAN_POINT ( 'NONE',  ( -84.60434550335787662, 25.76113146461752379, 87.01482005019980193 ) ) ;
#15962 = EDGE_LOOP ( 'NONE', ( #1800, #30542 ) ) ;
#15961 = LINE ( 'NONE', #58861, #14133 ) ;
#15963 = ORIENTED_EDGE ( 'NONE', *, *, #45998, .F. ) ;
#15964 = ORIENTED_EDGE ( 'NONE', *, *, #53374, .F. ) ;
#15965 = CARTESIAN_POINT ( 'NONE',  ( 116.6681538161788865, 33.09439081574002017, -74.16764814704670528 ) ) ;
#15966 = DIRECTION ( 'NONE',  ( 0.6234898018587431423, -0.7818314824680221431, 0.000000000000000000 ) ) ;
#15967 = DIRECTION ( 'NONE',  ( 1.000000000000000000, 0.000000000000000000, -0.000000000000000000 ) ) ;
#15968 = DIRECTION ( 'NONE',  ( -1.000000000000000000, 0.000000000000000000, 0.000000000000000000 ) ) ;
#15969 = CARTESIAN_POINT ( 'NONE',  ( -13.45956523846225217, 8.333781915634244086, -21.03003943873567394 ) ) ;
#15970 = CARTESIAN_POINT ( 'NONE',  ( 150.0433793199862862, 52.09973307442955104, -71.54900094989498882 ) ) ;
#15971 = DIRECTION ( 'NONE',  ( -1.000000000000000000, 0.000000000000000000, 0.000000000000000000 ) ) ;
#15972 = FACE_OUTER_BOUND ( 'NONE', #15531, .T. ) ;
#15973 = ORIENTED_EDGE ( 'NONE', *, *, #4660, .F. ) ;
#15974 = ORIENTED_EDGE ( 'NONE', *, *, #42075, .T. ) ;
#15975 = CARTESIAN_POINT ( 'NONE',  ( 65.39792658623288446, 14.27332852928128304, -9.260399453094194655 ) ) ;
#15976 = VECTOR ( 'NONE', #33431, 1000.000000000000000 ) ;
#15977 = DIRECTION ( 'NONE',  ( 0.000000000000000000, -0.000000000000000000, 1.000000000000000000 ) ) ;
#15978 = CARTESIAN_POINT ( 'NONE',  ( -23.97453345597386587, 9.499725116317328855, 90.60705203038679656 ) ) ;
#15979 = CARTESIAN_POINT ( 'NONE',  ( -152.9143627383494959, 68.46626892668653852, 18.07331903687195052 ) ) ;
#15980 = DIRECTION ( 'NONE',  ( 0.4738686624730094610, -0.8805955318567321166, 0.000000000000000000 ) ) ;
#15981 = CARTESIAN_POINT ( 'NONE',  ( 19.74724861314306423, 6.659670522263898107, 31.13995450494594763 ) ) ;
#15982 = EDGE_CURVE ( 'NONE', #25475, #33134, #46686, .T. ) ;
#15983 = CARTESIAN_POINT ( 'NONE',  ( -156.9818039471237512, 72.15818689871304059, 91.26512449016922801 ) ) ;
#15984 = ORIENTED_EDGE ( 'NONE', *, *, #38284, .T. ) ;
#15985 = VERTEX_POINT ( 'NONE', #68162 ) ;
#15986 = EDGE_LOOP ( 'NONE', ( #61363, #31722, #68845, #43596 ) ) ;
#15987 = CARTESIAN_POINT ( 'NONE',  ( 6.400000000000000355, 4.618802153517001408, -8.000000000000000000 ) ) ;
#15988 = CARTESIAN_POINT ( 'NONE',  ( 34.83823433017389704, 8.871835168107976344, -49.09195262392610459 ) ) ;
#15989 = AXIS2_PLACEMENT_3D ( 'NONE', #41048, #42076, #14321 ) ;
#15990 = CARTESIAN_POINT ( 'NONE',  ( -33.84080342750783643, 9.997552308299095358, 57.43914399132651027 ) ) ;
#15991 = CARTESIAN_POINT ( 'NONE',  ( -151.2410113808308836, 65.66338888995508682, -22.77829783373973527 ) ) ;
#15992 = ORIENTED_EDGE ( 'NONE', *, *, #20705, .T. ) ;
#15993 = CARTESIAN_POINT ( 'NONE',  ( 188.4920037102894526, 87.93425473911921131, 64.86267653291690749 ) ) ;
#15994 = CARTESIAN_POINT ( 'NONE',  ( -150.3791492925491298, 64.92185203933371440, 57.60335617069471681 ) ) ;
#15995 = CARTESIAN_POINT ( 'NONE',  ( 22.90619343622340054, 7.840927939412480896, 8.256274177387846080 ) ) ;
#15996 = CARTESIAN_POINT ( 'NONE',  ( 105.8203563788590884, 26.88901185006199412, 16.32877285998160133 ) ) ;
#15997 = DIRECTION ( 'NONE',  ( -0.000000000000000000, 0.000000000000000000, -1.000000000000000000 ) ) ;
#15998 = CARTESIAN_POINT ( 'NONE',  ( -7.825402957745081878, 7.899365992529270741, -50.41807073194384259 ) ) ;
#15999 = CARTESIAN_POINT ( 'NONE',  ( 21.88606409348644277, 6.772455198693822176, 59.98579804294136864 ) ) ;
#16000 = CARTESIAN_POINT ( 'NONE',  ( 36.64089410029661309, -65.45232906116366678, 170.0000000000000000 ) ) ;
#16001 = CARTESIAN_POINT ( 'NONE',  ( 12.46704290855392472, 6.417105965824390523, -76.59253135474965291 ) ) ;
#16002 = VERTEX_POINT ( 'NONE', #14675 ) ;
#16003 = LINE ( 'NONE', #29513, #43932 ) ;
#16004 = SHAPE_DEFINITION_REPRESENTATION ( #22614, #5548 ) ;
#16005 = CARTESIAN_POINT ( 'NONE',  ( 177.0024338932394130, 74.57605685449962607, 43.11700017356537984 ) ) ;
#16006 = CARTESIAN_POINT ( 'NONE',  ( 26.11269837220800127, -26.11269837220812207, 2.000000000000001776 ) ) ;
#16007 = CARTESIAN_POINT ( 'NONE',  ( -107.0809603157386931, 36.42942792191067980, -36.73190862903344112 ) ) ;
#16008 = CARTESIAN_POINT ( 'NONE',  ( 62.05396267233468421, 13.48332220860125830, -77.51919629011504753 ) ) ;
#16009 = ORIENTED_EDGE ( 'NONE', *, *, #1745, .T. ) ;
#16010 = PRODUCT_DEFINITION ( 'UNKNOWN', '', #38892, #48581 ) ;
#16011 = ORIENTED_EDGE ( 'NONE', *, *, #65424, .F. ) ;
#16012 = EDGE_CURVE ( 'NONE', #13713, #29482, #63903, .T. ) ;
#16013 = CARTESIAN_POINT ( 'NONE',  ( -26.87327614295024603, 8.886070347947285342, -10.00229891119611025 ) ) ;
#16014 = ADVANCED_FACE ( 'NONE', ( #69170 ), #20998, .T. ) ;
#16015 = CARTESIAN_POINT ( 'NONE',  ( 197.1979149960397990, 98.19687999752002838, 9.527816039588145713 ) ) ;
#16016 = ORIENTED_EDGE ( 'NONE', *, *, #42397, .T. ) ;
#16017 = ORIENTED_EDGE ( 'NONE', *, *, #45734, .T. ) ;
#16018 = ADVANCED_FACE ( 'NONE', ( #26618 ), #5159, .F. ) ;
#16019 = CARTESIAN_POINT ( 'NONE',  ( 116.6734749296699221, 31.97209464358269315, 67.84770262631175797 ) ) ;
#16020 = ORIENTED_EDGE ( 'NONE', *, *, #33633, .F. ) ;
#16021 = DIRECTION ( 'NONE',  ( 0.000000000000000000, -1.000000000000000000, 0.000000000000000000 ) ) ;
#16022 = CARTESIAN_POINT ( 'NONE',  ( 128.9253503890652439, 38.52561778336671949, 31.35415491786180908 ) ) ;
#16023 = CARTESIAN_POINT ( 'NONE',  ( 141.3036441389950255, 47.31002705502925920, 62.81493121066256435 ) ) ;
#16024 = DIRECTION ( 'NONE',  ( 0.000000000000000000, 0.000000000000000000, 1.000000000000000000 ) ) ;
#16025 = AXIS2_PLACEMENT_3D ( 'NONE', #15346, #59272, #37831 ) ;
#16026 = CARTESIAN_POINT ( 'NONE',  ( 82.47965707583895778, 18.04644375528062739, -90.75020385575585635 ) ) ;
#16027 = CARTESIAN_POINT ( 'NONE',  ( 31.11269837220812562, 31.11269837220800483, 0.000000000000000000 ) ) ;
#16028 =( GEOMETRIC_REPRESENTATION_CONTEXT ( 3 ) GLOBAL_UNCERTAINTY_ASSIGNED_CONTEXT ( ( #12815 ) ) GLOBAL_UNIT_ASSIGNED_CONTEXT ( ( #48462, #43201, #37241 ) ) REPRESENTATION_CONTEXT ( 'NONE', 'WORKASPACE' ) );
#16029 = CARTESIAN_POINT ( 'NONE',  ( -46.06722295615789875, 46.37372919877053334, 3.125053320693552861E-16 ) ) ;
#16030 = ORIENTED_EDGE ( 'NONE', *, *, #53600, .T. ) ;
#16031 = AXIS2_PLACEMENT_3D ( 'NONE', #6217, #49820, #44190 ) ;
#16032 = VERTEX_POINT ( 'NONE', #5501 ) ;
#16033 = CARTESIAN_POINT ( 'NONE',  ( -118.6288898061518466, 41.89286798341289142, -17.45136109783878808 ) ) ;
#16034 = VECTOR ( 'NONE', #26129, 1000.000000000000227 ) ;
#16035 = FACE_BOUND ( 'NONE', #33527, .T. ) ;
#16036 = ADVANCED_FACE ( 'NONE', ( #16055 ), #42779, .F. ) ;
#16037 = DIRECTION ( 'NONE',  ( -0.000000000000000000, -1.000000000000000000, -0.000000000000000000 ) ) ;
#16038 = EDGE_CURVE ( 'NONE', #65685, #27181, #66144, .T. ) ;
#16039 = CARTESIAN_POINT ( 'NONE',  ( -166.2065256787326462, 81.19093426984588291, -66.13749893354456333 ) ) ;
#16041 = ORIENTED_EDGE ( 'NONE', *, *, #37908, .T. ) ;
#16040 = CARTESIAN_POINT ( 'NONE',  ( -143.3925773749112693, 59.16144459815141943, -37.96278985645250259 ) ) ;
#16042 = CARTESIAN_POINT ( 'NONE',  ( 55.91133443650745960, 12.16263767238152660, 8.014282917357382630 ) ) ;
#16043 = CIRCLE ( 'NONE', #57638, 10.00000000000000178 ) ;
#16044 = ORIENTED_EDGE ( 'NONE', *, *, #22064, .F. ) ;
#16045 = CARTESIAN_POINT ( 'NONE',  ( -125.8938041572051105, 46.49392987655495091, 45.61994787315711619 ) ) ;
#16046 = DIRECTION ( 'NONE',  ( -1.000000000000000000, 0.000000000000000000, 0.000000000000000000 ) ) ;
#16047 = CARTESIAN_POINT ( 'NONE',  ( 84.73231936899559003, 18.78199960571078364, -23.74888722610129577 ) ) ;
#16048 = CARTESIAN_POINT ( 'NONE',  ( 133.8566784816069344, 42.60093787723652525, 29.51034083899533300 ) ) ;
#16049 = B_SPLINE_CURVE_WITH_KNOTS ( 'NONE', 3,
 ( #63655, #58356, #63985, #26363, #69262, #15799, #30955, #37243, #10172, #52402, #9151, #58693, #41849, #3872, #9842, #31632, #68908, #25688, #47116, #20734, #31981, #36228, #3519, #62621, #14431, #63309, #42189, #30606, #53067, #46777, #68247, #41505, #62957, #5914, #26703, #1356, #44254, #32669, #27034, #53410, #59727, #64327, #16487, #48463, #16139, #21414, #22110, #43552, #38641, #65028, #11200 ),
 .UNSPECIFIED., .F., .F.,
 ( 4, 2, 2, 2, 2, 2, 2, 2, 2, 2, 2, 2, 2, 2, 2, 2, 1, 2, 2, 2, 2, 2, 2, 2, 2, 4 ),
 ( 0.000000000000000000, 0.001945536185327564373, 0.002918304277991350896, 0.003891072370655136985, 0.005836608555982708731, 0.006809376648646493953, 0.007782144741310279175, 0.009727680926637829670, 0.01167321711196537756, 0.01264598520462914023, 0.01361875329729290290, 0.01459152138995666557, 0.01556428948262042825, 0.01750982566794795359, 0.01945536185327547893, 0.02042812994593924333, 0.02140089803860300774, 0.02237366613126677561, 0.02334643422393054002, 0.02529197040925803067, 0.02626473850192179507, 0.02723750659458555254, 0.02821027468724931347, 0.02918304277991307441, 0.03015581087257683882, 0.03112857896524059975 ),
 .UNSPECIFIED. ) ;
#16050 = FACE_OUTER_BOUND ( 'NONE', #34830, .T. ) ;
#16051 = DIRECTION ( 'NONE',  ( 0.000000000000000000, -0.000000000000000000, -1.000000000000000000 ) ) ;
#16052 = CARTESIAN_POINT ( 'NONE',  ( -97.47339919287387033, 30.40512551257288010, -63.58105464508946625 ) ) ;
#16053 = ORIENTED_EDGE ( 'NONE', *, *, #22290, .F. ) ;
#16054 = ORIENTED_EDGE ( 'NONE', *, *, #30902, .F. ) ;
#16055 = FACE_OUTER_BOUND ( 'NONE', #43661, .T. ) ;
#16056 = DIRECTION ( 'NONE',  ( -0.2660368455666687892, -0.9639628606958550172, 2.500042656554809847E-16 ) ) ;
#16057 = CARTESIAN_POINT ( 'NONE',  ( -165.7699288023689803, 79.30174988963855753, -43.72753680632582274 ) ) ;
#16058 = DIRECTION ( 'NONE',  ( 1.000000000000000000, 0.000000000000000000, 0.000000000000000000 ) ) ;
#16059 = CARTESIAN_POINT ( 'NONE',  ( 102.7414208686707582, 26.65627265923298594, -69.77758797498718479 ) ) ;
#16060 = CARTESIAN_POINT ( 'NONE',  ( -73.81801970646053235, 21.60231032711190480, 43.64555415764338164 ) ) ;
#16061 = CARTESIAN_POINT ( 'NONE',  ( -78.66644367742111399, 23.39876645725286153, -61.96000122218157458 ) ) ;
#16062 = LINE ( 'NONE', #58619, #49377 ) ;
#16063 = CARTESIAN_POINT ( 'NONE',  ( 41.33434189587760699, 9.684413566891871383, -35.86888733174379951 ) ) ;
#16064 = LINE ( 'NONE', #64605, #13841 ) ;
#16065 = VERTEX_POINT ( 'NONE', #10092 ) ;
#16066 = LINE ( 'NONE', #47722, #55764 ) ;
#16067 = ORIENTED_EDGE ( 'NONE', *, *, #54602, .T. ) ;
#16068 = CARTESIAN_POINT ( 'NONE',  ( -36.37371824399144060, 10.45334302951138028, 5.202302465703740886 ) ) ;
#16069 = CIRCLE ( 'NONE', #13973, 65.36598343705435354 ) ;
#16070 = CARTESIAN_POINT ( 'NONE',  ( 94.11595392909970315, 23.18887043179184460, 64.57093135896856495 ) ) ;
#16071 = CARTESIAN_POINT ( 'NONE',  ( 150.0889146124742695, 52.13243511955543141, -18.13589629245545964 ) ) ;
#16072 = CARTESIAN_POINT ( 'NONE',  ( 86.62931800182293784, -170.0000000000000000, 71.55663816294304524 ) ) ;
#16073 = CARTESIAN_POINT ( 'NONE',  ( 32.90953848114695290, 7.653665824624196645, -73.72727812858101970 ) ) ;
#16074 = DIRECTION ( 'NONE',  ( -0.000000000000000000, 1.000000000000000000, -0.000000000000000000 ) ) ;
#16075 = VECTOR ( 'NONE', #43651, 1000.000000000000000 ) ;
#16076 = CARTESIAN_POINT ( 'NONE',  ( 114.3151031867488712, 31.93066835014830929, -90.80084266641746638 ) ) ;
#16077 = ORIENTED_EDGE ( 'NONE', *, *, #50211, .F. ) ;
#16078 = FACE_OUTER_BOUND ( 'NONE', #65140, .T. ) ;
#16079 = CARTESIAN_POINT ( 'NONE',  ( 39.40195752203892710, -170.0000000000000000, 18.06928371549960133 ) ) ;
#16080 = ORIENTED_EDGE ( 'NONE', *, *, #39226, .F. ) ;
#16081 = CARTESIAN_POINT ( 'NONE',  ( 266.9165763529819628, -52.00000000000000711, 128.9999999999999716 ) ) ;
#16082 = CARTESIAN_POINT ( 'NONE',  ( -30.46060138092288128, 9.432375387772218289, 18.32403480767325377 ) ) ;
#16083 = AXIS2_PLACEMENT_3D ( 'NONE', #1692, #32316, #1341 ) ;
#16084 = DIRECTION ( 'NONE',  ( -0.000000000000000000, 1.000000000000000000, -0.000000000000000000 ) ) ;
#16085 = CARTESIAN_POINT ( 'NONE',  ( 280.0000000000000000, -21.42428528562853884, 4.999999999999990230 ) ) ;
#16086 = CARTESIAN_POINT ( 'NONE',  ( -99.31850058233798961, 31.30166762705809091, -8.775526202821598787 ) ) ;
#16087 = CARTESIAN_POINT ( 'NONE',  ( 81.09429416756655939, 18.66109123847838447, 85.82913394444857147 ) ) ;
#16088 = VECTOR ( 'NONE', #58732, 1000.000000000000000 ) ;
#16089 = ORIENTED_EDGE ( 'NONE', *, *, #47379, .T. ) ;
#16091 = CIRCLE ( 'NONE', #34092, 242.4895526022646379 ) ;
#16090 = CARTESIAN_POINT ( 'NONE',  ( 848.0071894358308100, 615.7169673593987227, 569.0068267248676648 ) ) ;
#16092 = CARTESIAN_POINT ( 'NONE',  ( -9.964117946888961797, -64.24592483216726180, 43.58025477438756923 ) ) ;
#16093 = CARTESIAN_POINT ( 'NONE',  ( -132.9409505933031710, 51.31241517713429801, 8.655732063095380013 ) ) ;
#16094 = CARTESIAN_POINT ( 'NONE',  ( -109.5157885508427142, 37.76058765671432838, 66.90473407092159164 ) ) ;
#16095 = EDGE_CURVE ( 'NONE', #51430, #38471, #11314, .T. ) ;
#16096 = CONTEXT_DEPENDENT_SHAPE_REPRESENTATION ( #28275, #2446 ) ;
#16097 = CARTESIAN_POINT ( 'NONE',  ( -180.5185845152422814, 95.75861486247472953, 93.30168827895523975 ) ) ;
#16098 = ORIENTED_EDGE ( 'NONE', *, *, #13517, .T. ) ;
#16099 = DIRECTION ( 'NONE',  ( 0.000000000000000000, 1.000000000000000000, 0.000000000000000000 ) ) ;
#16100 = CARTESIAN_POINT ( 'NONE',  ( 88.53517449242355042, 20.08005703101044759, 71.31441284595423724 ) ) ;
#16101 = CARTESIAN_POINT ( 'NONE',  ( 197.8598785550297521, 99.02620879292949496, -20.07738393529249166 ) ) ;
#16102 = EDGE_CURVE ( 'NONE', #33041, #68729, #40082, .T. ) ;
#16103 = CARTESIAN_POINT ( 'NONE',  ( 87.42971020158420004, 19.69418112884302374, -89.51066537983909654 ) ) ;
#16104 = ADVANCED_FACE ( 'NONE', ( #33985 ), #54367, .T. ) ;
#16105 = CARTESIAN_POINT ( 'NONE',  ( 138.1919700334460686, 44.10401742531042402, 30.87242645337029145 ) ) ;
#16106 = ORIENTED_EDGE ( 'NONE', *, *, #2101, .F. ) ;
#16107 = LINE ( 'NONE', #58321, #12047 ) ;
#16108 = CARTESIAN_POINT ( 'NONE',  ( 79.12879321038295188, 18.04902206524924679, 10.60344279547883062 ) ) ;
#16109 = DIRECTION ( 'NONE',  ( 0.000000000000000000, 1.000000000000000000, 0.000000000000000000 ) ) ;
#16110 = EDGE_CURVE ( 'NONE', #25506, #25227, #28710, .T. ) ;
#16111 = LINE ( 'NONE', #25992, #66781 ) ;
#16112 = EDGE_LOOP ( 'NONE', ( #27726, #56434 ) ) ;
#16113 = DIRECTION ( 'NONE',  ( 0.000000000000000000, 0.000000000000000000, 1.000000000000000000 ) ) ;
#16114 = EDGE_LOOP ( 'NONE', ( #38458, #65320, #44956, #19694 ) ) ;
#16115 = CARTESIAN_POINT ( 'NONE',  ( -75.01314391403414561, 20.96328762434827198, -22.33899052893390191 ) ) ;
#16116 = DIRECTION ( 'NONE',  ( -1.000000000000000000, -1.850474763383843014E-16, 1.697708136181793677E-16 ) ) ;
#16117 = VECTOR ( 'NONE', #30728, 1000.000000000000000 ) ;
#16118 = EDGE_CURVE ( 'NONE', #6225, #52460, #57437, .T. ) ;
#16119 = DIRECTION ( 'NONE',  ( -0.6579387259397027066, -0.7530714660036195163, 0.000000000000000000 ) ) ;
#16120 = VECTOR ( 'NONE', #33391, 1000.000000000000000 ) ;
#16122 = VERTEX_POINT ( 'NONE', #61057 ) ;
#16121 = DIRECTION ( 'NONE',  ( 0.000000000000000000, 1.000000000000000000, 0.000000000000000000 ) ) ;
#16123 = CARTESIAN_POINT ( 'NONE',  ( -180.0179082103088035, 95.14811732286295864, 41.28284462864509408 ) ) ;
#16124 = DIRECTION ( 'NONE',  ( 0.000000000000000000, 0.6427876096865404731, 0.7660444431189771253 ) ) ;
#16125 = PLANE ( 'NONE',  #12581 ) ;
#16126 = ORIENTED_EDGE ( 'NONE', *, *, #4360, .F. ) ;
#16127 = B_SPLINE_CURVE_WITH_KNOTS ( 'NONE', 3,
 ( #51523, #8956, #24790, #46228, #57486, #20191, #30404, #2992, #9293, #3668, #50820, #36374, #25142, #30756, #46574, #52204, #4020, #41649, #25488, #24101, #63105, #2638, #46928, #14906, #7917, #40269, #45540, #24451, #67022, #56438, #45892, #8262, #29715, #24017, #45461, #18736, #7839, #61644, #60948, #65540, #12768, #56027, #66255 ),
 .UNSPECIFIED., .F., .F.,
 ( 4, 2, 2, 2, 2, 2, 2, 2, 2, 2, 2, 2, 1, 2, 2, 2, 2, 2, 2, 2, 2, 4 ),
 ( 0.02379577142314829794, 0.02527778373276531876, 0.02601878988757382050, 0.02675979604238232223, 0.02824180835199933612, 0.02972382066161635000, 0.03046482681642484480, 0.03120583297123334654, 0.03268784528085035002, 0.03416985759046735349, 0.03565186990008435697, 0.03639287605489284483, 0.03713388220970133963, 0.03787488836450983443, 0.03861589451931832229, 0.04009790682893532576, 0.04157991913855232230, 0.04306193144816931884, 0.04380293760297782057, 0.04454394375778632231, 0.04602595606740331191, 0.04750796837702030845 ),
 .UNSPECIFIED. ) ;
#16128 = DIRECTION ( 'NONE',  ( -0.000000000000000000, -0.000000000000000000, 1.000000000000000000 ) ) ;
#16129 = CIRCLE ( 'NONE', #37463, 185.0000000000000000 ) ;
#16130 = CARTESIAN_POINT ( 'NONE',  ( 138.5721691894143248, 44.34516164557649631, 58.00226450593800109 ) ) ;
#16131 = CARTESIAN_POINT ( 'NONE',  ( -179.2128128997735246, 95.75254520622989673, 33.91814095447512756 ) ) ;
#16132 = CARTESIAN_POINT ( 'NONE',  ( 126.4757069339777473, 38.29528077539268338, 62.49800859209678094 ) ) ;
#16133 = B_SPLINE_CURVE_WITH_KNOTS ( 'NONE', 3,
 ( #39172, #21578, #12431, #61989, #1890, #24379, #56035, #57074 ),
 .UNSPECIFIED., .F., .F.,
 ( 4, 2, 2, 4 ),
 ( 0.004673709593152172194, 0.005837709341827659014, 0.007001709090503144967, 0.009329708587854116872 ),
 .UNSPECIFIED. ) ;
#16134 = ORIENTED_EDGE ( 'NONE', *, *, #3096, .F. ) ;
#16135 = ORIENTED_EDGE ( 'NONE', *, *, #47340, .T. ) ;
#16136 = ORIENTED_EDGE ( 'NONE', *, *, #59389, .T. ) ;
#16137 = VECTOR ( 'NONE', #23962, 1000.000000000000000 ) ;
#16138 = FILL_AREA_STYLE ('',( #37940 ) ) ;
#16139 = CARTESIAN_POINT ( 'NONE',  ( -47.61659327988082424, 12.81296103674151965, 92.53618404811727771 ) ) ;
#16140 = PLANE ( 'NONE',  #30203 ) ;
#16141 = CARTESIAN_POINT ( 'NONE',  ( 112.3013380801408658, 388.0000000000065938, -123.9497041420121235 ) ) ;
#16142 = CARTESIAN_POINT ( 'NONE',  ( 70.43248927385285185, 14.51614591398291410, 89.83896190036961116 ) ) ;
#16143 = CARTESIAN_POINT ( 'NONE',  ( 111.9975424824653487, 172.0000000000000284, 256.6193948016162381 ) ) ;
#16144 = CARTESIAN_POINT ( 'NONE',  ( -18.89790202299119315, -62.20684691518632548, 41.38025477438755928 ) ) ;
#16145 = DIRECTION ( 'NONE',  ( 0.000000000000000000, 0.000000000000000000, -1.000000000000000000 ) ) ;
#16146 = VERTEX_POINT ( 'NONE', #12884 ) ;
#16147 = CARTESIAN_POINT ( 'NONE',  ( -96.32309170788076358, 30.97039782218995541, -91.64132999366567844 ) ) ;
#16148 = VERTEX_POINT ( 'NONE', #17083 ) ;
#16149 = CARTESIAN_POINT ( 'NONE',  ( -71.23176719684946079, 20.69188312694500809, 65.78254442754143838 ) ) ;
#16150 =( REPRESENTATION_RELATIONSHIP ('NONE','NONE', #40274, #64096 ) REPRESENTATION_RELATIONSHIP_WITH_TRANSFORMATION ( #50545 )SHAPE_REPRESENTATION_RELATIONSHIP( ) );
#16151 = CARTESIAN_POINT ( 'NONE',  ( 188.5645326065590837, 86.51153908883289034, 36.18923501154701938 ) ) ;
#16152 = CARTESIAN_POINT ( 'NONE',  ( -15.55634918610396866, 36.11269837220808654, 2.000000000000001776 ) ) ;
#16153 = DIRECTION ( 'NONE',  ( -1.000000000000000000, -0.000000000000000000, -0.000000000000000000 ) ) ;
#16154 = CARTESIAN_POINT ( 'NONE',  ( 0.000000000000000000, 0.000000000000000000, 111.5502958579881749 ) ) ;
#16155 = CARTESIAN_POINT ( 'NONE',  ( 21.44191228441540531, 7.755009954762291713, 32.56178140903555374 ) ) ;
#16156 = DIRECTION ( 'NONE',  ( 1.000000000000000000, 0.000000000000000000, 0.000000000000000000 ) ) ;
#16157 = CARTESIAN_POINT ( 'NONE',  ( 164.1338586910085837, 64.33646242148857652, -67.01638482620461446 ) ) ;
#16158 = EDGE_LOOP ( 'NONE', ( #47934, #54871, #19275, #17353 ) ) ;
#16159 = EDGE_CURVE ( 'NONE', #15124, #16476, #38552, .T. ) ;
#16160 = FACE_OUTER_BOUND ( 'NONE', #18619, .T. ) ;
#16161 = CARTESIAN_POINT ( 'NONE',  ( -2.967675213622137598, -38.21895566658998433, 13.32819397642332149 ) ) ;
#16162 = VERTEX_POINT ( 'NONE', #62093 ) ;
#16163 = VERTEX_POINT ( 'NONE', #8295 ) ;
#16164 = CARTESIAN_POINT ( 'NONE',  ( -24.18158274621863768, 9.527343002918318149, -71.61677556244950438 ) ) ;
#16165 = CARTESIAN_POINT ( 'NONE',  ( 62.52742438962777527, 12.55954017561948532, -35.72069083216972984 ) ) ;
#16166 = CARTESIAN_POINT ( 'NONE',  ( -24.98026281234599821, -0.9932118737290694943, 0.000000000000000000 ) ) ;
#16167 = AXIS2_PLACEMENT_3D ( 'NONE', #27532, #44053, #55664 ) ;
#16168 = CARTESIAN_POINT ( 'NONE',  ( -143.2471548081022945, 59.04577938365767409, 7.214454213839029073 ) ) ;
#16169 = VERTEX_POINT ( 'NONE', #18846 ) ;
#16170 = VECTOR ( 'NONE', #23098, 1000.000000000000000 ) ;
#16171 = EDGE_LOOP ( 'NONE', ( #24794, #28283, #42185, #33426 ) ) ;
#16172 = CARTESIAN_POINT ( 'NONE',  ( -133.0921934900199801, 52.65587531157186874, 40.24238173231051263 ) ) ;
#16173 = ORIENTED_EDGE ( 'NONE', *, *, #7557, .T. ) ;
#16174 = CARTESIAN_POINT ( 'NONE',  ( -5.066666666666664653, 8.000000000000000000, 43.13333333333333286 ) ) ;
#16175 = CARTESIAN_POINT ( 'NONE',  ( -190.6985136298601731, 109.1272424661242582, 94.99999999999866418 ) ) ;
#16176 = VECTOR ( 'NONE', #20764, 1000.000000000000000 ) ;
#16177 = CARTESIAN_POINT ( 'NONE',  ( 56.66438910147189034, 11.28870326331392704, 60.16100584247962502 ) ) ;
#16178 = CARTESIAN_POINT ( 'NONE',  ( -5.888165822225389867, 7.780336669456523246, 71.70979528173234030 ) ) ;
#16179 = DIRECTION ( 'NONE',  ( -1.000000000000000000, 0.000000000000000000, 0.000000000000000000 ) ) ;
#16180 = AXIS2_PLACEMENT_3D ( 'NONE', #351, #21808, #60841 ) ;
#16181 = EDGE_CURVE ( 'NONE', #58719, #59923, #3697, .T. ) ;
#16182 = DIRECTION ( 'NONE',  ( 1.387778780781445922E-16, -1.000000000000000000, -1.232595164407830946E-32 ) ) ;
#16183 = VECTOR ( 'NONE', #30927, 1000.000000000000000 ) ;
#16184 = CARTESIAN_POINT ( 'NONE',  ( 26.69682282325711142, 59.27986298182224800, 41.38025477438755928 ) ) ;
#16185 = VERTEX_POINT ( 'NONE', #29742 ) ;
#16186 = ORIENTED_EDGE ( 'NONE', *, *, #57575, .F. ) ;
#16187 = CARTESIAN_POINT ( 'NONE',  ( 7.762887554996211747E-14, 46.66904755831208718, 0.000000000000000000 ) ) ;
#16188 = DIRECTION ( 'NONE',  ( -0.000000000000000000, 1.000000000000000000, -0.000000000000000000 ) ) ;
#16189 = AXIS2_PLACEMENT_3D ( 'NONE', #66087, #61139, #17519 ) ;
#16190 = CARTESIAN_POINT ( 'NONE',  ( -171.0758681675584114, 84.87997360100516175, -8.139245166615548754 ) ) ;
#16191 = LINE ( 'NONE', #715, #56817 ) ;
#16192 = EDGE_CURVE ( 'NONE', #30657, #55128, #34690, .T. ) ;
#16193 = CARTESIAN_POINT ( 'NONE',  ( 69.49862690228272299, 14.27023134440513275, 33.50967676719564281 ) ) ;
#16194 = CARTESIAN_POINT ( 'NONE',  ( 20.87644034061239751, 7.724420236077849999, 85.68391863677295817 ) ) ;
#16195 = ORIENTED_EDGE ( 'NONE', *, *, #56861, .F. ) ;
#16196 = CARTESIAN_POINT ( 'NONE',  ( 86.62931800182293784, 19.42108912189598158, 2.867536982015618019 ) ) ;
#16197 = EDGE_LOOP ( 'NONE', ( #4382, #31363, #62284, #2266 ) ) ;
#16198 = LINE ( 'NONE', #59103, #26127 ) ;
#16199 = VERTEX_POINT ( 'NONE', #19533 ) ;
#16200 = EDGE_CURVE ( 'NONE', #2906, #54626, #51885, .T. ) ;
#16201 = ORIENTED_EDGE ( 'NONE', *, *, #18981, .F. ) ;
#16202 = CARTESIAN_POINT ( 'NONE',  ( -119.1605144823340083, 43.39823405392969846, 7.961637200802151426 ) ) ;
#16203 = ADVANCED_FACE ( 'NONE', ( #67052 ), #51207, .F. ) ;
#16205 = EDGE_CURVE ( 'NONE', #52493, #46420, #2341, .T. ) ;
#16204 = CARTESIAN_POINT ( 'NONE',  ( 5.799999999999999822, -6.928203230275504332, 4.000000000000010658 ) ) ;
#16206 = CARTESIAN_POINT ( 'NONE',  ( 17.74393407086869701, 6.570779001277777809, 17.92757028238993655 ) ) ;
#16207 = ORIENTED_EDGE ( 'NONE', *, *, #6105, .T. ) ;
#16208 = DIRECTION ( 'NONE',  ( -1.000000000000000000, 0.000000000000000000, 0.000000000000000000 ) ) ;
#16209 = CARTESIAN_POINT ( 'NONE',  ( 150.0973882686024865, 52.13852366454150911, 38.31082999385310472 ) ) ;
#16210 = VECTOR ( 'NONE', #54709, 1000.000000000000000 ) ;
#16211 = CARTESIAN_POINT ( 'NONE',  ( -62.97854483871577713, 16.08424353203677271, 170.0000000000000000 ) ) ;
#16212 = DIRECTION ( 'NONE',  ( -1.000000000000000000, 0.000000000000000000, 0.000000000000000000 ) ) ;
#16213 = CARTESIAN_POINT ( 'NONE',  ( -46.66904755831212981, -15.55634918610397222, 0.000000000000000000 ) ) ;
#16214 = LINE ( 'NONE', #21485, #34986 ) ;
#16215 = CARTESIAN_POINT ( 'NONE',  ( -25.48237668717799664, 8.689083390666784368, 42.29997830577138984 ) ) ;
#16216 = CARTESIAN_POINT ( 'NONE',  ( -144.3939084932120807, 61.25241660819414591, -63.66557192140397348 ) ) ;
#16217 = ORIENTED_EDGE ( 'NONE', *, *, #13823, .F. ) ;
#16218 = FACE_BOUND ( 'NONE', #14885, .T. ) ;
#16219 = CARTESIAN_POINT ( 'NONE',  ( 64.16679220703380793, -10.37413986118096254, 40.00000000000003553 ) ) ;
#16220 = CARTESIAN_POINT ( 'NONE',  ( -177.5100621450479252, 93.70693725195827994, 59.06660155457885253 ) ) ;
#16221 = DIRECTION ( 'NONE',  ( 0.000000000000000000, 0.000000000000000000, 1.000000000000000000 ) ) ;
#16222 = CARTESIAN_POINT ( 'NONE',  ( -122.1940143064357187, 45.29738883755587153, -35.88556451797717983 ) ) ;
#16223 = CARTESIAN_POINT ( 'NONE',  ( -86.06525741550315445, 26.37048289224654951, 12.32731785139721303 ) ) ;
#16224 = DIRECTION ( 'NONE',  ( 0.000000000000000000, 0.000000000000000000, -1.000000000000000000 ) ) ;
#16225 = VECTOR ( 'NONE', #55096, 1000.000000000000000 ) ;
#16226 = CARTESIAN_POINT ( 'NONE',  ( -153.6931187576189473, 67.81270084382359187, 5.148524762051829740 ) ) ;
#16227 = DIRECTION ( 'NONE',  ( -1.000000000000000000, 0.000000000000000000, 0.000000000000000000 ) ) ;
#16228 = AXIS2_PLACEMENT_3D ( 'NONE', #6654, #38666, #23885 ) ;
#16229 = CARTESIAN_POINT ( 'NONE',  ( 125.2194818923508848, 188.0000000000000000, 7.478223336038896996 ) ) ;
#16230 = CARTESIAN_POINT ( 'NONE',  ( 164.0158927577712973, 62.92463143894072886, 6.365232034859697130 ) ) ;
#16231 = CARTESIAN_POINT ( 'NONE',  ( 88.98820631332499431, 21.30618275724810218, -23.61262677780854702 ) ) ;
#16232 = ORIENTED_EDGE ( 'NONE', *, *, #3985, .T. ) ;
#16234 = VECTOR ( 'NONE', #15347, 1000.000000000000000 ) ;
#16233 = CARTESIAN_POINT ( 'NONE',  ( -38.45778834351241926, 11.87434869453507247, 13.52690563419841752 ) ) ;
#16235 = VERTEX_POINT ( 'NONE', #37090 ) ;
#16236 = FACE_OUTER_BOUND ( 'NONE', #35562, .T. ) ;
#16237 = ORIENTED_EDGE ( 'NONE', *, *, #39393, .F. ) ;
#16238 = CARTESIAN_POINT ( 'NONE',  ( 19.75315861330098599, 7.667327050329335592, -76.23447365553329291 ) ) ;
#16239 = CARTESIAN_POINT ( 'NONE',  ( 117.7235023277067967, 33.62688311768400951, 91.44526349519324526 ) ) ;
#16240 = CARTESIAN_POINT ( 'NONE',  ( 429.8372781065085633, 400.0000000000109708, 96.05029585798436642 ) ) ;
#16241 = DIRECTION ( 'NONE',  ( -0.9909497617679332571, -0.1342332658176667581, 5.102127870520021228E-18 ) ) ;
#16242 = CARTESIAN_POINT ( 'NONE',  ( -24.95029760921700301, 9.631514785009935409, -46.58639476887002928 ) ) ;
#16243 = CARTESIAN_POINT ( 'NONE',  ( -48.34250119710924309, 14.01879126850790058, -72.92010011160856209 ) ) ;
#16244 = EDGE_CURVE ( 'NONE', #6794, #27439, #31571, .T. ) ;
#16245 = CARTESIAN_POINT ( 'NONE',  ( -74.81618585058957649, 21.96255056808530881, -89.86471030265687432 ) ) ;
#16246 = DIRECTION ( 'NONE',  ( 0.000000000000000000, 0.000000000000000000, 1.000000000000000000 ) ) ;
#16247 = ORIENTED_EDGE ( 'NONE', *, *, #52014, .F. ) ;
#16248 = ORIENTED_EDGE ( 'NONE', *, *, #50361, .T. ) ;
#16249 = CARTESIAN_POINT ( 'NONE',  ( 32.90051628396145134, 8.664124555952430029, 60.48702334666123193 ) ) ;
#16250 = EDGE_CURVE ( 'NONE', #62318, #59386, #42707, .T. ) ;
#16251 = CARTESIAN_POINT ( 'NONE',  ( 175.0857681883884140, 74.13486472930382831, 94.99999999999866418 ) ) ;
#16252 = CARTESIAN_POINT ( 'NONE',  ( 44.01696072965949469, 47.84694004974210912, 41.38025477438755928 ) ) ;
#16253 = PRODUCT_DEFINITION_CONTEXT ( 'detailed design', #53830, 'design' ) ;
#16254 = DIRECTION ( 'NONE',  ( 0.000000000000000000, -1.000000000000000000, 0.000000000000000000 ) ) ;
#16255 = EDGE_LOOP ( 'NONE', ( #51130, #61123 ) ) ;
#16256 = CARTESIAN_POINT ( 'NONE',  ( 149.0250918491436494, 0.000000000000000000, -36.68900338898720292 ) ) ;
#16257 = CARTESIAN_POINT ( 'NONE',  ( 187.8965227056807521, 87.27289477191496303, -13.73167551492022476 ) ) ;
#16258 = CARTESIAN_POINT ( 'NONE',  ( 211.8345664497467169, 118.5225165986914817, 7.535369598655396572 ) ) ;
#16259 = B_SPLINE_CURVE_WITH_KNOTS ( 'NONE', 3,
 ( #59825, #395, #59131, #4987, #64076, #21505, #58785, #10953, #33118, #10602, #6377, #27831, #26453, #21853, #22554, #32072, #53507, #26795, #48221, #60882, #28169, #49981, #24567, #55254 ),
 .UNSPECIFIED., .F., .F.,
 ( 4, 2, 2, 2, 2, 2, 2, 2, 2, 2, 2, 4 ),
 ( 0.009947828043730422634, 0.01119309618139666812, 0.01243836431906291534, 0.01306099838789603722, 0.01368363245672916083, 0.01492890059439544448, 0.01555153466322857503, 0.01617416873206170558, 0.01741943686972798055, 0.01804207093856113886, 0.01866470500739430063, 0.01990997314506061378 ),
 .UNSPECIFIED. ) ;
#16260 = CARTESIAN_POINT ( 'NONE',  ( 39.40195752203892710, 9.424259417798134919, -50.61981746542779348 ) ) ;
#16261 = CARTESIAN_POINT ( 'NONE',  ( 43.96465529479667111, 9.046527005589348747, -22.24810759540392269 ) ) ;
#16262 = DIRECTION ( 'NONE',  ( -0.000000000000000000, 1.000000000000000000, -0.000000000000000000 ) ) ;
#16263 = CARTESIAN_POINT ( 'NONE',  ( 3.000000000000003997, 24.69999999999999929, 0.000000000000000000 ) ) ;
#16264 = EDGE_CURVE ( 'NONE', #29832, #31339, #27479, .T. ) ;
#16265 = DIRECTION ( 'NONE',  ( -0.000000000000000000, -0.000000000000000000, -1.000000000000000000 ) ) ;
#16266 = EDGE_CURVE ( 'NONE', #44661, #14985, #54033, .T. ) ;
#16267 = ADVANCED_FACE ( 'NONE', ( #52577 ), #4729, .T. ) ;
#16268 = ORIENTED_EDGE ( 'NONE', *, *, #8130, .T. ) ;
#16269 = FACE_OUTER_BOUND ( 'NONE', #3575, .T. ) ;
#16270 = CARTESIAN_POINT ( 'NONE',  ( 88.52077179907880122, 21.14145351760140912, -36.06003046012785518 ) ) ;
#16271 = VECTOR ( 'NONE', #58432, 1000.000000000000000 ) ;
#16272 = CARTESIAN_POINT ( 'NONE',  ( 157.4703587214989113, 58.92748579479259519, -89.81328548006499091 ) ) ;
#16273 = CARTESIAN_POINT ( 'NONE',  ( -15.55634918610408945, -31.11269837220804035, 85.00100000000000477 ) ) ;
#16274 = EDGE_CURVE ( 'NONE', #11337, #41847, #60256, .T. ) ;
#16275 = CARTESIAN_POINT ( 'NONE',  ( 152.3102623290679958, 53.74757787434986511, 15.51308360347570137 ) ) ;
#16276 = CARTESIAN_POINT ( 'NONE',  ( -15.16750062833000001, 8.491651705883104029, 92.86961823882721490 ) ) ;
#16277 = AXIS2_PLACEMENT_3D ( 'NONE', #62356, #30348, #19093 ) ;
#16278 = AXIS2_PLACEMENT_3D ( 'NONE', #6128, #58900, #5447 ) ;
#16279 = ORIENTED_EDGE ( 'NONE', *, *, #41580, .T. ) ;
#16280 = AXIS2_PLACEMENT_3D ( 'NONE', #7548, #50450, #2270 ) ;
#16281 = FACE_OUTER_BOUND ( 'NONE', #3468, .T. ) ;
#16282 = VECTOR ( 'NONE', #11706, 999.9999999999998863 ) ;
#16283 = DIRECTION ( 'NONE',  ( 0.000000000000000000, 0.000000000000000000, -1.000000000000000000 ) ) ;
#16284 = ORIENTED_EDGE ( 'NONE', *, *, #16266, .T. ) ;
#16285 = ORIENTED_EDGE ( 'NONE', *, *, #37302, .T. ) ;
#16286 = LINE ( 'NONE', #27882, #17334 ) ;
#16287 = CARTESIAN_POINT ( 'NONE',  ( 15.55634918610406103, 15.55634918610400241, 2.000000000000001776 ) ) ;
#16288 = CARTESIAN_POINT ( 'NONE',  ( 91.67776154311745529, 22.27748043241296116, -64.61425086459156830 ) ) ;
#16290 = ORIENTED_EDGE ( 'NONE', *, *, #25885, .F. ) ;
#16289 = EDGE_CURVE ( 'NONE', #5114, #4283, #38120, .T. ) ;
#16291 = B_SPLINE_CURVE_WITH_KNOTS ( 'NONE', 3,
 ( #45129, #30346, #66273, #18401, #12786, #56378, #46165, #56734, #18754, #67639, #7856, #61658, #24386, #29304, #13812, #40210, #8550, #30002, #34935, #19091, #35629, #50756, #2577, #13477, #19433, #8199, #23349, #51460, #7520, #24034, #55687, #40544, #28971, #2922, #45829, #29649, #51112, #50416, #67305, #44793, #40895, #61995, #2237, #62354, #3271, #57081, #23685, #34604, #66609, #24731, #39857, #61314, #8893, #1896, #56040, #18064, #13140, #39515, #26100, #57769, #37000, #10598, #52815, #10256, #15200, #20818, #53150, #42617, #41929, #67989, #15884, #4636 ),
 .UNSPECIFIED., .F., .F.,
 ( 4, 2, 2, 2, 2, 2, 2, 2, 2, 2, 2, 2, 2, 2, 2, 2, 2, 2, 2, 2, 2, 2, 2, 2, 2, 2, 2, 2, 2, 2, 2, 2, 2, 2, 2, 4 ),
 ( 0.000000000000000000, 0.001364161439190743471, 0.002046242158786115099, 0.002728322878381486943, 0.004092484317572176421, 0.005456645756762866332, 0.006138726476358211288, 0.006820807195953556244, 0.007502887915548901200, 0.008184968635144247023, 0.008867049354739591979, 0.009549130074334936935, 0.01091329151352568756, 0.01227745295271643992, 0.01364161439190719055, 0.01500577583109794118, 0.01636993727028869181, 0.01909826014867019306, 0.02182658302705169431, 0.02319074446624243974, 0.02455490590543318516, 0.02728322878381467601, 0.02864739022300543531, 0.03001155166219619114, 0.03137571310138694697, 0.03273987454057770974, 0.03410403597976846557, 0.03546819741895922140, 0.03615027813855459238, 0.03683235885814997029, 0.03819652029734069837, 0.03887860101693609016, 0.03956068173653147502, 0.04092484317572224473, 0.04228900461491302137, 0.04365316605410379108 ),
 .UNSPECIFIED. ) ;
#16292 = CARTESIAN_POINT ( 'NONE',  ( -62.15324028806258383, 16.70091357159900980, -67.09546592820414901 ) ) ;
#16293 = MANIFOLD_SOLID_BREP ( 'Extrude-Thin1', #64247 ) ;
#16294 = CARTESIAN_POINT ( 'NONE',  ( 31.90184941268615759, 7.552181687745346039, -16.51731055372926704 ) ) ;
#16295 = ADVANCED_FACE ( 'NONE', ( #17728 ), #38474, .T. ) ;
#16297 = ADVANCED_FACE ( 'NONE', ( #59914 ), #16324, .T. ) ;
#16296 = CARTESIAN_POINT ( 'NONE',  ( 0.000000000000000000, 0.000000000000000000, 2.499999999999999556 ) ) ;
#16298 = DIRECTION ( 'NONE',  ( -1.000000000000000000, 0.000000000000000000, 0.000000000000000000 ) ) ;
#16299 = DIRECTION ( 'NONE',  ( -1.000000000000000000, 0.000000000000000000, 0.000000000000000000 ) ) ;
#16300 = EDGE_LOOP ( 'NONE', ( #49438, #14968, #24865, #35210 ) ) ;
#16301 = CARTESIAN_POINT ( 'NONE',  ( -48.34250119710923599, 14.01879126850789525, -46.07554952114484337 ) ) ;
#16302 = FACE_OUTER_BOUND ( 'NONE', #31686, .T. ) ;
#16303 = CARTESIAN_POINT ( 'NONE',  ( 9.275903038161096958, 7.385619229189526180, 41.26687823360024510 ) ) ;
#16304 = CARTESIAN_POINT ( 'NONE',  ( 447.3372781065086201, 400.0000000000044338, 113.5502958579838122 ) ) ;
#16305 = CARTESIAN_POINT ( 'NONE',  ( -86.11824579438169280, 26.39279658766581349, 92.51845406669916372 ) ) ;
#16306 = ORIENTED_EDGE ( 'NONE', *, *, #66591, .F. ) ;
#16307 = ORIENTED_EDGE ( 'NONE', *, *, #11472, .T. ) ;
#16308 = ORIENTED_EDGE ( 'NONE', *, *, #13966, .T. ) ;
#16309 = CARTESIAN_POINT ( 'NONE',  ( -15.07200981767290671, 7.471751903425206010, -14.12493423355625310 ) ) ;
#16310 = CARTESIAN_POINT ( 'NONE',  ( 204.6977192012829789, -170.0000000000000000, 9.863170148305760776 ) ) ;
#16311 = CARTESIAN_POINT ( 'NONE',  ( -5.000000000000000000, 0.000000000000000000, 85.00100000000000477 ) ) ;
#16312 = CARTESIAN_POINT ( 'NONE',  ( 0.000000000000000000, 190.0000000000000000, 2.000000000000000000 ) ) ;
#16313 = CARTESIAN_POINT ( 'NONE',  ( -59.96408504033280451, 17.10126854471816316, -37.02704747533549323 ) ) ;
#16314 = CARTESIAN_POINT ( 'NONE',  ( -9.524904342798459211, 8.016391612076530393, -23.38257539395581475 ) ) ;
#16315 = CARTESIAN_POINT ( 'NONE',  ( 150.2076397309211870, 52.21780102759852582, -72.36031576144425514 ) ) ;
#16316 = CARTESIAN_POINT ( 'NONE',  ( 21.73827885904431056, 6.764046335627708295, -20.74696102369355799 ) ) ;
#16317 = ORIENTED_EDGE ( 'NONE', *, *, #54699, .T. ) ;
#16318 = AXIS2_PLACEMENT_3D ( 'NONE', #14234, #18814, #68051 ) ;
#16319 = LINE ( 'NONE', #9675, #20560 ) ;
#16320 = VERTEX_POINT ( 'NONE', #12444 ) ;
#16321 = ORIENTED_EDGE ( 'NONE', *, *, #13768, .F. ) ;
#16322 = CARTESIAN_POINT ( 'NONE',  ( 67.54641595172913071, 14.80690682047551476, -10.37962302817197013 ) ) ;
#16323 = AXIS2_PLACEMENT_3D ( 'NONE', #34529, #19022, #67563 ) ;
#16324 = PLANE ( 'NONE',  #19259 ) ;
#16325 = CARTESIAN_POINT ( 'NONE',  ( 36.85262215550149278, -53.56030941157680303, 43.58025477438756923 ) ) ;
#16326 = CARTESIAN_POINT ( 'NONE',  ( -153.6946616617038899, 69.16142959008688251, 5.137162390210407992 ) ) ;
#16327 = VECTOR ( 'NONE', #50802, 1000.000000000000114 ) ;
#16328 = DIRECTION ( 'NONE',  ( 0.3090169943749446757, 0.9510565162951544194, 0.000000000000000000 ) ) ;
#16329 = DIRECTION ( 'NONE',  ( 0.000000000000000000, 0.8660254037844379305, -0.5000000000000013323 ) ) ;
#16330 = CARTESIAN_POINT ( 'NONE',  ( -156.6879335332043865, 71.88581156458076293, 89.73719858978633113 ) ) ;
#16331 = ORIENTED_EDGE ( 'NONE', *, *, #23228, .T. ) ;
#16332 = ORIENTED_EDGE ( 'NONE', *, *, #19845, .T. ) ;
#16333 = AXIS2_PLACEMENT_3D ( 'NONE', #11362, #65909, #22276 ) ;
#16334 = ORIENTED_EDGE ( 'NONE', *, *, #21343, .T. ) ;
#16335 = EDGE_CURVE ( 'NONE', #9782, #27522, #7168, .T. ) ;
#16336 = VECTOR ( 'NONE', #30334, 1000.000000000000000 ) ;
#16337 = CARTESIAN_POINT ( 'NONE',  ( -155.1204242627069902, 70.44799358128193489, -20.44876085833080381 ) ) ;
#16338 = CARTESIAN_POINT ( 'NONE',  ( 36.77024545412685086, 9.095083943590518416, -50.14715022776851328 ) ) ;
#16339 = PLANE ( 'NONE',  #16892 ) ;
#16340 = FACE_OUTER_BOUND ( 'NONE', #28740, .T. ) ;
#16341 = ORIENTED_EDGE ( 'NONE', *, *, #38765, .T. ) ;
#16342 = CARTESIAN_POINT ( 'NONE',  ( 185.7267155939802876, 84.90388481853130997, 57.75814002187100016 ) ) ;
#16343 = CARTESIAN_POINT ( 'NONE',  ( -153.5002794404626059, 67.64160439471098130, 58.71247530986894958 ) ) ;
#16344 = CARTESIAN_POINT ( 'NONE',  ( -1.118033988749894458, 2.632990618166809235E-15, 21.50000000000000000 ) ) ;
#16345 = CARTESIAN_POINT ( 'NONE',  ( 109.7724924842966061, 28.66436020578543520, 17.76666361527367144 ) ) ;
#16346 = DIRECTION ( 'NONE',  ( -0.000000000000000000, -0.000000000000000000, -1.000000000000000000 ) ) ;
#16347 = CARTESIAN_POINT ( 'NONE',  ( -84.55373779407982227, 24.65190748253138509, -47.28824730636777218 ) ) ;
#16348 = CARTESIAN_POINT ( 'NONE',  ( -17.50000000000000000, 207.5000000000000284, 1.999999999999998224 ) ) ;
#16349 = EDGE_CURVE ( 'NONE', #27957, #3914, #64515, .T. ) ;
#16350 = CARTESIAN_POINT ( 'NONE',  ( 16.78635691501517613, 6.000000000000000000, -41.68900338898716740 ) ) ;
#16351 = CARTESIAN_POINT ( 'NONE',  ( 14.80205238535216061, 6.470775952815777110, -77.31449080655163186 ) ) ;
#16352 = EDGE_CURVE ( 'NONE', #7544, #65894, #42564, .T. ) ;
#16353 = ORIENTED_EDGE ( 'NONE', *, *, #27798, .T. ) ;
#16354 = CARTESIAN_POINT ( 'NONE',  ( 74.99999999999998579, 9.184850993605147156E-15, 25.00000000000007816 ) ) ;
#16355 = APPLICATION_PROTOCOL_DEFINITION ( 'draft international standard', 'automotive_design', 1998, #24706 ) ;
#16356 = CARTESIAN_POINT ( 'NONE',  ( 429.8372781065087906, 395.0000000000066507, -133.9497041420121377 ) ) ;
#16357 = CARTESIAN_POINT ( 'NONE',  ( 0.000000000000000000, 0.000000000000000000, -10.00000000000000000 ) ) ;
#16358 = CARTESIAN_POINT ( 'NONE',  ( 43.14712943604299511, 8.926114770663650333, -63.46178131008120715 ) ) ;
#16359 = EDGE_CURVE ( 'NONE', #3478, #5170, #59665, .T. ) ;
#16360 = CARTESIAN_POINT ( 'NONE',  ( 55.64941011647476898, 12.11006142851269729, -68.59167301408281503 ) ) ;
#16361 = VERTEX_POINT ( 'NONE', #2586 ) ;
#16362 = PRODUCT_DEFINITION_SHAPE ( 'NONE', 'NONE',  #69611 ) ;
#16363 = ORIENTED_EDGE ( 'NONE', *, *, #10309, .T. ) ;
#16364 = CARTESIAN_POINT ( 'NONE',  ( -56.92000000000000171, -26.09918303830819397, 0.000000000000000000 ) ) ;
#16365 = CARTESIAN_POINT ( 'NONE',  ( -36.59702049363711041, -36.46867397787282528, 26.66469104408689006 ) ) ;
#16366 = VERTEX_POINT ( 'NONE', #40219 ) ;
#16367 = CIRCLE ( 'NONE', #13029, 200.0000000000000000 ) ;
#16368 = ORIENTED_EDGE ( 'NONE', *, *, #11596, .F. ) ;
#16369 = DIRECTION ( 'NONE',  ( -0.000000000000000000, -0.000000000000000000, -1.000000000000000000 ) ) ;
#16370 = EDGE_LOOP ( 'NONE', ( #4329, #45897 ) ) ;
#16371 = PLANE ( 'NONE',  #32333 ) ;
#16372 = DIRECTION ( 'NONE',  ( -0.000000000000000000, -1.000000000000000000, -0.000000000000000000 ) ) ;
#16373 = VECTOR ( 'NONE', #50952, 1000.000000000000000 ) ;
#16374 = CARTESIAN_POINT ( 'NONE',  ( -63.76691715686636996, 29.79383981485516841, -25.00000000000000711 ) ) ;
#16375 = LINE ( 'NONE', #59274, #44301 ) ;
#16376 = EDGE_CURVE ( 'NONE', #22589, #12081, #58562, .T. ) ;
#16377 = CARTESIAN_POINT ( 'NONE',  ( 81.83553453535668609, 17.84068330693397897, -91.23905641206360428 ) ) ;
#16379 = DIRECTION ( 'NONE',  ( -1.000000000000000000, -1.387778780781445922E-16, 0.000000000000000000 ) ) ;
#16378 = VECTOR ( 'NONE', #27514, 1000.000000000000000 ) ;
#16380 = CYLINDRICAL_SURFACE ( 'NONE', #44298, 7.500000000000013323 ) ;
#16381 =( GEOMETRIC_REPRESENTATION_CONTEXT ( 3 ) GLOBAL_UNCERTAINTY_ASSIGNED_CONTEXT ( ( #49374 ) ) GLOBAL_UNIT_ASSIGNED_CONTEXT ( ( #10284, #38062, #27503 ) ) REPRESENTATION_CONTEXT ( 'NONE', 'WORKASPACE' ) );
#16382 = EDGE_CURVE ( 'NONE', #780, #50735, #59369, .T. ) ;
#16383 = AXIS2_PLACEMENT_3D ( 'NONE', #63730, #41919, #47876 ) ;
#16384 = VERTEX_POINT ( 'NONE', #55699 ) ;
#16385 = ORIENTED_EDGE ( 'NONE', *, *, #52861, .T. ) ;
#16386 = FACE_OUTER_BOUND ( 'NONE', #25743, .T. ) ;
#16387 = AXIS2_PLACEMENT_3D ( 'NONE', #57693, #35890, #24999 ) ;
#16388 = DIRECTION ( 'NONE',  ( 0.000000000000000000, 1.000000000000000000, 0.000000000000000000 ) ) ;
#16389 = CARTESIAN_POINT ( 'NONE',  ( 40.37438610703016906, 8.537526699166104294, -50.57269136638377915 ) ) ;
#16390 = CARTESIAN_POINT ( 'NONE',  ( -166.9992034932274976, 82.01285191063136892, -64.69379323303392937 ) ) ;
#16392 = VERTEX_POINT ( 'NONE', #7530 ) ;
#16391 = CARTESIAN_POINT ( 'NONE',  ( -146.5268141329886475, 61.69196909035589726, -35.42679155757922871 ) ) ;
#16393 = CARTESIAN_POINT ( 'NONE',  ( 0.000000000000000000, 16.00000000000000000, 0.000000000000000000 ) ) ;
#16394 = ORIENTED_EDGE ( 'NONE', *, *, #45188, .F. ) ;
#16395 = CARTESIAN_POINT ( 'NONE',  ( 442.3372781065089612, 390.0000000000074465, -141.4497041420121377 ) ) ;
#16396 = CARTESIAN_POINT ( 'NONE',  ( -89.99999999999998579, 1.102182119232617596E-14, -10.00000000000000000 ) ) ;
#16397 = CARTESIAN_POINT ( 'NONE',  ( 135.6651581599210203, 42.52720121194706593, -23.96109018709176652 ) ) ;
#16398 = CARTESIAN_POINT ( 'NONE',  ( 90.31682503704260512, 20.71196693118262644, -63.61707171944141948 ) ) ;
#16399 = CARTESIAN_POINT ( 'NONE',  ( 62.20100515256353901, 12.48495193239473089, -89.44322602549407009 ) ) ;
#16400 = CARTESIAN_POINT ( 'NONE',  ( -98.46684543088105102, 30.88557736720389002, 17.63727003067570465 ) ) ;
#16401 = CARTESIAN_POINT ( 'NONE',  ( -94.77925136849374610, 29.13093715379787341, -69.12727919511270613 ) ) ;
#16402 = ORIENTED_EDGE ( 'NONE', *, *, #47134, .T. ) ;
#16403 = ORIENTED_EDGE ( 'NONE', *, *, #17879, .F. ) ;
#16404 = CARTESIAN_POINT ( 'NONE',  ( 186.2651679807462415, 84.00458780104315792, -76.01284985794765703 ) ) ;
#16405 = DIRECTION ( 'NONE',  ( 0.000000000000000000, 0.000000000000000000, 1.000000000000000000 ) ) ;
#16406 = FACE_OUTER_BOUND ( 'NONE', #14921, .T. ) ;
#16407 = CYLINDRICAL_SURFACE ( 'NONE', #45263, 7.500000000000027534 ) ;
#16408 = PRODUCT_DEFINITION ( 'UNKNOWN', '', #43332, #26815 ) ;
#16409 = CARTESIAN_POINT ( 'NONE',  ( 107.2614272668149198, 28.62909081796203381, -63.38104519901254008 ) ) ;
#16410 = CARTESIAN_POINT ( 'NONE',  ( -73.81801970646056077, 21.60231032711190835, -63.73264820421131560 ) ) ;
#16411 = PLANE ( 'NONE',  #18021 ) ;
#16412 = CARTESIAN_POINT ( 'NONE',  ( 46.51679720856118649, 10.46086439153924452, -45.54304003388800481 ) ) ;
#16413 = CARTESIAN_POINT ( 'NONE',  ( 210.0292194063021611, 113.9511645670926612, 68.83246835844813916 ) ) ;
#16415 = ORIENTED_EDGE ( 'NONE', *, *, #42188, .F. ) ;
#16414 = EDGE_CURVE ( 'NONE', #63967, #7544, #28981, .T. ) ;
#16416 = CARTESIAN_POINT ( 'NONE',  ( -108.1144194775597640, 35.84457139767599898, -20.40923384673128282 ) ) ;
#16417 = ORIENTED_EDGE ( 'NONE', *, *, #39722, .T. ) ;
#16418 = VECTOR ( 'NONE', #8890, 1000.000000000000000 ) ;
#16419 = CARTESIAN_POINT ( 'NONE',  ( -12.39413342787891281, 7.231444436041491564, -36.95011374576873209 ) ) ;
#16420 = ADVANCED_FACE ( 'NONE', ( #50765 ), #66968, .F. ) ;
#16421 = CARTESIAN_POINT ( 'NONE',  ( -86.16905982510307638, 25.32271692190228407, 91.86796594561636198 ) ) ;
#16422 = CARTESIAN_POINT ( 'NONE',  ( 87.10672734544989737, 20.64813880796637235, 56.55663816294299551 ) ) ;
#16423 = CARTESIAN_POINT ( 'NONE',  ( 152.2940756559018780, 53.73566983921583784, -22.21240161800733759 ) ) ;
#16424 = DIRECTION ( 'NONE',  ( -0.000000000000000000, -1.000000000000000000, -0.000000000000000000 ) ) ;
#16425 = B_SPLINE_CURVE_WITH_KNOTS ( 'NONE', 3,
 ( #43710, #33543, #48983, #10668, #38811, #37753, #38097, #48285, #6449, #11019, #33186, #27900 ),
 .UNSPECIFIED., .F., .F.,
 ( 4, 2, 2, 2, 2, 4 ),
 ( 0.000000000000000000, 0.002494459074786444484, 0.004988918149572888969, 0.007483377224359334320, 0.008730606761752562200, 0.009977836299145791815 ),
 .UNSPECIFIED. ) ;
#16426 = CARTESIAN_POINT ( 'NONE',  ( -96.45303203827904781, 31.03218867996497821, -64.61131369028386473 ) ) ;
#16427 = DIRECTION ( 'NONE',  ( -0.9909497617679352555, 0.1342332658176522697, 2.500042656554811326E-16 ) ) ;
#16428 = AXIS2_PLACEMENT_3D ( 'NONE', #41115, #4855, #68200 ) ;
#16429 = VECTOR ( 'NONE', #63796, 1000.000000000000000 ) ;
#16430 = ORIENTED_EDGE ( 'NONE', *, *, #6934, .T. ) ;
#16431 = DIRECTION ( 'NONE',  ( 1.000000000000000000, -0.000000000000000000, -0.000000000000000000 ) ) ;
#16432 = LINE ( 'NONE', #42803, #43181 ) ;
#16433 = VERTEX_POINT ( 'NONE', #41942 ) ;
#16434 = AXIS2_PLACEMENT_3D ( 'NONE', #32622, #32283, #65329 ) ;
#16435 = DIRECTION ( 'NONE',  ( 1.337618101958020291E-16, 0.000000000000000000, -1.000000000000000000 ) ) ;
#16436 = PLANE ( 'NONE',  #4823 ) ;
#16437 = CARTESIAN_POINT ( 'NONE',  ( -10.69547592951791160, 8.103864096836385755, 3.829060544445804570 ) ) ;
#16438 = CARTESIAN_POINT ( 'NONE',  ( 46.89016064832838993, 10.52130577388959409, -70.45255809555227700 ) ) ;
#16439 = EDGE_CURVE ( 'NONE', #57672, #37468, #62717, .T. ) ;
#16440 = VECTOR ( 'NONE', #36662, 1000.000000000000000 ) ;
#16441 = CARTESIAN_POINT ( 'NONE',  ( -4.081377963939786468, 6.676029627840591729, 31.11232541612353941 ) ) ;
#16442 = LINE ( 'NONE', #38951, #33360 ) ;
#16443 = CARTESIAN_POINT ( 'NONE',  ( 94.07925938825250967, 23.17492699065150319, 91.83144490676588134 ) ) ;
#16444 = ADVANCED_FACE ( 'NONE', ( #20143 ), #63752, .F. ) ;
#16445 = EDGE_CURVE ( 'NONE', #43093, #41688, #53164, .T. ) ;
#16446 = ORIENTED_EDGE ( 'NONE', *, *, #22642, .F. ) ;
#16447 = DIRECTION ( 'NONE',  ( 9.472378821425700939E-15, -3.218422636503495780E-15, 1.000000000000000000 ) ) ;
#16448 = CARTESIAN_POINT ( 'NONE',  ( -452.6627218934912662, 369.9999999999998295, 113.5502958579880328 ) ) ;
#16449 = CARTESIAN_POINT ( 'NONE',  ( -133.2698123908828904, 51.54642138335025692, 12.65949325828542804 ) ) ;
#16450 = CARTESIAN_POINT ( 'NONE',  ( -167.1619226259399227, 82.18315278115417755, -46.77288687742393591 ) ) ;
#16451 = CARTESIAN_POINT ( 'NONE',  ( -133.1566699306513613, 52.70203339370770834, -44.30393921777678656 ) ) ;
#16452 = ORIENTED_EDGE ( 'NONE', *, *, #20088, .T. ) ;
#16453 = CARTESIAN_POINT ( 'NONE',  ( 157.4703587214989398, -170.0000000000000000, 71.25401806271709404 ) ) ;
#16454 = CARTESIAN_POINT ( 'NONE',  ( -15.55634918610411077, -46.66904755831208718, 0.000000000000000000 ) ) ;
#16455 = CARTESIAN_POINT ( 'NONE',  ( 197.3756653044963230, 98.41886189307119537, -18.61350521218830423 ) ) ;
#16456 = DIRECTION ( 'NONE',  ( -1.000000000000000000, 0.000000000000000000, 0.000000000000000000 ) ) ;
#16457 = CARTESIAN_POINT ( 'NONE',  ( 138.6020257460769756, 44.36414356192209851, 42.83845183682598901 ) ) ;
#16458 = ORIENTED_EDGE ( 'NONE', *, *, #20675, .T. ) ;
#16459 = CARTESIAN_POINT ( 'NONE',  ( 0.000000000000000000, 296.0000000000000000, 0.000000000000000000 ) ) ;
#16460 = DIRECTION ( 'NONE',  ( 0.000000000000000000, 0.000000000000000000, 1.000000000000000000 ) ) ;
#16461 = CARTESIAN_POINT ( 'NONE',  ( 164.8444104055694481, 64.93678790243656351, 8.668489052207666745 ) ) ;
#16462 = DIRECTION ( 'NONE',  ( 1.000000000000000000, 0.000000000000000000, 0.000000000000000000 ) ) ;
#16463 = ORIENTED_EDGE ( 'NONE', *, *, #16352, .T. ) ;
#16464 = EDGE_CURVE ( 'NONE', #30354, #34477, #34996, .T. ) ;
#16465 = CARTESIAN_POINT ( 'NONE',  ( 444.9999999999999432, 225.0000000000000000, -2.000000000000000000 ) ) ;
#16466 = ORIENTED_EDGE ( 'NONE', *, *, #59378, .F. ) ;
#16467 = AXIS2_PLACEMENT_3D ( 'NONE', #49523, #7688, #49170 ) ;
#16468 = CARTESIAN_POINT ( 'NONE',  ( -76.31381168750407085, 21.43908608416556660, -8.633424497019335675 ) ) ;
#16469 = CARTESIAN_POINT ( 'NONE',  ( -56.72814287166056602, 15.13700122306437379, 45.13175927368157403 ) ) ;
#16470 = VECTOR ( 'NONE', #5196, 1000.000000000000000 ) ;
#16472 = ORIENTED_EDGE ( 'NONE', *, *, #21285, .T. ) ;
#16471 = CARTESIAN_POINT ( 'NONE',  ( 151.3136733342017521, 54.26417151662143112, 14.35556273797184446 ) ) ;
#16473 = CARTESIAN_POINT ( 'NONE',  ( 164.7167608259061069, 63.51199216609071385, 34.95606193614021606 ) ) ;
#16474 = DIRECTION ( 'NONE',  ( 0.000000000000000000, 0.000000000000000000, 1.000000000000000000 ) ) ;
#16475 = CARTESIAN_POINT ( 'NONE',  ( 157.4703587214989398, -170.0000000000000000, 63.75401806271707983 ) ) ;
#16476 = VERTEX_POINT ( 'NONE', #52499 ) ;
#16477 = CARTESIAN_POINT ( 'NONE',  ( 63.01563776193091826, 12.67277567978500130, -35.72069083216973695 ) ) ;
#16478 = LINE ( 'NONE', #37931, #67089 ) ;
#16479 = CARTESIAN_POINT ( 'NONE',  ( -31.93184248720560348, 9.672312402099827011, -8.472646774738155528 ) ) ;
#16480 = CARTESIAN_POINT ( 'NONE',  ( -180.5801285865471471, 97.42945596116099694, 37.52258506186108633 ) ) ;
#16481 = CARTESIAN_POINT ( 'NONE',  ( -37.38262509017737045, 10.64263598035110014, -65.06093979278308836 ) ) ;
#16482 = VERTEX_POINT ( 'NONE', #42628 ) ;
#16483 = ORIENTED_EDGE ( 'NONE', *, *, #62346, .T. ) ;
#16484 = VERTEX_POINT ( 'NONE', #57434 ) ;
#16485 = PLANE ( 'NONE',  #22767 ) ;
#16486 = ADVANCED_FACE ( 'NONE', ( #35978 ), #63407, .T. ) ;
#16487 = CARTESIAN_POINT ( 'NONE',  ( -47.54588915626003853, 12.79638599324405490, 91.55540593693795870 ) ) ;
#16488 = CARTESIAN_POINT ( 'NONE',  ( 0.000000000000000000, 0.000000000000000000, -10.00000000000000000 ) ) ;
#16489 = CARTESIAN_POINT ( 'NONE',  ( 7.762887554996211747E-14, 51.66904755831208718, 0.000000000000000000 ) ) ;
#16490 = CARTESIAN_POINT ( 'NONE',  ( -108.3113955865101161, 35.95170844434134239, 87.23892145708312285 ) ) ;
#16491 = DIRECTION ( 'NONE',  ( 0.8584487936018728726, -0.5128992774058949156, 0.000000000000000000 ) ) ;
#16492 = DIRECTION ( 'NONE',  ( -1.000000000000000000, 0.000000000000000000, 0.000000000000000000 ) ) ;
#16493 = EDGE_CURVE ( 'NONE', #34795, #49146, #41109, .T. ) ;
#16494 = DIRECTION ( 'NONE',  ( -0.8118923937861950435, -0.5838071093367415143, 0.000000000000000000 ) ) ;
#16495 = VERTEX_POINT ( 'NONE', #15210 ) ;
#16496 = CARTESIAN_POINT ( 'NONE',  ( 417.3372781065085633, 400.0000000000000568, -146.4497041420118251 ) ) ;
#16498 = ORIENTED_EDGE ( 'NONE', *, *, #33549, .F. ) ;
#16497 = ADVANCED_FACE ( 'NONE', ( #15897 ), #56323, .T. ) ;
#16499 = SURFACE_STYLE_USAGE ( .BOTH. , #17898 ) ;
#16500 = CARTESIAN_POINT ( 'NONE',  ( 181.0840389613909736, 78.60582251573003987, 29.30859410551139277 ) ) ;
#16501 = DIRECTION ( 'NONE',  ( 0.000000000000000000, 0.000000000000000000, -1.000000000000000000 ) ) ;
#16502 = CARTESIAN_POINT ( 'NONE',  ( -73.09185868250600038, 20.27574131633382137, 16.11495310017765803 ) ) ;
#16503 = FACE_OUTER_BOUND ( 'NONE', #41391, .T. ) ;
#16504 = ADVANCED_FACE ( 'NONE', ( #9593 ), #55216, .T. ) ;
#16505 = CARTESIAN_POINT ( 'NONE',  ( 23.04797191264876233, 7.849755664016362822, 35.56853372841017347 ) ) ;
#16506 = DIRECTION ( 'NONE',  ( 0.000000000000000000, 0.000000000000000000, -1.000000000000000000 ) ) ;
#16507 = CARTESIAN_POINT ( 'NONE',  ( -46.66904755831212981, -10.55634918610397222, 85.00100000000000477 ) ) ;
#16508 = CARTESIAN_POINT ( 'NONE',  ( 161.7031777507227162, 62.31724004902784486, -64.26033578956516124 ) ) ;
#16509 = ORIENTED_EDGE ( 'NONE', *, *, #26061, .T. ) ;
#16510 = FACE_OUTER_BOUND ( 'NONE', #25888, .T. ) ;
#16511 = CARTESIAN_POINT ( 'NONE',  ( 110.2429982417149574, -170.0000000000000000, -43.42243756565370205 ) ) ;
#16512 = ORIENTED_EDGE ( 'NONE', *, *, #32179, .T. ) ;
#16513 = ORIENTED_EDGE ( 'NONE', *, *, #8704, .F. ) ;
#16514 = CARTESIAN_POINT ( 'NONE',  ( -82.93267503967652488, 23.99263498936122474, 44.09127840080141425 ) ) ;
#16515 = CARTESIAN_POINT ( 'NONE',  ( 157.4703587214989113, 58.92748579479258808, -77.96873488960135035 ) ) ;
#16516 = CARTESIAN_POINT ( 'NONE',  ( 46.65974587859240330, 10.48396258569371042, 35.45994816272273908 ) ) ;
#16517 = VECTOR ( 'NONE', #62195, 1000.000000000000000 ) ;
#16518 = CARTESIAN_POINT ( 'NONE',  ( -29.51060362117876679, 9.282716514427260535, 57.30906105449729182 ) ) ;
#16519 = DIRECTION ( 'NONE',  ( 1.000000000000000000, 0.000000000000000000, -0.000000000000000000 ) ) ;
#16520 = EDGE_CURVE ( 'NONE', #29447, #327, #3970, .T. ) ;
#16521 = VECTOR ( 'NONE', #10457, 1000.000000000000227 ) ;
#16522 = EDGE_CURVE ( 'NONE', #7422, #33643, #52826, .T. ) ;
#16523 = ORIENTED_EDGE ( 'NONE', *, *, #65920, .T. ) ;
#16524 = MANIFOLD_SOLID_BREP ( 'Boss-Extrude4', #14838 ) ;
#16525 = VERTEX_POINT ( 'NONE', #49275 ) ;
#16526 = CARTESIAN_POINT ( 'NONE',  ( -129.6079169496900931, 50.20899308323959787, 44.63993178974271814 ) ) ;
#16527 = EDGE_LOOP ( 'NONE', ( #47798, #55734, #14091, #45753 ) ) ;
#16528 = CARTESIAN_POINT ( 'NONE',  ( 209.9999999999999716, 192.0000000000000000, 93.99999999999998579 ) ) ;
#16529 = CARTESIAN_POINT ( 'NONE',  ( 182.4828945259410773, 81.47614346340601799, -90.03736357220414277 ) ) ;
#16530 = CARTESIAN_POINT ( 'NONE',  ( 55.52750043885183828, 11.05966813607792787, 63.66763205657868951 ) ) ;
#16531 = CARTESIAN_POINT ( 'NONE',  ( -4.071369321747696723, 7.682719369516285646, 70.97146076770519585 ) ) ;
#16532 = AXIS2_PLACEMENT_3D ( 'NONE', #62277, #31318, #62972 ) ;
#16533 = CARTESIAN_POINT ( 'NONE',  ( -55.15976438495108169, -34.41253982194112382, 170.0000000000000000 ) ) ;
#16534 = CARTESIAN_POINT ( 'NONE',  ( 133.8566784816069060, 42.60093787723655367, 71.35489142945907304 ) ) ;
#16535 = AXIS2_PLACEMENT_3D ( 'NONE', #4386, #52562, #57505 ) ;
#16536 = DIRECTION ( 'NONE',  ( 1.000000000000000000, 0.000000000000000000, -0.000000000000000000 ) ) ;
#16537 = ORIENTED_EDGE ( 'NONE', *, *, #5789, .T. ) ;
#16538 = VERTEX_POINT ( 'NONE', #59140 ) ;
#16539 = CARTESIAN_POINT ( 'NONE',  ( 109.9975424824652634, 295.6904194069557548, 539.5330678552892323 ) ) ;
#16540 = DIRECTION ( 'NONE',  ( 0.000000000000000000, 0.000000000000000000, 1.000000000000000000 ) ) ;
#16541 = FACE_OUTER_BOUND ( 'NONE', #31950, .T. ) ;
#16542 = LINE ( 'NONE', #63703, #26524 ) ;
#16543 = CARTESIAN_POINT ( 'NONE',  ( 63.01563776193090405, 12.67277567978497643, 44.81296093922130552 ) ) ;
#16544 = ORIENTED_EDGE ( 'NONE', *, *, #26581, .T. ) ;
#16545 = CARTESIAN_POINT ( 'NONE',  ( 79.92465405224851338, 17.24122384219593940, 13.76543913484589510 ) ) ;
#16546 = CYLINDRICAL_SURFACE ( 'NONE', #13702, 7.500000000000020428 ) ;
#16547 = CARTESIAN_POINT ( 'NONE',  ( -75.00168449119587422, 20.95943092127970431, 44.46631830285968334 ) ) ;
#16548 = ORIENTED_EDGE ( 'NONE', *, *, #8179, .T. ) ;
#16549 = ORIENTED_EDGE ( 'NONE', *, *, #55046, .T. ) ;
#16550 = CARTESIAN_POINT ( 'NONE',  ( -452.6627218934912094, 399.9999999999998295, 113.5502958579882602 ) ) ;
#16551 = CARTESIAN_POINT ( 'NONE',  ( 94.12988949694084795, 22.11811104795076588, 10.60322717497807687 ) ) ;
#16552 = CARTESIAN_POINT ( 'NONE',  ( 8.000000000000007105, 249.8719672152120381, 94.99999999999866418 ) ) ;
#16553 = ORIENTED_EDGE ( 'NONE', *, *, #34877, .T. ) ;
#16554 = CIRCLE ( 'NONE', #34567, 20.00000000000000000 ) ;
#16555 = CARTESIAN_POINT ( 'NONE',  ( 0.7145311798161616545, -4.618802153517262532, -8.000000000000001776 ) ) ;
#16556 = DIRECTION ( 'NONE',  ( -2.497525279955785470E-16, 1.121639896553560265E-17, 1.000000000000000000 ) ) ;
#16557 = AXIS2_PLACEMENT_3D ( 'NONE', #18172, #45239, #6569 ) ;
#16558 = CARTESIAN_POINT ( 'NONE',  ( 154.4429418375333114, 55.33424769452794578, 30.03275206029211830 ) ) ;
#16559 = CARTESIAN_POINT ( 'NONE',  ( 63.01563776193090405, 13.70579113808097738, 44.81296093922130552 ) ) ;
#16560 = DIRECTION ( 'NONE',  ( -1.393823445737823288E-16, -0.7660444431189770143, 0.6427876096865403621 ) ) ;
#16561 = DIRECTION ( 'NONE',  ( -1.000000000000000000, 9.109522253334613014E-16, 1.697894969632811141E-16 ) ) ;
#16562 = LINE ( 'NONE', #64058, #31608 ) ;
#16563 = FACE_OUTER_BOUND ( 'NONE', #32019, .T. ) ;
#16564 = CARTESIAN_POINT ( 'NONE',  ( 6.000000000000000000, 23.07878402833891229, 9.999999999999998224 ) ) ;
#16565 = ORIENTED_EDGE ( 'NONE', *, *, #44150, .T. ) ;
#16566 = FACE_BOUND ( 'NONE', #12318, .T. ) ;
#16567 = DIRECTION ( 'NONE',  ( -0.000000000000000000, 1.000000000000000000, -0.000000000000000000 ) ) ;
#16568 = DIRECTION ( 'NONE',  ( -1.000000000000000000, 1.232595164407830946E-32, 7.703719777548943412E-34 ) ) ;
#16569 = CARTESIAN_POINT ( 'NONE',  ( 31.11269837220812562, 31.11269837220800483, 2.000000000000001776 ) ) ;
#16570 = CYLINDRICAL_SURFACE ( 'NONE', #41132, 65.00000000000000000 ) ;
#16571 = CIRCLE ( 'NONE', #59247, 4.999999999999997335 ) ;
#16572 = CARTESIAN_POINT ( 'NONE',  ( -3.364862276288897558, 74.92447999059858432, 43.58025477438756212 ) ) ;
#16573 = CARTESIAN_POINT ( 'NONE',  ( 114.7436796776308086, 21.94282408638629889, 1.613761426918485897 ) ) ;
#16574 = CARTESIAN_POINT ( 'NONE',  ( 0.000000000000000000, 0.000000000000000000, 0.000000000000000000 ) ) ;
#16575 = EDGE_CURVE ( 'NONE', #26339, #21211, #29985, .T. ) ;
#16576 = DIRECTION ( 'NONE',  ( -0.000000000000000000, -1.000000000000000000, -0.000000000000000000 ) ) ;
#16577 = CARTESIAN_POINT ( 'NONE',  ( -86.15466590221103615, 26.40813842494317498, 65.25490091457173492 ) ) ;
#16579 = CARTESIAN_POINT ( 'NONE',  ( 91.67776154311752634, 22.27748043241297538, -10.92514968366423034 ) ) ;
#16578 = B_SPLINE_CURVE_WITH_KNOTS ( 'NONE', 3,
 ( #14835, #10585, #68644, #32058, #31373, #20456, #59117, #53493, #63381, #16216, #5324, #10936, #15191, #36651, #21487, #58098, #26781, #48207, #47520, #9918, #32, #52802, #64404, #20808, #37670, #32408, #64758, #1436, #49962, #48900, #43633, #23254, #60170, #382, #22891, #48546, #60865, #6710, #5652, #54887, #28155, #11990, #22540, #65107, #49603, #43980 ),
 .UNSPECIFIED., .F., .F.,
 ( 4, 2, 2, 2, 2, 2, 2, 2, 2, 2, 2, 2, 2, 2, 2, 2, 2, 2, 2, 2, 2, 2, 4 ),
 ( 3.986091072867590107E-17, 0.003373244802897413987, 0.004216556003621757184, 0.005059867204346100815, 0.006746489605794788076, 0.007589800806519115227, 0.008433112007243441510, 0.009276423207967768661, 0.01011973440869209581, 0.01180635681014072062, 0.01349297921158934370, 0.01433629041231365524, 0.01517960161303797025, 0.01686622401448657424, 0.01770953521521087884, 0.01855284641593518344, 0.02023946881738376835, 0.02108278001810802785, 0.02192609121883228734, 0.02361271362028080287, 0.02445602482100502767, 0.02529933602172925594, 0.02698595842317763963 ),
 .UNSPECIFIED. ) ;
#16580 = ORIENTED_EDGE ( 'NONE', *, *, #2780, .F. ) ;
#16581 = CIRCLE ( 'NONE', #40194, 245.3095347406802773 ) ;
#16582 = CARTESIAN_POINT ( 'NONE',  ( -33.85171821065139852, 11.02091558840053764, 17.98985968378708122 ) ) ;
#16583 = ORIENTED_EDGE ( 'NONE', *, *, #17292, .F. ) ;
#16584 = DIRECTION ( 'NONE',  ( -0.000000000000000000, 1.000000000000000000, -0.000000000000000000 ) ) ;
#16585 = CARTESIAN_POINT ( 'NONE',  ( 82.95856197793166587, 19.25847567427441120, -76.72461906074219939 ) ) ;
#16586 = CARTESIAN_POINT ( 'NONE',  ( 115.7592475865162527, 32.64122214332899574, 85.70808474779904884 ) ) ;
#16587 = CARTESIAN_POINT ( 'NONE',  ( -142.1332311300253082, 59.44822332309658464, 63.66972751217561921 ) ) ;
#16588 = EDGE_CURVE ( 'NONE', #805, #37653, #36720, .T. ) ;
#16589 = FACE_OUTER_BOUND ( 'NONE', #56342, .T. ) ;
#16590 = CARTESIAN_POINT ( 'NONE',  ( -28.13527276074847805, 10.08983026464524713, -49.55478388655180311 ) ) ;
#16591 = CARTESIAN_POINT ( 'NONE',  ( -54.08816720029309977, 15.46531105893042124, -62.10765360863577200 ) ) ;
#16592 = CARTESIAN_POINT ( 'NONE',  ( -78.66644367742109978, 23.39876645725289706, -88.80455181264524356 ) ) ;
#16593 = CARTESIAN_POINT ( 'NONE',  ( 432.4999999999999432, -17.50000000000000000, 0.000000000000000000 ) ) ;
#16594 = VERTEX_POINT ( 'NONE', #18328 ) ;
#16595 = ORIENTED_EDGE ( 'NONE', *, *, #31517, .F. ) ;
#16596 = CARTESIAN_POINT ( 'NONE',  ( 38.91512155099544401, 9.360679678889624711, 56.75838489642694640 ) ) ;
#16597 = CARTESIAN_POINT ( 'NONE',  ( 132.3682272970516465, 41.70269401232697959, -89.82203283494803259 ) ) ;
#16598 = EDGE_CURVE ( 'NONE', #43800, #24193, #60889, .T. ) ;
#16599 = CARTESIAN_POINT ( 'NONE',  ( 69.67874066886028572, 15.35768729680762412, -93.44190485051720430 ) ) ;
#16600 = ORIENTED_EDGE ( 'NONE', *, *, #30899, .T. ) ;
#16601 = CARTESIAN_POINT ( 'NONE',  ( 89.20981392318257974, 21.38519354635263525, 17.41376394564116126 ) ) ;
#16602 = CARTESIAN_POINT ( 'NONE',  ( -7.825402957745087207, 6.891034867348159842, 71.96013162991091860 ) ) ;
#16603 = CARTESIAN_POINT ( 'NONE',  ( 212.0779786303465357, 118.9010947973413010, 8.485549497644882422 ) ) ;
#16604 = CIRCLE ( 'NONE', #4270, 5.000000000000000888 ) ;
#16605 = DIRECTION ( 'NONE',  ( 0.000000000000000000, 1.000000000000000000, 0.000000000000000000 ) ) ;
#16606 = DIRECTION ( 'NONE',  ( 0.000000000000000000, -0.02271222823333339177, 0.9997420440737084801 ) ) ;
#16607 = CARTESIAN_POINT ( 'NONE',  ( 210.1633650091870607, 114.1507944623967319, -22.12313984221156105 ) ) ;
#16608 = CARTESIAN_POINT ( 'NONE',  ( 107.7821011353898939, 21.53668059256674283, -4.493084242282758822 ) ) ;
#16609 = CARTESIAN_POINT ( 'NONE',  ( 160.9097745014958036, 61.67033591969548922, 70.42277619118128484 ) ) ;
#16610 = CONICAL_SURFACE ( 'NONE', #40229, 200.0000000000000000, 1.279339532317029793 ) ;
#16611 = ORIENTED_EDGE ( 'NONE', *, *, #14530, .T. ) ;
#16612 = VECTOR ( 'NONE', #69121, 1000.000000000000000 ) ;
#16613 = LINE ( 'NONE', #5377, #6582 ) ;
#16614 = CARTESIAN_POINT ( 'NONE',  ( 90.91356992076215704, 21.99794663086831292, -37.16094633631047373 ) ) ;
#16615 = CARTESIAN_POINT ( 'NONE',  ( -48.23389383802712871, 13.99288361739332132, 61.52903241797603329 ) ) ;
#16616 = CARTESIAN_POINT ( 'NONE',  ( -16.35146342289110422, 18.91109843266242052, 0.000000000000000000 ) ) ;
#16617 = CARTESIAN_POINT ( 'NONE',  ( 157.4703587214989113, 57.65129005721576050, 17.56491688178971700 ) ) ;
#16618 = CARTESIAN_POINT ( 'NONE',  ( -15.32007997986256953, 8.506358610388080166, 90.59327875642129868 ) ) ;
#16619 = AXIS2_PLACEMENT_3D ( 'NONE', #39594, #2656, #40976 ) ;
#16620 = ORIENTED_EDGE ( 'NONE', *, *, #51700, .F. ) ;
#16621 = CARTESIAN_POINT ( 'NONE',  ( 0.000000000000000000, 0.000000000000000000, 0.000000000000000000 ) ) ;
#16622 = CARTESIAN_POINT ( 'NONE',  ( -62.30463872474476972, 16.74658165105247676, 62.68421133332508077 ) ) ;
#16623 = EDGE_LOOP ( 'NONE', ( #32176, #25986, #16186, #30724, #41952 ) ) ;
#16624 = AXIS2_PLACEMENT_3D ( 'NONE', #3618, #30704, #62718 ) ;
#16625 = ORIENTED_EDGE ( 'NONE', *, *, #12907, .T. ) ;
#16626 = CARTESIAN_POINT ( 'NONE',  ( 0.000000000000000000, 0.000000000000000000, 40.00000000000003553 ) ) ;
#16627 = CARTESIAN_POINT ( 'NONE',  ( 111.9975424824652634, 20.00000000000003197, 256.6193948016162381 ) ) ;
#16628 = CARTESIAN_POINT ( 'NONE',  ( 103.4696172145934838, 25.87254488218942328, 40.34164898042279646 ) ) ;
#16629 = VERTEX_POINT ( 'NONE', #40138 ) ;
#16630 = CARTESIAN_POINT ( 'NONE',  ( -57.43251939610647838, 15.33203492375494470, -76.68981896774998575 ) ) ;
#16631 = CARTESIAN_POINT ( 'NONE',  ( 32.90953848114694580, 7.653665824624193093, -20.03817694765365331 ) ) ;
#16632 = CARTESIAN_POINT ( 'NONE',  ( 173.5844030397476274, 72.71952271766127751, -44.03001291059575806 ) ) ;
#16633 = CARTESIAN_POINT ( 'NONE',  ( -149.5074843970971017, 64.17983161892347255, 18.87627064943540134 ) ) ;
#16634 = LINE ( 'NONE', #19587, #32866 ) ;
#16635 = CARTESIAN_POINT ( 'NONE',  ( 88.99522780200238969, 20.24180937454203644, 44.33318672426325691 ) ) ;
#16636 = EDGE_CURVE ( 'NONE', #18961, #49715, #39787, .T. ) ;
#16637 = VERTEX_POINT ( 'NONE', #56306 ) ;
#16639 = EDGE_CURVE ( 'NONE', #29783, #35065, #49988, .T. ) ;
#16638 = CARTESIAN_POINT ( 'NONE',  ( 110.2429982417149574, 29.99119854320843714, -9.077886975189997543 ) ) ;
#16640 = DIRECTION ( 'NONE',  ( 1.000000000000000000, 0.000000000000000000, 0.000000000000000000 ) ) ;
#16641 = B_SPLINE_CURVE_WITH_KNOTS ( 'NONE', 3,
 ( #50412, #35270, #29994, #45824, #18059, #56372 ),
 .UNSPECIFIED., .F., .F.,
 ( 4, 2, 4 ),
 ( 0.03218933845493736345, 0.06469832000440858821, 0.09720730155387982685 ),
 .UNSPECIFIED. ) ;
#16642 = CARTESIAN_POINT ( 'NONE',  ( -4.999999999999971578, 20.55634918610402906, 2.000000000000001776 ) ) ;
#16643 = PLANE ( 'NONE',  #33831 ) ;
#16644 = CARTESIAN_POINT ( 'NONE',  ( 26.12852347772543737, 100.0000000000000000, 77.58025477438755502 ) ) ;
#16646 = VERTEX_POINT ( 'NONE', #45763 ) ;
#16645 = DIRECTION ( 'NONE',  ( -0.9009688679024155933, -0.4338837391175656699, 0.000000000000000000 ) ) ;
#16647 = EDGE_LOOP ( 'NONE', ( #32546, #36119, #68266, #28589 ) ) ;
#16648 = ORIENTED_EDGE ( 'NONE', *, *, #47937, .T. ) ;
#16649 = CARTESIAN_POINT ( 'NONE',  ( -11.14880195267006435, 7.129907723790824825, -9.332131539978064438 ) ) ;
#16650 = CARTESIAN_POINT ( 'NONE',  ( -169.8036256908229973, 84.98540282375472543, 85.26356001004853624 ) ) ;
#16651 = CARTESIAN_POINT ( 'NONE',  ( -52.68007207639880107, 14.05813534436550150, -22.99069914386438995 ) ) ;
#16652 = LINE ( 'NONE', #53237, #64671 ) ;
#16653 = EDGE_CURVE ( 'NONE', #42599, #2074, #35202, .T. ) ;
#16654 = CARTESIAN_POINT ( 'NONE',  ( -62.55184817504200367, 17.87278652436698323, -43.23193394049161498 ) ) ;
#16655 = EDGE_CURVE ( 'NONE', #16958, #38815, #24660, .T. ) ;
#16656 = CARTESIAN_POINT ( 'NONE',  ( -12.40598104375062860, 8.242193636955580160, -10.11445045639250040 ) ) ;
#16657 = AXIS2_PLACEMENT_3D ( 'NONE', #26661, #63948, #26322 ) ;
#16658 = CARTESIAN_POINT ( 'NONE',  ( 152.1327777395850660, 53.61712543276776444, -65.19409239134269285 ) ) ;
#16659 = CARTESIAN_POINT ( 'NONE',  ( 21.25987915030396280, 6.737472588634915382, -21.30969410552895127 ) ) ;
#16660 = B_SPLINE_CURVE_WITH_KNOTS ( 'NONE', 3,
 ( #10361, #55623, #28909, #17289, #33136, #37103 ),
 .UNSPECIFIED., .F., .F.,
 ( 4, 2, 4 ),
 ( 1.095770181109144105E-06, 0.03239442681617710207, 0.06478775786217309818 ),
 .UNSPECIFIED. ) ;
#16661 = ORIENTED_EDGE ( 'NONE', *, *, #59463, .F. ) ;
#16662 = CARTESIAN_POINT ( 'NONE',  ( 0.000000000000000000, 6.000000000000000000, 0.000000000000000000 ) ) ;
#16663 = EDGE_LOOP ( 'NONE', ( #35157, #62200, #1465, #48632, #20623, #41173, #55680 ) ) ;
#16664 = EDGE_LOOP ( 'NONE', ( #35732, #42595, #2716, #42915 ) ) ;
#16665 = AXIS2_PLACEMENT_3D ( 'NONE', #47766, #21050, #42497 ) ;
#16666 = CARTESIAN_POINT ( 'NONE',  ( -142.5087559769084748, 59.74468185400777998, 14.12501252483976977 ) ) ;
#16667 = CARTESIAN_POINT ( 'NONE',  ( -55.90809155135389830, 15.95534155093521633, -88.95128615556963325 ) ) ;
#16668 = CARTESIAN_POINT ( 'NONE',  ( -24.43167697712097208, 9.560946958255405193, 88.71272639884266198 ) ) ;
#16669 = EDGE_CURVE ( 'NONE', #69309, #32392, #34177, .T. ) ;
#16670 = CARTESIAN_POINT ( 'NONE',  ( -152.4930836497867404, 68.09400557494205941, 4.492453323582243918 ) ) ;
#16671 = CARTESIAN_POINT ( 'NONE',  ( -108.5289085648060450, 36.07014995015116199, 15.32950029942471737 ) ) ;
#16672 = CARTESIAN_POINT ( 'NONE',  ( 24.36509522348982060, 70.94296747916789059, 170.0000000000000000 ) ) ;
#16673 = CARTESIAN_POINT ( 'NONE',  ( -154.6185427734352515, 69.99209860720225151, 86.39051265489474929 ) ) ;
#16674 = EDGE_LOOP ( 'NONE', ( #43350, #15765, #37484, #21366 ) ) ;
#16675 = ORIENTED_EDGE ( 'NONE', *, *, #13355, .F. ) ;
#16676 = ORIENTED_EDGE ( 'NONE', *, *, #65529, .T. ) ;
#16677 = CARTESIAN_POINT ( 'NONE',  ( 0.000000000000000000, 0.000000000000000000, -9.500000000000000000 ) ) ;
#16678 = CARTESIAN_POINT ( 'NONE',  ( -149.9475539515598541, 65.87716206616011050, -7.968279941028271196 ) ) ;
#16679 = CARTESIAN_POINT ( 'NONE',  ( 90.44107021831128179, 21.82636779519387105, -90.53914462835739130 ) ) ;
#16680 = ADVANCED_FACE ( 'NONE', ( #62636 ), #47464, .F. ) ;
#16681 = CARTESIAN_POINT ( 'NONE',  ( -31.43908319763710679, 9.591432048623762086, 72.06100499665289760 ) ) ;
#16682 = EDGE_CURVE ( 'NONE', #55179, #65524, #14778, .T. ) ;
#16683 = CARTESIAN_POINT ( 'NONE',  ( -154.7998111145352027, 68.80117179139328698, -20.80406720516667463 ) ) ;
#16684 = ADVANCED_FACE ( 'NONE', ( #30972 ), #52418, .T. ) ;
#16685 = ORIENTED_EDGE ( 'NONE', *, *, #59213, .T. ) ;
#16686 = EDGE_CURVE ( 'NONE', #66948, #47684, #54082, .T. ) ;
#16687 = CARTESIAN_POINT ( 'NONE',  ( 187.5165082312809659, 86.85340440641661530, 59.78757442739207306 ) ) ;
#16688 = CARTESIAN_POINT ( 'NONE',  ( -156.3790798118593841, 70.23422112803316963, 62.04827372833165100 ) ) ;
#16689 = DIRECTION ( 'NONE',  ( -3.687791819402489765E-18, 3.525890001671242775E-18, -1.000000000000000000 ) ) ;
#16690 = CYLINDRICAL_SURFACE ( 'NONE', #563, 65.36598343705435354 ) ;
#16691 = DIRECTION ( 'NONE',  ( 1.850550996349095901E-16, -1.000000000000000000, 5.551115123125781470E-17 ) ) ;
#16692 = CARTESIAN_POINT ( 'NONE',  ( 24.36509522349078338, -70.94296747916756374, 170.0000000000000000 ) ) ;
#16693 = LINE ( 'NONE', #37449, #33263 ) ;
#16694 = CARTESIAN_POINT ( 'NONE',  ( 11.21653854975268949, 6.397128675385706842, -63.89780128798599890 ) ) ;
#16695 = ORIENTED_EDGE ( 'NONE', *, *, #59785, .T. ) ;
#16696 = LINE ( 'NONE', #21626, #6891 ) ;
#16697 = CARTESIAN_POINT ( 'NONE',  ( -131.2803255164624829, 50.14412978403780130, -64.03362474960219686 ) ) ;
#16698 = CARTESIAN_POINT ( 'NONE',  ( -133.3765738414514885, 51.62252165471728915, -41.83704703482699472 ) ) ;
#16699 = CARTESIAN_POINT ( 'NONE',  ( 43.35980717318837208, 8.957244490220915623, -63.58895816981770110 ) ) ;
#16700 = CARTESIAN_POINT ( 'NONE',  ( -84.49322488516129681, 0.000000000000000000, 43.58025477438756212 ) ) ;
#16701 = VERTEX_POINT ( 'NONE', #20748 ) ;
#16702 = EDGE_LOOP ( 'NONE', ( #56253, #49401, #28186, #20785 ) ) ;
#16703 = CARTESIAN_POINT ( 'NONE',  ( -30.46060138092287772, 9.432375387772211184, -8.520515782790420545 ) ) ;
#16704 = CARTESIAN_POINT ( 'NONE',  ( 185.5791793180738694, 83.26975658156528937, 84.46066206085653505 ) ) ;
#16705 = ORIENTED_EDGE ( 'NONE', *, *, #56859, .T. ) ;
#16706 = ORIENTED_EDGE ( 'NONE', *, *, #44302, .F. ) ;
#16707 = CARTESIAN_POINT ( 'NONE',  ( 188.5653887627528036, 88.01608521313127653, 36.19925310697095711 ) ) ;
#16708 = CARTESIAN_POINT ( 'NONE',  ( 0.000000000000000000, 0.000000000000000000, 170.0000000000000000 ) ) ;
#16709 = ORIENTED_EDGE ( 'NONE', *, *, #9605, .F. ) ;
#16710 = CARTESIAN_POINT ( 'NONE',  ( 112.5537757279407032, 31.07998172410697180, 71.10680706731751854 ) ) ;
#16711 = AXIS2_PLACEMENT_3D ( 'NONE', #23409, #55038, #27259 ) ;
#16712 = CARTESIAN_POINT ( 'NONE',  ( 137.6104751318276840, 44.92718313329107360, 57.35758373017568346 ) ) ;
#16713 = CYLINDRICAL_SURFACE ( 'NONE', #26342, 7.500000000000013323 ) ;
#16714 = CARTESIAN_POINT ( 'NONE',  ( 162.2907419228889410, 61.49817556009425346, -91.55379821537337648 ) ) ;
#16715 = AXIS2_PLACEMENT_3D ( 'NONE', #64722, #720, #53109 ) ;
#16716 = FACE_OUTER_BOUND ( 'NONE', #17583, .T. ) ;
#16717 = CARTESIAN_POINT ( 'NONE',  ( -189.4223925288096382, 107.3427006758676470, 40.14341618987140947 ) ) ;
#16718 = ORIENTED_EDGE ( 'NONE', *, *, #63160, .T. ) ;
#16719 = VERTEX_POINT ( 'NONE', #58370 ) ;
#16721 = EDGE_CURVE ( 'NONE', #62736, #36820, #9509, .T. ) ;
#16720 = PLANE ( 'NONE',  #44599 ) ;
#16722 = FACE_BOUND ( 'NONE', #46600, .T. ) ;
#16723 = CARTESIAN_POINT ( 'NONE',  ( 43.14356474118745410, 8.925336319666900664, -49.63851462474485743 ) ) ;
#16724 = DIRECTION ( 'NONE',  ( -3.035766082959413401E-16, 1.033681467326434846E-16, 1.000000000000000000 ) ) ;
#16726 = ORIENTED_EDGE ( 'NONE', *, *, #57514, .T. ) ;
#16725 = DIRECTION ( 'NONE',  ( -1.000000000000000000, 0.000000000000000000, 0.000000000000000000 ) ) ;
#16727 = CARTESIAN_POINT ( 'NONE',  ( 63.01563776193091826, 13.70579113808096849, 17.96841034875761878 ) ) ;
#16728 = ORIENTED_EDGE ( 'NONE', *, *, #66713, .F. ) ;
#16729 = CARTESIAN_POINT ( 'NONE',  ( -149.5074843970971301, -170.0000000000000000, 65.06537183036276417 ) ) ;
#16730 = CARTESIAN_POINT ( 'NONE',  ( -55.05276343752910151, 14.68156374112636264, -50.21632399845989170 ) ) ;
#16731 = PLANE ( 'NONE',  #65801 ) ;
#16732 = EDGE_CURVE ( 'NONE', #57123, #20617, #4569, .T. ) ;
#16733 = EDGE_CURVE ( 'NONE', #23556, #19234, #26033, .T. ) ;
#16734 = FACE_OUTER_BOUND ( 'NONE', #46287, .T. ) ;
#16735 = ADVANCED_FACE ( 'NONE', ( #57011 ), #35898, .F. ) ;
#16736 = CARTESIAN_POINT ( 'NONE',  ( 79.92465405224847075, 17.24122384219593584, -13.07911145561778099 ) ) ;
#16737 = CARTESIAN_POINT ( 'NONE',  ( 93.09528872995971938, 21.72934119836187250, -66.33386381959452649 ) ) ;
#16738 = CARTESIAN_POINT ( 'NONE',  ( 197.6316695787931224, 97.13022718399025734, 12.39526483620049291 ) ) ;
#16739 = CARTESIAN_POINT ( 'NONE',  ( -101.3492134984965105, 32.31003911421604613, 18.63133054193531635 ) ) ;
#16740 = DIRECTION ( 'NONE',  ( -1.000000000000000000, 0.000000000000000000, 0.000000000000000000 ) ) ;
#16741 = ORIENTED_EDGE ( 'NONE', *, *, #37471, .T. ) ;
#16742 = ORIENTED_EDGE ( 'NONE', *, *, #24162, .F. ) ;
#16743 = EDGE_CURVE ( 'NONE', #54393, #33166, #63104, .T. ) ;
#16744 = MANIFOLD_SOLID_BREP ( 'Angle iron 35 X 35 X 5(4)', #23850 ) ;
#16745 = CARTESIAN_POINT ( 'NONE',  ( 46.89006465517228861, 9.501960077668739402, 37.90267269328078470 ) ) ;
#16746 = CARTESIAN_POINT ( 'NONE',  ( 15.29899606819416924, 6.485153354884285903, 30.01470767270521733 ) ) ;
#16747 = LINE ( 'NONE', #17443, #12129 ) ;
#16748 = CIRCLE ( 'NONE', #4410, 246.3582898394607241 ) ;
#16749 = DIRECTION ( 'NONE',  ( 0.3090169943749582759, -0.9510565162951499785, 0.000000000000000000 ) ) ;
#16750 = DIRECTION ( 'NONE',  ( 0.000000000000000000, 0.000000000000000000, -1.000000000000000000 ) ) ;
#16751 = DIRECTION ( 'NONE',  ( 0.000000000000000000, 0.000000000000000000, -1.000000000000000000 ) ) ;
#16752 = DIRECTION ( 'NONE',  ( 0.000000000000000000, 0.000000000000000000, -1.000000000000000000 ) ) ;
#16753 = CARTESIAN_POINT ( 'NONE',  ( -121.1841775822198457, 44.65790002524552449, 32.26246926628499523 ) ) ;
#16754 = CARTESIAN_POINT ( 'NONE',  ( 207.8675797643809631, 110.7908513421271692, 70.36262409475189372 ) ) ;
#16755 = ORIENTED_EDGE ( 'NONE', *, *, #1334, .T. ) ;
#16756 = CARTESIAN_POINT ( 'NONE',  ( 4.000000000000012434, 6.928203230275504332, -9.500000000000000000 ) ) ;
#16757 = ORIENTED_EDGE ( 'NONE', *, *, #32356, .T. ) ;
#16758 = CARTESIAN_POINT ( 'NONE',  ( -35.17600017528510392, 10.23461991275926586, 4.364559136216419333 ) ) ;
#16759 = CARTESIAN_POINT ( 'NONE',  ( 93.87111289824404992, 23.09598275302505854, 66.07224964266130485 ) ) ;
#16760 = CARTESIAN_POINT ( 'NONE',  ( 150.0501577908836452, 52.10460126680130344, -15.65376044760501806 ) ) ;
#16761 = DIRECTION ( 'NONE',  ( -0.000000000000000000, 1.000000000000000000, -0.000000000000000000 ) ) ;
#16762 = CARTESIAN_POINT ( 'NONE',  ( -101.3502439362134737, 33.43728945125135965, -76.81582209555509166 ) ) ;
#16763 = CARTESIAN_POINT ( 'NONE',  ( 117.1629420986868695, 33.34326655207112822, -94.18893269630353871 ) ) ;
#16764 = EDGE_CURVE ( 'NONE', #58835, #56347, #61866, .T. ) ;
#16765 = EDGE_CURVE ( 'NONE', #52426, #16361, #42872, .T. ) ;
#16766 = VECTOR ( 'NONE', #53972, 1000.000000000000000 ) ;
#16767 = CARTESIAN_POINT ( 'NONE',  ( 207.0580434617101560, 109.6333291630981250, 83.25781485285460803 ) ) ;
#16768 = CARTESIAN_POINT ( 'NONE',  ( 14.66690460840479027, 20.39656099473415551, 3.061616997868437868E-16 ) ) ;
#16769 = EDGE_LOOP ( 'NONE', ( #50665, #59415, #63120, #56351, #10971, #17725 ) ) ;
#16770 = CARTESIAN_POINT ( 'NONE',  ( 31.11269837220806522, -6.375108774214766072E-14, 0.000000000000000000 ) ) ;
#16771 =( NAMED_UNIT ( * ) SI_UNIT ( $, .STERADIAN. ) SOLID_ANGLE_UNIT ( ) );
#16773 = EDGE_CURVE ( 'NONE', #13106, #63883, #37606, .T. ) ;
#16772 = CARTESIAN_POINT ( 'NONE',  ( -25.80058235236790765, 8.733375263008339218, 15.84155572553979141 ) ) ;
#16774 = CARTESIAN_POINT ( 'NONE',  ( 43.14669449386823885, 9.942681284149134768, -63.44779378956349802 ) ) ;
#16775 = CARTESIAN_POINT ( 'NONE',  ( 283.0516338319616807, -21.63887047452759305, 3.974065166673101057 ) ) ;
#16776 = CARTESIAN_POINT ( 'NONE',  ( -107.0584934212648278, 35.27493744466469394, -63.55753797633620650 ) ) ;
#16777 = CARTESIAN_POINT ( 'NONE',  ( 79.37286005156086333, 18.12402286788021044, 92.82794357717375533 ) ) ;
#16778 = VERTEX_POINT ( 'NONE', #1026 ) ;
#16779 = CARTESIAN_POINT ( 'NONE',  ( 571.0906130828542473, 908.9915846175127854, 550.6483088597192364 ) ) ;
#16780 = AXIS2_PLACEMENT_3D ( 'NONE', #63648, #31294, #58017 ) ;
#16781 = CARTESIAN_POINT ( 'NONE',  ( -36.11269837220809364, -15.55634918610397754, 2.000000000000001776 ) ) ;
#16782 = CARTESIAN_POINT ( 'NONE',  ( -131.2803255164625114, 50.14412978403783683, 16.50002702178883851 ) ) ;
#16783 = CARTESIAN_POINT ( 'NONE',  ( -168.0052514572427071, 83.06849406765624622, -36.72215715079727261 ) ) ;
#16784 = CONTEXT_DEPENDENT_SHAPE_REPRESENTATION ( #46251, #33875 ) ;
#16785 = CARTESIAN_POINT ( 'NONE',  ( 0.000000000000000000, 0.000000000000000000, 41.38025477438755928 ) ) ;
#16786 = ORIENTED_EDGE ( 'NONE', *, *, #55022, .T. ) ;
#16787 = DIRECTION ( 'NONE',  ( -0.000000000000000000, -1.000000000000000000, -0.000000000000000000 ) ) ;
#16788 = CARTESIAN_POINT ( 'NONE',  ( 15.55634918610403261, -3.079134169858832593E-14, 2.000000000000001776 ) ) ;
#16789 = CARTESIAN_POINT ( 'NONE',  ( 200.4574930424075490, 102.3536505870638393, -10.77782775283908379 ) ) ;
#16790 = CARTESIAN_POINT ( 'NONE',  ( -143.4430361498845343, 59.20144672606826219, 87.48578625622529614 ) ) ;
#16791 = CARTESIAN_POINT ( 'NONE',  ( 8.000000000000007105, 249.8719672152120381, -95.00000000000133582 ) ) ;
#16792 = ORIENTED_EDGE ( 'NONE', *, *, #28778, .F. ) ;
#16793 = CARTESIAN_POINT ( 'NONE',  ( 30.12852347772543027, 100.0000000000000000, 73.58025477438755502 ) ) ;
#16794 = CARTESIAN_POINT ( 'NONE',  ( 79.92842440418705507, 18.29578799637232578, 6.962318630869309466 ) ) ;
#16795 = LINE ( 'NONE', #54417, #56618 ) ;
#16796 = VECTOR ( 'NONE', #31636, 1000.000000000000114 ) ;
#16797 = PLANE ( 'NONE',  #66318 ) ;
#16798 = ORIENTED_EDGE ( 'NONE', *, *, #50903, .F. ) ;
#16799 = CARTESIAN_POINT ( 'NONE',  ( 180.2494929075577943, 79.18888319146950039, 71.15314469597512925 ) ) ;
#16800 = ORIENTED_EDGE ( 'NONE', *, *, #5234, .F. ) ;
#16801 = ORIENTED_EDGE ( 'NONE', *, *, #25667, .F. ) ;
#16803 = EDGE_CURVE ( 'NONE', #29332, #45699, #59974, .T. ) ;
#16802 = CARTESIAN_POINT ( 'NONE',  ( -78.18913509716431065, 22.13995206110505265, -8.270900041254195756 ) ) ;
#16804 = CARTESIAN_POINT ( 'NONE',  ( 0.000000000000000000, 0.000000000000000000, 3.469446951953614189E-15 ) ) ;
#16805 = VECTOR ( 'NONE', #68316, 1000.000000000000000 ) ;
#16807 = VERTEX_POINT ( 'NONE', #53772 ) ;
#16806 = CARTESIAN_POINT ( 'NONE',  ( 154.4435090467314637, 56.59612921827834953, 16.93085897233502379 ) ) ;
#16808 = CARTESIAN_POINT ( 'NONE',  ( 159.6725804802005655, 59.38339663535511903, 44.09291707571413355 ) ) ;
#16809 = LINE ( 'NONE', #49156, #47554 ) ;
#16810 = VECTOR ( 'NONE', #52108, 1000.000000000000000 ) ;
#16811 = DIRECTION ( 'NONE',  ( -0.000000000000000000, 1.000000000000000000, -0.000000000000000000 ) ) ;
#16812 = VERTEX_POINT ( 'NONE', #49538 ) ;
#16813 = CARTESIAN_POINT ( 'NONE',  ( -146.7478996615323013, 63.17828545741220836, -89.01584858309800552 ) ) ;
#16814 = EDGE_CURVE ( 'NONE', #30284, #59217, #60099, .T. ) ;
#16815 = CARTESIAN_POINT ( 'NONE',  ( -31.92580063159128301, 9.671320706097189301, -23.47264677473817684 ) ) ;
#16816 = CARTESIAN_POINT ( 'NONE',  ( -179.8989115484066303, 96.59045402602910713, 41.54463800193268241 ) ) ;
#16817 = CARTESIAN_POINT ( 'NONE',  ( 126.6464677212869532, 38.39096133771044350, 61.72361273423263839 ) ) ;
#16818 = EDGE_CURVE ( 'NONE', #54444, #27441, #48481, .T. ) ;
#16819 = EDGE_LOOP ( 'NONE', ( #21639, #37982, #55218, #3453 ) ) ;
#16820 = EDGE_CURVE ( 'NONE', #37239, #33479, #49187, .T. ) ;
#16821 = ORIENTED_EDGE ( 'NONE', *, *, #42918, .F. ) ;
#16822 = ORIENTED_EDGE ( 'NONE', *, *, #45120, .T. ) ;
#16823 = VECTOR ( 'NONE', #42945, 1000.000000000000000 ) ;
#16824 = DIRECTION ( 'NONE',  ( 0.000000000000000000, -1.000000000000000000, 0.000000000000000000 ) ) ;
#16825 = LINE ( 'NONE', #38286, #66869 ) ;
#16826 = CARTESIAN_POINT ( 'NONE',  ( 0.000000000000000000, 0.000000000000000000, 41.38025477438755928 ) ) ;
#16827 = CARTESIAN_POINT ( 'NONE',  ( -38.15923928782687824, 10.79140400702259406, -39.47796947194431993 ) ) ;
#16828 = CARTESIAN_POINT ( 'NONE',  ( -58.33959211650994092, -29.48226216511403308, 3.125053320693560257E-16 ) ) ;
#16829 = DIRECTION ( 'NONE',  ( -1.000000000000000000, 0.000000000000000000, 0.000000000000000000 ) ) ;
#16830 = CARTESIAN_POINT ( 'NONE',  ( -128.1219934350341418, 47.97781708504714970, 72.14052271541459049 ) ) ;
#16831 = CARTESIAN_POINT ( 'NONE',  ( -48.11161266749828513, 13.96357804763626120, 94.42152535799866087 ) ) ;
#16832 = DIRECTION ( 'NONE',  ( -1.000000000000000000, 0.000000000000000000, -0.000000000000000000 ) ) ;
#16835 = ORIENTED_EDGE ( 'NONE', *, *, #37296, .T. ) ;
#16834 = B_SPLINE_CURVE_WITH_KNOTS ( 'NONE', 3,
 ( #67805, #19608, #41068, #62527, #14342, #27292, #10087, #47360, #26613, #5835, #48052, #68817, #52982, #213, #69507, #21327, #5498, #42442, #42775, #43121, #15712, #16401, #53676, #63559, #4470, #57933, #15368, #48730, #64241, #64947, #32582, #37503, #20636, #16052, #47707, #20993, #26951, #10423, #36831, #64594, #63900, #54006, #58269, #42099 ),
 .UNSPECIFIED., .F., .F.,
 ( 4, 2, 2, 2, 2, 2, 2, 2, 2, 2, 2, 2, 2, 2, 2, 2, 2, 2, 2, 2, 2, 4 ),
 ( 0.02495775893651560814, 0.02650251144344294152, 0.02804726395037027489, 0.02959201645729760827, 0.03113676896422493817, 0.03268152147115227502, 0.03345389772461594691, 0.03422627397807962574, 0.03577102648500703197, 0.03654340273847073856, 0.03731577899193443820, 0.03808815524539813785, 0.03886053149886183750, 0.04040528400578929230, 0.04117766025925302664, 0.04195003651271676792, 0.04349478901964425048, 0.04503954152657171917, 0.04581191778003547432, 0.04658429403349922254, 0.04812904654042673980, 0.04967379904735427093 ),
 .UNSPECIFIED. ) ;
#16833 =( BOUNDED_CURVE ( )  B_SPLINE_CURVE ( 3, ( #50094, #28279, #66633, #13162 ),
 .UNSPECIFIED., .F., .F. ) 
 B_SPLINE_CURVE_WITH_KNOTS ( ( 4, 4 ),
 ( 2.394390999492760841E-14, 1.570796326794902997 ),
 .UNSPECIFIED. ) 
 CURVE ( )  GEOMETRIC_REPRESENTATION_ITEM ( )  RATIONAL_B_SPLINE_CURVE ( ( 1.000000000000000000, 0.8047378541243690453, 0.8047378541243690453, 1.000000000000000000 ) ) 
 REPRESENTATION_ITEM ( '' )  );
#16836 = CARTESIAN_POINT ( 'NONE',  ( -98.26894608163135558, 31.90835830144592222, -89.86268561939382948 ) ) ;
#16837 = ORIENTED_EDGE ( 'NONE', *, *, #53571, .F. ) ;
#16838 = PLANE ( 'NONE',  #403 ) ;
#16839 = CARTESIAN_POINT ( 'NONE',  ( 210.4897348480408255, 114.6382060222044430, -75.44159559921389757 ) ) ;
#16840 = PLANE ( 'NONE',  #54513 ) ;
#16841 = CARTESIAN_POINT ( 'NONE',  ( 29.69502258243350923, 57.82046033912877903, 133.5802547743875550 ) ) ;
#16842 = CARTESIAN_POINT ( 'NONE',  ( 0.000000000000000000, 3.000000000000030198, 0.000000000000000000 ) ) ;
#16843 = CARTESIAN_POINT ( 'NONE',  ( 19.10949903373832015, 7.636938177523840743, 30.78566702077129591 ) ) ;
#16844 = CARTESIAN_POINT ( 'NONE',  ( 197.2820712633967730, 96.69730079225780628, 89.25354394473986019 ) ) ;
#16845 = CARTESIAN_POINT ( 'NONE',  ( 183.2136430849847955, 6.000000000000000000, -46.68900338898722424 ) ) ;
#16846 = CARTESIAN_POINT ( 'NONE',  ( 164.6561571795775194, 64.77723933022093661, -68.24917283303342685 ) ) ;
#16847 = ORIENTED_EDGE ( 'NONE', *, *, #54150, .F. ) ;
#16848 = CARTESIAN_POINT ( 'NONE',  ( -15.55634918610408945, -31.11269837220804035, 85.00100000000000477 ) ) ;
#16849 = CYLINDRICAL_SURFACE ( 'NONE', #18414, 7.500000000000013323 ) ;
#16850 = ORIENTED_EDGE ( 'NONE', *, *, #25356, .T. ) ;
#16851 = LINE ( 'NONE', #59752, #54425 ) ;
#16852 =( LENGTH_UNIT ( ) NAMED_UNIT ( * ) SI_UNIT ( .MILLI., .METRE. ) );
#16853 = EDGE_CURVE ( 'NONE', #46836, #60768, #1369, .T. ) ;
#16854 = VERTEX_POINT ( 'NONE', #16841 ) ;
#16855 = CARTESIAN_POINT ( 'NONE',  ( -84.55373779407982227, 24.65190748253136732, 33.24540446502325608 ) ) ;
#16856 = CARTESIAN_POINT ( 'NONE',  ( -28.35957743809534648, 10.12373109553625206, -76.50474426647431869 ) ) ;
#16857 = CARTESIAN_POINT ( 'NONE',  ( 43.14565945994675644, 9.942782559600567893, 30.91037901312404657 ) ) ;
#16858 = CARTESIAN_POINT ( 'NONE',  ( 130.7531879853686121, 39.58149302537889724, -9.835301198007991630 ) ) ;
#16859 = ORIENTED_EDGE ( 'NONE', *, *, #33602, .T. ) ;
#16860 = MANIFOLD_SOLID_BREP ( 'Angle iron 35 X 35 X 5(5)', #59713 ) ;
#16861 = ORIENTED_EDGE ( 'NONE', *, *, #55163, .F. ) ;
#16862 = AXIS2_PLACEMENT_3D ( 'NONE', #34998, #29716, #68052 ) ;
#16863 = PLANE ( 'NONE',  #64930 ) ;
#16864 = VERTEX_POINT ( 'NONE', #7704 ) ;
#16865 = DIRECTION ( 'NONE',  ( 0.000000000000000000, 0.000000000000000000, -1.000000000000000000 ) ) ;
#16866 = FACE_OUTER_BOUND ( 'NONE', #15939, .T. ) ;
#16867 = CARTESIAN_POINT ( 'NONE',  ( 59.95259601283825646, 11.98300577492411456, 57.30717056780049745 ) ) ;
#16868 = CARTESIAN_POINT ( 'NONE',  ( -0.5658006089934847216, 7.533733779014707643, 62.51359026650904127 ) ) ;
#16869 = CARTESIAN_POINT ( 'NONE',  ( -26.87787777325848992, 9.903749977739218835, -90.54880160837116421 ) ) ;
#16870 = FILL_AREA_STYLE ('',( #69571 ) ) ;
#16871 = ORIENTED_EDGE ( 'NONE', *, *, #11540, .F. ) ;
#16872 = CARTESIAN_POINT ( 'NONE',  ( -119.5576859660651508, 42.46117483543970650, -73.27934440310555431 ) ) ;
#16873 = ORIENTED_EDGE ( 'NONE', *, *, #19374, .T. ) ;
#16874 = ORIENTED_EDGE ( 'NONE', *, *, #10389, .F. ) ;
#16875 = DIRECTION ( 'NONE',  ( 0.000000000000000000, 0.000000000000000000, 1.000000000000000000 ) ) ;
#16876 = DIRECTION ( 'NONE',  ( 0.000000000000000000, 0.000000000000000000, 1.000000000000000000 ) ) ;
#16877 = FACE_OUTER_BOUND ( 'NONE', #27609, .T. ) ;
#16878 = LINE ( 'NONE', #53117, #14183 ) ;
#16879 = PLANE ( 'NONE',  #64442 ) ;
#16880 = AXIS2_PLACEMENT_3D ( 'NONE', #67142, #46691, #50938 ) ;
#16881 = VERTEX_POINT ( 'NONE', #38301 ) ;
#16882 = ADVANCED_FACE ( 'NONE', ( #17902 ), #66456, .T. ) ;
#16883 = CARTESIAN_POINT ( 'NONE',  ( 79.22946426532584496, 17.02750615740071183, 9.120237246954173926 ) ) ;
#16884 = EDGE_CURVE ( 'NONE', #46731, #17356, #67154, .T. ) ;
#16885 = LINE ( 'NONE', #65798, #219 ) ;
#16886 = CARTESIAN_POINT ( 'NONE',  ( -78.19460645047367109, 22.14203592077027949, 30.41820113967310490 ) ) ;
#16887 = ORIENTED_EDGE ( 'NONE', *, *, #4436, .T. ) ;
#16888 = EDGE_CURVE ( 'NONE', #17738, #11802, #18945, .T. ) ;
#16889 = CARTESIAN_POINT ( 'NONE',  ( 63.01563776193091826, -170.0000000000000000, 17.96841034875761878 ) ) ;
#16890 = ORIENTED_EDGE ( 'NONE', *, *, #24481, .F. ) ;
#16891 = CARTESIAN_POINT ( 'NONE',  ( 5.354491962338135735, -6.146186931204420389, -0.06809871960543693870 ) ) ;
#16892 = AXIS2_PLACEMENT_3D ( 'NONE', #27233, #43749, #21272 ) ;
#16893 = CARTESIAN_POINT ( 'NONE',  ( 26.99999999999999645, -27.00000000000000355, 15.00000000000000000 ) ) ;
#16894 = CARTESIAN_POINT ( 'NONE',  ( 15.55634918610406103, 15.55634918610400241, 2.000000000000001776 ) ) ;
#16895 = VERTEX_POINT ( 'NONE', #50258 ) ;
#16896 = FACE_OUTER_BOUND ( 'NONE', #57231, .T. ) ;
#16897 = CARTESIAN_POINT ( 'NONE',  ( 0.000000000000000000, 0.000000000000000000, 41.38025477438755928 ) ) ;
#16898 = CARTESIAN_POINT ( 'NONE',  ( 32.09610685027467980, 8.582590950734841684, 35.70073703131771481 ) ) ;
#16899 = CARTESIAN_POINT ( 'NONE',  ( -173.5372686962700755, 89.10569330281724376, -49.71195716475001802 ) ) ;
#16900 = DIRECTION ( 'NONE',  ( -0.000000000000000000, -0.000000000000000000, 1.000000000000000000 ) ) ;
#16901 = DIRECTION ( 'NONE',  ( -0.000000000000000000, -0.000000000000000000, -1.000000000000000000 ) ) ;
#16902 = EDGE_CURVE ( 'NONE', #18178, #27607, #49897, .T. ) ;
#16903 = CARTESIAN_POINT ( 'NONE',  ( 78.57571471437145760, 6.000000000000000000, -20.00000000000000000 ) ) ;
#16904 = ORIENTED_EDGE ( 'NONE', *, *, #31935, .F. ) ;
#16905 = CARTESIAN_POINT ( 'NONE',  ( 141.2361973397653401, 47.26569015399787332, -69.00318946062078851 ) ) ;
#16907 = EDGE_CURVE ( 'NONE', #17378, #28478, #1724, .T. ) ;
#16906 = DIRECTION ( 'NONE',  ( -0.000000000000000000, -0.000000000000000000, -1.000000000000000000 ) ) ;
#16908 = ORIENTED_EDGE ( 'NONE', *, *, #10558, .F. ) ;
#16909 = FACE_BOUND ( 'NONE', #34496, .T. ) ;
#16910 = CARTESIAN_POINT ( 'NONE',  ( -1.728570918131772993, 6.570609986804656799, -74.13742151377635992 ) ) ;
#16911 = PLANE ( 'NONE',  #6591 ) ;
#16912 = CARTESIAN_POINT ( 'NONE',  ( 111.7879975195216815, 29.60186808535944891, -89.73033128225488042 ) ) ;
#16913 = DIRECTION ( 'NONE',  ( 1.000000000000000000, 0.000000000000000000, 0.000000000000000000 ) ) ;
#16914 = CARTESIAN_POINT ( 'NONE',  ( 34.43940527065381474, 66.63700071734669450, 43.58025477438756923 ) ) ;
#16915 = CARTESIAN_POINT ( 'NONE',  ( 200.0000000000000000, 0.000000000000000000, -7.000000000000000000 ) ) ;
#16916 = CARTESIAN_POINT ( 'NONE',  ( -151.2410113808308552, 65.66338888995507261, 4.066252756723934603 ) ) ;
#16917 = CARTESIAN_POINT ( 'NONE',  ( -73.26882986836166367, 20.33842609887990704, -91.07877570767612951 ) ) ;
#16918 = CARTESIAN_POINT ( 'NONE',  ( -10.24974837193994404, 8.069704751038626611, 44.72969724616100251 ) ) ;
#16919 = CARTESIAN_POINT ( 'NONE',  ( 111.8699272271189216, 29.64190505307780654, 2.941473855310829943 ) ) ;
#16920 = CARTESIAN_POINT ( 'NONE',  ( 93.08174259058942823, 22.79847752828720786, -12.62219101434053847 ) ) ;
#16921 = EDGE_LOOP ( 'NONE', ( #7121, #28218 ) ) ;
#16922 = CARTESIAN_POINT ( 'NONE',  ( 0.000000000000000000, 0.000000000000000000, 380.0000000000000000 ) ) ;
#16923 = ORIENTED_EDGE ( 'NONE', *, *, #29596, .T. ) ;
#16924 = CARTESIAN_POINT ( 'NONE',  ( -417.6627218934913230, 399.9999999999997726, 113.5502958579881891 ) ) ;
#16925 = CARTESIAN_POINT ( 'NONE',  ( 81.05403189674299824, 18.64820877954959499, -75.20638625924833320 ) ) ;
#16926 = CARTESIAN_POINT ( 'NONE',  ( 102.7974068605285396, 26.68003355195580539, 91.76817536871718062 ) ) ;
#16927 = CARTESIAN_POINT ( 'NONE',  ( 39.40195752203892710, -170.0000000000000000, 71.75838489642698903 ) ) ;
#16928 = DIRECTION ( 'NONE',  ( 0.1342332658176667304, -0.9909497617679331460, 0.000000000000000000 ) ) ;
#16929 = AXIS2_PLACEMENT_3D ( 'NONE', #24746, #55704, #56055 ) ;
#16930 = CARTESIAN_POINT ( 'NONE',  ( -27.70185240367226598, 10.02491413133430953, -49.32437352143211484 ) ) ;
#16931 = CARTESIAN_POINT ( 'NONE',  ( -47.80251179448169552, 13.89045662648309687, -67.57686690419204467 ) ) ;
#16932 = CARTESIAN_POINT ( 'NONE',  ( -76.99081612991844281, 22.76418914851637254, -88.98189906751177602 ) ) ;
#16933 = CARTESIAN_POINT ( 'NONE',  ( -3.120068547127581748, 41.61225688647869703, 13.79046412284830048 ) ) ;
#16934 = EDGE_LOOP ( 'NONE', ( #44814, #6395, #30494, #3017 ) ) ;
#16935 = ORIENTED_EDGE ( 'NONE', *, *, #48989, .F. ) ;
#16936 = CARTESIAN_POINT ( 'NONE',  ( 31.90170717962883273, 8.563261373066632487, 64.49853757514532049 ) ) ;
#16937 = CARTESIAN_POINT ( 'NONE',  ( 175.8855729601531550, 73.50624012737691260, 58.22573703953762703 ) ) ;
#16938 = VECTOR ( 'NONE', #27193, 1000.000000000000000 ) ;
#16939 = CARTESIAN_POINT ( 'NONE',  ( -165.7140086129056442, 80.68381997492571145, -16.58285276488415150 ) ) ;
#16940 = AXIS2_PLACEMENT_3D ( 'NONE', #60644, #12459, #12117 ) ;
#16941 = CYLINDRICAL_SURFACE ( 'NONE', #311, 7.500000000000027534 ) ;
#16942 = VERTEX_POINT ( 'NONE', #23186 ) ;
#16943 = CARTESIAN_POINT ( 'NONE',  ( 87.10672734544989737, 20.64813880796635104, 2.867536982015616687 ) ) ;
#16944 = CARTESIAN_POINT ( 'NONE',  ( 188.0103583326377361, 87.39896620268120842, -13.98969534752448496 ) ) ;
#16945 = CARTESIAN_POINT ( 'NONE',  ( -80.54757501605355685, 23.04700348514568020, -8.506729827231833241 ) ) ;
#16946 = CARTESIAN_POINT ( 'NONE',  ( -79.09055197094342304, 23.56106361828856777, -88.80455181264522935 ) ) ;
#16947 = CARTESIAN_POINT ( 'NONE',  ( 45.90693067088658808, 9.344800815249305614, -12.51017037632520790 ) ) ;
#16948 = CARTESIAN_POINT ( 'NONE',  ( 211.3917124729449881, 115.9987099435923028, -13.58743899467040528 ) ) ;
#16949 = FACE_BOUND ( 'NONE', #37163, .T. ) ;
#16950 = CARTESIAN_POINT ( 'NONE',  ( -59.94781924509481286, 16.04872117907065743, -37.02872815368100845 ) ) ;
#16951 = ORIENTED_EDGE ( 'NONE', *, *, #55915, .T. ) ;
#16952 = DIRECTION ( 'NONE',  ( 0.000000000000000000, 1.000000000000000000, -0.000000000000000000 ) ) ;
#16953 = CARTESIAN_POINT ( 'NONE',  ( 94.06699947028484132, 23.17027898120150198, -44.31905308565868040 ) ) ;
#16954 = CARTESIAN_POINT ( 'NONE',  ( 311.8713128290285113, 190.0000000000000000, 346.5826552340383842 ) ) ;
#16955 = CARTESIAN_POINT ( 'NONE',  ( -15.55634918610396866, 31.11269837220809009, 2.000000000000001776 ) ) ;
#16956 = CARTESIAN_POINT ( 'NONE',  ( 151.7956716830626647, 53.36999433148312733, 14.97506466355020471 ) ) ;
#16957 = CARTESIAN_POINT ( 'NONE',  ( 19.00668540189185407, 62.54164772954719353, 3.125053320693570118E-16 ) ) ;
#16958 = VERTEX_POINT ( 'NONE', #18596 ) ;
#16959 = CARTESIAN_POINT ( 'NONE',  ( 56.53776994993147298, 11.26292242501185115, 14.25638008219111619 ) ) ;
#16960 = CARTESIAN_POINT ( 'NONE',  ( -60.66241560458681903, 16.25736033771447708, 59.65924898650886377 ) ) ;
#16961 = ADVANCED_FACE ( 'NONE', ( #23533 ), #40052, .F. ) ;
#16962 = ORIENTED_EDGE ( 'NONE', *, *, #25375, .F. ) ;
#16963 = ORIENTED_EDGE ( 'NONE', *, *, #40963, .T. ) ;
#16964 = CARTESIAN_POINT ( 'NONE',  ( -79.61931371420119774, 22.68640080971621487, -62.00571751209825777 ) ) ;
#16965 = CARTESIAN_POINT ( 'NONE',  ( 433.3728120124415568, 388.0000000000110276, 99.58582976391704733 ) ) ;
#16966 = EDGE_CURVE ( 'NONE', #27319, #8997, #51411, .T. ) ;
#16967 = CARTESIAN_POINT ( 'NONE',  ( 105.4375968828853161, 26.72149058755205431, 42.87463743524401139 ) ) ;
#16968 = ORIENTED_EDGE ( 'NONE', *, *, #24320, .T. ) ;
#16969 = EDGE_CURVE ( 'NONE', #31046, #54939, #60461, .T. ) ;
#16970 = AXIS2_PLACEMENT_3D ( 'NONE', #49920, #65779, #33763 ) ;
#16971 = EDGE_LOOP ( 'NONE', ( #34913, #19927, #24153, #42529 ) ) ;
#16972 = CARTESIAN_POINT ( 'NONE',  ( 86.62931800182293784, -170.0000000000000000, 2.867536982015617575 ) ) ;
#16973 = PLANE ( 'NONE',  #58291 ) ;
#16974 = CARTESIAN_POINT ( 'NONE',  ( 106.0228389049370321, 28.07756796303169722, 4.061978269566077770 ) ) ;
#16975 = CARTESIAN_POINT ( 'NONE',  ( 63.49941241090384381, 13.81848793187418600, 2.968410348757589912 ) ) ;
#16976 = FACE_OUTER_BOUND ( 'NONE', #38309, .T. ) ;
#16977 = CIRCLE ( 'NONE', #41701, 8.000000000000000000 ) ;
#16978 = AXIS2_PLACEMENT_3D ( 'NONE', #38721, #60167, #11986 ) ;
#16979 = AXIS2_PLACEMENT_3D ( 'NONE', #15572, #54572, #420 ) ;
#16980 = CARTESIAN_POINT ( 'NONE',  ( -55.05276343752909440, 15.72344139423349141, -35.21632399845986328 ) ) ;
#16981 = DIRECTION ( 'NONE',  ( -1.000000000000000000, 0.000000000000000000, 2.775557561562891844E-16 ) ) ;
#16983 = ADVANCED_FACE ( 'NONE', ( #29841 ), #39356, .F. ) ;
#16982 = CARTESIAN_POINT ( 'NONE',  ( 15.29305096970403710, 7.491604910111013815, 45.01470767270526352 ) ) ;
#16984 = FACE_OUTER_BOUND ( 'NONE', #6561, .T. ) ;
#16985 = LINE ( 'NONE', #49686, #46669 ) ;
#16987 = VERTEX_POINT ( 'NONE', #17548 ) ;
#16986 = DIRECTION ( 'NONE',  ( -1.000000000000000000, -0.000000000000000000, -0.000000000000000000 ) ) ;
#16988 = VERTEX_POINT ( 'NONE', #55173 ) ;
#16989 = MECHANICAL_DESIGN_GEOMETRIC_PRESENTATION_REPRESENTATION (  '', ( #12545 ), #31618 ) ;
#16990 = ORIENTED_EDGE ( 'NONE', *, *, #25293, .F. ) ;
#16991 = CARTESIAN_POINT ( 'NONE',  ( -12.39413342787891104, 7.231444436041488011, -10.10556315530504889 ) ) ;
#16992 = CARTESIAN_POINT ( 'NONE',  ( -165.6292614779507346, 80.59684587977122305, 92.52285916119727460 ) ) ;
#16993 = CARTESIAN_POINT ( 'NONE',  ( 412.3372781065085633, 179.4906275429376024, -146.4497041420117682 ) ) ;
#16994 = PLANE ( 'NONE',  #43317 ) ;
#16995 = CARTESIAN_POINT ( 'NONE',  ( -62.41727061481083183, 17.83188723492277461, -41.23329363980502649 ) ) ;
#16996 = CARTESIAN_POINT ( 'NONE',  ( -7.825402957745081878, 7.899365992529268965, -23.57352014148015584 ) ) ;
#16997 = CARTESIAN_POINT ( 'NONE',  ( -74.40004226286976063, 20.74218500375955898, -75.63308164639384756 ) ) ;
#16998 = CARTESIAN_POINT ( 'NONE',  ( 23.09784929786602703, 6.844738137842332648, -14.47737765197590853 ) ) ;
#16999 = ORIENTED_EDGE ( 'NONE', *, *, #5622, .T. ) ;
#17000 = DIRECTION ( 'NONE',  ( -0.04486483035050446017, -0.9989930665413151445, 0.000000000000000000 ) ) ;
#17001 = ORIENTED_EDGE ( 'NONE', *, *, #56949, .F. ) ;
#17002 = ORIENTED_EDGE ( 'NONE', *, *, #3642, .F. ) ;
#17003 = CARTESIAN_POINT ( 'NONE',  ( -144.9412191745148846, 61.69548892475975066, 17.34567004948121749 ) ) ;
#17004 = SURFACE_SIDE_STYLE ('',( #1190 ) ) ;
#17005 = CARTESIAN_POINT ( 'NONE',  ( 63.01563776193091826, -170.0000000000000000, 91.00206212014866480 ) ) ;
#17006 = DIRECTION ( 'NONE',  ( 0.3090169943749582759, -0.9510565162951499785, 0.000000000000000000 ) ) ;
#17007 = CARTESIAN_POINT ( 'NONE',  ( -104.1244073710070097, 33.72720758483609416, 18.45900469992847093 ) ) ;
#17008 = DIRECTION ( 'NONE',  ( 0.000000000000000000, 1.000000000000000000, -0.000000000000000000 ) ) ;
#17009 = CARTESIAN_POINT ( 'NONE',  ( 134.7708899521911121, 43.15864772107689618, -24.12637467660490387 ) ) ;
#17010 = EDGE_LOOP ( 'NONE', ( #23143, #4788, #41545, #54607 ) ) ;
#17011 = ORIENTED_EDGE ( 'NONE', *, *, #32636, .F. ) ;
#17012 = EDGE_LOOP ( 'NONE', ( #19883, #40202 ) ) ;
#17013 = CARTESIAN_POINT ( 'NONE',  ( -8.000000000000001776, 0.000000000000000000, 0.000000000000000000 ) ) ;
#17014 = CARTESIAN_POINT ( 'NONE',  ( -149.5074843970971017, 65.50121172469319220, -7.968279941028269420 ) ) ;
#17015 = CARTESIAN_POINT ( 'NONE',  ( 55.51597771111714508, 11.05737652677078664, -15.87642975587560912 ) ) ;
#17016 = AXIS2_PLACEMENT_3D ( 'NONE', #1854, #44753, #34562 ) ;
#17017 = CARTESIAN_POINT ( 'NONE',  ( -38.16002576456689610, 10.79155573432543491, 61.22331852717874767 ) ) ;
#17018 = CARTESIAN_POINT ( 'NONE',  ( -24.39249304643438521, 60.24953346690454481, 170.0000000000000000 ) ) ;
#17019 = ORIENTED_EDGE ( 'NONE', *, *, #29254, .T. ) ;
#17020 = DIRECTION ( 'NONE',  ( 1.387778780781446169E-16, -1.000000000000000000, -3.469446951953615421E-17 ) ) ;
#17021 = DIRECTION ( 'NONE',  ( -0.000000000000000000, -1.000000000000000000, -0.000000000000000000 ) ) ;
#17022 = SHAPE_REPRESENTATION_RELATIONSHIP ( 'NONE' , 'NONE' ,  #5548, #33268 ) ;
#17023 = EDGE_CURVE ( 'NONE', #44947, #9547, #6996, .T. ) ;
#17024 = CARTESIAN_POINT ( 'NONE',  ( -0.3252226420479328861, 7.525368746738510417, -43.40480950733539345 ) ) ;
#17025 = CARTESIAN_POINT ( 'NONE',  ( -14.35185884954381308, 8.414771159230838293, 94.99999999999866418 ) ) ;
#17026 = CARTESIAN_POINT ( 'NONE',  ( -125.8938041572051389, 46.49392987655491538, 18.77539728269342945 ) ) ;
#17027 = CARTESIAN_POINT ( 'NONE',  ( -443.8104064242511413, 394.8690347851185152, -131.3748745853282287 ) ) ;
#17028 = CARTESIAN_POINT ( 'NONE',  ( 23.28869764673362042, 6.856674305776600420, 64.84761802070974568 ) ) ;
#17029 = CARTESIAN_POINT ( 'NONE',  ( 0.000000000000000000, 0.000000000000000000, 41.38025477438755928 ) ) ;
#17030 = CARTESIAN_POINT ( 'NONE',  ( 9.290502160020464473, 6.379616279862540651, -73.61710939586298252 ) ) ;
#17031 = VECTOR ( 'NONE', #5416, 999.9999999999998863 ) ;
#17032 = MECHANICAL_DESIGN_GEOMETRIC_PRESENTATION_REPRESENTATION (  '', ( #67622 ), #27126 ) ;
#17033 = EDGE_LOOP ( 'NONE', ( #11052, #18161, #35926, #18037, #24687, #38998, #33546 ) ) ;
#17034 = DIRECTION ( 'NONE',  ( 1.000000000000000000, 0.000000000000000000, 0.000000000000000000 ) ) ;
#17035 = CIRCLE ( 'NONE', #56369, 243.4957430088094839 ) ;
#17036 = FACE_OUTER_BOUND ( 'NONE', #55740, .T. ) ;
#17037 = CYLINDRICAL_SURFACE ( 'NONE', #1730, 89.99999999999998579 ) ;
#17038 = CARTESIAN_POINT ( 'NONE',  ( 46.50207827473963107, 9.439498081273468344, -72.39330090572757115 ) ) ;
#17039 = CARTESIAN_POINT ( 'NONE',  ( 60.40531521312254171, 13.11276739283243309, -77.10049446495987979 ) ) ;
#17040 = VERTEX_POINT ( 'NONE', #28449 ) ;
#17041 = ORIENTED_EDGE ( 'NONE', *, *, #39582, .T. ) ;
#17042 = CARTESIAN_POINT ( 'NONE',  ( 437.3372781065085633, 400.0000000000000568, -141.4497041420118251 ) ) ;
#17043 = PLANE ( 'NONE',  #54015 ) ;
#17044 = ADVANCED_FACE ( 'NONE', ( #60799 ), #66112, .F. ) ;
#17045 = ORIENTED_EDGE ( 'NONE', *, *, #61298, .T. ) ;
#17046 = ORIENTED_EDGE ( 'NONE', *, *, #62766, .T. ) ;
#17047 = LINE ( 'NONE', #60325, #19563 ) ;
#17048 = CARTESIAN_POINT ( 'NONE',  ( 0.000000000000000000, 0.000000000000000000, 0.000000000000000000 ) ) ;
#17049 = VERTEX_POINT ( 'NONE', #4492 ) ;
#17050 = CARTESIAN_POINT ( 'NONE',  ( 47.99999999999997158, -19.99999999999997868, 0.000000000000000000 ) ) ;
#17051 = CARTESIAN_POINT ( 'NONE',  ( 140.4769819293526893, 46.76840769395179365, 60.32113923860118376 ) ) ;
#17052 = CARTESIAN_POINT ( 'NONE',  ( -78.66644367742111399, 22.32174330031317311, -35.11545063171788428 ) ) ;
#17053 = EDGE_CURVE ( 'NONE', #15739, #2593, #267, .T. ) ;
#17054 = DIRECTION ( 'NONE',  ( -1.000000000000000000, 0.000000000000000000, 0.000000000000000000 ) ) ;
#17055 = CARTESIAN_POINT ( 'NONE',  ( 16.63342912721455491, 6.527857407601582729, -89.20804527961315955 ) ) ;
#17056 = CARTESIAN_POINT ( 'NONE',  ( -189.4248691432192686, 107.3461292335514798, 36.68996308917169813 ) ) ;
#17057 = ORIENTED_EDGE ( 'NONE', *, *, #46761, .F. ) ;
#17058 = CARTESIAN_POINT ( 'NONE',  ( 112.7784411285249035, 30.07270878825232430, -50.48479703671700491 ) ) ;
#17059 = DIRECTION ( 'NONE',  ( 0.000000000000000000, -2.500042656554809847E-16, 1.000000000000000000 ) ) ;
#17060 = EDGE_CURVE ( 'NONE', #43922, #58687, #3457, .T. ) ;
#17061 = CARTESIAN_POINT ( 'NONE',  ( 39.40195752203892710, 8.409560354027394879, -50.61981746542779348 ) ) ;
#17062 = PLANE ( 'NONE',  #64592 ) ;
#17064 = ORIENTED_EDGE ( 'NONE', *, *, #23131, .F. ) ;
#17063 = CARTESIAN_POINT ( 'NONE',  ( -129.7656201304987746, 49.09621953108914028, 85.37891732438063741 ) ) ;
#17065 = CARTESIAN_POINT ( 'NONE',  ( -450.6627218934913230, 217.8591479523843475, -111.4497041420117966 ) ) ;
#17066 = VECTOR ( 'NONE', #7659, 1000.000000000000114 ) ;
#17067 = ADVANCED_FACE ( 'NONE', ( #52332 ), #62894, .F. ) ;
#17068 = EDGE_CURVE ( 'NONE', #12427, #10027, #41783, .T. ) ;
#17069 = EDGE_LOOP ( 'NONE', ( #68928, #22191, #44318, #37748 ) ) ;
#17070 = CIRCLE ( 'NONE', #24942, 242.4895526022646379 ) ;
#17071 = DIRECTION ( 'NONE',  ( 0.000000000000000000, 0.000000000000000000, -1.000000000000000000 ) ) ;
#17072 = CARTESIAN_POINT ( 'NONE',  ( 21.27121078971695312, -61.42097029141944375, 170.0000000000000000 ) ) ;
#17073 = DIRECTION ( 'NONE',  ( -0.000000000000000000, 0.000000000000000000, -1.000000000000000000 ) ) ;
#17074 = DIRECTION ( 'NONE',  ( 0.000000000000000000, 0.000000000000000000, 1.000000000000000000 ) ) ;
#17075 = AXIS2_PLACEMENT_3D ( 'NONE', #18933, #8384, #12971 ) ;
#17076 = CARTESIAN_POINT ( 'NONE',  ( 79.14242532928582818, 17.00090225993928428, -15.96730280997515194 ) ) ;
#17077 = CARTESIAN_POINT ( 'NONE',  ( 65.35403040894466642, 1.250000000000021982, 43.58025477438756212 ) ) ;
#17078 = CARTESIAN_POINT ( 'NONE',  ( 93.08533330311585985, 21.72562315962721868, -74.01562841799706405 ) ) ;
#17079 = LINE ( 'NONE', #49787, #13455 ) ;
#17080 = CARTESIAN_POINT ( 'NONE',  ( 25.00000000000000000, 65.13282190615278466, 5.000000000000000000 ) ) ;
#17081 = ORIENTED_EDGE ( 'NONE', *, *, #67499, .F. ) ;
#17082 = ORIENTED_EDGE ( 'NONE', *, *, #21130, .T. ) ;
#17083 = CARTESIAN_POINT ( 'NONE',  ( 15.55634918610400241, -10.55634918610406281, 2.000000000000001776 ) ) ;
#17084 = CIRCLE ( 'NONE', #4744, 4.999999999999997335 ) ;
#17085 = CYLINDRICAL_SURFACE ( 'NONE', #54215, 7.500000000000020428 ) ;
#17086 = PLANE ( 'NONE',  #52536 ) ;
#17087 = FACE_OUTER_BOUND ( 'NONE', #28040, .T. ) ;
#17088 = DIRECTION ( 'NONE',  ( -1.000000000000000000, 0.000000000000000000, 0.000000000000000000 ) ) ;
#17089 = CARTESIAN_POINT ( 'NONE',  ( -71.22896441287285541, 20.69091426169410397, -70.45909810321082034 ) ) ;
#17090 = LINE ( 'NONE', #10781, #28050 ) ;
#17091 = CARTESIAN_POINT ( 'NONE',  ( 45.76553115525425852, 10.34124506813254918, -47.09660741898280634 ) ) ;
#17092 = CARTESIAN_POINT ( 'NONE',  ( 160.4963793545268800, 60.04225845346907420, -77.34568484721802406 ) ) ;
#17093 = EDGE_LOOP ( 'NONE', ( #27174, #12989, #52996, #35907 ) ) ;
#17094 = CARTESIAN_POINT ( 'NONE',  ( 0.000000000000000000, 0.000000000000000000, 41.41421356237313489 ) ) ;
#17095 = EDGE_LOOP ( 'NONE', ( #52386, #18112, #28006, #32395 ) ) ;
#17096 = CARTESIAN_POINT ( 'NONE',  ( 409.0783954480987745, 190.0000000000000000, 174.7010307253933092 ) ) ;
#17097 = DIRECTION ( 'NONE',  ( -0.000000000000000000, -1.000000000000000000, 0.000000000000000000 ) ) ;
#17098 = CARTESIAN_POINT ( 'NONE',  ( 93.32756701508621688, 22.89083686918420213, 67.46732691414862870 ) ) ;
#17099 = CARTESIAN_POINT ( 'NONE',  ( -19.46539569203812903, -15.68752276659308365, 0.000000000000000000 ) ) ;
#17100 = CARTESIAN_POINT ( 'NONE',  ( 329.1355598199467636, 2.000000000000001776, -129.5087625010780812 ) ) ;
#17101 = CARTESIAN_POINT ( 'NONE',  ( 31.11269837220809364, 20.55634918610396866, 2.000000000000001776 ) ) ;
#17102 = CARTESIAN_POINT ( 'NONE',  ( 1.667562369267789890, -64.99262834925670518, 170.0000000000000000 ) ) ;
#17103 = DIRECTION ( 'NONE',  ( -0.8660254037844362651, 0.000000000000000000, -0.5000000000000038858 ) ) ;
#17104 = CARTESIAN_POINT ( 'NONE',  ( -7.825402957745085430, 7.899365992529246761, 18.27103044898354511 ) ) ;
#17105 = CARTESIAN_POINT ( 'NONE',  ( 64.08056813503714011, -12.89932471814424630, 41.38025477438755928 ) ) ;
#17107 = ORIENTED_EDGE ( 'NONE', *, *, #20071, .F. ) ;
#17106 = ADVANCED_FACE ( 'NONE', ( #30536 ), #63581, .T. ) ;
#17108 = CARTESIAN_POINT ( 'NONE',  ( 59.08202327466402437, 12.82375733818954089, 70.54788376517701920 ) ) ;
#17109 = CARTESIAN_POINT ( 'NONE',  ( 10.82760985890678640, 7.398654328676807168, -64.21712473681512279 ) ) ;
#17110 = DIRECTION ( 'NONE',  ( 0.9268618657695262275, 0.3754025596372950191, 0.000000000000000000 ) ) ;
#17111 = LINE ( 'NONE', #60029, #37916 ) ;
#17112 = CARTESIAN_POINT ( 'NONE',  ( -0.7215816834507543520, 6.532459459468098473, 35.19760772530012360 ) ) ;
#17113 = CARTESIAN_POINT ( 'NONE',  ( 83.19706090114061681, 19.33633638213343531, 84.22436956647520390 ) ) ;
#17114 = EDGE_CURVE ( 'NONE', #12845, #19095, #20318, .T. ) ;
#17115 = ORIENTED_EDGE ( 'NONE', *, *, #13200, .F. ) ;
#17116 = VECTOR ( 'NONE', #61963, 1000.000000000000000 ) ;
#17117 = DIRECTION ( 'NONE',  ( -9.394183029811381172E-15, 4.252793660009627612E-15, -1.000000000000000000 ) ) ;
#17118 = DIRECTION ( 'NONE',  ( -0.000000000000000000, -1.000000000000000000, -0.000000000000000000 ) ) ;
#17119 = CARTESIAN_POINT ( 'NONE',  ( -129.3963145237381127, 48.84337839101545597, 17.91139487216891624 ) ) ;
#17120 = CARTESIAN_POINT ( 'NONE',  ( -167.4860113959265391, 82.52233889531184730, -37.25610511775715850 ) ) ;
#17121 = ITEM_DEFINED_TRANSFORMATION ( 'NONE', 'NONE', #26529,  #66832 ) ;
#17122 = CARTESIAN_POINT ( 'NONE',  ( -133.0835080491125098, 52.64966140620843049, -44.56526587904586734 ) ) ;
#17123 = VERTEX_POINT ( 'NONE', #10111 ) ;
#17124 = CARTESIAN_POINT ( 'NONE',  ( 45.82394788922869822, -46.11928342727429708, 170.0000000000000000 ) ) ;
#17125 = AXIS2_PLACEMENT_3D ( 'NONE', #54806, #50934, #23164 ) ;
#17126 = CARTESIAN_POINT ( 'NONE',  ( -33.37998527947969052, -1.749200578933713279, 6.893343212288926658 ) ) ;
#17127 = EDGE_CURVE ( 'NONE', #25708, #50267, #25270, .T. ) ;
#17128 = CARTESIAN_POINT ( 'NONE',  ( -147.7860806339125475, 62.73248524776227697, -22.78099747642112760 ) ) ;
#17129 = LINE ( 'NONE', #976, #57530 ) ;
#17130 = EDGE_CURVE ( 'NONE', #19443, #13106, #47384, .T. ) ;
#17131 = CARTESIAN_POINT ( 'NONE',  ( 0.000000000000000000, 0.000000000000000000, 0.000000000000000000 ) ) ;
#17132 = EDGE_CURVE ( 'NONE', #68787, #51614, #36159, .T. ) ;
#17133 = ORIENTED_EDGE ( 'NONE', *, *, #4240, .T. ) ;
#17134 = DIRECTION ( 'NONE',  ( -0.000000000000000000, 1.000000000000000000, -0.000000000000000000 ) ) ;
#17135 = LINE ( 'NONE', #1671, #17066 ) ;
#17136 = CARTESIAN_POINT ( 'NONE',  ( -99.98584758882479662, 32.75338129098886242, 30.86302090401612119 ) ) ;
#17137 = EDGE_CURVE ( 'NONE', #14098, #12427, #41711, .T. ) ;
#17138 = DIRECTION ( 'NONE',  ( 0.6246950475544236214, 0.000000000000000000, 0.7808688094430308313 ) ) ;
#17140 = ORIENTED_EDGE ( 'NONE', *, *, #46793, .T. ) ;
#17139 = DIRECTION ( 'NONE',  ( -0.000000000000000000, 1.000000000000000000, -0.000000000000000000 ) ) ;
#17141 = PLANE ( 'NONE',  #40700 ) ;
#17142 = ORIENTED_EDGE ( 'NONE', *, *, #29637, .F. ) ;
#17143 = ORIENTED_EDGE ( 'NONE', *, *, #49882, .F. ) ;
#17144 = CARTESIAN_POINT ( 'NONE',  ( -118.4753258120605324, 41.79945864152914936, -95.00000000000133582 ) ) ;
#17145 = CARTESIAN_POINT ( 'NONE',  ( 8.000000000000007105, 249.8719672152120381, -95.00000000000133582 ) ) ;
#17147 = ORIENTED_EDGE ( 'NONE', *, *, #54778, .F. ) ;
#17146 = CARTESIAN_POINT ( 'NONE',  ( -14.84903512415885629, 8.461292896365065985, -67.12079146646519234 ) ) ;
#17148 = CARTESIAN_POINT ( 'NONE',  ( 164.8471526211110927, 63.62172173173269130, 38.29138183902061598 ) ) ;
#17149 = LINE ( 'NONE', #43191, #57535 ) ;
#17150 = EDGE_CURVE ( 'NONE', #61608, #62240, #54025, .T. ) ;
#17151 = ADVANCED_FACE ( 'NONE', ( #46707 ), #19279, .F. ) ;
#17152 = CARTESIAN_POINT ( 'NONE',  ( -75.43271753227892873, 22.18711452892410918, -35.83126050068450041 ) ) ;
#17153 = EDGE_CURVE ( 'NONE', #35973, #65355, #25953, .T. ) ;
#17154 = ORIENTED_EDGE ( 'NONE', *, *, #30555, .F. ) ;
#17155 = EDGE_CURVE ( 'NONE', #16, #38237, #57955, .T. ) ;
#17156 = CARTESIAN_POINT ( 'NONE',  ( 174.3243312526346642, 73.41378903026858893, -94.13505484421320091 ) ) ;
#17157 = CARTESIAN_POINT ( 'NONE',  ( -38.93878980550033475, 10.94326053663841769, -15.47548683381646129 ) ) ;
#17159 = CARTESIAN_POINT ( 'NONE',  ( 125.0000000000000000, 1.530808498934191561E-14, -5.000000000000000000 ) ) ;
#17158 = VECTOR ( 'NONE', #66814, 1000.000000000000114 ) ;
#17160 = CARTESIAN_POINT ( 'NONE',  ( -34.74312654625182972, 10.15703162223799971, -76.39920896306614395 ) ) ;
#17161 = CARTESIAN_POINT ( 'NONE',  ( 19.54452863209719382, 7.657034792877148277, 70.86930329570787990 ) ) ;
#17162 = B_SPLINE_CURVE_WITH_KNOTS ( 'NONE', 3,
 ( #8296, #55426, #23777, #7252, #29063, #18153, #13911, #51208, #39952, #56834, #34344, #24819, #29743, #3020, #45923, #67391, #2328, #35026, #61405, #46256, #55787, #45224, #34691, #67735, #19534, #40993, #67053, #56473, #63140, #62451, #14265, #31473, #9680, #10022, #25861, #47289, #31816, #15299, #36754, #10350, #52908, #53248, #4058, #26542 ),
 .UNSPECIFIED., .F., .F.,
 ( 4, 2, 2, 2, 2, 2, 2, 2, 2, 2, 2, 2, 2, 2, 2, 2, 2, 2, 2, 2, 2, 4 ),
 ( 0.02638217555535139758, 0.02805347641364859188, 0.02972477727194578964, 0.03139607813024298394, 0.03306737898854018171, 0.03390302941768880141, 0.03473867984683742804, 0.03640998070513465357, 0.03724563113428327327, 0.03808128156343189297, 0.03891693199258051267, 0.03975258242172913237, 0.04058823285087774513, 0.04142388328002636483, 0.04225953370917498453, 0.04309518413832360423, 0.04476648499662086444, 0.04643778585491813160, 0.04810908671321538488, 0.04978038757151265203, 0.05145168842980990531, 0.05312298928810717247 ),
 .UNSPECIFIED. ) ;
#17163 = ORIENTED_EDGE ( 'NONE', *, *, #43245, .F. ) ;
#17164 = EDGE_LOOP ( 'NONE', ( #5083, #6954, #53341, #53385 ) ) ;
#17165 = ORIENTED_EDGE ( 'NONE', *, *, #45838, .F. ) ;
#17166 = COLOUR_RGB ( '',0.7921568627450980005, 0.8196078431372548767, 0.9333333333333333481 ) ;
#17167 = DIRECTION ( 'NONE',  ( 0.000000000000000000, 0.000000000000000000, -1.000000000000000000 ) ) ;
#17168 = CARTESIAN_POINT ( 'NONE',  ( -102.2801239173131052, 33.91021738430207222, 3.674523915951417585 ) ) ;
#17169 = DIRECTION ( 'NONE',  ( -0.000000000000000000, -0.000000000000000000, -1.000000000000000000 ) ) ;
#17170 = VECTOR ( 'NONE', #5162, 1000.000000000000114 ) ;
#17171 = CARTESIAN_POINT ( 'NONE',  ( -38.55214349681827457, 10.86754840574842262, -45.24580720952189239 ) ) ;
#17172 = CARTESIAN_POINT ( 'NONE',  ( -104.6581597602948221, 34.00455924016704046, 84.57040083051070667 ) ) ;
#17173 = DIRECTION ( 'NONE',  ( 0.000000000000000000, 0.000000000000000000, -1.000000000000000000 ) ) ;
#17174 = CARTESIAN_POINT ( 'NONE',  ( -129.6001310305488516, 48.98284622040321068, 71.48886441875946218 ) ) ;
#17175 = CARTESIAN_POINT ( 'NONE',  ( 14.99999999999997158, 0.000000000000000000, 0.000000000000000000 ) ) ;
#17177 = CARTESIAN_POINT ( 'NONE',  ( 79.52861599156695149, 17.11914630560287875, 61.59085265089968431 ) ) ;
#17176 = AXIS2_PLACEMENT_3D ( 'NONE', #3994, #68363, #63773 ) ;
#17178 = ORIENTED_EDGE ( 'NONE', *, *, #62319, .T. ) ;
#17179 = DIRECTION ( 'NONE',  ( -0.5508969814521065267, 0.8345732537212999791, 0.000000000000000000 ) ) ;
#17180 = AXIS2_PLACEMENT_3D ( 'NONE', #57037, #56332, #46463 ) ;
#17181 = ORIENTED_EDGE ( 'NONE', *, *, #57602, .F. ) ;
#17182 = CARTESIAN_POINT ( 'NONE',  ( 209.6877167158270368, 113.4449353909247407, -65.06643844799334886 ) ) ;
#17183 = DIRECTION ( 'NONE',  ( -0.7071067811865474617, -0.7071067811865474617, 1.196099074440432629E-16 ) ) ;
#17184 = CARTESIAN_POINT ( 'NONE',  ( -72.21652659655762818, 19.96855882996548459, 7.213640616729523281 ) ) ;
#17185 = CARTESIAN_POINT ( 'NONE',  ( 45.74764628539832501, -59.37057832282265935, 41.38025477438755928 ) ) ;
#17186 = CARTESIAN_POINT ( 'NONE',  ( -51.34325167237331300, 13.71819364263221708, 17.49572699254425245 ) ) ;
#17187 = VECTOR ( 'NONE', #52834, 1000.000000000000000 ) ;
#17188 = CARTESIAN_POINT ( 'NONE',  ( 153.8366942494330374, 54.87992279068316037, -37.05910186496495129 ) ) ;
#17189 = CARTESIAN_POINT ( 'NONE',  ( 433.3728120124416137, 400.0000000000066507, 99.58582976392122532 ) ) ;
#17190 = ORIENTED_EDGE ( 'NONE', *, *, #13648, .F. ) ;
#17191 = CARTESIAN_POINT ( 'NONE',  ( -45.81425895439424778, 46.10914959592843587, 170.0000000000000000 ) ) ;
#17192 = CARTESIAN_POINT ( 'NONE',  ( -34.79003307268509815, -38.19633032695429620, 26.66469066592268788 ) ) ;
#17193 = ORIENTED_EDGE ( 'NONE', *, *, #64153, .F. ) ;
#17194 = CARTESIAN_POINT ( 'NONE',  ( 164.6046919270428930, 63.41782451559755174, -95.00000000000133582 ) ) ;
#17195 = ORIENTED_EDGE ( 'NONE', *, *, #11489, .F. ) ;
#17196 = B_SPLINE_CURVE_WITH_KNOTS ( 'NONE', 3,
 ( #5301, #47167, #52455, #14481, #31352, #58749, #41899, #15168, #36634, #52109, #48188, #31014, #58081, #30659, #21144, #57737, #3926, #31688, #52780, #4607, #20783, #41556, #32037, #42251, #63709, #15, #64043, #53471, #15853, #37297, #20103, #14811, #15520, #25398, #36974, #21470, #26759, #47857, #69320, #35936, #46829, #25737, #68298, #63010 ),
 .UNSPECIFIED., .F., .F.,
 ( 4, 2, 2, 2, 2, 2, 2, 2, 2, 2, 2, 2, 2, 2, 2, 2, 2, 2, 2, 2, 2, 4 ),
 ( 0.02495775893651562202, 0.02650251144344300744, 0.02804726395037039632, 0.02959201645729778174, 0.03113676896422517063, 0.03268152147115255951, 0.03345389772461624528, 0.03422627397807993799, 0.03577102648500731646, 0.03654340273847100223, 0.03731577899193469494, 0.03808815524539838071, 0.03886053149886206648, 0.04040528400578949353, 0.04117766025925322093, 0.04195003651271693446, 0.04349478901964438926, 0.04503954152657183019, 0.04581191778003557147, 0.04658429403349930581, 0.04812904654042679531, 0.04967379904735429175 ),
 .UNSPECIFIED. ) ;
#17197 = CARTESIAN_POINT ( 'NONE',  ( -85.91089317961402116, 25.21459833389209493, 35.91092548939403883 ) ) ;
#17198 = CARTESIAN_POINT ( 'NONE',  ( -25.48750459758503339, 9.705678256319570707, -74.25185047208405820 ) ) ;
#17199 = CARTESIAN_POINT ( 'NONE',  ( 46.90208227351339332, 10.52324439420451618, 37.17192485722242168 ) ) ;
#17200 = CARTESIAN_POINT ( 'NONE',  ( -56.92000000000000171, 0.000000000000000000, 0.000000000000000000 ) ) ;
#17201 = EDGE_CURVE ( 'NONE', #30930, #9949, #51985, .T. ) ;
#17202 = CARTESIAN_POINT ( 'NONE',  ( 126.9201538765324386, 37.39093565120715112, -13.81500352634632378 ) ) ;
#17203 = ORIENTED_EDGE ( 'NONE', *, *, #18397, .T. ) ;
#17204 = MANIFOLD_SOLID_BREP ( 'Boss-Extrude1', #30577 ) ;
#17205 = EDGE_LOOP ( 'NONE', ( #19991, #26235, #26728, #57821, #46100, #14171, #53172, #19, #60739, #40724, #18457, #14597 ) ) ;
#17206 = DIRECTION ( 'NONE',  ( -0.000000000000000000, -1.000000000000000000, -0.000000000000000000 ) ) ;
#17207 = EDGE_LOOP ( 'NONE', ( #59578, #14563, #1327, #44123 ) ) ;
#17208 = DIRECTION ( 'NONE',  ( -0.000000000000000000, 1.000000000000000000, -0.000000000000000000 ) ) ;
#17209 = CARTESIAN_POINT ( 'NONE',  ( -60.57719029284778145, -27.78504199349144699, 34.48241795236666007 ) ) ;
#17210 = CARTESIAN_POINT ( 'NONE',  ( -3.253130881186333756, 7.643323950922366272, 58.49497839819474621 ) ) ;
#17211 = ADVANCED_FACE ( 'NONE', ( #6117 ), #9775, .T. ) ;
#17212 = CARTESIAN_POINT ( 'NONE',  ( 198.0161777302107851, 99.22276840862558345, -94.07682923140444586 ) ) ;
#17213 = CARTESIAN_POINT ( 'NONE',  ( 60.00000000000000000, 0.000000000000000000, 5.000000000000000000 ) ) ;
#17214 = ORIENTED_EDGE ( 'NONE', *, *, #12997, .F. ) ;
#17215 = VECTOR ( 'NONE', #2187, 1000.000000000000000 ) ;
#17216 = EDGE_CURVE ( 'NONE', #1714, #1913, #28634, .T. ) ;
#17217 = CARTESIAN_POINT ( 'NONE',  ( -122.3963566076408114, 44.23346594671846788, -75.90953027873555925 ) ) ;
#17218 = EDGE_LOOP ( 'NONE', ( #5968, #40866, #12860, #11528 ) ) ;
#17219 = EDGE_CURVE ( 'NONE', #56212, #863, #39451, .T. ) ;
#17220 = VERTEX_POINT ( 'NONE', #17370 ) ;
#17221 = CARTESIAN_POINT ( 'NONE',  ( 447.3372781065085064, 400.0000000000001137, -146.4497041420118535 ) ) ;
#17222 = FACE_OUTER_BOUND ( 'NONE', #46725, .T. ) ;
#17223 = CARTESIAN_POINT ( 'NONE',  ( 447.3372781065085633, 400.0000000000000568, -111.4497041420118251 ) ) ;
#17224 = CARTESIAN_POINT ( 'NONE',  ( 136.1037846510192821, 43.98155406734452555, 17.33612899941342178 ) ) ;
#17225 = DIRECTION ( 'NONE',  ( -0.8584487936018727616, 0.5128992774058949156, 0.000000000000000000 ) ) ;
#17226 = CIRCLE ( 'NONE', #65550, 5.000000000000004441 ) ;
#17227 = ORIENTED_EDGE ( 'NONE', *, *, #20983, .T. ) ;
#17228 = AXIS2_PLACEMENT_3D ( 'NONE', #4230, #14441, #63318 ) ;
#17229 = FACE_OUTER_BOUND ( 'NONE', #68189, .T. ) ;
#17230 = DIRECTION ( 'NONE',  ( 0.000000000000000000, 0.000000000000000000, 1.000000000000000000 ) ) ;
#17231 = VECTOR ( 'NONE', #54501, 1000.000000000000000 ) ;
#17232 = CARTESIAN_POINT ( 'NONE',  ( -77.71448999903257970, 21.96089801565738853, 45.37296549835471637 ) ) ;
#17233 = VERTEX_POINT ( 'NONE', #69192 ) ;
#17234 = LINE ( 'NONE', #55221, #13986 ) ;
#17235 = CIRCLE ( 'NONE', #34136, 5.000000000000004441 ) ;
#17236 = AXIS2_PLACEMENT_3D ( 'NONE', #42553, #15822, #37264 ) ;
#17237 = VERTEX_POINT ( 'NONE', #49718 ) ;
#17238 = FACE_OUTER_BOUND ( 'NONE', #51093, .T. ) ;
#17239 = CARTESIAN_POINT ( 'NONE',  ( 93.86680996363769225, 22.01878169039503419, 12.35045139323386643 ) ) ;
#17240 = EDGE_CURVE ( 'NONE', #8652, #10029, #46217, .T. ) ;
#17241 = FACE_OUTER_BOUND ( 'NONE', #46103, .T. ) ;
#17242 = EDGE_LOOP ( 'NONE', ( #52824, #58022, #67424, #2546 ) ) ;
#17243 = EDGE_CURVE ( 'NONE', #64171, #45918, #55001, .T. ) ;
#17244 = LINE ( 'NONE', #49952, #47995 ) ;
#17246 =( BOUNDED_CURVE ( )  B_SPLINE_CURVE ( 3, ( #8772, #30218, #41464, #15756 ),
 .UNSPECIFIED., .F., .F. ) 
 B_SPLINE_CURVE_WITH_KNOTS ( ( 4, 4 ),
 ( 2.506209174768083692, 3.776976132411494103 ),
 .UNSPECIFIED. ) 
 CURVE ( )  GEOMETRIC_REPRESENTATION_ITEM ( )  RATIONAL_B_SPLINE_CURVE ( ( 1.000000000000000000, 0.8698961108463045822, 0.8698961108463045822, 1.000000000000000000 ) ) 
 REPRESENTATION_ITEM ( '' )  );
#17245 = DIRECTION ( 'NONE',  ( -0.000000000000000000, -0.000000000000000000, -1.000000000000000000 ) ) ;
#17247 = CARTESIAN_POINT ( 'NONE',  ( 31.96192885395476679, 8.569232728322429438, 38.39183651277110698 ) ) ;
#17248 = CARTESIAN_POINT ( 'NONE',  ( -179.2210908201800521, 95.76260491022613053, -37.81988327838237751 ) ) ;
#17249 = CARTESIAN_POINT ( 'NONE',  ( -133.1527834403230770, 51.46311219732125153, -13.66430714595139051 ) ) ;
#17250 = LINE ( 'NONE', #49250, #63738 ) ;
#17251 = CARTESIAN_POINT ( 'NONE',  ( -31.90315521289150524, 56.64813493366005304, 0.000000000000000000 ) ) ;
#17252 = ORIENTED_EDGE ( 'NONE', *, *, #66000, .F. ) ;
#17253 = DIRECTION ( 'NONE',  ( 0.000000000000000000, 1.000000000000000000, 0.000000000000000000 ) ) ;
#17254 = DIRECTION ( 'NONE',  ( -0.000000000000000000, -0.000000000000000000, -1.000000000000000000 ) ) ;
#17255 = VERTEX_POINT ( 'NONE', #7178 ) ;
#17256 = FACE_BOUND ( 'NONE', #28707, .T. ) ;
#17257 = CARTESIAN_POINT ( 'NONE',  ( -1.319107422865891888, 6.554467368239800251, -73.52547515260555144 ) ) ;
#17258 = CARTESIAN_POINT ( 'NONE',  ( -175.9944734395085675, 91.92390745845760591, 72.10689250308911369 ) ) ;
#17259 = CARTESIAN_POINT ( 'NONE',  ( -143.8756912989387047, 60.83492035645719653, -10.50900835034600433 ) ) ;
#17260 = LINE ( 'NONE', #14346, #59255 ) ;
#17261 = FACE_OUTER_BOUND ( 'NONE', #21729, .T. ) ;
#17262 = CARTESIAN_POINT ( 'NONE',  ( 15.78827728214693416, 6.500811158483329244, -62.36349468914946925 ) ) ;
#17263 = CARTESIAN_POINT ( 'NONE',  ( 113.3030319151915251, 21.67621409537482080, -3.767785295203596618 ) ) ;
#17264 = DIRECTION ( 'NONE',  ( 0.000000000000000000, 0.000000000000000000, 1.000000000000000000 ) ) ;
#17265 = CARTESIAN_POINT ( 'NONE',  ( 55.76286625948333864, 11.10663164471739606, -95.00000000000133582 ) ) ;
#17266 = CARTESIAN_POINT ( 'NONE',  ( 110.2429982417149290, 28.88204397445231209, 2.766663615273646570 ) ) ;
#17267 = CARTESIAN_POINT ( 'NONE',  ( 90.91356992076214283, 21.99794663086828450, -10.31639574584678343 ) ) ;
#17268 = VERTEX_POINT ( 'NONE', #65222 ) ;
#17269 = VECTOR ( 'NONE', #27888, 1000.000000000000000 ) ;
#17270 = CARTESIAN_POINT ( 'NONE',  ( -38.54237244144231056, 11.89088379031761811, 13.29149674035523176 ) ) ;
#17271 = ORIENTED_EDGE ( 'NONE', *, *, #58265, .F. ) ;
#17272 = CARTESIAN_POINT ( 'NONE',  ( -444.4229916354186116, 394.6798985497181889, 95.69015420990594123 ) ) ;
#17273 = CARTESIAN_POINT ( 'NONE',  ( 81.57915404881514121, 18.81499384983930057, -75.71637441921426159 ) ) ;
#17274 = AXIS2_PLACEMENT_3D ( 'NONE', #13578, #7269, #39963 ) ;
#17275 = CARTESIAN_POINT ( 'NONE',  ( 109.0088647218444464, 29.42125915259915203, 83.39562742996727707 ) ) ;
#17276 = DIRECTION ( 'NONE',  ( 1.000000000000000000, 1.110223024625155594E-14, -1.110223024625155594E-14 ) ) ;
#17277 = CARTESIAN_POINT ( 'NONE',  ( 70.11766033381769603, 14.43277633974326335, -18.83692018523840517 ) ) ;
#17278 = CARTESIAN_POINT ( 'NONE',  ( -27.49195330402088544, 9.993776132065304907, -49.19917853453215173 ) ) ;
#17279 = PRODUCT_RELATED_PRODUCT_CATEGORY ( 'part', '', ( #37747 ) ) ;
#17280 = DIRECTION ( 'NONE',  ( -1.000000000000000000, 0.000000000000000000, 0.000000000000000000 ) ) ;
#17281 = AXIS2_PLACEMENT_3D ( 'NONE', #24497, #8659, #51565 ) ;
#17282 = CARTESIAN_POINT ( 'NONE',  ( -71.98415129531598211, 20.95325475002097804, -92.86987620278186739 ) ) ;
#17283 = ORIENTED_EDGE ( 'NONE', *, *, #36081, .F. ) ;
#17284 = AXIS2_PLACEMENT_3D ( 'NONE', #26807, #25448, #47216 ) ;
#17285 = ORIENTED_EDGE ( 'NONE', *, *, #22337, .T. ) ;
#17286 = EDGE_CURVE ( 'NONE', #863, #24361, #39197, .T. ) ;
#17287 = AXIS2_PLACEMENT_3D ( 'NONE', #66229, #27870, #65879 ) ;
#17288 = CARTESIAN_POINT ( 'NONE',  ( 427.4999999999999432, 207.5000000000000284, 378.0000000000000000 ) ) ;
#17289 = CARTESIAN_POINT ( 'NONE',  ( -10.50008294601455106, -40.38642021005834692, 13.79046340968178974 ) ) ;
#17290 = CARTESIAN_POINT ( 'NONE',  ( 35.39413431650373099, 0.000000000000000000, -5.000000000000000000 ) ) ;
#17291 = CARTESIAN_POINT ( 'NONE',  ( -165.7713056973201731, 80.74264649718247711, 66.68892821721664177 ) ) ;
#17292 = EDGE_CURVE ( 'NONE', #39465, #8984, #43745, .T. ) ;
#17293 = VECTOR ( 'NONE', #19939, 1000.000000000000000 ) ;
#17294 = CARTESIAN_POINT ( 'NONE',  ( -44.00727179482512241, -47.83680621839620528, 40.00000000000003553 ) ) ;
#17295 = VECTOR ( 'NONE', #48936, 1000.000000000000000 ) ;
#17296 = CARTESIAN_POINT ( 'NONE',  ( -31.11269837220806878, 5.594483210025202879E-14, 0.000000000000000000 ) ) ;
#17297 = ORIENTED_EDGE ( 'NONE', *, *, #64380, .T. ) ;
#17298 = CARTESIAN_POINT ( 'NONE',  ( 105.4134760436918441, 27.80903124201756427, -37.66340175651738775 ) ) ;
#17299 = CARTESIAN_POINT ( 'NONE',  ( 182.7686108735401547, 81.77235358504611895, -24.20125551499105754 ) ) ;
#17300 = CARTESIAN_POINT ( 'NONE',  ( -85.75947274862031122, 25.15128705015481358, -18.25927382592571036 ) ) ;
#17301 = DIRECTION ( 'NONE',  ( 0.000000000000000000, 1.000000000000000000, -0.000000000000000000 ) ) ;
#17302 = CYLINDRICAL_SURFACE ( 'NONE', #47535, 5.000000000000000888 ) ;
#17303 = FACE_OUTER_BOUND ( 'NONE', #65406, .T. ) ;
#17304 = FACE_BOUND ( 'NONE', #35211, .T. ) ;
#17305 = CARTESIAN_POINT ( 'NONE',  ( -62.15799747763097827, 16.70234469631019536, -45.16847623433110925 ) ) ;
#17306 = EDGE_CURVE ( 'NONE', #50199, #34598, #1917, .T. ) ;
#17307 = EDGE_CURVE ( 'NONE', #37904, #65910, #1547, .T. ) ;
#17308 = ORIENTED_EDGE ( 'NONE', *, *, #27041, .T. ) ;
#17309 = EDGE_CURVE ( 'NONE', #39573, #51452, #60293, .T. ) ;
#17310 = PLANE ( 'NONE',  #63872 ) ;
#17311 = CARTESIAN_POINT ( 'NONE',  ( 92.21252738308864139, 22.47457138983956781, -48.35361511676679669 ) ) ;
#17312 = CARTESIAN_POINT ( 'NONE',  ( -47.61402178322637013, 13.84598486314981969, 63.67307924642992845 ) ) ;
#17313 = CARTESIAN_POINT ( 'NONE',  ( -180.6021503146988607, 97.45669259943416307, 12.09742955499907247 ) ) ;
#17314 = CARTESIAN_POINT ( 'NONE',  ( 211.8345664497466032, 118.5225165986914533, 61.22447077958275941 ) ) ;
#17315 = DIRECTION ( 'NONE',  ( 1.000000000000000000, 1.850550996349095901E-16, 1.228197773518735191E-20 ) ) ;
#17316 = VERTEX_POINT ( 'NONE', #50088 ) ;
#17317 = CARTESIAN_POINT ( 'NONE',  ( 56.19513604272052021, 11.19349063094195174, 13.59754376101736817 ) ) ;
#17318 = CARTESIAN_POINT ( 'NONE',  ( -55.05276343752909440, 14.68156374112638929, 57.16187836339483397 ) ) ;
#17319 = EDGE_LOOP ( 'NONE', ( #16011, #64545, #1545, #18990 ) ) ;
#17320 = ORIENTED_EDGE ( 'NONE', *, *, #13419, .F. ) ;
#17321 = VECTOR ( 'NONE', #42765, 1000.000000000000000 ) ;
#17322 = CARTESIAN_POINT ( 'NONE',  ( -4.180838820195678096, -65.23214221112786504, 41.38025477438755928 ) ) ;
#17323 = LINE ( 'NONE', #38798, #19808 ) ;
#17324 = CARTESIAN_POINT ( 'NONE',  ( 102.7571040248401033, 25.57023079238897267, 37.63868481140666944 ) ) ;
#17325 = VERTEX_POINT ( 'NONE', #17013 ) ;
#17326 = ORIENTED_EDGE ( 'NONE', *, *, #15864, .T. ) ;
#17327 = LINE ( 'NONE', #11701, #11643 ) ;
#17328 = CARTESIAN_POINT ( 'NONE',  ( 160.5018603162735360, 61.33906090758085838, 30.03480990559012298 ) ) ;
#17329 = CARTESIAN_POINT ( 'NONE',  ( 103.8325688302027316, 27.12251147381400784, 6.365378839190652727 ) ) ;
#17330 = CARTESIAN_POINT ( 'NONE',  ( 67.54641595172915913, 14.80690682047551299, 16.46492756229169530 ) ) ;
#17331 = CONICAL_SURFACE ( 'NONE', #18456, 65.00000000000000000, 0.7853981633974497223 ) ;
#17332 = CARTESIAN_POINT ( 'NONE',  ( 88.53517449242353621, 20.08005703101045114, 44.46986225549056115 ) ) ;
#17333 = AXIS2_PLACEMENT_3D ( 'NONE', #16848, #21436, #32007 ) ;
#17334 = VECTOR ( 'NONE', #54952, 1000.000000000000000 ) ;
#17335 = CARTESIAN_POINT ( 'NONE',  ( -39.55079474733624068, -51.59997227571040668, 0.000000000000000000 ) ) ;
#17336 = CARTESIAN_POINT ( 'NONE',  ( 209.9999999999999716, 192.0000000000000000, 72.99999999999998579 ) ) ;
#17337 = CARTESIAN_POINT ( 'NONE',  ( 181.0840389613909736, 80.03940679743416808, 56.15314469597509373 ) ) ;
#17338 = CARTESIAN_POINT ( 'NONE',  ( -149.9125899128210051, 65.84729237358621390, -88.50193171241929235 ) ) ;
#17339 = CARTESIAN_POINT ( 'NONE',  ( 311.9975424824652350, 20.00000000000003197, 536.6193948016162949 ) ) ;
#17340 = CARTESIAN_POINT ( 'NONE',  ( 89.81152435583800298, 20.53127581368840282, 84.10198394837142644 ) ) ;
#17342 = ORIENTED_EDGE ( 'NONE', *, *, #34077, .T. ) ;
#17341 = CARTESIAN_POINT ( 'NONE',  ( 437.3372781065085633, 399.9999999999998863, 103.5502958579881891 ) ) ;
#17343 = EDGE_LOOP ( 'NONE', ( #3238, #66763, #25825, #6216 ) ) ;
#17344 = ORIENTED_EDGE ( 'NONE', *, *, #66988, .T. ) ;
#17345 = CARTESIAN_POINT ( 'NONE',  ( -15.22871623201694646, 7.486724405784664249, -17.29878459576774574 ) ) ;
#17346 = CARTESIAN_POINT ( 'NONE',  ( -50.13771638889891591, 13.41835215703893347, 43.50352009537876086 ) ) ;
#17347 = DIRECTION ( 'NONE',  ( 1.000000000000000000, 0.000000000000000000, 0.000000000000000000 ) ) ;
#17348 = DIRECTION ( 'NONE',  ( 0.000000000000000000, -1.000000000000000000, 0.000000000000000000 ) ) ;
#17349 = CARTESIAN_POINT ( 'NONE',  ( -62.29496909743951960, 17.79481128341706153, -40.75095302798493435 ) ) ;
#17350 = CARTESIAN_POINT ( 'NONE',  ( 26.98325885506551813, 31.83109204562614636, 13.79046340968179152 ) ) ;
#17351 = CARTESIAN_POINT ( 'NONE',  ( 5.799999999999999822, -4.618802153517012954, -8.000000000000001776 ) ) ;
#17352 = CARTESIAN_POINT ( 'NONE',  ( 23.03578842369135415, 6.840884649289440844, -18.11974505773217103 ) ) ;
#17353 = ORIENTED_EDGE ( 'NONE', *, *, #38024, .F. ) ;
#17354 = LINE ( 'NONE', #38831, #27280 ) ;
#17355 = ORIENTED_EDGE ( 'NONE', *, *, #55101, .T. ) ;
#17356 = VERTEX_POINT ( 'NONE', #18084 ) ;
#17357 = CARTESIAN_POINT ( 'NONE',  ( -142.0860844253782886, 59.41107357617635643, 10.25687802980160690 ) ) ;
#17358 = CARTESIAN_POINT ( 'NONE',  ( -28.93113808661575703, 10.21102608966478265, 84.32986548825184059 ) ) ;
#17359 = CARTESIAN_POINT ( 'NONE',  ( -95.21430597939259144, 29.33390900154321912, -45.08002014446414307 ) ) ;
#17360 = B_SPLINE_CURVE_WITH_KNOTS ( 'NONE', 3,
 ( #1182, #12436, #49348, #17350, #13141, #17718 ),
 .UNSPECIFIED., .F., .F.,
 ( 4, 2, 4 ),
 ( 1.095770181108053550E-06, 0.03239442681617710207, 0.06478775786217309818 ),
 .UNSPECIFIED. ) ;
#17361 = EDGE_CURVE ( 'NONE', #9937, #28396, #59573, .T. ) ;
#17362 = PLANE ( 'NONE',  #24832 ) ;
#17363 = CARTESIAN_POINT ( 'NONE',  ( -72.99999999999998579, 0.000000000000000000, 85.00000000000000000 ) ) ;
#17364 = CARTESIAN_POINT ( 'NONE',  ( 139.2794027252093940, 45.99190465195507471, -11.47524523421667553 ) ) ;
#17365 = VERTEX_POINT ( 'NONE', #28271 ) ;
#17366 = ORIENTED_EDGE ( 'NONE', *, *, #60571, .T. ) ;
#17367 = EDGE_CURVE ( 'NONE', #6690, #17220, #55711, .T. ) ;
#17368 = ORIENTED_EDGE ( 'NONE', *, *, #39723, .F. ) ;
#17369 = VECTOR ( 'NONE', #43543, 999.9999999999998863 ) ;
#17370 = CARTESIAN_POINT ( 'NONE',  ( 99.99999999999997158, 6.000000000000000000, -3.000000000000030198 ) ) ;
#17371 = CARTESIAN_POINT ( 'NONE',  ( -154.8006992380339000, 70.15733562427992354, -10.13360984257536579 ) ) ;
#17372 = DIRECTION ( 'NONE',  ( -1.000000000000000000, -1.110223024625155594E-14, 1.110223024625155594E-14 ) ) ;
#17373 = ADVANCED_FACE ( 'NONE', ( #34266 ), #44459, .T. ) ;
#17374 = CARTESIAN_POINT ( 'NONE',  ( 55.76066037845579615, 11.10616952318092387, -18.34132239558550737 ) ) ;
#17375 = ADVANCED_FACE ( 'NONE', ( #54294 ), #17740, .T. ) ;
#17376 = DIRECTION ( 'NONE',  ( 0.9639628606958512425, 0.2660368455666826670, 0.000000000000000000 ) ) ;
#17377 = DIRECTION ( 'NONE',  ( 1.000000000000000000, 0.000000000000000000, 0.000000000000000000 ) ) ;
#17378 = VERTEX_POINT ( 'NONE', #61337 ) ;
#17379 = CARTESIAN_POINT ( 'NONE',  ( 188.2962140587030149, 87.71627202537838741, 61.57422339708019621 ) ) ;
#17380 = CARTESIAN_POINT ( 'NONE',  ( 203.9228889538744909, 106.9879579748728275, -78.14080293397877597 ) ) ;
#17381 =( NAMED_UNIT ( * ) SI_UNIT ( $, .STERADIAN. ) SOLID_ANGLE_UNIT ( ) );
#17382 = FACE_OUTER_BOUND ( 'NONE', #10829, .T. ) ;
#17383 = CARTESIAN_POINT ( 'NONE',  ( 103.0103829243729194, 25.67737053862328622, 12.31638664800049909 ) ) ;
#17384 = CARTESIAN_POINT ( 'NONE',  ( -166.2546536130332981, 79.79692681634925577, -92.87286366454794972 ) ) ;
#17385 = CARTESIAN_POINT ( 'NONE',  ( 0.2727178028659107412, 0.000000000000000000, 0.000000000000000000 ) ) ;
#17386 = AXIS2_PLACEMENT_3D ( 'NONE', #32273, #11843, #37189 ) ;
#17387 = DIRECTION ( 'NONE',  ( 0.000000000000000000, 0.000000000000000000, -1.000000000000000000 ) ) ;
#17388 = CARTESIAN_POINT ( 'NONE',  ( -29.47687737404360675, -68.96458294135908318, 43.58025477438756212 ) ) ;
#17389 = VECTOR ( 'NONE', #12285, 1000.000000000000000 ) ;
#17390 = AXIS2_PLACEMENT_3D ( 'NONE', #45904, #13889, #35352 ) ;
#17391 = EDGE_CURVE ( 'NONE', #64034, #55870, #7538, .T. ) ;
#17392 = VERTEX_POINT ( 'NONE', #18774 ) ;
#17393 = CARTESIAN_POINT ( 'NONE',  ( -8.000000000000000000, 3.871967595402113105, -0.4989386132324536427 ) ) ;
#17394 = CARTESIAN_POINT ( 'NONE',  ( 180.2572128312847894, 77.77323980479704346, 29.34246328274604210 ) ) ;
#17395 = CARTESIAN_POINT ( 'NONE',  ( -102.2801239173131052, 33.91021738430207932, -76.85912785543962400 ) ) ;
#17396 = CARTESIAN_POINT ( 'NONE',  ( 46.50704915687942531, 9.440294391580046351, -67.55012544208800307 ) ) ;
#17397 = LINE ( 'NONE', #60663, #62487 ) ;
#17398 = EDGE_LOOP ( 'NONE', ( #68463, #64651, #6878, #41873 ) ) ;
#17399 = ORIENTED_EDGE ( 'NONE', *, *, #56393, .F. ) ;
#17400 = DIRECTION ( 'NONE',  ( -0.000000000000000000, 1.000000000000000000, -0.000000000000000000 ) ) ;
#17401 = CARTESIAN_POINT ( 'NONE',  ( 176.0086785549255239, 73.62390276844820391, 84.96622182719073635 ) ) ;
#17402 = ORIENTED_EDGE ( 'NONE', *, *, #67514, .T. ) ;
#17403 = EDGE_LOOP ( 'NONE', ( #32111, #34903 ) ) ;
#17404 = CARTESIAN_POINT ( 'NONE',  ( -190.6985136298601731, 109.1272424661242582, -95.00000000000133582 ) ) ;
#17405 = CARTESIAN_POINT ( 'NONE',  ( 0.000000000000000000, 0.000000000000000000, 0.000000000000000000 ) ) ;
#17406 = ORIENTED_EDGE ( 'NONE', *, *, #45812, .T. ) ;
#17407 = CARTESIAN_POINT ( 'NONE',  ( -62.97854483871577713, 16.08424353203677271, 170.0000000000000000 ) ) ;
#17408 = CARTESIAN_POINT ( 'NONE',  ( 133.8566784816069344, 42.60093787723652525, 56.35489142945903751 ) ) ;
#17409 = CARTESIAN_POINT ( 'NONE',  ( -75.00168449119584579, 20.95943092127969365, -36.06733346853133071 ) ) ;
#17410 = CARTESIAN_POINT ( 'NONE',  ( 36.85262215550067566, 53.56030941157737146, 170.0000000000000000 ) ) ;
#17411 = DIRECTION ( 'NONE',  ( -1.000000000000000000, 0.000000000000000000, 2.312964634635743450E-16 ) ) ;
#17412 = CARTESIAN_POINT ( 'NONE',  ( -52.68206656346369243, 15.09776187114412593, -8.752186859763938287 ) ) ;
#17413 = ORIENTED_EDGE ( 'NONE', *, *, #68150, .T. ) ;
#17414 = CARTESIAN_POINT ( 'NONE',  ( 115.0454575488273576, 31.16784721673995406, -49.18829330954620360 ) ) ;
#17415 = VECTOR ( 'NONE', #21481, 1000.000000000000000 ) ;
#17416 = CARTESIAN_POINT ( 'NONE',  ( -71.86568654225716557, 20.91200104397923809, 7.901464635737869280 ) ) ;
#17417 = CARTESIAN_POINT ( 'NONE',  ( -142.1332311300252798, 59.44822332309656332, -43.70847484967913488 ) ) ;
#17418 = CARTESIAN_POINT ( 'NONE',  ( -171.0950923142953570, 86.38958441093222973, -76.29032179032941485 ) ) ;
#17419 = AXIS2_PLACEMENT_3D ( 'NONE', #744, #37673, #22198 ) ;
#17421 = ORIENTED_EDGE ( 'NONE', *, *, #7470, .F. ) ;
#17420 = CARTESIAN_POINT ( 'NONE',  ( -120.6555520024721488, 43.14028137839566313, 86.43234750685729750 ) ) ;
#17422 = CARTESIAN_POINT ( 'NONE',  ( 56.52205390515079131, 12.28646189164057390, 14.25333810830040804 ) ) ;
#17423 = AXIS2_PLACEMENT_3D ( 'NONE', #49104, #6567, #33660 ) ;
#17424 = VECTOR ( 'NONE', #21291, 1000.000000000000000 ) ;
#17425 = VERTEX_POINT ( 'NONE', #61678 ) ;
#17427 = EDGE_CURVE ( 'NONE', #35065, #1572, #19818, .T. ) ;
#17426 = CARTESIAN_POINT ( 'NONE',  ( -131.3154845336012500, 50.16828105866952825, 32.91510348359927463 ) ) ;
#17428 = DIRECTION ( 'NONE',  ( -1.000000000000000000, 0.000000000000000000, 0.000000000000000000 ) ) ;
#17429 = FACE_OUTER_BOUND ( 'NONE', #4820, .T. ) ;
#17430 =( GEOMETRIC_REPRESENTATION_CONTEXT ( 3 ) GLOBAL_UNCERTAINTY_ASSIGNED_CONTEXT ( ( #29000 ) ) GLOBAL_UNIT_ASSIGNED_CONTEXT ( ( #46628, #56851, #51226 ) ) REPRESENTATION_CONTEXT ( 'NONE', 'WORKASPACE' ) );
#17432 = CARTESIAN_POINT ( 'NONE',  ( 88.98820631332496589, 21.30618275724810573, 30.07647440311880871 ) ) ;
#17431 = CIRCLE ( 'NONE', #32011, 5.000000000000018652 ) ;
#17433 = CARTESIAN_POINT ( 'NONE',  ( 134.3172730033262496, 41.70277427218488953, -9.178760341931965883 ) ) ;
#17434 = CARTESIAN_POINT ( 'NONE',  ( -79.14094329813315198, 23.58034730000056811, -23.27090004125423661 ) ) ;
#17435 = CARTESIAN_POINT ( 'NONE',  ( 90.30166390191405412, 20.70652093100730440, -76.72363925761264625 ) ) ;
#17436 = VECTOR ( 'NONE', #30089, 1000.000000000000000 ) ;
#17437 = CARTESIAN_POINT ( 'NONE',  ( -24.80529805274337463, 8.596106904667630388, -92.98064582061705607 ) ) ;
#17438 = CARTESIAN_POINT ( 'NONE',  ( -156.9402586331177361, 70.74941713998435944, -95.00000000000133582 ) ) ;
#17439 = ORIENTED_EDGE ( 'NONE', *, *, #48024, .T. ) ;
#17440 = ORIENTED_EDGE ( 'NONE', *, *, #38264, .F. ) ;
#17441 = CARTESIAN_POINT ( 'NONE',  ( 46.85206196242845067, 9.495795933269473466, 36.42025845728678490 ) ) ;
#17442 = FACE_OUTER_BOUND ( 'NONE', #36251, .T. ) ;
#17443 = CARTESIAN_POINT ( 'NONE',  ( 55.14772863908673628, -34.40534879854659778, 170.0000000000000000 ) ) ;
#17444 = CARTESIAN_POINT ( 'NONE',  ( 0.000000000000000000, 0.000000000000000000, 0.000000000000000000 ) ) ;
#17445 = CARTESIAN_POINT ( 'NONE',  ( 212.1978255065450583, 119.0880569674902603, -43.47704106856255635 ) ) ;
#17446 = PLANE ( 'NONE',  #53920 ) ;
#17447 = CARTESIAN_POINT ( 'NONE',  ( 442.3372781065086201, 0.000000000000000000, -136.4497041420118251 ) ) ;
#17448 = CARTESIAN_POINT ( 'NONE',  ( -23.93880457192868860, 8.479983864459176957, -42.57752331243816002 ) ) ;
#17449 = DIRECTION ( 'NONE',  ( -0.000000000000000000, 1.000000000000000000, -0.000000000000000000 ) ) ;
#17450 = ORIENTED_EDGE ( 'NONE', *, *, #42234, .F. ) ;
#17451 = CARTESIAN_POINT ( 'NONE',  ( -24.18158274621863413, 9.527343002918312820, 8.916876208941543425 ) ) ;
#17452 = EDGE_CURVE ( 'NONE', #5465, #2912, #28994, .T. ) ;
#17453 = EDGE_LOOP ( 'NONE', ( #28439, #67569, #39886, #58487 ) ) ;
#17454 = DIRECTION ( 'NONE',  ( -0.000000000000000000, 1.000000000000000000, 0.000000000000000000 ) ) ;
#17455 = CARTESIAN_POINT ( 'NONE',  ( -85.57988666922054222, 25.07649479135944048, 88.68161927237834163 ) ) ;
#17456 = CARTESIAN_POINT ( 'NONE',  ( 0.000000000000000000, 190.0000000000000000, 161.3522585083728700 ) ) ;
#17457 = CARTESIAN_POINT ( 'NONE',  ( 130.3035708464390154, 40.48418876551452428, 43.63269443261444991 ) ) ;
#17458 = CARTESIAN_POINT ( 'NONE',  ( 39.40195752203891999, 9.424259417798145577, 18.06928371549960133 ) ) ;
#17459 = CARTESIAN_POINT ( 'NONE',  ( 36.44731296966019585, -20.32014095137187581, 13.79046412351413586 ) ) ;
#17460 = EDGE_CURVE ( 'NONE', #11439, #59098, #35652, .T. ) ;
#17461 = FACE_OUTER_BOUND ( 'NONE', #21587, .T. ) ;
#17462 = DIRECTION ( 'NONE',  ( -1.000000000000000000, 0.000000000000000000, 0.000000000000000000 ) ) ;
#17463 = CARTESIAN_POINT ( 'NONE',  ( -41.31727360890798906, 62.59299402909750398, 0.000000000000000000 ) ) ;
#17464 =( NAMED_UNIT ( * ) SI_UNIT ( $, .STERADIAN. ) SOLID_ANGLE_UNIT ( ) );
#17465 = VERTEX_POINT ( 'NONE', #24408 ) ;
#17466 = CARTESIAN_POINT ( 'NONE',  ( -29.68020330876228030, 0.000000000000000000, 4.368699068434031219 ) ) ;
#17467 = CARTESIAN_POINT ( 'NONE',  ( 15.29305096970403355, 7.491604910111013815, -62.36349468914947636 ) ) ;
#17468 = CARTESIAN_POINT ( 'NONE',  ( -14.56631729561072675, 8.434645566888201884, 14.09560095912131139 ) ) ;
#17469 = DIRECTION ( 'NONE',  ( -0.8090169943749506709, 0.5877852522924686962, 0.000000000000000000 ) ) ;
#17470 = FACE_OUTER_BOUND ( 'NONE', #1746, .T. ) ;
#17471 = CARTESIAN_POINT ( 'NONE',  ( 85.36151321841643380, 20.05356632597361255, 83.50184739982738336 ) ) ;
#17472 = ADVANCED_FACE ( 'NONE', ( #3626 ), #2258, .F. ) ;
#17473 = VERTEX_POINT ( 'NONE', #62729 ) ;
#17474 = VECTOR ( 'NONE', #59486, 1000.000000000000000 ) ;
#17475 = CARTESIAN_POINT ( 'NONE',  ( 620.5071894358300142, 928.5915846175157640, 815.0951305877183586 ) ) ;
#17476 = CARTESIAN_POINT ( 'NONE',  ( -190.6985136298602015, 109.1272424661243434, -10.81538671745452795 ) ) ;
#17478 = ADVANCED_FACE ( 'NONE', ( #57104 ), #24057, .F. ) ;
#17477 = CARTESIAN_POINT ( 'NONE',  ( -131.6508182719823878, 50.40277850441008667, 6.442247626404384420 ) ) ;
#17479 = CARTESIAN_POINT ( 'NONE',  ( -165.7713056973202015, 80.74264649718247711, -40.68927414463811232 ) ) ;
#17480 = CONTEXT_DEPENDENT_SHAPE_REPRESENTATION ( #65157, #38271 ) ;
#17481 = CARTESIAN_POINT ( 'NONE',  ( -169.0769811399541709, 82.73718697014336954, 85.68819937027275557 ) ) ;
#17482 = ORIENTED_EDGE ( 'NONE', *, *, #6648, .T. ) ;
#17484 = CARTESIAN_POINT ( 'NONE',  ( -31.11269837220806878, 0.000000000000000000, 0.000000000000000000 ) ) ;
#17483 = VECTOR ( 'NONE', #17469, 1000.000000000000114 ) ;
#17485 = AXIS2_PLACEMENT_3D ( 'NONE', #24691, #14475, #41550 ) ;
#17486 = CARTESIAN_POINT ( 'NONE',  ( 313.9975424824652350, 295.8720703627916464, 535.5371946177799600 ) ) ;
#17487 = CARTESIAN_POINT ( 'NONE',  ( -417.6627218934913230, 397.0710678118653618, -111.4497041420117824 ) ) ;
#17488 = CARTESIAN_POINT ( 'NONE',  ( -1.096061481932293358, 7.553048580900442843, -73.08327283968297650 ) ) ;
#17489 = AXIS2_PLACEMENT_3D ( 'NONE', #9157, #66880, #18676 ) ;
#17490 = B_SPLINE_CURVE_WITH_KNOTS ( 'NONE', 3,
 ( #32138, #31792, #52885, #53226, #11359, #32827, #10667, #53575, #58179, #21918, #20892, #54256, #42684, #64143, #15616, #48284, #15957, #37401, #48982, #115, #9998, #64842, #4711, #36735, #69060, #21571, #825, #22273, #43015, #64492, #31451, #16303, #37752, #59200, #11018, #32480, #53913, #5736, #26170, #48626, #42349, #470, #44421, #16982, #39503 ),
 .UNSPECIFIED., .F., .F.,
 ( 4, 2, 2, 1, 2, 2, 2, 2, 2, 2, 2, 2, 2, 2, 2, 2, 2, 2, 2, 2, 2, 2, 4 ),
 ( 0.02346057189573570387, 0.02492590417315497867, 0.02565857031186461606, 0.02639123645057425346, 0.02712390258928389086, 0.02785656872799353173, 0.02932190100541279265, 0.03005456714412241964, 0.03078723328283204316, 0.03225256556025128674, 0.03298523169896092067, 0.03371789783767055459, 0.03518323011508982245, 0.03664856239250909031, 0.03738122853121871036, 0.03811389466992833736, 0.03957922694734757746, 0.04104455922476682450, 0.04250989150218606460, 0.04324255764089569160, 0.04397522377960531165, 0.04544055605702455869, 0.04690588833444379879 ),
 .UNSPECIFIED. ) ;
#17491 =( REPRESENTATION_RELATIONSHIP ('NONE','NONE', #40274, #50551 ) REPRESENTATION_RELATIONSHIP_WITH_TRANSFORMATION ( #21039 )SHAPE_REPRESENTATION_RELATIONSHIP( ) );
#17492 = CARTESIAN_POINT ( 'NONE',  ( 1.224646799147353256E-15, 200.0000000000000000, 10.00000000000000000 ) ) ;
#17493 = ORIENTED_EDGE ( 'NONE', *, *, #22963, .F. ) ;
#17494 = CARTESIAN_POINT ( 'NONE',  ( -61.52761555060400411, 17.56359742150278791, 7.155479614208617001 ) ) ;
#17495 = CARTESIAN_POINT ( 'NONE',  ( 201.9869293910475392, 102.6997661182766990, -36.82124265982815814 ) ) ;
#17496 = CARTESIAN_POINT ( 'NONE',  ( -95.04371414958066566, 30.36527049547257917, 35.98012675971163787 ) ) ;
#17497 = CARTESIAN_POINT ( 'NONE',  ( 20.37135563017389828, 6.690359945346088466, -37.06178491685137288 ) ) ;
#17499 = ORIENTED_EDGE ( 'NONE', *, *, #48620, .F. ) ;
#17498 = CARTESIAN_POINT ( 'NONE',  ( -8.663926357538780820, -23.45072237845004182, 0.000000000000000000 ) ) ;
#17500 = CARTESIAN_POINT ( 'NONE',  ( 266.9165763529819628, -52.00000000000000711, 128.9999999999999716 ) ) ;
#17501 = ORIENTED_EDGE ( 'NONE', *, *, #46286, .T. ) ;
#17502 = ORIENTED_EDGE ( 'NONE', *, *, #42918, .T. ) ;
#17503 = DIRECTION ( 'NONE',  ( -0.000000000000000000, -0.000000000000000000, -1.000000000000000000 ) ) ;
#17504 = CARTESIAN_POINT ( 'NONE',  ( -7.329206686002009974E-14, -41.66904755831212270, 2.000000000000001776 ) ) ;
#17506 = VERTEX_POINT ( 'NONE', #68011 ) ;
#17505 = CARTESIAN_POINT ( 'NONE',  ( -14.84452950307166752, 8.460866451887705253, -72.41633501155601493 ) ) ;
#17507 = CARTESIAN_POINT ( 'NONE',  ( 164.7250737226289914, 63.51898362052163804, 38.83193614737182742 ) ) ;
#17508 = CYLINDRICAL_SURFACE ( 'NONE', #16083, 65.00000000000000000 ) ;
#17509 = FACE_OUTER_BOUND ( 'NONE', #44683, .T. ) ;
#17510 = VERTEX_POINT ( 'NONE', #62378 ) ;
#17511 = ADVANCED_FACE ( 'NONE', ( #56755 ), #45147, .F. ) ;
#17512 = DIRECTION ( 'NONE',  ( 0.1342332658176522697, 0.9909497617679352555, 0.000000000000000000 ) ) ;
#17513 = EDGE_CURVE ( 'NONE', #29791, #6856, #34187, .T. ) ;
#17514 = VECTOR ( 'NONE', #46505, 1000.000000000000000 ) ;
#17515 = CARTESIAN_POINT ( 'NONE',  ( -37.38262509017738466, 10.64263598035110192, -11.37183861185575751 ) ) ;
#17516 = DIRECTION ( 'NONE',  ( -0.000000000000000000, -0.000000000000000000, 1.000000000000000000 ) ) ;
#17517 = CARTESIAN_POINT ( 'NONE',  ( -133.3220917939969468, 52.82057604964899866, 12.34504307300762882 ) ) ;
#17519 = DIRECTION ( 'NONE',  ( 1.000000000000000000, 0.000000000000000000, 0.000000000000000000 ) ) ;
#17518 = B_SPLINE_CURVE_WITH_KNOTS ( 'NONE', 3,
 ( #833, #32149, #53583, #22631, #22281, #49343, #65197, #16992, #1523, #6458, #44070, #22986, #12085, #43719, #5413, #38461, #43027, #28247, #48292, #60615, #37763, #33552, #54979, #6092, #59208, #64850, #16650, #6796, #11028, #44430, #59898, #53923, #5746, #27551, #38107, #65916, #27201, #17713, #24726, #29642, #66952, #7515, #50061, #39852, #12780, #46160, #3266, #39511, #28967, #2572, #67634, #61310, #19428, #13135, #40888, #34242, #13472, #60958, #56036, #29299 ),
 .UNSPECIFIED., .F., .F.,
 ( 4, 2, 2, 2, 2, 2, 2, 2, 2, 2, 2, 2, 2, 2, 2, 2, 2, 2, 2, 2, 2, 2, 2, 2, 2, 2, 2, 2, 2, 4 ),
 ( 0.000000000000000000, 0.001130461533176197342, 0.001695692299764287123, 0.002260923066352376904, 0.003391384599528505725, 0.003956615366116568618, 0.004521846132704631510, 0.005652307665880724336, 0.006782769199056818028, 0.007913230732232909986, 0.009043692265409002812, 0.01017415379858509737, 0.01130461533176118846, 0.01356553839811334809, 0.01469599993128941490, 0.01582646146446547650, 0.01808738453081752684, 0.01921784606399359191, 0.02034830759716966392, 0.02260923066352179406, 0.02487015372987392767, 0.02600061526304999968, 0.02713107679622606822, 0.02826153832940213328, 0.02939199986257820529, 0.03052246139575427383, 0.03165292292893034237, 0.03278338446210641438, 0.03391384599528247945, 0.03617476906163466510 ),
 .UNSPECIFIED. ) ;
#17520 = ORIENTED_EDGE ( 'NONE', *, *, #5526, .F. ) ;
#17521 = ORIENTED_EDGE ( 'NONE', *, *, #50890, .T. ) ;
#17522 = AXIS2_PLACEMENT_3D ( 'NONE', #10445, #68838, #3801 ) ;
#17523 = VERTEX_POINT ( 'NONE', #68352 ) ;
#17524 = FACE_OUTER_BOUND ( 'NONE', #6650, .T. ) ;
#17525 = DIRECTION ( 'NONE',  ( 0.7071067811865475727, 0.000000000000000000, 0.7071067811865474617 ) ) ;
#17526 = VECTOR ( 'NONE', #20340, 1000.000000000000000 ) ;
#17527 = AXIS2_PLACEMENT_3D ( 'NONE', #64127, #58841, #48968 ) ;
#17528 = DIRECTION ( 'NONE',  ( -0.1342332658176667304, 0.9909497617679331460, 0.000000000000000000 ) ) ;
#17529 = CARTESIAN_POINT ( 'NONE',  ( -14.79841479960649053, 20.14961338137236524, 0.000000000000000000 ) ) ;
#17530 = CARTESIAN_POINT ( 'NONE',  ( 8.000000000000007105, 249.8719672152120381, -95.00000000000133582 ) ) ;
#17531 = AXIS2_PLACEMENT_3D ( 'NONE', #1308, #42814, #33332 ) ;
#17532 = DIRECTION ( 'NONE',  ( 1.000000000000000000, 0.000000000000000000, 0.000000000000000000 ) ) ;
#17533 = EDGE_CURVE ( 'NONE', #14951, #19095, #167, .T. ) ;
#17534 = CARTESIAN_POINT ( 'NONE',  ( -133.3926783185151521, 51.63401075114365568, 65.26579531883123764 ) ) ;
#17535 = LINE ( 'NONE', #23175, #36340 ) ;
#17536 = CIRCLE ( 'NONE', #48948, 200.0000000000000000 ) ;
#17537 = ORIENTED_EDGE ( 'NONE', *, *, #37954, .T. ) ;
#17538 = PLANE ( 'NONE',  #29861 ) ;
#17539 = ADVANCED_FACE ( 'NONE', ( #58810 ), #57445, .T. ) ;
#17540 = ORIENTED_EDGE ( 'NONE', *, *, #37282, .T. ) ;
#17542 = AXIS2_PLACEMENT_3D ( 'NONE', #22566, #65486, #17280 ) ;
#17541 = CARTESIAN_POINT ( 'NONE',  ( -95.38834349408374180, 30.52734377185649350, -93.20934587920034176 ) ) ;
#17543 = DIRECTION ( 'NONE',  ( 1.000000000000000000, 0.000000000000000000, 0.000000000000000000 ) ) ;
#17544 = ORIENTED_EDGE ( 'NONE', *, *, #62686, .T. ) ;
#17545 = CARTESIAN_POINT ( 'NONE',  ( 187.9007786055418308, 85.78077355327279463, 39.94804133362764276 ) ) ;
#17546 = EDGE_CURVE ( 'NONE', #25148, #67708, #25754, .T. ) ;
#17547 = PLANE ( 'NONE',  #4031 ) ;
#17548 = CARTESIAN_POINT ( 'NONE',  ( 280.0000000000000000, -21.42428528562853884, 4.999999999999990230 ) ) ;
#17549 = CARTESIAN_POINT ( 'NONE',  ( -64.83840629396344468, -4.580509716060184644, 170.0000000000000000 ) ) ;
#17550 = CARTESIAN_POINT ( 'NONE',  ( 50.97490815085634352, 0.000000000000000000, -36.68900338898716740 ) ) ;
#17551 = EDGE_CURVE ( 'NONE', #33479, #56882, #57423, .T. ) ;
#17552 = CARTESIAN_POINT ( 'NONE',  ( 151.7956716830626362, 53.36999433148314154, -38.71403651737715279 ) ) ;
#17553 = CARTESIAN_POINT ( 'NONE',  ( 0.000000000000000000, 0.000000000000000000, 41.38025477438755928 ) ) ;
#17554 = VERTEX_POINT ( 'NONE', #64097 ) ;
#17555 = CARTESIAN_POINT ( 'NONE',  ( -36.11269837220809364, -10.55634918610397932, 85.00100000000000477 ) ) ;
#17556 = FACE_OUTER_BOUND ( 'NONE', #58132, .T. ) ;
#17557 = EDGE_LOOP ( 'NONE', ( #65306, #34157 ) ) ;
#17558 = CARTESIAN_POINT ( 'NONE',  ( 3.660532965668831462, -7.124194613927639530, -9.499999999999994671 ) ) ;
#17559 = LINE ( 'NONE', #12286, #52032 ) ;
#17560 = VERTEX_POINT ( 'NONE', #31740 ) ;
#17561 = CARTESIAN_POINT ( 'NONE',  ( -27.00000000000000355, -27.00000000000000355, 12.00000000000000000 ) ) ;
#17562 = CARTESIAN_POINT ( 'NONE',  ( -7.825402957745087207, 6.891034867348160731, -62.26262132240749736 ) ) ;
#17563 = LINE ( 'NONE', #65769, #42289 ) ;
#17564 = CARTESIAN_POINT ( 'NONE',  ( 0.000000000000000000, 0.000000000000000000, 170.0000000000000000 ) ) ;
#17565 = EDGE_CURVE ( 'NONE', #43248, #67200, #20489, .T. ) ;
#17566 = VERTEX_POINT ( 'NONE', #32091 ) ;
#17567 = MANIFOLD_SOLID_BREP ( 'OuterRace', #41822 ) ;
#17568 = ORIENTED_EDGE ( 'NONE', *, *, #27312, .T. ) ;
#17569 = EDGE_CURVE ( 'NONE', #47669, #25095, #68658, .T. ) ;
#17570 = EDGE_CURVE ( 'NONE', #1454, #6738, #64794, .T. ) ;
#17571 = EDGE_CURVE ( 'NONE', #41223, #53910, #22928, .T. ) ;
#17572 = PLANE ( 'NONE',  #67174 ) ;
#17573 = ORIENTED_EDGE ( 'NONE', *, *, #17607, .F. ) ;
#17574 = CYLINDRICAL_SURFACE ( 'NONE', #21146, 7.500000000000013323 ) ;
#17575 = CARTESIAN_POINT ( 'NONE',  ( -15.55634918610403439, 5.000000000000028422, 2.000000000000001776 ) ) ;
#17576 = DIRECTION ( 'NONE',  ( -0.000000000000000000, 1.000000000000000000, -0.000000000000000000 ) ) ;
#17577 = CARTESIAN_POINT ( 'NONE',  ( 141.2164820244224188, 47.25271033009985189, 89.21155399097146699 ) ) ;
#17578 = PRODUCT_DEFINITION_SHAPE ( 'NONE', 'NONE',  #38320 ) ;
#17579 = FACE_OUTER_BOUND ( 'NONE', #59747, .T. ) ;
#17580 = VECTOR ( 'NONE', #931, 1000.000000000000000 ) ;
#17581 = ORIENTED_EDGE ( 'NONE', *, *, #54690, .T. ) ;
#17582 = CARTESIAN_POINT ( 'NONE',  ( -118.4553071845215015, 41.78724769484929169, -70.35621148235168221 ) ) ;
#17583 = EDGE_LOOP ( 'NONE', ( #20389, #66667, #24078, #48547 ) ) ;
#17584 = EDGE_LOOP ( 'NONE', ( #46465, #58255, #4281, #68143 ) ) ;
#17585 = CARTESIAN_POINT ( 'NONE',  ( 164.7250737226290482, 63.51898362052163804, -14.85716503355553186 ) ) ;
#17586 = DIRECTION ( 'NONE',  ( 1.000000000000000000, 0.000000000000000000, -0.000000000000000000 ) ) ;
#17587 = VECTOR ( 'NONE', #2861, 1000.000000000000000 ) ;
#17588 = CARTESIAN_POINT ( 'NONE',  ( 26.11269837220806167, -6.375108774214766072E-14, 0.000000000000000000 ) ) ;
#17589 = CARTESIAN_POINT ( 'NONE',  ( 137.5911612413395630, 44.91497189902067078, 16.67414218509417267 ) ) ;
#17590 = DIRECTION ( 'NONE',  ( 0.000000000000000000, -1.000000000000000000, 0.000000000000000000 ) ) ;
#17591 = VECTOR ( 'NONE', #45793, 1000.000000000000000 ) ;
#17592 = ORIENTED_EDGE ( 'NONE', *, *, #2324, .T. ) ;
#17593 = PRODUCT_DEFINITION_FORMATION_WITH_SPECIFIED_SOURCE ( 'ANY', '', #45109, .NOT_KNOWN. ) ;
#17594 = CARTESIAN_POINT ( 'NONE',  ( 79.93126905972556528, 17.24332478304278027, 6.983910173289804568 ) ) ;
#17595 = ORIENTED_EDGE ( 'NONE', *, *, #23035, .F. ) ;
#17596 = DIRECTION ( 'NONE',  ( -0.000000000000000000, 1.000000000000000000, -0.000000000000000000 ) ) ;
#17597 = ORIENTED_EDGE ( 'NONE', *, *, #58189, .F. ) ;
#17598 = CONICAL_SURFACE ( 'NONE', #21014, 65.00000000000000000, 0.7853981633974497223 ) ;
#17599 = CARTESIAN_POINT ( 'NONE',  ( 442.3372781065085633, 369.9999999999999432, 108.5502958579885870 ) ) ;
#17600 = ORIENTED_EDGE ( 'NONE', *, *, #17782, .F. ) ;
#17601 = CYLINDRICAL_SURFACE ( 'NONE', #28581, 5.000000000000004441 ) ;
#17602 = CARTESIAN_POINT ( 'NONE',  ( 87.10668362745096260, 19.58396519288861981, 2.867536982015615799 ) ) ;
#17603 = FACE_OUTER_BOUND ( 'NONE', #19671, .T. ) ;
#17604 = ORIENTED_EDGE ( 'NONE', *, *, #18567, .T. ) ;
#17605 = PLANE ( 'NONE',  #55914 ) ;
#17606 = CARTESIAN_POINT ( 'NONE',  ( 15.78827728214693416, 7.507518794609589818, 30.01470767270522089 ) ) ;
#17607 = EDGE_CURVE ( 'NONE', #34928, #25277, #34973, .T. ) ;
#17608 = CARTESIAN_POINT ( 'NONE',  ( 34.82939798935584719, 8.870855050008911391, 43.37903875302355061 ) ) ;
#17609 = CARTESIAN_POINT ( 'NONE',  ( -180.5234362879040191, 97.35934147644944403, -40.96444954319694887 ) ) ;
#17610 = CARTESIAN_POINT ( 'NONE',  ( -129.4098618459772183, 48.85263848239744533, -22.19798343946113306 ) ) ;
#17611 = PLANE ( 'NONE',  #8718 ) ;
#17612 = DIRECTION ( 'NONE',  ( -0.000000000000000000, -0.000000000000000000, 1.000000000000000000 ) ) ;
#17613 = ORIENTED_EDGE ( 'NONE', *, *, #66169, .F. ) ;
#17614 = DIRECTION ( 'NONE',  ( -0.7530714660036196273, 0.6579387259397027066, 0.000000000000000000 ) ) ;
#17615 = FACE_OUTER_BOUND ( 'NONE', #45884, .T. ) ;
#17616 = ORIENTED_EDGE ( 'NONE', *, *, #57350, .F. ) ;
#17617 = CARTESIAN_POINT ( 'NONE',  ( -155.7455325080990747, 71.01834415181984639, -38.14091650697321967 ) ) ;
#17618 = DIRECTION ( 'NONE',  ( 0.9362348706397417564, -0.3513748240813305279, 0.000000000000000000 ) ) ;
#17619 = CARTESIAN_POINT ( 'NONE',  ( -173.9617926765113509, 89.58633395456782011, 72.63082148245895553 ) ) ;
#17620 = CARTESIAN_POINT ( 'NONE',  ( -142.0729208125266609, 59.40063722436772053, -14.33066429808441455 ) ) ;
#17621 = DIRECTION ( 'NONE',  ( 0.000000000000000000, 0.000000000000000000, 1.000000000000000000 ) ) ;
#17622 = LINE ( 'NONE', #61233, #5173 ) ;
#17623 = DIRECTION ( 'NONE',  ( 0.000000000000000000, 0.000000000000000000, 1.000000000000000000 ) ) ;
#17624 = CARTESIAN_POINT ( 'NONE',  ( 114.7429971699385192, 21.94267019860760470, -1.616224894600706952 ) ) ;
#17625 = EDGE_CURVE ( 'NONE', #39196, #66387, #66888, .T. ) ;
#17626 = CYLINDRICAL_SURFACE ( 'NONE', #6955, 5.000000000000004441 ) ;
#17627 = ADVANCED_FACE ( 'NONE', ( #8140 ), #29583, .T. ) ;
#17628 = CARTESIAN_POINT ( 'NONE',  ( -12.77550690612892481, 8.273784096785062658, 31.96002631522175363 ) ) ;
#17630 = EDGE_CURVE ( 'NONE', #20617, #14760, #51897, .T. ) ;
#17629 = CARTESIAN_POINT ( 'NONE',  ( 117.4830770399667728, 32.37795270233550582, 12.29057018420397540 ) ) ;
#17631 = CARTESIAN_POINT ( 'NONE',  ( -51.01327085356715685, 14.67279453898819774, -90.08252356086848067 ) ) ;
#17632 = VERTEX_POINT ( 'NONE', #57026 ) ;
#17633 = CONICAL_SURFACE ( 'NONE', #26609, 65.00000000000000000, 0.7853981633974497223 ) ;
#17634 = CARTESIAN_POINT ( 'NONE',  ( -98.68609963468200874, 32.11186931716878945, -35.91459565328016623 ) ) ;
#17635 = ORIENTED_EDGE ( 'NONE', *, *, #14292, .T. ) ;
#17636 = CYLINDRICAL_SURFACE ( 'NONE', #14969, 7.500000000000020428 ) ;
#17637 = EDGE_CURVE ( 'NONE', #68404, #3111, #47517, .T. ) ;
#17638 = CARTESIAN_POINT ( 'NONE',  ( 81.74250361646205931, 18.86685472882136949, -64.45562340701054893 ) ) ;
#17639 = VECTOR ( 'NONE', #43849, 1000.000000000000000 ) ;
#17640 = CARTESIAN_POINT ( 'NONE',  ( 117.6852192568308197, 33.60745169181582526, 91.79304235087180075 ) ) ;
#17641 = FACE_OUTER_BOUND ( 'NONE', #12191, .T. ) ;
#17642 = CARTESIAN_POINT ( 'NONE',  ( -2.609024107869115977E-14, 3.000000000000030198, -46.99999999999997158 ) ) ;
#17643 = CARTESIAN_POINT ( 'NONE',  ( -25.49247221749738301, 9.706368398275721177, -38.22028984111819483 ) ) ;
#17644 = DIRECTION ( 'NONE',  ( 0.000000000000000000, -0.000000000000000000, -1.000000000000000000 ) ) ;
#17646 = VECTOR ( 'NONE', #67327, 1000.000000000000000 ) ;
#17645 = DIRECTION ( 'NONE',  ( 1.000000000000000000, 0.000000000000000000, 0.000000000000000000 ) ) ;
#17647 = CARTESIAN_POINT ( 'NONE',  ( -121.5680658099883829, 44.89994870382101055, -21.71427755356253897 ) ) ;
#17648 = ORIENTED_EDGE ( 'NONE', *, *, #58052, .T. ) ;
#17649 = ORIENTED_EDGE ( 'NONE', *, *, #57077, .T. ) ;
#17650 = CARTESIAN_POINT ( 'NONE',  ( -5.000000000000058620, -31.11269837220806878, 0.000000000000000000 ) ) ;
#17651 = CARTESIAN_POINT ( 'NONE',  ( 177.0075766083212443, 74.58167636505953624, 57.35343608575345797 ) ) ;
#17652 = DIRECTION ( 'NONE',  ( -0.000000000000000000, -0.000000000000000000, -1.000000000000000000 ) ) ;
#17653 = CARTESIAN_POINT ( 'NONE',  ( -169.8972248494843313, 85.08697738648015729, 71.95279267074467100 ) ) ;
#17654 = AXIS2_PLACEMENT_3D ( 'NONE', #20544, #52896, #63471 ) ;
#17655 = CARTESIAN_POINT ( 'NONE',  ( -165.6404838346739155, 80.60836113891888033, -14.74958753143211077 ) ) ;
#17656 = DIRECTION ( 'NONE',  ( -0.8160245890732938934, -0.5780171883497599028, 0.000000000000000000 ) ) ;
#17657 = VERTEX_POINT ( 'NONE', #55985 ) ;
#17658 = EDGE_CURVE ( 'NONE', #366, #66548, #7797, .T. ) ;
#17659 = ADVANCED_FACE ( 'NONE', ( #57365 ), #26050, .T. ) ;
#17660 = CARTESIAN_POINT ( 'NONE',  ( 104.7042813665017746, 27.49927371769996753, -38.34174927681518597 ) ) ;
#17661 = CARTESIAN_POINT ( 'NONE',  ( -13.78709718204647139, 7.352743657744180261, 59.88331151981780209 ) ) ;
#17662 = CARTESIAN_POINT ( 'NONE',  ( 3.000000000000004441, 2.999999999999969802, -50.00000000000000000 ) ) ;
#17663 = CARTESIAN_POINT ( 'NONE',  ( 63.74253542338308165, -39.54050679744447905, 43.58025477438756212 ) ) ;
#17664 = DIRECTION ( 'NONE',  ( -0.000000000000000000, -0.000000000000000000, 1.000000000000000000 ) ) ;
#17665 = CARTESIAN_POINT ( 'NONE',  ( 206.7099580236349254, 109.1417833474364301, -9.744738879524000197 ) ) ;
#17666 = FACE_BOUND ( 'NONE', #30682, .T. ) ;
#17667 = EDGE_CURVE ( 'NONE', #28478, #25024, #15828, .T. ) ;
#17668 = CARTESIAN_POINT ( 'NONE',  ( -450.6627218934913230, 177.8591479523843475, 78.55029585798814651 ) ) ;
#17669 = ORIENTED_EDGE ( 'NONE', *, *, #7254, .F. ) ;
#17670 = CARTESIAN_POINT ( 'NONE',  ( 8.828807734114020533, 74.48902371486721563, 170.0000000000000000 ) ) ;
#17671 = DIRECTION ( 'NONE',  ( -0.000000000000000000, 0.001173758924898823768, 0.9999993111447559313 ) ) ;
#17672 = DIRECTION ( 'NONE',  ( 0.000000000000000000, 1.000000000000000000, -0.000000000000000000 ) ) ;
#17673 = CARTESIAN_POINT ( 'NONE',  ( -173.1211646369891355, 88.63826465341151106, 3.977144016177345254 ) ) ;
#17674 = CARTESIAN_POINT ( 'NONE',  ( 212.0779786303465926, 118.9010947973413579, 62.17465067857224881 ) ) ;
#17675 = CARTESIAN_POINT ( 'NONE',  ( -4.681481898397006347, 6.534749472788140778, 5.780152832063345514E-15 ) ) ;
#17676 = CIRCLE ( 'NONE', #49075, 65.00000000000000000 ) ;
#17677 = ORIENTED_EDGE ( 'NONE', *, *, #54218, .T. ) ;
#17678 = CARTESIAN_POINT ( 'NONE',  ( 57.07734607129818016, 11.37318329671160377, 5.860985816944734417 ) ) ;
#17679 = DIRECTION ( 'NONE',  ( -0.000000000000000000, -0.000000000000000000, -1.000000000000000000 ) ) ;
#17680 = EDGE_LOOP ( 'NONE', ( #14190, #12567, #57398, #24199, #58595, #12975, #31349, #24377 ) ) ;
#17681 =( BOUNDED_CURVE ( )  B_SPLINE_CURVE ( 3, ( #21262, #42030, #47636, #27223 ),
 .UNSPECIFIED., .F., .F. ) 
 B_SPLINE_CURVE_WITH_KNOTS ( ( 4, 4 ),
 ( 2.506209174768083692, 3.034697867209401601 ),
 .UNSPECIFIED. ) 
 CURVE ( )  GEOMETRIC_REPRESENTATION_ITEM ( )  RATIONAL_B_SPLINE_CURVE ( ( 1.000000000000000000, 0.9768600920338827986, 0.9768600920338827986, 1.000000000000000000 ) ) 
 REPRESENTATION_ITEM ( '' )  );
#17683 = FACE_OUTER_BOUND ( 'NONE', #37687, .T. ) ;
#17682 = AXIS2_PLACEMENT_3D ( 'NONE', #44552, #28726, #2004 ) ;
#17684 = ORIENTED_EDGE ( 'NONE', *, *, #16682, .T. ) ;
#17685 = CARTESIAN_POINT ( 'NONE',  ( 0.7145311798163268557, -9.237604307034018802, 5.946466066724412554E-16 ) ) ;
#17686 = CARTESIAN_POINT ( 'NONE',  ( -55.05276343752910151, -170.0000000000000000, -69.56087458892355357 ) ) ;
#17687 = CARTESIAN_POINT ( 'NONE',  ( 109.7774723066848424, 28.66666416591278832, 29.61121420573730489 ) ) ;
#17688 = ORIENTED_EDGE ( 'NONE', *, *, #16902, .F. ) ;
#17689 = AXIS2_PLACEMENT_3D ( 'NONE', #48586, #6041, #63769 ) ;
#17690 = MANIFOLD_SOLID_BREP ( 'HeadFillet', #55266 ) ;
#17691 = ORIENTED_EDGE ( 'NONE', *, *, #55587, .T. ) ;
#17692 = CARTESIAN_POINT ( 'NONE',  ( 36.99625334683020128, 8.108440754877195289, -23.39589001747485497 ) ) ;
#17693 = CARTESIAN_POINT ( 'NONE',  ( 164.9547823171479877, 65.03046442419433504, 36.34978599136820776 ) ) ;
#17694 = VECTOR ( 'NONE', #63460, 1000.000000000000000 ) ;
#17695 = CARTESIAN_POINT ( 'NONE',  ( -156.4797890011541597, 71.69341087347113728, -71.93454050753067008 ) ) ;
#17696 = PLANE ( 'NONE',  #64303 ) ;
#17697 = CARTESIAN_POINT ( 'NONE',  ( 87.59061758233885087, 19.75077892934018919, 44.66581936989094004 ) ) ;
#17698 = VECTOR ( 'NONE', #27453, 1000.000000000000000 ) ;
#17699 = CARTESIAN_POINT ( 'NONE',  ( -54.57263979903870421, 15.59415114099632049, -50.21632399845990591 ) ) ;
#17700 = AXIS2_PLACEMENT_3D ( 'NONE', #38029, #5659, #59473 ) ;
#17701 = ADVANCED_FACE ( 'NONE', ( #63681 ), #5274, .T. ) ;
#17702 = CARTESIAN_POINT ( 'NONE',  ( -49.43836229152577744, 14.28302414152159905, 5.975335436052684912 ) ) ;
#17703 = CARTESIAN_POINT ( 'NONE',  ( -132.9227230387960788, 52.53474289881226156, -12.93935600963513721 ) ) ;
#17704 = LINE ( 'NONE', #44780, #4884 ) ;
#17705 = DIRECTION ( 'NONE',  ( 1.000000000000000000, 0.000000000000000000, 0.000000000000000000 ) ) ;
#17706 = DIRECTION ( 'NONE',  ( 0.000000000000000000, 0.000000000000000000, 1.000000000000000000 ) ) ;
#17708 = ORIENTED_EDGE ( 'NONE', *, *, #68531, .F. ) ;
#17707 = LINE ( 'NONE', #2226, #45621 ) ;
#17709 = ORIENTED_EDGE ( 'NONE', *, *, #35255, .T. ) ;
#17710 = ORIENTED_EDGE ( 'NONE', *, *, #9935, .F. ) ;
#17711 = B_SPLINE_CURVE_WITH_KNOTS ( 'NONE', 3,
 ( #19043, #35922, #62992, #30642, #19387, #46117, #4259, #9883, #40845, #36262, #52763, #4589, #47150, #68613, #56679, #20420, #67588, #62302, #35576, #41884, #63341, #15153, #36611, #58064, #26741, #37631, #42227, #32369, #27072, #10202, #5232, #15836, #53451, #37280, #53106, #58730, #21454, #59427, #38323, #48510, #59768, #10549, #11239, #31671, #5960, #64718 ),
 .UNSPECIFIED., .F., .F.,
 ( 4, 2, 2, 2, 2, 2, 2, 2, 2, 2, 2, 2, 2, 2, 2, 2, 2, 2, 2, 2, 2, 2, 4 ),
 ( 0.000000000000000000, 0.003373244802897285618, 0.004216556003621607131, 0.005059867204345928210, 0.006746489605794571236, 0.007589800806518892315, 0.008433112007243214261, 0.009276423207967534473, 0.01011973440869185642, 0.01180635681014048990, 0.01349297921158912339, 0.01433629041231343146, 0.01517960161303773606, 0.01686622401448635220, 0.01770953521521063945, 0.01855284641593493364, 0.02023946881738356018, 0.02108278001810784397, 0.02192609121883212428, 0.02361271362028066756, 0.02445602482100491318, 0.02529933602172915880, 0.02698595842317764310 ),
 .UNSPECIFIED. ) ;
#17712 = CARTESIAN_POINT ( 'NONE',  ( -74.99999999999998579, 0.000000000000000000, 85.00000000000000000 ) ) ;
#17713 = CARTESIAN_POINT ( 'NONE',  ( -175.2570726302115247, 91.06836304649893066, 84.80383358225134316 ) ) ;
#17714 = CYLINDRICAL_SURFACE ( 'NONE', #64840, 5.000000000000170530 ) ;
#17715 = PLANE ( 'NONE',  #51236 ) ;
#17716 = EDGE_CURVE ( 'NONE', #1146, #44628, #14458, .T. ) ;
#17717 = CARTESIAN_POINT ( 'NONE',  ( -32.41898580403142205, 10.77423026598439648, 72.01293556506519167 ) ) ;
#17718 = CARTESIAN_POINT ( 'NONE',  ( 16.62148331457488837, 18.83783649008728744, 0.000000000000000000 ) ) ;
#17719 = CARTESIAN_POINT ( 'NONE',  ( -71.26675986148646302, 19.63956187826083166, -68.21173518103694278 ) ) ;
#17720 = DIRECTION ( 'NONE',  ( 1.000000000000000000, 1.748184826783646563E-16, 0.000000000000000000 ) ) ;
#17721 = ORIENTED_EDGE ( 'NONE', *, *, #66260, .T. ) ;
#17722 = CARTESIAN_POINT ( 'NONE',  ( 0.000000000000000000, 0.000000000000000000, -9.500000000000000000 ) ) ;
#17723 = ORIENTED_EDGE ( 'NONE', *, *, #17216, .T. ) ;
#17724 = ADVANCED_FACE ( 'NONE', ( #46806 ), #4252, .F. ) ;
#17725 = ORIENTED_EDGE ( 'NONE', *, *, #19769, .F. ) ;
#17726 = EDGE_CURVE ( 'NONE', #36414, #4077, #60120, .T. ) ;
#17727 = CARTESIAN_POINT ( 'NONE',  ( -146.1201263095600780, 62.66021356509621398, 18.07158695027811035 ) ) ;
#17728 = FACE_OUTER_BOUND ( 'NONE', #19222, .T. ) ;
#17729 = CARTESIAN_POINT ( 'NONE',  ( -166.0012244511291328, 80.97916541034756222, 35.94679821911269357 ) ) ;
#17730 = FACE_OUTER_BOUND ( 'NONE', #10068, .T. ) ;
#17731 = EDGE_CURVE ( 'NONE', #30832, #56795, #50739, .T. ) ;
#17733 = LINE ( 'NONE', #59919, #23677 ) ;
#17732 = CIRCLE ( 'NONE', #3739, 243.4957430088094839 ) ;
#17734 = DIRECTION ( 'NONE',  ( 0.000000000000000000, 0.000000000000000000, 1.000000000000000000 ) ) ;
#17735 = CARTESIAN_POINT ( 'NONE',  ( 140.7888851157409817, 46.97220912571249585, -13.80429249087656451 ) ) ;
#17736 = ORIENTED_EDGE ( 'NONE', *, *, #14636, .T. ) ;
#17737 = ORIENTED_EDGE ( 'NONE', *, *, #49048, .F. ) ;
#17738 = VERTEX_POINT ( 'NONE', #41878 ) ;
#17739 = AXIS2_PLACEMENT_3D ( 'NONE', #33762, #17208, #49919 ) ;
#17740 = PLANE ( 'NONE',  #9125 ) ;
#17741 = CARTESIAN_POINT ( 'NONE',  ( -14.76369756425704161, 7.442560416198674034, 13.65010214637367447 ) ) ;
#17742 = CARTESIAN_POINT ( 'NONE',  ( 2.905661822261151883E-14, 15.55634918610403084, 2.000000000000001776 ) ) ;
#17743 = CARTESIAN_POINT ( 'NONE',  ( 55.57657751403271362, 11.06944050856662187, -17.36232739209965459 ) ) ;
#17744 = UNCERTAINTY_MEASURE_WITH_UNIT (LENGTH_MEASURE( 1.000000000000000082E-05 ), #46815, 'distance_accuracy_value', 'NONE');
#17745 = CARTESIAN_POINT ( 'NONE',  ( -47.61380558691495679, 12.81230778489787703, 38.80435849991815189 ) ) ;
#17746 = CARTESIAN_POINT ( 'NONE',  ( 198.7129816317746247, 100.1061386900356069, 68.08044006511057944 ) ) ;
#17747 = ORIENTED_EDGE ( 'NONE', *, *, #33006, .F. ) ;
#17748 = MECHANICAL_DESIGN_GEOMETRIC_PRESENTATION_REPRESENTATION (  '', ( #58158 ), #57014 ) ;
#17749 = CARTESIAN_POINT ( 'NONE',  ( -62.15063206372443005, 17.75106610013996189, -72.03382600977727179 ) ) ;
#17750 = CARTESIAN_POINT ( 'NONE',  ( 198.4045886930829568, 99.71425793793704884, -74.75928238610738674 ) ) ;
#17751 = CARTESIAN_POINT ( 'NONE',  ( 279.6700404598698242, -21.42428528562853529, -4.999999999999990230 ) ) ;
#17752 = CARTESIAN_POINT ( 'NONE',  ( -168.7150276173047700, 82.35404041280325771, 17.56479690237895142 ) ) ;
#17753 = LINE ( 'NONE', #13173, #364 ) ;
#17755 = EDGE_CURVE ( 'NONE', #34426, #55546, #62984, .T. ) ;
#17754 = FACE_BOUND ( 'NONE', #57706, .T. ) ;
#17756 = CARTESIAN_POINT ( 'NONE',  ( -189.6160969562817229, 107.6113660112011843, 89.72857030643531573 ) ) ;
#17757 = AXIS2_PLACEMENT_3D ( 'NONE', #6812, #53597, #6108 ) ;
#17758 = ORIENTED_EDGE ( 'NONE', *, *, #13797, .T. ) ;
#17759 = CARTESIAN_POINT ( 'NONE',  ( -56.44201257846587083, -32.26641783793643725, 43.58025477438756923 ) ) ;
#17760 = CARTESIAN_POINT ( 'NONE',  ( 179.4279766878530609, 76.94722012158234747, 29.48164326234083887 ) ) ;
#17761 = CARTESIAN_POINT ( 'NONE',  ( -104.7956873821849086, 35.21322275870667795, -76.42854020113006186 ) ) ;
#17762 = CARTESIAN_POINT ( 'NONE',  ( 44.35071890818839790, 9.104600422692254114, -64.30759515882533606 ) ) ;
#17763 = LINE ( 'NONE', #39217, #59096 ) ;
#17764 = ORIENTED_EDGE ( 'NONE', *, *, #28676, .T. ) ;
#17765 = EDGE_LOOP ( 'NONE', ( #2901, #50975 ) ) ;
#17766 = CARTESIAN_POINT ( 'NONE',  ( -132.7866146733880726, 51.20302913291856584, -93.10660668597851952 ) ) ;
#17767 = CARTESIAN_POINT ( 'NONE',  ( 188.0368405038881860, 85.93000590718348519, 87.66130298660245046 ) ) ;
#17768 = EDGE_LOOP ( 'NONE', ( #60113, #17227, #58862, #42747, #60664, #7768 ) ) ;
#17769 = ORIENTED_EDGE ( 'NONE', *, *, #41809, .F. ) ;
#17770 = LINE ( 'NONE', #22342, #1576 ) ;
#17771 = CARTESIAN_POINT ( 'NONE',  ( 150.7770046255793090, 53.87214803240242844, 40.30350261447307503 ) ) ;
#17772 = FACE_OUTER_BOUND ( 'NONE', #51618, .T. ) ;
#17773 = ORIENTED_EDGE ( 'NONE', *, *, #25587, .F. ) ;
#17774 = DIRECTION ( 'NONE',  ( 0.000000000000000000, -1.000000000000000000, 0.000000000000000000 ) ) ;
#17775 = CARTESIAN_POINT ( 'NONE',  ( -173.1211646369891071, 87.12891641440859303, 3.977144016177345254 ) ) ;
#17776 = CARTESIAN_POINT ( 'NONE',  ( 50.97490815085634352, 6.000000000000000000, -4.435653166495503896 ) ) ;
#17777 = CARTESIAN_POINT ( 'NONE',  ( -447.6627218934912662, 389.9999999999998295, 113.5502958579881465 ) ) ;
#17778 = CARTESIAN_POINT ( 'NONE',  ( 21.66908387089111443, 6.759772951853439515, -91.97708651838377136 ) ) ;
#17779 = EDGE_CURVE ( 'NONE', #52894, #61203, #12292, .T. ) ;
#17780 = CARTESIAN_POINT ( 'NONE',  ( -189.5329886872043232, 107.4958891766010964, 36.29115481271927734 ) ) ;
#17781 = ADVANCED_FACE ( 'NONE', ( #47478 ), #69291, .T. ) ;
#17782 = EDGE_CURVE ( 'NONE', #20616, #25774, #21118, .T. ) ;
#17783 = ORIENTED_EDGE ( 'NONE', *, *, #50041, .T. ) ;
#17784 = CIRCLE ( 'NONE', #9950, 65.36598343705435354 ) ;
#17785 = CARTESIAN_POINT ( 'NONE',  ( 21.38432669263065833, -61.76910524360950916, 43.58025477438756212 ) ) ;
#17786 = EDGE_CURVE ( 'NONE', #41171, #24590, #53784, .T. ) ;
#17787 = CARTESIAN_POINT ( 'NONE',  ( -78.19438069111008360, 23.21811806230640229, 3.573650549209444804 ) ) ;
#17788 = CARTESIAN_POINT ( 'NONE',  ( -148.0058283997320814, 64.22864592525513672, -49.66416448871609646 ) ) ;
#17789 = VECTOR ( 'NONE', #12479, 1000.000000000000114 ) ;
#17790 = CARTESIAN_POINT ( 'NONE',  ( -167.1619226259399227, 82.18315278115416334, -73.61743746788761200 ) ) ;
#17792 = VERTEX_POINT ( 'NONE', #16166 ) ;
#17791 = CARTESIAN_POINT ( 'NONE',  ( 126.6904219525097659, -170.0000000000000000, -95.00000000000133582 ) ) ;
#17793 = CARTESIAN_POINT ( 'NONE',  ( 79.19132716134487282, 17.01584750883626995, -44.31649721339067582 ) ) ;
#17794 = EDGE_CURVE ( 'NONE', #64838, #18961, #5949, .T. ) ;
#17795 = ORIENTED_EDGE ( 'NONE', *, *, #28573, .F. ) ;
#17796 = CARTESIAN_POINT ( 'NONE',  ( 26.12852347772543737, 70.00000000000000000, 129.5802547743875550 ) ) ;
#17797 = DIRECTION ( 'NONE',  ( -0.000000000000000000, 1.000000000000000000, -0.000000000000000000 ) ) ;
#17798 = DIRECTION ( 'NONE',  ( 0.000000000000000000, 0.000000000000000000, 1.000000000000000000 ) ) ;
#17799 = CARTESIAN_POINT ( 'NONE',  ( 187.2354698746857196, 85.05376776489252677, -21.20039874324467988 ) ) ;
#17800 = CARTESIAN_POINT ( 'NONE',  ( -72.99999999999998579, 0.000000000000000000, 25.70156211871649887 ) ) ;
#17801 = LINE ( 'NONE', #7243, #14031 ) ;
#17802 = CARTESIAN_POINT ( 'NONE',  ( 94.07616572255072640, 22.09777530676766943, -71.19049505762396279 ) ) ;
#17803 = CARTESIAN_POINT ( 'NONE',  ( -31.43908319763710679, 10.61114334766715928, -35.31719736520183517 ) ) ;
#17804 = VERTEX_POINT ( 'NONE', #43234 ) ;
#17805 = ADVANCED_FACE ( 'NONE', ( #12291 ), #27063, .T. ) ;
#17806 = ORIENTED_EDGE ( 'NONE', *, *, #5955, .T. ) ;
#17807 = EDGE_CURVE ( 'NONE', #62528, #42408, #59759, .T. ) ;
#17808 = MANIFOLD_SOLID_BREP ( 'Cut-Extrude1[3]', #67631 ) ;
#17809 = CARTESIAN_POINT ( 'NONE',  ( 42.71504753277077526, 8.863481902720392824, 44.14684118498996668 ) ) ;
#17810 = CARTESIAN_POINT ( 'NONE',  ( 197.8436586345019919, 97.39326576892290177, -20.07941126599159887 ) ) ;
#17811 = CARTESIAN_POINT ( 'NONE',  ( 54.99999999999995026, 0.000000000000000000, 0.000000000000000000 ) ) ;
#17812 = CYLINDRICAL_SURFACE ( 'NONE', #40787, 245.3095347406802205 ) ;
#17813 = CARTESIAN_POINT ( 'NONE',  ( 212.0104729185452186, 118.7959000526603148, -42.12969124680917332 ) ) ;
#17814 = CARTESIAN_POINT ( 'NONE',  ( -71.97658551692138929, 20.95070248419150261, -72.85986904017757126 ) ) ;
#17815 = LINE ( 'NONE', #40302, #46079 ) ;
#17816 = CARTESIAN_POINT ( 'NONE',  ( -29.75049355503753645, 9.320234381800286627, -50.12873137353120256 ) ) ;
#17817 = DIRECTION ( 'NONE',  ( -0.000000000000000000, 0.000000000000000000, -1.000000000000000000 ) ) ;
#17818 = VERTEX_POINT ( 'NONE', #42889 ) ;
#17819 = ORIENTED_EDGE ( 'NONE', *, *, #7117, .T. ) ;
#17820 = DIRECTION ( 'NONE',  ( 1.000000000000000000, 0.000000000000000000, 0.000000000000000000 ) ) ;
#17821 = DIRECTION ( 'NONE',  ( 0.000000000000000000, 0.000000000000000000, 1.000000000000000000 ) ) ;
#17822 = CARTESIAN_POINT ( 'NONE',  ( -86.09999398724994535, 25.29376521564880065, 65.79117337328426629 ) ) ;
#17823 = LINE ( 'NONE', #61074, #45554 ) ;
#17824 = CARTESIAN_POINT ( 'NONE',  ( -15.45727656667689409, 73.34020256436167529, 41.38025477438755928 ) ) ;
#17825 = CARTESIAN_POINT ( 'NONE',  ( 0.000000000000000000, 0.000000000000000000, -3.000000000000030198 ) ) ;
#17826 = DIRECTION ( 'NONE',  ( 2.241020959626597081E-17, 2.489978219820159838E-16, 1.000000000000000000 ) ) ;
#17827 = CARTESIAN_POINT ( 'NONE',  ( -35.00000000000000000, -35.00000000000000000, 2.000000000000000000 ) ) ;
#17828 = CARTESIAN_POINT ( 'NONE',  ( 45.18191557310396433, 9.231730719146584718, 86.31199235815032011 ) ) ;
#17829 = LINE ( 'NONE', #60729, #44345 ) ;
#17830 = ORIENTED_EDGE ( 'NONE', *, *, #22083, .F. ) ;
#17831 = CARTESIAN_POINT ( 'NONE',  ( 0.000000000000000000, 0.000000000000000000, 0.000000000000000000 ) ) ;
#17832 =( LENGTH_UNIT ( ) NAMED_UNIT ( * ) SI_UNIT ( .MILLI., .METRE. ) );
#17833 = CARTESIAN_POINT ( 'NONE',  ( -11.14668121284976010, 8.139398342256731311, 17.50002341736112399 ) ) ;
#17834 = CARTESIAN_POINT ( 'NONE',  ( 284.8388622179743948, -21.96384902133207362, 1.301157935232950980 ) ) ;
#17835 = CARTESIAN_POINT ( 'NONE',  ( 209.9999999999999716, -57.00000000000007816, 93.99999999999998579 ) ) ;
#17836 = CARTESIAN_POINT ( 'NONE',  ( 126.7877523219523255, 38.47018873135925077, -14.11887035946164204 ) ) ;
#17837 = AXIS2_PLACEMENT_3D ( 'NONE', #23048, #1953, #38166 ) ;
#17838 = VERTEX_POINT ( 'NONE', #11574 ) ;
#17839 =( NAMED_UNIT ( * ) SI_UNIT ( $, .STERADIAN. ) SOLID_ANGLE_UNIT ( ) );
#17840 = DIRECTION ( 'NONE',  ( 0.000000000000000000, 0.000000000000000000, 1.000000000000000000 ) ) ;
#17841 = CARTESIAN_POINT ( 'NONE',  ( -35.17718245314462422, 11.25729435722175786, -36.31055870647146833 ) ) ;
#17842 = CARTESIAN_POINT ( 'NONE',  ( -169.1122507277982834, 84.24359299875008844, -48.56609460568329695 ) ) ;
#17843 = AXIS2_PLACEMENT_3D ( 'NONE', #23168, #60786, #23518 ) ;
#17844 = CONTEXT_DEPENDENT_SHAPE_REPRESENTATION ( #68740, #9215 ) ;
#17845 = CARTESIAN_POINT ( 'NONE',  ( -21.27554331372911989, -61.43430442924893953, 3.061616997868437868E-16 ) ) ;
#17846 = ORIENTED_EDGE ( 'NONE', *, *, #13433, .F. ) ;
#17847 = CARTESIAN_POINT ( 'NONE',  ( -118.3960663196801306, 41.75130200162921312, -42.98165142137420958 ) ) ;
#17848 = DIRECTION ( 'NONE',  ( -1.000000000000000000, 0.000000000000000000, 1.734723475976805517E-15 ) ) ;
#17849 = CARTESIAN_POINT ( 'NONE',  ( -146.5341851369305743, 61.69744206542952014, -22.36787375243187981 ) ) ;
#17850 = CARTESIAN_POINT ( 'NONE',  ( -3.862560291631544018, 7.672660553664876204, -76.13487047467812374 ) ) ;
#17851 = DIRECTION ( 'NONE',  ( -0.000000000000000000, 1.000000000000000000, -0.000000000000000000 ) ) ;
#17852 = VERTEX_POINT ( 'NONE', #44283 ) ;
#17853 = CARTESIAN_POINT ( 'NONE',  ( -102.2801239173131194, -170.0000000000000000, -69.35912785543959558 ) ) ;
#17854 = CARTESIAN_POINT ( 'NONE',  ( 199.3743599161302882, 99.31857334527873604, -38.51805329884761164 ) ) ;
#17855 = DIRECTION ( 'NONE',  ( -4.974206872490789458E-18, 1.135330258912604340E-18, -1.000000000000000000 ) ) ;
#17856 = CARTESIAN_POINT ( 'NONE',  ( 21.42484406671928809, 6.746536496442158359, -47.97273126929388809 ) ) ;
#17858 = ORIENTED_EDGE ( 'NONE', *, *, #53236, .F. ) ;
#17857 = CARTESIAN_POINT ( 'NONE',  ( 117.6924004117966689, 33.61107268965020722, 9.252808361665987746 ) ) ;
#17859 = DIRECTION ( 'NONE',  ( -0.000000000000000000, -0.000000000000000000, -1.000000000000000000 ) ) ;
#17860 = EDGE_CURVE ( 'NONE', #37583, #1914, #57591, .T. ) ;
#17861 = VERTEX_POINT ( 'NONE', #39721 ) ;
#17862 = ORIENTED_EDGE ( 'NONE', *, *, #52723, .F. ) ;
#17863 = CARTESIAN_POINT ( 'NONE',  ( -125.8938041572051105, 46.49392987655493670, -88.60280507916129977 ) ) ;
#17864 = EDGE_CURVE ( 'NONE', #64513, #69562, #9747, .T. ) ;
#17865 = DIRECTION ( 'NONE',  ( 1.000000000000000000, -0.000000000000000000, 0.000000000000000000 ) ) ;
#17867 = ORIENTED_EDGE ( 'NONE', *, *, #36948, .F. ) ;
#17866 = FACE_OUTER_BOUND ( 'NONE', #67352, .T. ) ;
#17868 = CARTESIAN_POINT ( 'NONE',  ( 163.2886151008987667, 62.32020850087170061, 32.17011112544247453 ) ) ;
#17869 = EDGE_CURVE ( 'NONE', #52056, #41640, #43996, .T. ) ;
#17871 = CIRCLE ( 'NONE', #53788, 5.000000000000004441 ) ;
#17870 = CARTESIAN_POINT ( 'NONE',  ( 0.000000000000000000, 0.000000000000000000, 2.000000000000000000 ) ) ;
#17872 = FACE_BOUND ( 'NONE', #20153, .T. ) ;
#17873 = ORIENTED_EDGE ( 'NONE', *, *, #9597, .F. ) ;
#17874 = CARTESIAN_POINT ( 'NONE',  ( 173.9832054143776077, 73.09312616907610050, -95.00000000000133582 ) ) ;
#17875 = CARTESIAN_POINT ( 'NONE',  ( -35.17686701826945495, 10.23452050416467962, -9.452137265833972180 ) ) ;
#17876 = CARTESIAN_POINT ( 'NONE',  ( 112.5537757279407316, 31.07998172410697180, 44.26225647685382114 ) ) ;
#17877 = DIRECTION ( 'NONE',  ( -0.000000000000000000, 1.000000000000000000, -0.000000000000000000 ) ) ;
#17878 = CARTESIAN_POINT ( 'NONE',  ( 19.10949903373830594, 7.636938177523838078, 57.63021761123498266 ) ) ;
#17879 = EDGE_CURVE ( 'NONE', #25774, #37010, #1396, .T. ) ;
#17880 = ORIENTED_EDGE ( 'NONE', *, *, #15387, .T. ) ;
#17881 = AXIS2_PLACEMENT_3D ( 'NONE', #58938, #5817, #27628 ) ;
#17882 = ORIENTED_EDGE ( 'NONE', *, *, #60011, .F. ) ;
#17883 = EDGE_LOOP ( 'NONE', ( #37970, #45888, #31388, #36630 ) ) ;
#17884 = CARTESIAN_POINT ( 'NONE',  ( 210.5151926960689366, 114.6764308336227600, -92.77687245054279686 ) ) ;
#17885 = CIRCLE ( 'NONE', #4384, 5.000000000000004441 ) ;
#17886 = CARTESIAN_POINT ( 'NONE',  ( -109.3386876948163859, 37.66246927061209249, 8.589132535061098750 ) ) ;
#17887 = CARTESIAN_POINT ( 'NONE',  ( -49.42000000000000171, -36.09918303830819752, 10.41169613715280740 ) ) ;
#17888 = B_SPLINE_CURVE_WITH_KNOTS ( 'NONE', 3,
 ( #52897, #20545, #41669, #52563, #69070, #52221, #8976, #14254, #63472, #42358, #30426, #46948, #63817, #35361, #63126, #14928, #3349, #4719, #24809, #56821, #46244, #47279, #35713, #36396, #41332, #62786, #68073, #26182, #68732, #47617, #19876, #14590, #57848, #9667, #4387, #25850, #42013, #15285 ),
 .UNSPECIFIED., .F., .F.,
 ( 4, 2, 2, 2, 2, 2, 2, 2, 2, 2, 2, 2, 2, 2, 2, 2, 2, 2, 4 ),
 ( 0.000000000000000000, 0.003908178031105422924, 0.005862267046658093186, 0.007816356062210764316, 0.009770445077763435446, 0.01172453409331610484, 0.01270157860109243607, 0.01367862310886876556, 0.01465566761664509506, 0.01563271212442142455, 0.01660975663219775231, 0.01758680113997408007, 0.01954089015552678762, 0.02051793466330317436, 0.02149497917107956110, 0.02344906818663230683, 0.02540315720218505602, 0.02735724621773780174, 0.03126542424884326543 ),
 .UNSPECIFIED. ) ;
#17889 = CARTESIAN_POINT ( 'NONE',  ( -31.93184248720559637, 9.672312402099827011, -35.31719736520184227 ) ) ;
#17890 = CARTESIAN_POINT ( 'NONE',  ( -106.0165346013910721, 34.71969978529867262, 85.19816686951331519 ) ) ;
#17891 = CARTESIAN_POINT ( 'NONE',  ( -144.7571537022063808, 60.25265659240450589, 32.41201323233473630 ) ) ;
#17892 = CARTESIAN_POINT ( 'NONE',  ( 0.000000000000000000, 70.00000000000000000, 0.000000000000000000 ) ) ;
#17893 = CARTESIAN_POINT ( 'NONE',  ( -71.26746920569854638, 20.70422440535244135, -17.02378192568739479 ) ) ;
#17894 = ORIENTED_EDGE ( 'NONE', *, *, #31767, .F. ) ;
#17895 = CARTESIAN_POINT ( 'NONE',  ( 79.92465405224845654, 17.24122384219593229, 67.45454031577327214 ) ) ;
#17896 = VERTEX_POINT ( 'NONE', #15748 ) ;
#17897 = CARTESIAN_POINT ( 'NONE',  ( 38.90894112122320081, 8.345444037631239098, 44.91383430596326320 ) ) ;
#17898 = SURFACE_SIDE_STYLE ('',( #54818 ) ) ;
#17899 = ORIENTED_EDGE ( 'NONE', *, *, #24220, .F. ) ;
#17900 = DIRECTION ( 'NONE',  ( -1.000000000000000000, 0.000000000000000000, 0.000000000000000000 ) ) ;
#17901 = CARTESIAN_POINT ( 'NONE',  ( -452.6627218934913230, 399.9999999999998295, 113.5502958579881465 ) ) ;
#17902 = FACE_OUTER_BOUND ( 'NONE', #68575, .T. ) ;
#17903 = CARTESIAN_POINT ( 'NONE',  ( 37.70762885381311236, 8.195134395012281914, 17.87944627234856299 ) ) ;
#17904 = DIRECTION ( 'NONE',  ( 0.000000000000000000, 0.000000000000000000, -1.000000000000000000 ) ) ;
#17905 = AXIS2_PLACEMENT_3D ( 'NONE', #34759, #57593, #3097 ) ;
#17906 = CARTESIAN_POINT ( 'NONE',  ( 311.9975424824652350, 20.00000000000003197, 256.6193948016162381 ) ) ;
#17907 = DIRECTION ( 'NONE',  ( -1.000000000000000000, 0.000000000000000000, 0.000000000000000000 ) ) ;
#17908 = EDGE_LOOP ( 'NONE', ( #68565, #52422, #15256, #14576 ) ) ;
#17909 = CARTESIAN_POINT ( 'NONE',  ( -105.1656308559908410, 34.27066904145148385, -89.26805114713427258 ) ) ;
#17910 = LINE ( 'NONE', #65403, #4895 ) ;
#17911 = ORIENTED_EDGE ( 'NONE', *, *, #1652, .F. ) ;
#17912 = CARTESIAN_POINT ( 'NONE',  ( 1.310872448937988821, -8.480771745766432446, -9.182649155111331396 ) ) ;
#17913 = DIRECTION ( 'NONE',  ( 1.000000000000000000, 0.000000000000000000, 0.000000000000000000 ) ) ;
#17914 = PLANE ( 'NONE',  #53266 ) ;
#17915 = ORIENTED_EDGE ( 'NONE', *, *, #42965, .F. ) ;
#17916 = CARTESIAN_POINT ( 'NONE',  ( -84.97622048504842951, 24.82614411847758262, 33.85642420924052232 ) ) ;
#17917 = DIRECTION ( 'NONE',  ( -1.000000000000000000, -1.001918046209079887E-14, 9.729495617646301779E-15 ) ) ;
#17918 = CARTESIAN_POINT ( 'NONE',  ( 46.23113030541875190, 10.41513832761375902, 40.52388841428868460 ) ) ;
#17919 = CARTESIAN_POINT ( 'NONE',  ( -30.94753041835915042, 9.510749728915506296, 72.06100499665289760 ) ) ;
#17920 = APPLICATION_CONTEXT ( 'automotive_design' ) ;
#17921 = ORIENTED_EDGE ( 'NONE', *, *, #26267, .T. ) ;
#17922 = MANIFOLD_SOLID_BREP ( 'Cut-Extrude4', #1340 ) ;
#17923 = FACE_OUTER_BOUND ( 'NONE', #38591, .T. ) ;
#17924 = ORIENTED_EDGE ( 'NONE', *, *, #64817, .F. ) ;
#17925 = CARTESIAN_POINT ( 'NONE',  ( 32.15284246740099405, 8.588257691344876932, -14.33592182630315293 ) ) ;
#17926 = PLANE ( 'NONE',  #11349 ) ;
#17927 = CARTESIAN_POINT ( 'NONE',  ( -2.177337698256113452, 7.595833446947584555, 15.72975283661752499 ) ) ;
#17928 = EDGE_CURVE ( 'NONE', #964, #347, #59319, .T. ) ;
#17929 = CARTESIAN_POINT ( 'NONE',  ( 139.9539301108215739, 46.42810403146213361, 86.31909232689017131 ) ) ;
#17930 = CARTESIAN_POINT ( 'NONE',  ( -26.06926405629031862, 9.787505506543544342, -91.25298045410747250 ) ) ;
#17931 = LINE ( 'NONE', #44999, #62993 ) ;
#17932 = EDGE_LOOP ( 'NONE', ( #34840, #54443, #53824, #57914 ) ) ;
#17933 = DIRECTION ( 'NONE',  ( 0.000000000000000000, 0.000000000000000000, -1.000000000000000000 ) ) ;
#17934 = AXIS2_PLACEMENT_3D ( 'NONE', #21570, #37400, #5403 ) ;
#17935 = EDGE_LOOP ( 'NONE', ( #14977, #42204, #58935, #65359 ) ) ;
#17936 = CARTESIAN_POINT ( 'NONE',  ( 157.9160637431159842, 57.99786926216935257, -9.279633708673957315 ) ) ;
#17937 = DIRECTION ( 'NONE',  ( -0.000000000000000000, -0.000000000000000000, -1.000000000000000000 ) ) ;
#17938 = FACE_OUTER_BOUND ( 'NONE', #8458, .T. ) ;
#17939 = CARTESIAN_POINT ( 'NONE',  ( -132.1086844338047968, 51.95575954690575315, -91.87852830952506622 ) ) ;
#17940 = LINE ( 'NONE', #22514, #67826 ) ;
#17941 = AXIS2_PLACEMENT_3D ( 'NONE', #4771, #42409, #9720 ) ;
#17942 = VERTEX_POINT ( 'NONE', #21709 ) ;
#17943 = EDGE_CURVE ( 'NONE', #64838, #47377, #60396, .T. ) ;
#17944 = VERTEX_POINT ( 'NONE', #13259 ) ;
#17945 = B_SPLINE_CURVE_WITH_KNOTS ( 'NONE', 3,
 ( #11277, #43282, #64757, #68979, #32746, #38021, #32407, #59466, #10584, #31707, #20807, #42267, #36989, #58428, #4970, #53492, #39416, #50325, #6709, #16905, #34155, #60864, #38365, #7423, #1798, #17968, #65460, #12689, #2143, #60523, #33460, #55590, #22192, #43632, #45034, #28517, #27815, #54535, #66517, #7059, #11989, #54176, #5998, #23253, #1435, #28875, #59810, #6361 ),
 .UNSPECIFIED., .F., .F.,
 ( 4, 2, 2, 2, 2, 2, 2, 2, 2, 2, 2, 2, 2, 2, 2, 2, 2, 2, 2, 2, 2, 2, 2, 4 ),
 ( 0.000000000000000000, 0.001591515129442145314, 0.003183030258884290628, 0.003978787823605363719, 0.004774545388326435942, 0.006366060517768672329, 0.007957575647210907849, 0.009549090776653144236, 0.01034484834137428325, 0.01114060590609542052, 0.01193636347081656127, 0.01273212103553770028, 0.01432363616497998003, 0.01591515129442225632, 0.01671090885914341614, 0.01750666642386457250, 0.01830242398858572886, 0.01909818155330688522, 0.02068969668274922222, 0.02148545424747039245, 0.02228121181219156269, 0.02387272694163382683, 0.02466848450635492421, 0.02546424207107601118 ),
 .UNSPECIFIED. ) ;
#17946 = EDGE_CURVE ( 'NONE', #32357, #23050, #35792, .T. ) ;
#17947 = CARTESIAN_POINT ( 'NONE',  ( 8.288104306525688969, 6.376394648992966374, 37.02812928323293562 ) ) ;
#17948 = ORIENTED_EDGE ( 'NONE', *, *, #4289, .T. ) ;
#17949 = CARTESIAN_POINT ( 'NONE',  ( -62.15799747763099248, 16.70234469631019891, -72.01302682479479245 ) ) ;
#17950 = CARTESIAN_POINT ( 'NONE',  ( 74.62299871641495486, 5.461138973199058277, 170.0000000000000000 ) ) ;
#17951 = ORIENTED_EDGE ( 'NONE', *, *, #47687, .F. ) ;
#17952 = CARTESIAN_POINT ( 'NONE',  ( -142.6264002846223491, 58.55577336362196661, -72.15276126393024470 ) ) ;
#17953 = EDGE_CURVE ( 'NONE', #40777, #45231, #65183, .T. ) ;
#17954 = VECTOR ( 'NONE', #45044, 1000.000000000000000 ) ;
#17955 = CARTESIAN_POINT ( 'NONE',  ( 93.08533330311588827, 21.72562315962718316, 6.518023353393929575 ) ) ;
#17956 = ADVANCED_FACE ( 'NONE', ( #25119 ), #45111, .T. ) ;
#17957 = LINE ( 'NONE', #39066, #49661 ) ;
#17958 = ORIENTED_EDGE ( 'NONE', *, *, #57887, .T. ) ;
#17959 = CARTESIAN_POINT ( 'NONE',  ( 311.9975424824652350, 170.0000000000000284, 536.6193948016162949 ) ) ;
#17960 = CARTESIAN_POINT ( 'NONE',  ( 68.58775259640211175, 15.07340320468039430, 85.97092029086265086 ) ) ;
#17961 = CARTESIAN_POINT ( 'NONE',  ( 26.11269837220800127, -31.11269837220812562, 0.000000000000000000 ) ) ;
#17962 = CARTESIAN_POINT ( 'NONE',  ( -180.2188652555597059, 96.98354576637424884, -44.65256448004029721 ) ) ;
#17963 = CARTESIAN_POINT ( 'NONE',  ( -127.6861178856153174, 47.68458428355324941, -8.272562232425640261 ) ) ;
#17964 = DIRECTION ( 'NONE',  ( 0.000000000000000000, 0.000000000000000000, -1.000000000000000000 ) ) ;
#17965 = DIRECTION ( 'NONE',  ( 1.000000000000000000, 0.000000000000000000, 0.000000000000000000 ) ) ;
#17966 = EDGE_CURVE ( 'NONE', #38367, #62594, #14847, .T. ) ;
#17967 = VERTEX_POINT ( 'NONE', #2614 ) ;
#17968 = CARTESIAN_POINT ( 'NONE',  ( 141.0792860804899362, 47.16255757051794006, -72.45897467894479860 ) ) ;
#17969 = LINE ( 'NONE', #39417, #19754 ) ;
#17970 = ORIENTED_EDGE ( 'NONE', *, *, #59862, .T. ) ;
#17971 = AXIS2_PLACEMENT_3D ( 'NONE', #1360, #16491, #22815 ) ;
#17972 = ADVANCED_FACE ( 'NONE', ( #24076 ), #45519, .T. ) ;
#17973 = ADVANCED_FACE ( 'NONE', ( #11244, #705 ), #26746, .T. ) ;
#17974 = CARTESIAN_POINT ( 'NONE',  ( -156.9919426121902575, 72.16759471857101005, -41.74996328242564658 ) ) ;
#17975 = CARTESIAN_POINT ( 'NONE',  ( -26.83517958587572494, -59.60356471962950309, 43.58025477438756212 ) ) ;
#17976 = CARTESIAN_POINT ( 'NONE',  ( -34.52542994698665524, 11.14027065218092538, 44.55630013575089521 ) ) ;
#17977 = B_SPLINE_CURVE_WITH_KNOTS ( 'NONE', 3,
 ( #7505, #13124, #60602, #7840, #24019, #28958, #39502, #45463, #27898, #65541 ),
 .UNSPECIFIED., .F., .F.,
 ( 4, 2, 2, 2, 4 ),
 ( 0.000000000000000000, 0.002532684671119367868, 0.005065369342238735736, 0.007598054013358103605, 0.01013073868447747147 ),
 .UNSPECIFIED. ) ;
#17978 = CARTESIAN_POINT ( 'NONE',  ( -125.4463376280758666, 47.40387005565908396, -49.90373998702522584 ) ) ;
#17979 = CARTESIAN_POINT ( 'NONE',  ( 41.72486082342750535, 50.31647622756258187, 41.38025477438755928 ) ) ;
#17980 = DIRECTION ( 'NONE',  ( 1.000000000000000000, 0.000000000000000000, 0.000000000000000000 ) ) ;
#17981 = CARTESIAN_POINT ( 'NONE',  ( 204.6977192012829789, 106.3443248447423315, -90.01503221354893469 ) ) ;
#17982 = DIRECTION ( 'NONE',  ( 0.1342332658176522420, 0.9909497617679351444, 0.000000000000000000 ) ) ;
#17983 = CARTESIAN_POINT ( 'NONE',  ( -8.800520192024523070, 7.964629484975260354, 30.16296264417345796 ) ) ;
#17984 = CARTESIAN_POINT ( 'NONE',  ( 115.7561705820728832, 31.51689401996054940, 5.158855458972969821 ) ) ;
#17985 = CARTESIAN_POINT ( 'NONE',  ( -49.24265782934394764, 14.23563200896309944, -91.65785725018901076 ) ) ;
#17986 = VERTEX_POINT ( 'NONE', #15507 ) ;
#17987 = CARTESIAN_POINT ( 'NONE',  ( -95.88693721180811735, 30.76307528361166632, -38.58507135938980781 ) ) ;
#17988 = ORIENTED_EDGE ( 'NONE', *, *, #58843, .T. ) ;
#17989 = CARTESIAN_POINT ( 'NONE',  ( -46.66904755831210139, 0.000000000000000000, 0.000000000000000000 ) ) ;
#17990 = CARTESIAN_POINT ( 'NONE',  ( -24.53636015449704644, -60.58612729876431047, 43.58025477438756212 ) ) ;
#17991 = CARTESIAN_POINT ( 'NONE',  ( 46.50207827473964528, 9.439498081273466568, 61.82945204659085903 ) ) ;
#17992 = CARTESIAN_POINT ( 'NONE',  ( 4.681481898397010788, -6.534749472788160318, -9.499999999999994671 ) ) ;
#17993 = DIRECTION ( 'NONE',  ( 1.000000000000000000, 1.243449787580175325E-14, 0.000000000000000000 ) ) ;
#17994 = CARTESIAN_POINT ( 'NONE',  ( -31.11269837220812207, -31.11269837220801193, 0.000000000000000000 ) ) ;
#17995 = DIRECTION ( 'NONE',  ( 0.000000000000000000, 0.000000000000000000, 1.000000000000000000 ) ) ;
#17996 = CARTESIAN_POINT ( 'NONE',  ( -7.662721893488489755, 395.0000000000064801, 308.5502958579854180 ) ) ;
#17997 = ORIENTED_EDGE ( 'NONE', *, *, #11256, .T. ) ;
#17998 = ORIENTED_EDGE ( 'NONE', *, *, #72, .F. ) ;
#17999 = DIRECTION ( 'NONE',  ( 0.000000000000000000, -0.000000000000000000, -1.000000000000000000 ) ) ;
#18000 = CARTESIAN_POINT ( 'NONE',  ( 173.6718135456487175, 71.42581476597409562, 64.83443665985362259 ) ) ;
#18001 = PLANE ( 'NONE',  #41285 ) ;
#18002 = DIRECTION ( 'NONE',  ( 1.000000000000000000, 0.000000000000000000, 0.000000000000000000 ) ) ;
#18003 = FACE_OUTER_BOUND ( 'NONE', #25734, .T. ) ;
#18004 = AXIS2_PLACEMENT_3D ( 'NONE', #38558, #60003, #11825 ) ;
#18005 = CARTESIAN_POINT ( 'NONE',  ( 74.01791526339553684, 12.16185512414947034, 43.58025477438756212 ) ) ;
#18006 = ORIENTED_EDGE ( 'NONE', *, *, #44062, .F. ) ;
#18007 = CARTESIAN_POINT ( 'NONE',  ( 103.1695711638930675, 26.83837309506523994, -45.96618726772155128 ) ) ;
#18008 = CARTESIAN_POINT ( 'NONE',  ( -13.47680110791658414, 7.324966777230640602, 59.50465629245588417 ) ) ;
#18009 = CARTESIAN_POINT ( 'NONE',  ( 8.113421703707349053, 70.00000000000000000, 5.845715376051984435 ) ) ;
#18010 = FACE_OUTER_BOUND ( 'NONE', #6956, .T. ) ;
#18011 = LINE ( 'NONE', #39461, #51141 ) ;
#18012 = EDGE_CURVE ( 'NONE', #17792, #42599, #48442, .T. ) ;
#18013 = FACE_BOUND ( 'NONE', #12083, .T. ) ;
#18014 = EDGE_CURVE ( 'NONE', #5114, #308, #63096, .T. ) ;
#18015 = VERTEX_POINT ( 'NONE', #27780 ) ;
#18016 = CARTESIAN_POINT ( 'NONE',  ( -62.31345272479885011, -18.49415068377726712, 170.0000000000000000 ) ) ;
#18017 = CARTESIAN_POINT ( 'NONE',  ( 311.9975424824652350, 296.0000000000000000, 420.0000000000000000 ) ) ;
#18018 = CARTESIAN_POINT ( 'NONE',  ( -47.55256438668344998, 13.83151366677316751, 64.41967513731664496 ) ) ;
#18019 = LINE ( 'NONE', #22593, #45555 ) ;
#18020 = CARTESIAN_POINT ( 'NONE',  ( 212.0104729185451617, 118.7959000526603148, 65.24851111504561629 ) ) ;
#18021 = AXIS2_PLACEMENT_3D ( 'NONE', #21007, #26962, #42452 ) ;
#18022 = CARTESIAN_POINT ( 'NONE',  ( -452.6627218934860366, 395.0000000000064801, -116.4497041420121377 ) ) ;
#18023 = ORIENTED_EDGE ( 'NONE', *, *, #67996, .T. ) ;
#18025 = ADVANCED_FACE ( 'NONE', ( #48861 ), #48173, .F. ) ;
#18024 = CARTESIAN_POINT ( 'NONE',  ( -27.00000000000000355, -30.00000000000000355, 12.00000000000000000 ) ) ;
#18026 = CARTESIAN_POINT ( 'NONE',  ( -61.86845765289631771, 16.61548683002701310, 61.52210724104570261 ) ) ;
#18027 = ORIENTED_EDGE ( 'NONE', *, *, #34391, .F. ) ;
#18028 = EDGE_CURVE ( 'NONE', #2060, #60359, #15841, .T. ) ;
#18029 = DIRECTION ( 'NONE',  ( 0.000000000000000000, 0.000000000000000000, 1.000000000000000000 ) ) ;
#18030 = VERTEX_POINT ( 'NONE', #43602 ) ;
#18031 = DIRECTION ( 'NONE',  ( 1.000000000000000000, 0.000000000000000000, 0.000000000000000000 ) ) ;
#18032 = DIRECTION ( 'NONE',  ( 0.000000000000000000, -1.000000000000000000, 0.000000000000000000 ) ) ;
#18033 = CARTESIAN_POINT ( 'NONE',  ( 93.87650740736114585, 23.09802612281732337, -72.16249582444707755 ) ) ;
#18034 = EDGE_LOOP ( 'NONE', ( #31761, #19492, #64500, #278 ) ) ;
#18035 = ADVANCED_FACE ( 'NONE', ( #42232, #64032 ), #36959, .F. ) ;
#18036 = MANIFOLD_SOLID_BREP ( 'Cut-Extrude1', #38393 ) ;
#18037 = ORIENTED_EDGE ( 'NONE', *, *, #40758, .F. ) ;
#18038 = CARTESIAN_POINT ( 'NONE',  ( 45.35146934743632841, 10.27620685439441672, 68.85146973395555392 ) ) ;
#18039 = DIRECTION ( 'NONE',  ( 0.000000000000000000, -0.000000000000000000, -1.000000000000000000 ) ) ;
#18040 = CARTESIAN_POINT ( 'NONE',  ( -153.6994314938755508, 69.16570456337667849, -62.92160878217510600 ) ) ;
#18041 = CARTESIAN_POINT ( 'NONE',  ( 65.39792658623288446, 14.27332852928128304, 17.58415113736946722 ) ) ;
#18042 = DIRECTION ( 'NONE',  ( 0.000000000000000000, 0.000000000000000000, 1.000000000000000000 ) ) ;
#18043 = ORIENTED_EDGE ( 'NONE', *, *, #41689, .T. ) ;
#18044 = DIRECTION ( 'NONE',  ( 1.000000000000000000, 0.000000000000000000, 0.000000000000000000 ) ) ;
#18045 = CARTESIAN_POINT ( 'NONE',  ( -52.45048892661851170, 15.03803514841137989, 18.01105719937357108 ) ) ;
#18046 = CARTESIAN_POINT ( 'NONE',  ( -133.1566699306513613, 52.70203339370773676, -17.45938862731309982 ) ) ;
#18047 = LINE ( 'NONE', #49, #61033 ) ;
#18048 = CARTESIAN_POINT ( 'NONE',  ( 116.6457744947906576, 31.95847117670277271, -20.49168429770345057 ) ) ;
#18049 = CARTESIAN_POINT ( 'NONE',  ( 89.21144084104753347, 20.31809526687001011, 83.85219840701643079 ) ) ;
#18051 = ORIENTED_EDGE ( 'NONE', *, *, #22900, .F. ) ;
#18050 = DIRECTION ( 'NONE',  ( 1.387778780781446169E-16, -1.000000000000000000, -3.469446951953615421E-17 ) ) ;
#18052 = ORIENTED_EDGE ( 'NONE', *, *, #29527, .F. ) ;
#18053 = VECTOR ( 'NONE', #53939, 1000.000000000000000 ) ;
#18054 = EDGE_CURVE ( 'NONE', #11417, #1085, #10209, .T. ) ;
#18055 = EDGE_CURVE ( 'NONE', #5211, #62965, #53110, .T. ) ;
#18056 = ORIENTED_EDGE ( 'NONE', *, *, #49135, .F. ) ;
#18057 = CARTESIAN_POINT ( 'NONE',  ( 39.40195752203892710, 8.409560354027373563, 3.069283715499574683 ) ) ;
#18059 = CARTESIAN_POINT ( 'NONE',  ( -13.60872009721716935, -65.24114748995962998, 34.48241823981439325 ) ) ;
#18058 = VECTOR ( 'NONE', #18971, 1000.000000000000000 ) ;
#18060 = CARTESIAN_POINT ( 'NONE',  ( -47.55235941796723154, 12.79790236059689690, -15.63410455582077496 ) ) ;
#18061 = CARTESIAN_POINT ( 'NONE',  ( 109.3079614081140249, 28.45126415661782104, -9.121775627028522848 ) ) ;
#18062 = EDGE_CURVE ( 'NONE', #15601, #22641, #32373, .T. ) ;
#18063 = DIRECTION ( 'NONE',  ( 0.000000000000000000, 0.000000000000000000, 1.000000000000000000 ) ) ;
#18064 = CARTESIAN_POINT ( 'NONE',  ( 197.6004232003112691, 98.70028881297372436, 87.96336489920018664 ) ) ;
#18066 = DIRECTION ( 'NONE',  ( 0.000000000000000000, 0.000000000000000000, 1.000000000000000000 ) ) ;
#18065 = AXIS2_PLACEMENT_3D ( 'NONE', #46487, #58088, #27100 ) ;
#18067 = CARTESIAN_POINT ( 'NONE',  ( -31.43908319763710679, -170.0000000000000000, -69.66174795566553257 ) ) ;
#18068 = CARTESIAN_POINT ( 'NONE',  ( -14.66033866466834290, 7.432913330382390882, 34.51814378902125213 ) ) ;
#18069 = VERTEX_POINT ( 'NONE', #48514 ) ;
#18070 = PLANE ( 'NONE',  #65463 ) ;
#18071 = VERTEX_POINT ( 'NONE', #343 ) ;
#18072 = VERTEX_POINT ( 'NONE', #16534 ) ;
#18073 = CARTESIAN_POINT ( 'NONE',  ( 66.94365390260637128, 14.65531706601760220, -22.76986491362554332 ) ) ;
#18074 = CARTESIAN_POINT ( 'NONE',  ( 185.1660960081723601, 84.30194217633005849, -76.86554811553853028 ) ) ;
#18075 = CARTESIAN_POINT ( 'NONE',  ( -165.7713056973201731, 80.74264649718247711, 39.84437762675292305 ) ) ;
#18076 = VECTOR ( 'NONE', #20236, 1000.000000000000000 ) ;
#18077 = LINE ( 'NONE', #65214, #41948 ) ;
#18078 = DIRECTION ( 'NONE',  ( 0.000000000000000000, -1.000000000000000000, 0.000000000000000000 ) ) ;
#18079 = LINE ( 'NONE', #60633, #65164 ) ;
#18080 = CARTESIAN_POINT ( 'NONE',  ( -20.55634918610405748, -15.55634918610400774, 2.000000000000001776 ) ) ;
#18081 = VERTEX_POINT ( 'NONE', #43246 ) ;
#18082 = EDGE_LOOP ( 'NONE', ( #39911, #22805, #5836, #12268 ) ) ;
#18083 = ORIENTED_EDGE ( 'NONE', *, *, #63136, .F. ) ;
#18084 = CARTESIAN_POINT ( 'NONE',  ( 112.3013380801406100, 400.0000000000077307, 91.05029585798746439 ) ) ;
#18085 = CARTESIAN_POINT ( 'NONE',  ( -14.66033866466835178, 7.432913330382392658, 7.673593198557576045 ) ) ;
#18086 = CARTESIAN_POINT ( 'NONE',  ( 445.3372781065086201, 177.8591479523844612, 78.55029585798806124 ) ) ;
#18087 = CARTESIAN_POINT ( 'NONE',  ( -20.00000000000000000, 2.449293598294706513E-15, 5.000000000000000000 ) ) ;
#18088 = CARTESIAN_POINT ( 'NONE',  ( -50.52927270563907314, 13.51486287463704450, 31.81483795138946036 ) ) ;
#18089 = CARTESIAN_POINT ( 'NONE',  ( 200.4574930424075774, 102.3536505870638393, 69.75582401855196224 ) ) ;
#18090 = ORIENTED_EDGE ( 'NONE', *, *, #43488, .T. ) ;
#18091 = DIRECTION ( 'NONE',  ( -0.000000000000000000, 1.000000000000000000, -0.000000000000000000 ) ) ;
#18092 = CARTESIAN_POINT ( 'NONE',  ( 203.9203998321608537, 106.9845510704142697, -63.20045979005953285 ) ) ;
#18093 =( LENGTH_UNIT ( ) NAMED_UNIT ( * ) SI_UNIT ( .MILLI., .METRE. ) );
#18094 = CARTESIAN_POINT ( 'NONE',  ( -176.3791001330698975, 90.82833141237287577, -35.44199699171532103 ) ) ;
#18095 = CARTESIAN_POINT ( 'NONE',  ( 104.3805245147141392, 26.26278144139197579, 5.562406129255382581 ) ) ;
#18096 = CARTESIAN_POINT ( 'NONE',  ( -166.6071433144410037, 80.15880179908651826, -92.17533033734891035 ) ) ;
#18097 = CARTESIAN_POINT ( 'NONE',  ( 230.9999999999999432, 225.0000000000000000, -2.000000000000000000 ) ) ;
#18098 = DIRECTION ( 'NONE',  ( 0.000000000000000000, 1.000000000000000000, -0.000000000000000000 ) ) ;
#18099 = CARTESIAN_POINT ( 'NONE',  ( -189.2325002986007689, 107.0800987204799526, 92.40455112761441114 ) ) ;
#18100 = ADVANCED_FACE ( 'NONE', ( #64723 ), #66142, .T. ) ;
#18101 = ORIENTED_EDGE ( 'NONE', *, *, #64138, .T. ) ;
#18102 = CARTESIAN_POINT ( 'NONE',  ( 15.55634918610397399, -31.11269837220809364, 2.000000000000001776 ) ) ;
#18103 = CARTESIAN_POINT ( 'NONE',  ( -132.9409505933031710, 51.31241517713429090, -71.87791970829563581 ) ) ;
#18104 = CARTESIAN_POINT ( 'NONE',  ( 44.99999999999995737, -22.99999999999998579, 4.000000000000000000 ) ) ;
#18105 = LINE ( 'NONE', #56424, #61526 ) ;
#18106 = LINE ( 'NONE', #61015, #42342 ) ;
#18107 = VECTOR ( 'NONE', #53554, 1000.000000000000000 ) ;
#18108 = ORIENTED_EDGE ( 'NONE', *, *, #38584, .F. ) ;
#18110 = EDGE_CURVE ( 'NONE', #59334, #67246, #54851, .T. ) ;
#18109 = CARTESIAN_POINT ( 'NONE',  ( -131.2343730941296371, 50.11186611108016820, -90.81774647483901219 ) ) ;
#18111 = CARTESIAN_POINT ( 'NONE',  ( 188.5644522364758870, 86.51145810658317714, 91.17804384666513329 ) ) ;
#18112 = ORIENTED_EDGE ( 'NONE', *, *, #3029, .F. ) ;
#18113 = VECTOR ( 'NONE', #44422, 1000.000000000000114 ) ;
#18114 = AXIS2_PLACEMENT_3D ( 'NONE', #47557, #30716, #69016 ) ;
#18115 = ORIENTED_EDGE ( 'NONE', *, *, #9996, .F. ) ;
#18116 = CARTESIAN_POINT ( 'NONE',  ( 176.6258282025055166, 74.21441092921637050, -49.76063806208458118 ) ) ;
#18117 = CARTESIAN_POINT ( 'NONE',  ( -179.5178913137216341, 94.54206947403386607, -65.10235975007549314 ) ) ;
#18118 = EDGE_CURVE ( 'NONE', #36200, #1187, #17931, .T. ) ;
#18119 = FACE_OUTER_BOUND ( 'NONE', #69094, .T. ) ;
#18120 = ORIENTED_EDGE ( 'NONE', *, *, #50893, .T. ) ;
#18121 = FACE_OUTER_BOUND ( 'NONE', #15269, .T. ) ;
#18122 = EDGE_CURVE ( 'NONE', #31482, #13050, #12304, .T. ) ;
#18123 = CARTESIAN_POINT ( 'NONE',  ( -5.000000000000073719, -46.66904755831211560, 2.000000000000000000 ) ) ;
#18124 = CARTESIAN_POINT ( 'NONE',  ( -6.851003965218992242, 6.829052369041588300, 3.318326975726704209 ) ) ;
#18125 = VECTOR ( 'NONE', #926, 1000.000000000000000 ) ;
#18126 = EDGE_CURVE ( 'NONE', #3913, #63882, #12656, .T. ) ;
#18127 = CARTESIAN_POINT ( 'NONE',  ( 187.0823097343935331, -170.0000000000000000, 94.99999999999866418 ) ) ;
#18128 = CARTESIAN_POINT ( 'NONE',  ( -28.81071653159242629, 10.19258396314335080, -8.944014519512462513 ) ) ;
#18129 = CARTESIAN_POINT ( 'NONE',  ( -51.34562532494748410, 14.75613283840036694, -9.333915665647241511 ) ) ;
#18130 = ORIENTED_EDGE ( 'NONE', *, *, #69308, .T. ) ;
#18131 = LINE ( 'NONE', #35347, #47991 ) ;
#18132 = CARTESIAN_POINT ( 'NONE',  ( -73.80418150970712077, 21.59712875466423654, 5.341802012060386851 ) ) ;
#18133 = CARTESIAN_POINT ( 'NONE',  ( 39.40195752203891999, 8.409560354027407314, -35.61981746542776506 ) ) ;
#18134 = CARTESIAN_POINT ( 'NONE',  ( 93.85477471612979627, -170.0000000000000000, -95.00000000000133582 ) ) ;
#18136 = ORIENTED_EDGE ( 'NONE', *, *, #41695, .T. ) ;
#18135 = CARTESIAN_POINT ( 'NONE',  ( -127.0849870577083749, 47.28206282326217291, 84.38230841396455162 ) ) ;
#18137 = CARTESIAN_POINT ( 'NONE',  ( 81.57482918025354479, 17.75786713398421313, -37.77517181019251780 ) ) ;
#18138 = VERTEX_POINT ( 'NONE', #22505 ) ;
#18139 = DIRECTION ( 'NONE',  ( -0.000000000000000000, 1.000000000000000000, -0.000000000000000000 ) ) ;
#18140 = CARTESIAN_POINT ( 'NONE',  ( 86.62931800182293784, 20.48449268398422518, 29.71208757247930521 ) ) ;
#18141 = LINE ( 'NONE', #44523, #23114 ) ;
#18142 = ADVANCED_FACE ( 'NONE', ( #55555 ), #50626, .F. ) ;
#18143 = CARTESIAN_POINT ( 'NONE',  ( 311.9975424824652350, 307.8795515535290974, 6.994434899193393562 ) ) ;
#18144 = CARTESIAN_POINT ( 'NONE',  ( 29.86806733335506436, 70.00000000000000000, 2.810436579993893957 ) ) ;
#18145 = LINE ( 'NONE', #66696, #21894 ) ;
#18146 = CARTESIAN_POINT ( 'NONE',  ( -178.2448732545370547, 94.58403736950705820, -9.870808133259494355 ) ) ;
#18147 = DIRECTION ( 'NONE',  ( -0.000000000000000000, -0.000000000000000000, -1.000000000000000000 ) ) ;
#18148 = VERTEX_POINT ( 'NONE', #18625 ) ;
#18149 = ORIENTED_EDGE ( 'NONE', *, *, #17551, .T. ) ;
#18150 = MANIFOLD_SOLID_BREP ( 'Cut-Extrude1', #60892 ) ;
#18151 = AXIS2_PLACEMENT_3D ( 'NONE', #47319, #25553, #48006 ) ;
#18152 = CARTESIAN_POINT ( 'NONE',  ( 45.04360969585144403, 9.210232288266709588, 42.37982661523464856 ) ) ;
#18153 = CARTESIAN_POINT ( 'NONE',  ( 160.4963793545269084, 60.04225845346905999, 56.87706810510036348 ) ) ;
#18154 = DIRECTION ( 'NONE',  ( 1.000000000000000000, -1.540743955509788682E-33, -1.110223024625156540E-16 ) ) ;
#18155 = CARTESIAN_POINT ( 'NONE',  ( 212.1734186221015932, 119.0499290057855291, -43.13375900917836248 ) ) ;
#18156 = B_SPLINE_CURVE_WITH_KNOTS ( 'NONE', 3,
 ( #44586, #34399, #33700, #44223, #7306, #33350, #50215, #28402, #60054, #2376, #23491, #6606, #65709, #12235, #66067, #50559, #65350, #23836, #54782, #55843, #17857, #44931, #11516, #66416, #18206, #39659, #45278, #18551, #32986, #54420, #6248, #27702, #10793, #11138, #37526, #21348 ),
 .UNSPECIFIED., .F., .F.,
 ( 4, 2, 2, 2, 2, 2, 2, 2, 2, 2, 2, 2, 2, 2, 2, 2, 2, 4 ),
 ( 3.469446951953614189E-18, 0.001545474820159047037, 0.003090949640318090604, 0.004636424460477133955, 0.006181899280636177739, 0.007727374100795224125, 0.008500111510874739512, 0.009272848920954255766, 0.01081832374111328654, 0.01236379856127231558, 0.01390927338143134462, 0.01545474820159037539, 0.01700022302174940617, 0.01854569784190843520, 0.02009117266206746424, 0.02163664748222649328, 0.02318212230238552579, 0.02472759712254455136 ),
 .UNSPECIFIED. ) ;
#18157 = CARTESIAN_POINT ( 'NONE',  ( -75.65611349188964141, 22.26947559308019819, -76.33353871646717437 ) ) ;
#18158 = CARTESIAN_POINT ( 'NONE',  ( -109.7078892845591582, 36.71702188566217728, 65.93493008401821953 ) ) ;
#18159 = CARTESIAN_POINT ( 'NONE',  ( -31.43908319763710679, -170.0000000000000000, -96.50629854612921577 ) ) ;
#18160 = CARTESIAN_POINT ( 'NONE',  ( 15.55634918610397399, -31.11269837220809364, 85.00100000000000477 ) ) ;
#18161 = ORIENTED_EDGE ( 'NONE', *, *, #10155, .F. ) ;
#18162 = PRODUCT_DEFINITION_SHAPE ( 'NONE', 'NONE',  #69604 ) ;
#18163 = ORIENTED_EDGE ( 'NONE', *, *, #13260, .F. ) ;
#18164 = ORIENTED_EDGE ( 'NONE', *, *, #23112, .F. ) ;
#18165 = VECTOR ( 'NONE', #53831, 1000.000000000000000 ) ;
#18166 = AXIS2_PLACEMENT_3D ( 'NONE', #37635, #4942, #59085 ) ;
#18167 = PLANE ( 'NONE',  #46464 ) ;
#18168 = FACE_OUTER_BOUND ( 'NONE', #23410, .T. ) ;
#18169 = DIRECTION ( 'NONE',  ( -0.8805955318567321166, -0.4738686624730094055, 0.000000000000000000 ) ) ;
#18170 = CARTESIAN_POINT ( 'NONE',  ( 132.9453095272139649, 42.04754713161463542, 44.51034083899536853 ) ) ;
#18171 = DIRECTION ( 'NONE',  ( -0.000000000000000000, 1.000000000000000000, -0.000000000000000000 ) ) ;
#18172 = CARTESIAN_POINT ( 'NONE',  ( 0.000000000000000000, 0.000000000000000000, -10.00000000000000000 ) ) ;
#18173 = PRESENTATION_LAYER_ASSIGNMENT (  '', '', ( #33887 ) ) ;
#18174 = CARTESIAN_POINT ( 'NONE',  ( 442.3372781065086201, 395.0000000000043201, 108.5502958579839117 ) ) ;
#18175 = CARTESIAN_POINT ( 'NONE',  ( 61.33840119549017800, 13.32121602003046590, 29.99886885364463041 ) ) ;
#18176 = CARTESIAN_POINT ( 'NONE',  ( 33.20336330085616083, 7.683867620844146984, 86.82877894857017509 ) ) ;
#18177 = CARTESIAN_POINT ( 'NONE',  ( 230.9999999999999432, 190.0000000000000000, 72.99999999999998579 ) ) ;
#18178 = VERTEX_POINT ( 'NONE', #6674 ) ;
#18179 = CARTESIAN_POINT ( 'NONE',  ( 55.64941011647476898, 12.11006142851271505, 65.63107993823560093 ) ) ;
#18180 = CARTESIAN_POINT ( 'NONE',  ( -12.50000000000000000, -17.50000000000000000, 20.00000000000000000 ) ) ;
#18182 = ADVANCED_FACE ( 'NONE', ( #60135 ), #39732, .F. ) ;
#18181 = CARTESIAN_POINT ( 'NONE',  ( 80.34841469379381351, 17.37275484083203381, 94.99999999999866418 ) ) ;
#18183 = CARTESIAN_POINT ( 'NONE',  ( 203.9181091394787302, 105.2759068139671399, 71.05227132923315025 ) ) ;
#18184 = CARTESIAN_POINT ( 'NONE',  ( -95.30586079737264527, 29.37688003290242733, -93.43552264237898441 ) ) ;
#18185 = EDGE_CURVE ( 'NONE', #19578, #55116, #61191, .T. ) ;
#18186 = ORIENTED_EDGE ( 'NONE', *, *, #1415, .T. ) ;
#18187 = CARTESIAN_POINT ( 'NONE',  ( 565.8357120730591987, 861.3826715180497331, 663.5068267248710754 ) ) ;
#18188 = DIRECTION ( 'NONE',  ( 1.020422603260505347E-14, -1.000000000000000000, -5.551115123125782702E-17 ) ) ;
#18189 = CARTESIAN_POINT ( 'NONE',  ( -27.00000000000000355, 0.000000000000000000, 12.00000000000000000 ) ) ;
#18190 = FACE_OUTER_BOUND ( 'NONE', #66226, .T. ) ;
#18191 = ITEM_DEFINED_TRANSFORMATION ( 'NONE', 'NONE', #48946,  #66832 ) ;
#18192 = CARTESIAN_POINT ( 'NONE',  ( -173.0336157925723910, 87.03110432393005169, 84.50715133059941309 ) ) ;
#18193 = ORIENTED_EDGE ( 'NONE', *, *, #45326, .F. ) ;
#18194 = CARTESIAN_POINT ( 'NONE',  ( -439.4229916354185548, 388.0000000000064801, -133.9497041420121377 ) ) ;
#18195 = CARTESIAN_POINT ( 'NONE',  ( -142.1381007084227406, 58.17237452544243581, -16.88903420692564339 ) ) ;
#18196 = CARTESIAN_POINT ( 'NONE',  ( -4.502148936856957384, 7.704491846230415497, -63.02114756112786864 ) ) ;
#18197 = EDGE_CURVE ( 'NONE', #4486, #19070, #56251, .T. ) ;
#18198 = DIRECTION ( 'NONE',  ( -7.703719777548945123E-34, -1.479221584281240009E-31, 1.000000000000000000 ) ) ;
#18199 = EDGE_LOOP ( 'NONE', ( #1495, #55031, #69116, #52228 ) ) ;
#18200 = CARTESIAN_POINT ( 'NONE',  ( -55.05276343752909440, 15.72344139423348430, 3.472777182467473800 ) ) ;
#18201 = CARTESIAN_POINT ( 'NONE',  ( 60.58000000000000540, -36.09918303830819752, 20.41169613715280207 ) ) ;
#18202 = EDGE_CURVE ( 'NONE', #17425, #2403, #29517, .T. ) ;
#18203 = CARTESIAN_POINT ( 'NONE',  ( -98.67557579989345129, 32.10670856967971076, 31.42459644286125453 ) ) ;
#18204 = CARTESIAN_POINT ( 'NONE',  ( 18.19980344696536534, 6.589834367837007711, -50.12491448036190889 ) ) ;
#18205 = AXIS2_PLACEMENT_3D ( 'NONE', #28227, #39156, #54964 ) ;
#18207 = ORIENTED_EDGE ( 'NONE', *, *, #41309, .F. ) ;
#18206 = CARTESIAN_POINT ( 'NONE',  ( 116.6681538161788865, 33.09439081574000596, 6.366003624344346967 ) ) ;
#18208 = DIRECTION ( 'NONE',  ( 0.000000000000000000, 0.000000000000000000, -1.000000000000000000 ) ) ;
#18209 = ORIENTED_EDGE ( 'NONE', *, *, #15852, .F. ) ;
#18210 = VECTOR ( 'NONE', #61236, 1000.000000000000114 ) ;
#18211 = TOROIDAL_SURFACE ( 'NONE', #14827, 22.50000000000000000, 1.500000000000000444 ) ;
#18212 = ORIENTED_EDGE ( 'NONE', *, *, #24367, .T. ) ;
#18213 = AXIS2_PLACEMENT_3D ( 'NONE', #4155, #20663, #67832 ) ;
#18214 = CARTESIAN_POINT ( 'NONE',  ( 173.9405361758639117, 73.05302209498820787, 39.11095342079327963 ) ) ;
#18216 = CARTESIAN_POINT ( 'NONE',  ( 22.29513692215318343, 6.796052026456516515, -73.62533078381031260 ) ) ;
#18215 = VECTOR ( 'NONE', #67203, 1000.000000000000000 ) ;
#18218 = VERTEX_POINT ( 'NONE', #33423 ) ;
#18217 = CARTESIAN_POINT ( 'NONE',  ( -15.07533778868020136, 8.482826962130836534, -67.82638443619325130 ) ) ;
#18219 = CARTESIAN_POINT ( 'NONE',  ( 3.000000000000004441, 0.000000000000000000, -46.99999999999997158 ) ) ;
#18220 = CARTESIAN_POINT ( 'NONE',  ( -30.46358361599563480, 10.45190018822943578, 45.16857927621155966 ) ) ;
#18221 = CARTESIAN_POINT ( 'NONE',  ( -71.26746920569853216, 20.70422440535242359, -43.86833251615107088 ) ) ;
#18222 = ORIENTED_EDGE ( 'NONE', *, *, #39057, .F. ) ;
#18223 = CARTESIAN_POINT ( 'NONE',  ( 210.0122310839192039, 115.7355030290287488, -65.35538431068530940 ) ) ;
#18224 = DIRECTION ( 'NONE',  ( 0.000000000000000000, -1.000000000000000000, 0.000000000000000000 ) ) ;
#18225 = CARTESIAN_POINT ( 'NONE',  ( -180.5234362879040191, 97.35934147644942982, 39.56920222819405808 ) ) ;
#18226 = CARTESIAN_POINT ( 'NONE',  ( -24.53636015449705354, -60.58612729876431047, 41.38025477438755928 ) ) ;
#18227 = CARTESIAN_POINT ( 'NONE',  ( 23.04797191264876233, 7.849755664016357493, 62.41308431887384955 ) ) ;
#18228 = ORIENTED_EDGE ( 'NONE', *, *, #51150, .F. ) ;
#18229 = ORIENTED_EDGE ( 'NONE', *, *, #33056, .T. ) ;
#18230 = EDGE_LOOP ( 'NONE', ( #63511, #47058, #41676, #63 ) ) ;
#18231 = CARTESIAN_POINT ( 'NONE',  ( 207.0339556760109474, 109.6008634273003111, -90.38007673268727160 ) ) ;
#18232 = CARTESIAN_POINT ( 'NONE',  ( -33.36721086971962080, 9.915747831546610769, -35.56515356514455561 ) ) ;
#18233 = DIRECTION ( 'NONE',  ( 1.000000000000000000, 0.000000000000000000, 0.000000000000000000 ) ) ;
#18234 = CARTESIAN_POINT ( 'NONE',  ( -142.0062637385109952, 58.06920992247431457, 38.77129379673751686 ) ) ;
#18235 = CARTESIAN_POINT ( 'NONE',  ( -127.6992109187851980, 47.69334801994794049, 57.67066701129382267 ) ) ;
#18236 = CARTESIAN_POINT ( 'NONE',  ( 50.98853755884125860, 400.0000000000071054, 91.05029585798797598 ) ) ;
#18237 = ORIENTED_EDGE ( 'NONE', *, *, #8738, .F. ) ;
#18238 = CARTESIAN_POINT ( 'NONE',  ( 26.11269837220806167, 4.999999999999936939, 2.000000000000001776 ) ) ;
#18239 = VERTEX_POINT ( 'NONE', #28123 ) ;
#18240 = CARTESIAN_POINT ( 'NONE',  ( -94.87734348028330089, 30.28727895192195874, -95.00000000000133582 ) ) ;
#18241 = CARTESIAN_POINT ( 'NONE',  ( 35.16506477614511539, 22.46626293537709529, 13.79046412351414475 ) ) ;
#18242 = CARTESIAN_POINT ( 'NONE',  ( -447.6627218934918915, 367.0710678118718988, -141.4497041420121377 ) ) ;
#18243 = CARTESIAN_POINT ( 'NONE',  ( 6.400000000000000355, 4.618802153517004960, 7.999999999999998224 ) ) ;
#18244 = DIRECTION ( 'NONE',  ( -0.000000000000000000, -0.000000000000000000, -1.000000000000000000 ) ) ;
#18245 = CARTESIAN_POINT ( 'NONE',  ( -47.95193882091086834, 12.89180642785319897, 8.508404476638974145 ) ) ;
#18246 = AXIS2_PLACEMENT_3D ( 'NONE', #29107, #2373, #23830 ) ;
#18247 = CARTESIAN_POINT ( 'NONE',  ( 156.5977259323288138, 56.97512126940429766, -51.08633290075279376 ) ) ;
#18248 = ADVANCED_FACE ( 'NONE', ( #49569 ), #1398, .F. ) ;
#18249 = CARTESIAN_POINT ( 'NONE',  ( 159.2258951716709419, 60.31399909112328572, -77.77388725095455868 ) ) ;
#18250 = ORIENTED_EDGE ( 'NONE', *, *, #42370, .T. ) ;
#18251 = PRESENTATION_LAYER_ASSIGNMENT (  '', '', ( #24993 ) ) ;
#18252 = CARTESIAN_POINT ( 'NONE',  ( -106.1135431881943134, 34.77124450854139326, -89.75381755830838415 ) ) ;
#18253 = LINE ( 'NONE', #47302, #47562 ) ;
#18254 = ORIENTED_EDGE ( 'NONE', *, *, #37790, .T. ) ;
#18255 = CARTESIAN_POINT ( 'NONE',  ( 51.85299110299440173, 39.21848821248450179, 0.000000000000000000 ) ) ;
#18256 = CARTESIAN_POINT ( 'NONE',  ( -56.01329802674225533, 15.98369420723827083, 57.20787140630700662 ) ) ;
#18257 = CARTESIAN_POINT ( 'NONE',  ( 126.6904219525097659, 37.26255867422720058, -95.00000000000133582 ) ) ;
#18258 = ORIENTED_EDGE ( 'NONE', *, *, #30823, .T. ) ;
#18259 = CARTESIAN_POINT ( 'NONE',  ( 447.3372781065082791, 400.0000000000044338, 78.55029585798382641 ) ) ;
#18261 = EDGE_CURVE ( 'NONE', #23841, #30847, #2349, .T. ) ;
#18260 = CARTESIAN_POINT ( 'NONE',  ( -12.39413342787891459, 7.231444436041488899, -63.79466433623242949 ) ) ;
#18262 = CARTESIAN_POINT ( 'NONE',  ( -34.06864996337442619, 10.03773626259441976, 44.74462983094167612 ) ) ;
#18263 = VECTOR ( 'NONE', #68671, 1000.000000000000000 ) ;
#18264 = CARTESIAN_POINT ( 'NONE',  ( -28.13266652174641180, 9.071935854491416151, 71.29729791657065618 ) ) ;
#18265 = EDGE_CURVE ( 'NONE', #27416, #21875, #30226, .T. ) ;
#18266 = EDGE_LOOP ( 'NONE', ( #12719, #17064, #44879, #58736 ) ) ;
#18268 = MANIFOLD_SOLID_BREP ( 'Cut-Extrude3', #12595 ) ;
#18267 = EDGE_CURVE ( 'NONE', #38316, #40305, #10203, .T. ) ;
#18270 = VECTOR ( 'NONE', #27351, 1000.000000000000000 ) ;
#18269 = DIRECTION ( 'NONE',  ( 1.000000000000000000, 1.015474350197485566E-14, 3.682371605725279925E-16 ) ) ;
#18271 = DIRECTION ( 'NONE',  ( 0.7071067811865476838, 1.110223024625156294E-16, 0.7071067811865474617 ) ) ;
#18272 = ORIENTED_EDGE ( 'NONE', *, *, #35809, .F. ) ;
#18273 = CARTESIAN_POINT ( 'NONE',  ( -185.0000000000000000, 2.265596578422603396E-14, 0.000000000000000000 ) ) ;
#18274 = DIRECTION ( 'NONE',  ( -0.000000000000000000, -0.000000000000000000, -1.000000000000000000 ) ) ;
#18275 = CARTESIAN_POINT ( 'NONE',  ( -2.869721780807581002, 7.625909776230889392, 16.42176429208887711 ) ) ;
#18276 = CARTESIAN_POINT ( 'NONE',  ( -0.5178428571329636299, 7.532057582089301206, 66.16617111386234740 ) ) ;
#18277 = CARTESIAN_POINT ( 'NONE',  ( -20.63749999999999574, 0.000000000000000000, 0.000000000000000000 ) ) ;
#18278 = EDGE_CURVE ( 'NONE', #63051, #18617, #41470, .T. ) ;
#18279 = CARTESIAN_POINT ( 'NONE',  ( -123.4531143159639157, 44.90777521523904880, -76.35369456291449808 ) ) ;
#18280 = ORIENTED_EDGE ( 'NONE', *, *, #28584, .F. ) ;
#18281 = CARTESIAN_POINT ( 'NONE',  ( -1.148430018225573557, 500.0000000000000000, -53.65523180892861177 ) ) ;
#18282 = LINE ( 'NONE', #2803, #15976 ) ;
#18283 = CARTESIAN_POINT ( 'NONE',  ( 70.11766033381769603, 14.43277633974325980, 61.69673158615264441 ) ) ;
#18284 = CARTESIAN_POINT ( 'NONE',  ( -131.2399641789143061, 51.34350731997123063, -90.82310783052086833 ) ) ;
#18285 = CARTESIAN_POINT ( 'NONE',  ( 14.99999999999998579, 0.000000000000000000, 55.00000000000001421 ) ) ;
#18286 = EDGE_LOOP ( 'NONE', ( #10547, #44440 ) ) ;
#18287 = CARTESIAN_POINT ( 'NONE',  ( 164.8914542114683286, 64.97670918603530765, -17.90087482810826813 ) ) ;
#18288 = CARTESIAN_POINT ( 'NONE',  ( 9.058156535714477542, 6.378495712187263855, 34.19564460572066622 ) ) ;
#18289 = ORIENTED_EDGE ( 'NONE', *, *, #69173, .T. ) ;
#18290 = CARTESIAN_POINT ( 'NONE',  ( -58.33245019990697244, 15.58496056636070470, -62.79849011809130133 ) ) ;
#18291 = DIRECTION ( 'NONE',  ( -0.000000000000000000, 1.000000000000000000, -0.000000000000000000 ) ) ;
#18292 = AXIS2_PLACEMENT_3D ( 'NONE', #48383, #16056, #220 ) ;
#18293 = ORIENTED_EDGE ( 'NONE', *, *, #49593, .T. ) ;
#18294 = CARTESIAN_POINT ( 'NONE',  ( 164.9700808964341832, 65.04346068891118193, -43.33544459004915694 ) ) ;
#18295 = DIRECTION ( 'NONE',  ( 0.000000000000000000, 0.000000000000000000, -1.000000000000000000 ) ) ;
#18296 = FACE_OUTER_BOUND ( 'NONE', #2256, .T. ) ;
#18297 = AXIS2_PLACEMENT_3D ( 'NONE', #41682, #35373, #19181 ) ;
#18298 = ORIENTED_EDGE ( 'NONE', *, *, #65042, .F. ) ;
#18299 = CARTESIAN_POINT ( 'NONE',  ( -96.43817545481741149, 31.02509717589734706, 6.444619006422381169 ) ) ;
#18300 = VECTOR ( 'NONE', #15661, 1000.000000000000000 ) ;
#18301 = CARTESIAN_POINT ( 'NONE',  ( 69.86170716612186027, 15.40591680861103363, 87.92076547287929600 ) ) ;
#18302 = LINE ( 'NONE', #61216, #7348 ) ;
#18303 = CARTESIAN_POINT ( 'NONE',  ( -179.2128128997734962, 95.75254520622993937, -46.61551081691593623 ) ) ;
#18304 = CARTESIAN_POINT ( 'NONE',  ( -128.9786047358386156, 48.55852351614670681, -8.728974343352884802 ) ) ;
#18305 = VECTOR ( 'NONE', #66556, 1000.000000000000000 ) ;
#18306 = CARTESIAN_POINT ( 'NONE',  ( -145.7962722587128894, 61.09447270426119303, -89.48102063609030665 ) ) ;
#18307 = CARTESIAN_POINT ( 'NONE',  ( 130.3019683985926349, 39.31883119822048656, -76.98905284259865311 ) ) ;
#18308 = ORIENTED_EDGE ( 'NONE', *, *, #61547, .T. ) ;
#18309 = CARTESIAN_POINT ( 'NONE',  ( -452.6627218934913230, 400.0000000000000568, -146.4497041420117398 ) ) ;
#18310 = DIRECTION ( 'NONE',  ( 1.000000000000000000, 0.000000000000000000, 0.000000000000000000 ) ) ;
#18311 = VERTEX_POINT ( 'NONE', #3830 ) ;
#18312 = VECTOR ( 'NONE', #48647, 1000.000000000000000 ) ;
#18313 = CARTESIAN_POINT ( 'NONE',  ( -154.0716379918897303, 69.49957566103796580, -48.28304949762831910 ) ) ;
#18314 = DIRECTION ( 'NONE',  ( 0.000000000000000000, 0.000000000000000000, 1.000000000000000000 ) ) ;
#18315 = CARTESIAN_POINT ( 'NONE',  ( -31.93169728792083362, 10.69234447276977029, 45.21645440618919309 ) ) ;
#18316 = EDGE_CURVE ( 'NONE', #11917, #51047, #36189, .T. ) ;
#18317 = FACE_OUTER_BOUND ( 'NONE', #22447, .T. ) ;
#18318 = LINE ( 'NONE', #39773, #64040 ) ;
#18319 = DIRECTION ( 'NONE',  ( -0.000000000000000000, -0.000000000000000000, -1.000000000000000000 ) ) ;
#18320 = CARTESIAN_POINT ( 'NONE',  ( -1.454841858088666839, 7.566772088227303961, -20.03908844737443218 ) ) ;
#18321 = CARTESIAN_POINT ( 'NONE',  ( -13.92109095214680003, 8.375243258322932149, 33.23919069653987179 ) ) ;
#18322 = CARTESIAN_POINT ( 'NONE',  ( -31.43908319763709258, 9.591432048623767415, -35.31719736520183517 ) ) ;
#18323 = VERTEX_POINT ( 'NONE', #52364 ) ;
#18324 = CARTESIAN_POINT ( 'NONE',  ( -40.24154210098803475, 63.23235722614447951, 41.38025477438755928 ) ) ;
#18325 = ORIENTED_EDGE ( 'NONE', *, *, #27485, .F. ) ;
#18326 = CARTESIAN_POINT ( 'NONE',  ( 105.2506154496929867, 26.63995206619730638, -64.66458505761366382 ) ) ;
#18327 = CARTESIAN_POINT ( 'NONE',  ( 45.04020069093780876, 10.22779424730543063, -11.30540839519373719 ) ) ;
#18328 = CARTESIAN_POINT ( 'NONE',  ( -62.66631205405160188, -18.59153367093452047, 41.38025477438755928 ) ) ;
#18329 = CARTESIAN_POINT ( 'NONE',  ( -439.4229916354182706, 400.0000000000064801, 91.05029585798840230 ) ) ;
#18330 = PLANE ( 'NONE',  #31153 ) ;
#18331 = CARTESIAN_POINT ( 'NONE',  ( 0.7145311798163210826, 4.618802153517001408, -8.000000000000000000 ) ) ;
#18332 = CYLINDRICAL_SURFACE ( 'NONE', #29699, 5.000000000000004441 ) ;
#18333 = CARTESIAN_POINT ( 'NONE',  ( 204.6977192012829789, 106.3443248447423315, 71.05227132923315025 ) ) ;
#18334 = VERTEX_POINT ( 'NONE', #35497 ) ;
#18335 = VERTEX_POINT ( 'NONE', #25303 ) ;
#18337 = EDGE_CURVE ( 'NONE', #30965, #8346, #38434, .T. ) ;
#18336 = DIRECTION ( 'NONE',  ( -0.000000000000000000, -6.405132834375902056E-16, 1.000000000000000000 ) ) ;
#18338 = CARTESIAN_POINT ( 'NONE',  ( 0.000000000000000000, 0.000000000000000000, 40.00000000000003553 ) ) ;
#18339 = CARTESIAN_POINT ( 'NONE',  ( 46.68054346512387554, 9.468156054376091646, -95.00000000000133582 ) ) ;
#18340 = CARTESIAN_POINT ( 'NONE',  ( 109.3047140914111708, 29.55674059952506738, 71.41186036636744916 ) ) ;
#18341 = VECTOR ( 'NONE', #54932, 1000.000000000000000 ) ;
#18342 = CARTESIAN_POINT ( 'NONE',  ( -170.2856292770788684, 85.50720222068218845, -22.32389805880076850 ) ) ;
#18343 = VECTOR ( 'NONE', #12709, 1000.000000000000000 ) ;
#18344 = EDGE_CURVE ( 'NONE', #55226, #27257, #68542, .T. ) ;
#18345 = LINE ( 'NONE', #17296, #49879 ) ;
#18346 = VERTEX_POINT ( 'NONE', #63268 ) ;
#18347 = CARTESIAN_POINT ( 'NONE',  ( 106.4072861358878441, 28.24787347451998443, -36.97294736244227664 ) ) ;
#18348 = CARTESIAN_POINT ( 'NONE',  ( 20.35964562795319921, 7.697260051881318788, -37.05298214970821391 ) ) ;
#18349 = DIRECTION ( 'NONE',  ( -0.5773502691896258421, 0.5773502691896257311, -0.5773502691896257311 ) ) ;
#18350 = DIRECTION ( 'NONE',  ( -0.000000000000000000, -0.000000000000000000, -1.000000000000000000 ) ) ;
#18351 = CARTESIAN_POINT ( 'NONE',  ( -59.09450113343241640, 27.07101652673493319, 40.00000000000003553 ) ) ;
#18352 = FACE_BOUND ( 'NONE', #59547, .T. ) ;
#18353 = VECTOR ( 'NONE', #2846, 1000.000000000000000 ) ;
#18354 = VECTOR ( 'NONE', #11675, 1000.000000000000000 ) ;
#18355 = VECTOR ( 'NONE', #68024, 1000.000000000000000 ) ;
#18356 = EDGE_CURVE ( 'NONE', #40674, #18627, #20345, .T. ) ;
#18357 = ORIENTED_EDGE ( 'NONE', *, *, #13431, .F. ) ;
#18358 = FACE_OUTER_BOUND ( 'NONE', #34983, .T. ) ;
#18359 = CARTESIAN_POINT ( 'NONE',  ( 90.51709546286271291, 21.85407654229979713, -49.73978282941543938 ) ) ;
#18360 = VECTOR ( 'NONE', #40304, 1000.000000000000000 ) ;
#18361 = CARTESIAN_POINT ( 'NONE',  ( 36.09469435220862721, 9.015003538710471886, -76.71338776024327899 ) ) ;
#18362 = CARTESIAN_POINT ( 'NONE',  ( 181.0840389613909736, -170.0000000000000000, -70.56960825634330092 ) ) ;
#18363 = CARTESIAN_POINT ( 'NONE',  ( 152.1190604254709626, 53.60705199010332933, 4.804158789010992692 ) ) ;
#18364 = EDGE_CURVE ( 'NONE', #28296, #29979, #46383, .T. ) ;
#18365 = CARTESIAN_POINT ( 'NONE',  ( 450.2085304802404835, 0.000000000000000000, -219.9999999999999147 ) ) ;
#18366 = B_SPLINE_CURVE_WITH_KNOTS ( 'NONE', 3,
 ( #40486, #61934, #46107, #32014 ),
 .UNSPECIFIED., .F., .F.,
 ( 4, 4 ),
 ( 0.1259919275528360583, 0.1829744153748752433 ),
 .UNSPECIFIED. ) ;
#18367 = ORIENTED_EDGE ( 'NONE', *, *, #15242, .F. ) ;
#18368 = CARTESIAN_POINT ( 'NONE',  ( 0.000000000000000000, 0.000000000000000000, 0.000000000000000000 ) ) ;
#18369 = CARTESIAN_POINT ( 'NONE',  ( 200.8303160266299301, 102.8412051751308809, -37.38573241369641664 ) ) ;
#18370 = ORIENTED_EDGE ( 'NONE', *, *, #42418, .T. ) ;
#18371 = CARTESIAN_POINT ( 'NONE',  ( -72.57286576968809300, 18.73210786364346703, 41.38025477438755928 ) ) ;
#18372 = ORIENTED_EDGE ( 'NONE', *, *, #69569, .T. ) ;
#18373 = CARTESIAN_POINT ( 'NONE',  ( -85.10774223992955001, 24.88053943842881566, -73.31006263638853682 ) ) ;
#18374 = CARTESIAN_POINT ( 'NONE',  ( -60.95805269991217301, 17.39401718769327232, -20.50189859807008830 ) ) ;
#18375 = CARTESIAN_POINT ( 'NONE',  ( -189.2776534485022069, 108.4862893474047638, -95.00000000000133582 ) ) ;
#18376 = VERTEX_POINT ( 'NONE', #62581 ) ;
#18377 = ORIENTED_EDGE ( 'NONE', *, *, #1674, .F. ) ;
#18378 = CARTESIAN_POINT ( 'NONE',  ( 46.90170507415071910, 10.52318308703818417, 64.75371562520641078 ) ) ;
#18379 = CARTESIAN_POINT ( 'NONE',  ( 164.9706294237034570, 65.04392654036658428, 36.63534575754673028 ) ) ;
#18380 = CARTESIAN_POINT ( 'NONE',  ( -27.00000000000000355, 0.000000000000000000, 15.00000000000000000 ) ) ;
#18381 = ORIENTED_EDGE ( 'NONE', *, *, #56224, .F. ) ;
#18382 =( NAMED_UNIT ( * ) SI_UNIT ( $, .STERADIAN. ) SOLID_ANGLE_UNIT ( ) );
#18383 = CARTESIAN_POINT ( 'NONE',  ( -20.00000000000002842, -6.319444444444441089, 0.000000000000000000 ) ) ;
#18384 = CIRCLE ( 'NONE', #22907, 23.97499999999999787 ) ;
#18385 = CARTESIAN_POINT ( 'NONE',  ( -128.1267916618074594, 49.19573276651588856, -8.394488801384238030 ) ) ;
#18386 = CARTESIAN_POINT ( 'NONE',  ( 31.11269837220803325, -10.55634918610409656, 85.00100000000000477 ) ) ;
#18387 = CYLINDRICAL_SURFACE ( 'NONE', #2897, 7.500000000000013323 ) ;
#18389 = EDGE_LOOP ( 'NONE', ( #26028, #25915, #68270, #1705, #65220, #49982 ) ) ;
#18388 = DIRECTION ( 'NONE',  ( -0.000000000000000000, 1.000000000000000000, -0.000000000000000000 ) ) ;
#18390 = VERTEX_POINT ( 'NONE', #41812 ) ;
#18391 =( GEOMETRIC_REPRESENTATION_CONTEXT ( 3 ) GLOBAL_UNCERTAINTY_ASSIGNED_CONTEXT ( ( #24754 ) ) GLOBAL_UNIT_ASSIGNED_CONTEXT ( ( #33734, #65747, #48828 ) ) REPRESENTATION_CONTEXT ( 'NONE', 'WORKASPACE' ) );
#18392 = ORIENTED_EDGE ( 'NONE', *, *, #7295, .T. ) ;
#18393 = AXIS2_PLACEMENT_3D ( 'NONE', #64098, #53179, #58465 ) ;
#18394 = CARTESIAN_POINT ( 'NONE',  ( 42.03492317486906416, 8.766487167902388578, 3.542427428059454986 ) ) ;
#18395 = CARTESIAN_POINT ( 'NONE',  ( 174.6307688320643479, 73.70327352127003451, 6.133243260141832742 ) ) ;
#18396 = CARTESIAN_POINT ( 'NONE',  ( 2.307317748320714124E-15, -6.534749472788169200, -4.681481898396984143 ) ) ;
#18397 = EDGE_CURVE ( 'NONE', #67683, #36964, #11304, .T. ) ;
#18398 = CARTESIAN_POINT ( 'NONE',  ( 105.2506154496929014, 26.63995206619730638, -10.97548387668630809 ) ) ;
#18399 = CARTESIAN_POINT ( 'NONE',  ( 140.7314320101251610, 45.73329916786966720, -94.18496931662966176 ) ) ;
#18400 = VECTOR ( 'NONE', #13322, 1000.000000000000000 ) ;
#18401 = CARTESIAN_POINT ( 'NONE',  ( 211.2889559786411269, 117.6796425177967507, 93.97986437182990471 ) ) ;
#18402 = AXIS2_PLACEMENT_3D ( 'NONE', #59592, #11770, #22328 ) ;
#18403 = DIRECTION ( 'NONE',  ( -0.000000000000000000, -0.000000000000000000, -1.000000000000000000 ) ) ;
#18404 = CARTESIAN_POINT ( 'NONE',  ( -73.10694748374055507, 20.28107308417883914, -74.51766719739275402 ) ) ;
#18405 = LINE ( 'NONE', #50420, #11791 ) ;
#18407 = EDGE_LOOP ( 'NONE', ( #28057, #60553 ) ) ;
#18406 = EDGE_CURVE ( 'NONE', #18346, #31575, #57987, .T. ) ;
#18408 = AXIS2_PLACEMENT_3D ( 'NONE', #30223, #51674, #18622 ) ;
#18409 = DIRECTION ( 'NONE',  ( -1.000000000000000000, -0.000000000000000000, -0.000000000000000000 ) ) ;
#18410 = ORIENTED_EDGE ( 'NONE', *, *, #29227, .F. ) ;
#18411 = ORIENTED_EDGE ( 'NONE', *, *, #43333, .F. ) ;
#18412 = DIRECTION ( 'NONE',  ( -0.000000000000000000, 1.000000000000000000, -0.000000000000000000 ) ) ;
#18413 = CARTESIAN_POINT ( 'NONE',  ( 183.7875981612219789, 82.83906702837187197, -63.57054041331110028 ) ) ;
#18414 = AXIS2_PLACEMENT_3D ( 'NONE', #43582, #28458, #44640 ) ;
#18415 = CARTESIAN_POINT ( 'NONE',  ( -167.4860113959265675, 82.52233889531186151, 43.27754665363389108 ) ) ;
#18416 = CARTESIAN_POINT ( 'NONE',  ( -98.69283175933884422, 30.99524616306738523, -49.11836846358093567 ) ) ;
#18417 = DIRECTION ( 'NONE',  ( 1.000000000000000000, 0.000000000000000000, 0.000000000000000000 ) ) ;
#18418 = DIRECTION ( 'NONE',  ( -0.000000000000000000, -0.000000000000000000, 1.000000000000000000 ) ) ;
#18419 = CARTESIAN_POINT ( 'NONE',  ( 139.6150621148398159, 46.20856238844172026, -11.84746746713147481 ) ) ;
#18420 = ORIENTED_EDGE ( 'NONE', *, *, #56136, .F. ) ;
#18421 = EDGE_CURVE ( 'NONE', #18508, #49272, #25709, .T. ) ;
#18422 = ORIENTED_EDGE ( 'NONE', *, *, #67439, .F. ) ;
#18423 = EDGE_CURVE ( 'NONE', #16594, #13447, #49507, .T. ) ;
#18424 = CARTESIAN_POINT ( 'NONE',  ( 187.9768140620194856, 87.36183560332112563, 93.45980768820729168 ) ) ;
#18425 = CARTESIAN_POINT ( 'NONE',  ( -10.23867141318105922, 7.059827648235819098, 3.652912843573254076 ) ) ;
#18426 = CYLINDRICAL_SURFACE ( 'NONE', #56970, 5.000000000000004441 ) ;
#18427 = CARTESIAN_POINT ( 'NONE',  ( 56.53776994993148008, 11.26292242501184937, -12.58817050827255990 ) ) ;
#18428 = EDGE_CURVE ( 'NONE', #51453, #6148, #10477, .T. ) ;
#18429 = UNCERTAINTY_MEASURE_WITH_UNIT (LENGTH_MEASURE( 1.000000000000000082E-05 ), #44825, 'distance_accuracy_value', 'NONE');
#18430 = EDGE_CURVE ( 'NONE', #22557, #47203, #66833, .T. ) ;
#18431 = CARTESIAN_POINT ( 'NONE',  ( -190.6985136298601731, 109.1272424661242582, 33.97142148329322708 ) ) ;
#18432 = DIRECTION ( 'NONE',  ( -0.000000000000000000, -1.000000000000000000, -0.000000000000000000 ) ) ;
#18433 = EDGE_LOOP ( 'NONE', ( #64907, #54509, #37131, #39710 ) ) ;
#18434 = CARTESIAN_POINT ( 'NONE',  ( 43.96062659677685502, 10.06332325923985849, -63.98880687523393362 ) ) ;
#18435 = CARTESIAN_POINT ( 'NONE',  ( -55.53456145826333312, 15.85318253404851419, -77.06087458892361042 ) ) ;
#18436 = CARTESIAN_POINT ( 'NONE',  ( 201.9822477997852843, 104.3642793804899469, -77.67341262940828983 ) ) ;
#18437 = CARTESIAN_POINT ( 'NONE',  ( -178.0633751203918393, 92.80295726428047942, -36.56588663441552711 ) ) ;
#18438 = CARTESIAN_POINT ( 'NONE',  ( 103.5588133492865239, 25.91050225236394056, 6.827373951400315555 ) ) ;
#18439 = CARTESIAN_POINT ( 'NONE',  ( -166.7068579965636559, 80.26142964949319492, 7.581365930921141860 ) ) ;
#18440 = DIRECTION ( 'NONE',  ( -0.000000000000000000, 1.000000000000000000, -0.000000000000000000 ) ) ;
#18441 = FACE_BOUND ( 'NONE', #40769, .T. ) ;
#18442 = B_SPLINE_CURVE_WITH_KNOTS ( 'NONE', 3,
 ( #9347, #31167, #25545, #51912, #36427, #57882, #42045, #68439, #63168, #45944, #41368, #15318, #8673, #58224, #67411, #30811, #9701, #13934, #36781, #9017, #14288, #52596, #3719, #19557, #57544, #4417, #25881, #68768, #30127, #52258, #20583, #4080, #56855, #19202, #41017, #51578, #24842, #46281, #46980, #35748, #57199, #25198, #46633, #161, #516, #17026 ),
 .UNSPECIFIED., .F., .F.,
 ( 4, 2, 2, 2, 2, 2, 2, 2, 2, 2, 2, 2, 2, 2, 2, 2, 2, 2, 2, 2, 2, 2, 4 ),
 ( 0.02584318557310394740, 0.02743529570732768444, 0.02823135077443953908, 0.02902740584155139719, 0.03061951597577510994, 0.03221162610999882270, 0.03380373624422253892, 0.03459979131133440050, 0.03539584637844626902, 0.03619190144555813060, 0.03698795651266999218, 0.03858006664689372228, 0.03937612171400558386, 0.04017217678111744544, 0.04096823184822930702, 0.04176428691534117554, 0.04335639704956488483, 0.04494850718378860799, 0.04654061731801232421, 0.04813272745223604043, 0.04892878251934790201, 0.04972483758645974972, 0.05131694772068350757 ),
 .UNSPECIFIED. ) ;
#18443 = LINE ( 'NONE', #17388, #27619 ) ;
#18444 = EDGE_CURVE ( 'NONE', #454, #40730, #65339, .T. ) ;
#18445 = CARTESIAN_POINT ( 'NONE',  ( -5.416136198635856935, 6.745992685878681172, 57.35339821038935781 ) ) ;
#18446 = EDGE_LOOP ( 'NONE', ( #24342, #16850, #5267, #18222 ) ) ;
#18448 = CARTESIAN_POINT ( 'NONE',  ( 278.7021502624938876, 21.46117544541993638, 4.839652729015472943 ) ) ;
#18447 = VECTOR ( 'NONE', #8224, 1000.000000000000000 ) ;
#18449 = CARTESIAN_POINT ( 'NONE',  ( 150.7770046255792522, 53.87214803240241423, 67.14805320493677243 ) ) ;
#18450 = DIRECTION ( 'NONE',  ( 1.000000000000000000, 0.000000000000000000, 0.000000000000000000 ) ) ;
#18451 = ADVANCED_FACE ( 'NONE', ( #54411 ), #18211, .T. ) ;
#18452 = DIRECTION ( 'NONE',  ( -0.000000000000000000, -1.000000000000000000, 0.000000000000000000 ) ) ;
#18453 = EDGE_CURVE ( 'NONE', #68783, #42507, #60045, .T. ) ;
#18454 = CARTESIAN_POINT ( 'NONE',  ( 63.01563776193090405, 13.70579113808097382, -62.56524142263340593 ) ) ;
#18455 = EDGE_CURVE ( 'NONE', #38758, #12492, #17129, .T. ) ;
#18456 = AXIS2_PLACEMENT_3D ( 'NONE', #57201, #57546, #9019 ) ;
#18457 = ORIENTED_EDGE ( 'NONE', *, *, #68283, .T. ) ;
#18458 = VECTOR ( 'NONE', #51216, 1000.000000000000000 ) ;
#18459 = CARTESIAN_POINT ( 'NONE',  ( -190.6985136298602015, 109.1272424661243434, -91.34903848884556510 ) ) ;
#18460 = VECTOR ( 'NONE', #1582, 1000.000000000000000 ) ;
#18461 = PLANE ( 'NONE',  #20354 ) ;
#18462 = EDGE_LOOP ( 'NONE', ( #1534, #61505, #63091, #67080 ) ) ;
#18463 = VERTEX_POINT ( 'NONE', #39995 ) ;
#18464 = DIRECTION ( 'NONE',  ( 1.000000000000000000, 0.000000000000000000, 0.000000000000000000 ) ) ;
#18465 = CARTESIAN_POINT ( 'NONE',  ( 157.4703587214989113, 58.92748579479260229, 44.40946747225338953 ) ) ;
#18466 = CARTESIAN_POINT ( 'NONE',  ( 422.4999999999999432, -18.06806526123148160, 378.0000000000000000 ) ) ;
#18467 = ORIENTED_EDGE ( 'NONE', *, *, #61492, .T. ) ;
#18468 = CARTESIAN_POINT ( 'NONE',  ( 112.5612011511789916, 31.08353758940340583, 56.80732943995488426 ) ) ;
#18469 = CARTESIAN_POINT ( 'NONE',  ( -173.9548930713590948, 88.06040582145364226, 4.011895594186154490 ) ) ;
#18470 = CARTESIAN_POINT ( 'NONE',  ( -0.3249717932738292459, 6.518578686837482650, 11.25919877780879119 ) ) ;
#18471 = CARTESIAN_POINT ( 'NONE',  ( -80.54915509118116290, 24.12810583352861826, 30.65442206072611597 ) ) ;
#18472 = CARTESIAN_POINT ( 'NONE',  ( -24.95010104166213694, 9.631487977190600347, -12.20383126445008948 ) ) ;
#18473 = LINE ( 'NONE', #39921, #64588 ) ;
#18474 = ORIENTED_EDGE ( 'NONE', *, *, #13190, .T. ) ;
#18475 = B_SPLINE_CURVE_WITH_KNOTS ( 'NONE', 3,
 ( #55619, #49635, #16933, #7087, #54913, #6737 ),
 .UNSPECIFIED., .F., .F.,
 ( 4, 2, 4 ),
 ( 0.03218932480516799310, 0.06469831007220608332, 0.09720729533924417354 ),
 .UNSPECIFIED. ) ;
#18476 = CARTESIAN_POINT ( 'NONE',  ( 78.57571471437145760, 6.000000000000000000, -30.00000000000000000 ) ) ;
#18477 = CARTESIAN_POINT ( 'NONE',  ( -75.00636493611888511, 22.03142602679957207, 17.63766438757768995 ) ) ;
#18478 = CARTESIAN_POINT ( 'NONE',  ( 46.76970795284346138, 9.482505412758889918, -41.65468810189092608 ) ) ;
#18479 = CARTESIAN_POINT ( 'NONE',  ( 175.0857681883884140, 74.13486472930382831, 94.99999999999866418 ) ) ;
#18481 = ORIENTED_EDGE ( 'NONE', *, *, #9993, .F. ) ;
#18480 = CARTESIAN_POINT ( 'NONE',  ( 5.799999999999999822, 4.618802153517001408, -8.000000000000000000 ) ) ;
#18482 = CARTESIAN_POINT ( 'NONE',  ( -20.06363827490053708, -32.66413954409357245, 13.32819299319723427 ) ) ;
#18483 = ORIENTED_EDGE ( 'NONE', *, *, #14, .F. ) ;
#18484 = CARTESIAN_POINT ( 'NONE',  ( -149.0732005398558329, 63.81212100765652906, 72.55592966969389579 ) ) ;
#18485 = CARTESIAN_POINT ( 'NONE',  ( 79.13041963748371188, 18.04952109592811738, 36.69187788337345069 ) ) ;
#18486 = DIRECTION ( 'NONE',  ( 0.000000000000000000, 0.000000000000000000, 1.000000000000000000 ) ) ;
#18487 = CARTESIAN_POINT ( 'NONE',  ( 187.5325688887158435, 85.37769363979909087, -13.01233762806074168 ) ) ;
#18488 = CARTESIAN_POINT ( 'NONE',  ( 136.1310312718402713, 42.81430973242787985, -9.516980025434266466 ) ) ;
#18489 = DIRECTION ( 'NONE',  ( -1.282270072030875824E-16, -2.146158602472697874E-16, 1.000000000000000000 ) ) ;
#18490 = CARTESIAN_POINT ( 'NONE',  ( -179.2128128997735246, 95.75254520622988252, -19.77096022645222106 ) ) ;
#18491 = EDGE_CURVE ( 'NONE', #30189, #12795, #18969, .T. ) ;
#18492 = AXIS2_PLACEMENT_3D ( 'NONE', #7674, #66771, #66427 ) ;
#18493 = CARTESIAN_POINT ( 'NONE',  ( -152.9121563765243934, 67.12206067149027433, -35.62635434278646329 ) ) ;
#18494 = ORIENTED_EDGE ( 'NONE', *, *, #43804, .T. ) ;
#18495 = ORIENTED_EDGE ( 'NONE', *, *, #29789, .T. ) ;
#18496 = CARTESIAN_POINT ( 'NONE',  ( 104.3805245147141818, 26.26278144139195447, 59.25150731018273831 ) ) ;
#18497 = CARTESIAN_POINT ( 'NONE',  ( 0.000000000000000000, 0.000000000000000000, 40.00000000000003553 ) ) ;
#18498 = CARTESIAN_POINT ( 'NONE',  ( 209.3223706822284100, 0.000000000000000000, 31.44247402469554942 ) ) ;
#18499 = VECTOR ( 'NONE', #45598, 1000.000000000000000 ) ;
#18500 = CARTESIAN_POINT ( 'NONE',  ( -42.36049017605873956, -61.90437280228297112, 170.0000000000000000 ) ) ;
#18501 = DIRECTION ( 'NONE',  ( 0.5877852522924685852, 0.8090169943749507819, -0.000000000000000000 ) ) ;
#18502 = CARTESIAN_POINT ( 'NONE',  ( -107.7893514267588273, 35.66840175773126731, 59.75090616082049166 ) ) ;
#18503 = AXIS2_PLACEMENT_3D ( 'NONE', #57279, #8754, #41447 ) ;
#18504 = CARTESIAN_POINT ( 'NONE',  ( -29.51060362117876323, 9.282716514427262311, -50.06914130735744095 ) ) ;
#18505 = LINE ( 'NONE', #29069, #37427 ) ;
#18506 = ORIENTED_EDGE ( 'NONE', *, *, #27230, .T. ) ;
#18507 = EDGE_CURVE ( 'NONE', #7734, #18523, #23129, .T. ) ;
#18508 = VERTEX_POINT ( 'NONE', #67099 ) ;
#18509 = AXIS2_PLACEMENT_3D ( 'NONE', #3757, #34743, #19584 ) ;
#18510 = ORIENTED_EDGE ( 'NONE', *, *, #52020, .F. ) ;
#18511 = DIRECTION ( 'NONE',  ( -0.000000000000000000, 1.000000000000000000, -0.000000000000000000 ) ) ;
#18512 = CIRCLE ( 'NONE', #48798, 30.00000000000000000 ) ;
#18513 = CYLINDRICAL_SURFACE ( 'NONE', #17274, 7.500000000000013323 ) ;
#18514 = LINE ( 'NONE', #33312, #55494 ) ;
#18515 = DIRECTION ( 'NONE',  ( -1.000000000000000000, -1.850550996349095901E-16, -1.228197773518735191E-20 ) ) ;
#18516 = CARTESIAN_POINT ( 'NONE',  ( 106.0271074675581673, -21.78879721737672526, -3.053546265906987855 ) ) ;
#18517 = ADVANCED_FACE ( 'NONE', ( #14307 ), #68459, .T. ) ;
#18518 = CARTESIAN_POINT ( 'NONE',  ( 57.84269266929310049, -33.10328523389011934, 34.48241823993598842 ) ) ;
#18519 = CARTESIAN_POINT ( 'NONE',  ( -2.999999999999992450, 0.000000000000000000, 0.000000000000000000 ) ) ;
#18520 = ADVANCED_FACE ( 'NONE', ( #62496 ), #67427, .F. ) ;
#18521 = CARTESIAN_POINT ( 'NONE',  ( 62.05396267233468421, 13.48332220860126185, 29.85900607173965682 ) ) ;
#18522 = DIRECTION ( 'NONE',  ( -0.000000000000000000, -0.000000000000000000, 1.000000000000000000 ) ) ;
#18523 = VERTEX_POINT ( 'NONE', #18888 ) ;
#18524 = CARTESIAN_POINT ( 'NONE',  ( 24.36509522349081536, -70.94296747916753532, 43.58025477438756923 ) ) ;
#18525 = CARTESIAN_POINT ( 'NONE',  ( 0.000000000000000000, 0.000000000000000000, 73.58025477438756923 ) ) ;
#18526 = CARTESIAN_POINT ( 'NONE',  ( -190.6985136298601731, 109.1272424661242582, -46.56223028809779407 ) ) ;
#18527 = CARTESIAN_POINT ( 'NONE',  ( -143.8566410313463280, 59.53044870492033880, 16.33386445224493144 ) ) ;
#18528 = FACE_OUTER_BOUND ( 'NONE', #8559, .T. ) ;
#18529 = DIRECTION ( 'NONE',  ( 0.000000000000000000, 0.000000000000000000, 1.000000000000000000 ) ) ;
#18530 = CARTESIAN_POINT ( 'NONE',  ( 129.5225439633634892, 40.02995148249141266, -22.81789598513682549 ) ) ;
#18531 = VERTEX_POINT ( 'NONE', #57560 ) ;
#18532 = DIRECTION ( 'NONE',  ( 0.9998063756620102493, 0.01967768242440563753, -8.868226791112241738E-15 ) ) ;
#18533 = CARTESIAN_POINT ( 'NONE',  ( 128.3889472838589256, 39.37765603157611594, -38.36644464280026057 ) ) ;
#18534 = CARTESIAN_POINT ( 'NONE',  ( -38.54237244144231056, 11.89088379031760034, -40.39760444057212396 ) ) ;
#18535 = EDGE_CURVE ( 'NONE', #34756, #48801, #39441, .T. ) ;
#18536 = DIRECTION ( 'NONE',  ( 0.000000000000000000, 1.000000000000000000, -0.000000000000000000 ) ) ;
#18537 = CARTESIAN_POINT ( 'NONE',  ( -190.6985136298602015, 109.1272424661243434, -37.65993730791821292 ) ) ;
#18538 = VERTEX_POINT ( 'NONE', #35765 ) ;
#18539 = CARTESIAN_POINT ( 'NONE',  ( -121.5677746760273834, 43.71038933438992302, -36.26883008344502457 ) ) ;
#18540 = EDGE_CURVE ( 'NONE', #65894, #16032, #16977, .T. ) ;
#18541 = CARTESIAN_POINT ( 'NONE',  ( -46.66904755831212981, -15.55634918610397222, 85.00100000000000477 ) ) ;
#18542 = CARTESIAN_POINT ( 'NONE',  ( -142.2166122762983491, 58.23386571792348576, 93.70268379333128905 ) ) ;
#18543 = AXIS2_PLACEMENT_3D ( 'NONE', #38467, #5420, #43035 ) ;
#18544 = CARTESIAN_POINT ( 'NONE',  ( 18.89356949897907967, -62.19351277735683681, 40.00000000000003553 ) ) ;
#18545 = ORIENTED_EDGE ( 'NONE', *, *, #34312, .F. ) ;
#18546 = CARTESIAN_POINT ( 'NONE',  ( 447.3372781065086201, 217.8591479523844612, 78.55029585798806124 ) ) ;
#18547 = CARTESIAN_POINT ( 'NONE',  ( 197.5334904971816741, 97.00846725096931777, -41.58470127245635695 ) ) ;
#18548 = CARTESIAN_POINT ( 'NONE',  ( -156.9232798886536955, 72.10386843399173529, 37.06393818096253767 ) ) ;
#18549 = CARTESIAN_POINT ( 'NONE',  ( 22.52576749827964164, 6.809805260274350402, -46.35021364760256546 ) ) ;
#18550 = VECTOR ( 'NONE', #66655, 1000.000000000000000 ) ;
#18552 = EDGE_LOOP ( 'NONE', ( #65546, #9077, #16706, #1228 ) ) ;
#18551 = CARTESIAN_POINT ( 'NONE',  ( 115.0606351894211201, 32.29586232625067055, 4.497561513806664024 ) ) ;
#18553 = CARTESIAN_POINT ( 'NONE',  ( -26.69131247781301752, 59.26697088776972322, 170.0000000000000000 ) ) ;
#18554 = VECTOR ( 'NONE', #50047, 1000.000000000000000 ) ;
#18555 = ORIENTED_EDGE ( 'NONE', *, *, #1826, .F. ) ;
#18556 = ORIENTED_EDGE ( 'NONE', *, *, #26148, .F. ) ;
#18557 = CARTESIAN_POINT ( 'NONE',  ( 173.6024011093111028, 72.73634049052010653, 36.20546616912848492 ) ) ;
#18558 = VECTOR ( 'NONE', #44861, 1000.000000000000000 ) ;
#18559 = CARTESIAN_POINT ( 'NONE',  ( -38.78626392836186909, 10.91334659013840103, -95.00000000000133582 ) ) ;
#18561 = ORIENTED_EDGE ( 'NONE', *, *, #38763, .T. ) ;
#18560 = CARTESIAN_POINT ( 'NONE',  ( -8.810383862755527318, 7.965311326754785703, -62.31117607751706089 ) ) ;
#18562 = DIRECTION ( 'NONE',  ( -1.000000000000000000, -0.000000000000000000, -0.000000000000000000 ) ) ;
#18563 = CARTESIAN_POINT ( 'NONE',  ( -24.18158274621863768, 9.527343002918312820, 35.76142679940522129 ) ) ;
#18564 = FACE_BOUND ( 'NONE', #33083, .T. ) ;
#18565 = ORIENTED_EDGE ( 'NONE', *, *, #960, .F. ) ;
#18566 = CARTESIAN_POINT ( 'NONE',  ( 207.8407634284391463, 112.5209879629464069, -63.84769439563109472 ) ) ;
#18567 = EDGE_CURVE ( 'NONE', #34081, #41081, #46649, .T. ) ;
#18568 = CARTESIAN_POINT ( 'NONE',  ( 141.3586046882815310, 47.34625111366352002, 36.50144467960451777 ) ) ;
#18569 = ADVANCED_FACE ( 'NONE', ( #29438 ), #9370, .F. ) ;
#18570 = CARTESIAN_POINT ( 'NONE',  ( -430.1627218934915504, 399.9999999999996021, 91.05029585798840230 ) ) ;
#18571 = CARTESIAN_POINT ( 'NONE',  ( 133.8566784816069060, 42.60093787723655367, 71.35489142945907304 ) ) ;
#18572 = FACE_OUTER_BOUND ( 'NONE', #17242, .T. ) ;
#18573 = ORIENTED_EDGE ( 'NONE', *, *, #11327, .F. ) ;
#18574 = ORIENTED_EDGE ( 'NONE', *, *, #36060, .F. ) ;
#18575 = ORIENTED_EDGE ( 'NONE', *, *, #46533, .F. ) ;
#18576 = DIRECTION ( 'NONE',  ( -1.000000000000000000, 0.000000000000000000, 0.000000000000000000 ) ) ;
#18577 = CARTESIAN_POINT ( 'NONE',  ( 0.000000000000000000, 5.000000000000000000, 2.000000000000001776 ) ) ;
#18578 = CARTESIAN_POINT ( 'NONE',  ( -53.36220652957118915, 14.23444203126018337, -89.08613737882753014 ) ) ;
#18579 = CARTESIAN_POINT ( 'NONE',  ( 111.9975424824652634, 295.8720703627916464, 535.5371946177799600 ) ) ;
#18580 = CARTESIAN_POINT ( 'NONE',  ( -45.00000000000002132, 20.00000000000000355, 4.000000000000000000 ) ) ;
#18581 = DIRECTION ( 'NONE',  ( -1.000000000000000000, 0.000000000000000000, 0.000000000000000000 ) ) ;
#18582 = CARTESIAN_POINT ( 'NONE',  ( -62.29227808534486144, 17.79399661465416926, 93.49242969035836381 ) ) ;
#18583 = ADVANCED_FACE ( 'NONE', ( #24526 ), #66432, .T. ) ;
#18584 = ORIENTED_EDGE ( 'NONE', *, *, #49564, .F. ) ;
#18585 = CARTESIAN_POINT ( 'NONE',  ( -107.0544991134679691, 36.41543129049375693, 32.22994866574824613 ) ) ;
#18586 = ORIENTED_EDGE ( 'NONE', *, *, #54298, .T. ) ;
#18587 = CONICAL_SURFACE ( 'NONE', #42136, 75.31295361348104223, 1.273485274044411586 ) ;
#18588 = CARTESIAN_POINT ( 'NONE',  ( 32.67604581760325289, 7.629767527669977234, 40.74140668430740675 ) ) ;
#18589 = FACE_OUTER_BOUND ( 'NONE', #4190, .T. ) ;
#18590 = EDGE_CURVE ( 'NONE', #36560, #21953, #40677, .T. ) ;
#18591 = VERTEX_POINT ( 'NONE', #67778 ) ;
#18592 = CARTESIAN_POINT ( 'NONE',  ( -7.825402957745085430, 7.899365992529246761, 45.11558103944722120 ) ) ;
#18593 = DIRECTION ( 'NONE',  ( 0.000000000000000000, 1.000000000000000000, 0.000000000000000000 ) ) ;
#18594 = EDGE_CURVE ( 'NONE', #46320, #35107, #61924, .T. ) ;
#18596 = CARTESIAN_POINT ( 'NONE',  ( -5.000000000000058620, -26.11269837220806522, 2.000000000000001776 ) ) ;
#18595 = AXIS2_PLACEMENT_3D ( 'NONE', #1722, #28448, #48480 ) ;
#18597 = CARTESIAN_POINT ( 'NONE',  ( 0.000000000000000000, 70.00000000000000000, -30.00000000000000000 ) ) ;
#18598 = CARTESIAN_POINT ( 'NONE',  ( -11.78188048797445653, 8.190559674012728664, -49.29436824631886083 ) ) ;
#18599 = CARTESIAN_POINT ( 'NONE',  ( 60.82895951008336510, 30.68107831874607072, 41.38025477438755928 ) ) ;
#18600 = AXIS2_PLACEMENT_3D ( 'NONE', #43927, #54482, #27407 ) ;
#18601 = CIRCLE ( 'NONE', #47803, 243.4957430088094839 ) ;
#18602 = ORIENTED_EDGE ( 'NONE', *, *, #12454, .T. ) ;
#18603 = CARTESIAN_POINT ( 'NONE',  ( 0.000000000000000000, 190.0000000000000000, 0.000000000000000000 ) ) ;
#18604 = DIRECTION ( 'NONE',  ( -0.000000000000000000, -1.000000000000000000, -0.000000000000000000 ) ) ;
#18605 = ORIENTED_EDGE ( 'NONE', *, *, #3121, .F. ) ;
#18606 = AXIS2_PLACEMENT_3D ( 'NONE', #40755, #35137, #24601 ) ;
#18607 = DIRECTION ( 'NONE',  ( 0.000000000000000000, 0.000000000000000000, -1.000000000000000000 ) ) ;
#18608 = CARTESIAN_POINT ( 'NONE',  ( -55.05276343752909440, 15.72344139423348430, 57.16187836339483397 ) ) ;
#18609 = LINE ( 'NONE', #7009, #42040 ) ;
#18610 = VERTEX_POINT ( 'NONE', #51255 ) ;
#18611 = CARTESIAN_POINT ( 'NONE',  ( 0.000000000000000000, 190.0000000000000000, 0.000000000000000000 ) ) ;
#18612 = VECTOR ( 'NONE', #68065, 1000.000000000000000 ) ;
#18613 = CARTESIAN_POINT ( 'NONE',  ( 150.0516754638056511, 53.34587188591232376, -71.60412932141241527 ) ) ;
#18614 = CARTESIAN_POINT ( 'NONE',  ( -97.88309373898358956, 30.60238467438961862, -21.76468407524414417 ) ) ;
#18615 = CARTESIAN_POINT ( 'NONE',  ( 136.1081004736419402, 42.80058051492065374, -50.68110568597454346 ) ) ;
#18616 = VECTOR ( 'NONE', #52054, 1000.000000000000000 ) ;
#18617 = VERTEX_POINT ( 'NONE', #13953 ) ;
#18618 = CARTESIAN_POINT ( 'NONE',  ( -124.9927180788553898, 45.90286323198616714, 45.57935678244711397 ) ) ;
#18619 = EDGE_LOOP ( 'NONE', ( #47590, #16308, #12317, #11208 ) ) ;
#18620 = DIRECTION ( 'NONE',  ( 0.000000000000000000, 0.000000000000000000, 1.000000000000000000 ) ) ;
#18621 = CARTESIAN_POINT ( 'NONE',  ( 182.7720841008444097, 80.32850885226589810, 2.653340975719014949 ) ) ;
#18622 = DIRECTION ( 'NONE',  ( -1.000000000000000000, 0.000000000000000000, 0.000000000000000000 ) ) ;
#18623 = EDGE_CURVE ( 'NONE', #61739, #5291, #28183, .T. ) ;
#18624 = DIRECTION ( 'NONE',  ( -0.000000000000000000, -0.000000000000000000, -1.000000000000000000 ) ) ;
#18625 = CARTESIAN_POINT ( 'NONE',  ( 149.0250918491436778, 0.000000000000000000, -14.43565316649551811 ) ) ;
#18626 = FACE_OUTER_BOUND ( 'NONE', #24803, .T. ) ;
#18627 = VERTEX_POINT ( 'NONE', #41386 ) ;
#18628 = DIRECTION ( 'NONE',  ( 0.000000000000000000, 0.000000000000000000, 1.000000000000000000 ) ) ;
#18629 = DIRECTION ( 'NONE',  ( 1.000000000000000000, 0.000000000000000000, 0.000000000000000000 ) ) ;
#18630 = CARTESIAN_POINT ( 'NONE',  ( 66.94779593213117153, 13.61918177102166361, 70.54877072614397093 ) ) ;
#18631 = CARTESIAN_POINT ( 'NONE',  ( 159.2325040199867203, 60.31699144791975442, 17.41041423679662259 ) ) ;
#18632 = CARTESIAN_POINT ( 'NONE',  ( 1.667562369267757916, -64.99262834925670518, 41.38025477438755928 ) ) ;
#18633 = B_SPLINE_CURVE_WITH_KNOTS ( 'NONE', 3,
 ( #62878, #19973, #30180, #45662, #67812, #3782, #51292, #68166, #67468, #67141, #57255, #51634, #62175, #19262, #14678, #19615, #34769, #40716, #18578, #30520, #56555, #13995, #9068, #35451 ),
 .UNSPECIFIED., .F., .F.,
 ( 4, 2, 2, 2, 2, 2, 2, 2, 2, 2, 2, 4 ),
 ( 0.000000000000000000, 0.001312585275339593583, 0.002625170550679187167, 0.003937755826018780533, 0.004594048463688570928, 0.005250341101358362191, 0.006562926376697901347, 0.007219219014367670925, 0.007875511652037439636, 0.009188096927376999609, 0.009844389565046790871, 0.01050068220271658387 ),
 .UNSPECIFIED. ) ;
#18634 = EDGE_LOOP ( 'NONE', ( #57150, #997, #27031 ) ) ;
#18635 = CARTESIAN_POINT ( 'NONE',  ( 162.8034185388970059, 63.22443559329413176, -22.07472928994418737 ) ) ;
#18636 = CARTESIAN_POINT ( 'NONE',  ( 109.9975424824652634, 172.0000000000001705, 529.9060149868646477 ) ) ;
#18637 = VERTEX_POINT ( 'NONE', #56512 ) ;
#18638 = VECTOR ( 'NONE', #62079, 1000.000000000000000 ) ;
#18639 = CARTESIAN_POINT ( 'NONE',  ( 70.45451534980408326, 15.56315969138428557, 63.16980466599618182 ) ) ;
#18640 = CARTESIAN_POINT ( 'NONE',  ( 132.3624812100102304, 40.52933787053994052, -89.85320261638416639 ) ) ;
#18641 = VECTOR ( 'NONE', #39015, 1000.000000000000000 ) ;
#18642 = ORIENTED_EDGE ( 'NONE', *, *, #6323, .F. ) ;
#18643 = CARTESIAN_POINT ( 'NONE',  ( 164.1352994389932007, 64.33767534192698179, -47.07368343251171439 ) ) ;
#18644 = CARTESIAN_POINT ( 'NONE',  ( -26.83517958587572494, -59.60356471962950309, 6.377659838150123602E-18 ) ) ;
#18645 = CARTESIAN_POINT ( 'NONE',  ( 51.85299110299440173, 39.21848821248450179, 43.58025477438756923 ) ) ;
#18646 = EDGE_CURVE ( 'NONE', #62158, #1104, #3898, .T. ) ;
#18647 = CARTESIAN_POINT ( 'NONE',  ( 159.2319614735956179, 59.03334608081210177, -50.92782365232224606 ) ) ;
#18648 = AXIS2_PLACEMENT_3D ( 'NONE', #23723, #11763, #22323 ) ;
#18649 = AXIS2_PLACEMENT_3D ( 'NONE', #18714, #60576, #2195 ) ;
#18650 = EDGE_CURVE ( 'NONE', #2615, #17123, #40022, .T. ) ;
#18651 = EDGE_LOOP ( 'NONE', ( #3213, #53932, #7657, #61442 ) ) ;
#18652 = CARTESIAN_POINT ( 'NONE',  ( -99.10674985723787245, 32.31836975419498970, 4.362585564299135577 ) ) ;
#18653 = EDGE_CURVE ( 'NONE', #47821, #15908, #27285, .T. ) ;
#18654 = CIRCLE ( 'NONE', #57969, 245.3095347406802773 ) ;
#18655 = EDGE_CURVE ( 'NONE', #52004, #35148, #12844, .T. ) ;
#18656 = CARTESIAN_POINT ( 'NONE',  ( 65.29852862277677161, 14.24903302186932841, 83.85046607615447556 ) ) ;
#18657 = DIRECTION ( 'NONE',  ( -1.000000000000000000, 0.000000000000000000, 0.000000000000000000 ) ) ;
#18658 = AXIS2_PLACEMENT_3D ( 'NONE', #26451, #26793, #48219 ) ;
#18659 = CARTESIAN_POINT ( 'NONE',  ( 79.12879321038293767, 18.04902206524927166, -16.24110779498484547 ) ) ;
#18660 = EDGE_CURVE ( 'NONE', #54950, #43717, #31605, .T. ) ;
#18661 = CARTESIAN_POINT ( 'NONE',  ( -165.6398193834832853, 79.16932278174807891, 37.71096669259078737 ) ) ;
#18662 = CARTESIAN_POINT ( 'NONE',  ( 37.76393697770887314, 9.215659441295981580, -89.47842326396359169 ) ) ;
#18663 = CARTESIAN_POINT ( 'NONE',  ( 129.5193594945039308, 38.86618897895344560, -64.23098118280410063 ) ) ;
#18664 = VERTEX_POINT ( 'NONE', #50467 ) ;
#18665 = DIRECTION ( 'NONE',  ( 1.000000000000000000, 0.000000000000000000, 0.000000000000000000 ) ) ;
#18666 = CARTESIAN_POINT ( 'NONE',  ( -14.93280618462406650, 8.469244267267916015, 66.86749277915568257 ) ) ;
#18667 = EDGE_LOOP ( 'NONE', ( #61356, #55529 ) ) ;
#18668 = EDGE_CURVE ( 'NONE', #13178, #61651, #9120, .T. ) ;
#18669 = CARTESIAN_POINT ( 'NONE',  ( -156.9232798886536671, 72.10386843399172108, -43.46971359042848349 ) ) ;
#18670 = CARTESIAN_POINT ( 'NONE',  ( 208.9585401441656245, 114.1617785893844399, -10.79275703727707203 ) ) ;
#18671 = CARTESIAN_POINT ( 'NONE',  ( -442.6627218934914367, 399.9999999999998863, -141.4497041420118251 ) ) ;
#18672 = CARTESIAN_POINT ( 'NONE',  ( -0.5178428571329642960, 7.532057582089303871, 39.32162052339865710 ) ) ;
#18673 = FACE_OUTER_BOUND ( 'NONE', #2666, .T. ) ;
#18674 = CARTESIAN_POINT ( 'NONE',  ( -52.66507163626135224, 14.05394608175174476, -62.43469777390021136 ) ) ;
#18675 = CARTESIAN_POINT ( 'NONE',  ( -0.3732240621745012144, 7.527003275829102336, -15.09420860379144891 ) ) ;
#18676 = DIRECTION ( 'NONE',  ( 0.000000000000000000, 0.000000000000000000, 1.000000000000000000 ) ) ;
#18677 = CARTESIAN_POINT ( 'NONE',  ( -59.57733000654213384, 15.94108165424592016, 4.971641029624789709 ) ) ;
#18678 = ORIENTED_EDGE ( 'NONE', *, *, #60333, .T. ) ;
#18679 = DIRECTION ( 'NONE',  ( 0.000000000000000000, 3.469446951953616038E-17, -1.000000000000000000 ) ) ;
#18680 = EDGE_LOOP ( 'NONE', ( #44285, #28630, #15149, #64999 ) ) ;
#18681 = CARTESIAN_POINT ( 'NONE',  ( 109.7774723066848850, 28.66666416591279187, -77.76698815611739235 ) ) ;
#18682 = EDGE_CURVE ( 'NONE', #65787, #9934, #55142, .T. ) ;
#18683 = FACE_OUTER_BOUND ( 'NONE', #37789, .T. ) ;
#18684 = ADVANCED_FACE ( 'NONE', ( #43777 ), #17043, .T. ) ;
#18685 = CARTESIAN_POINT ( 'NONE',  ( 42.03492317486906416, 8.766487167902386801, 57.23152860898684224 ) ) ;
#18686 = CARTESIAN_POINT ( 'NONE',  ( 141.9165763529819344, 242.0000000000000000, 129.0000000000000000 ) ) ;
#18687 = CARTESIAN_POINT ( 'NONE',  ( 0.000000000000000000, 0.000000000000000000, 10.00000000000000000 ) ) ;
#18688 = CARTESIAN_POINT ( 'NONE',  ( 15.78827728214693416, -170.0000000000000000, 10.67015708224156079 ) ) ;
#18689 = CARTESIAN_POINT ( 'NONE',  ( 0.000000000000000000, 0.000000000000000000, 5.000000000000000000 ) ) ;
#18690 = CARTESIAN_POINT ( 'NONE',  ( -171.4867114763003713, 85.32693843184999594, 57.83474805468819113 ) ) ;
#18691 = ORIENTED_EDGE ( 'NONE', *, *, #64559, .F. ) ;
#18692 = ORIENTED_EDGE ( 'NONE', *, *, #22283, .T. ) ;
#18693 = CARTESIAN_POINT ( 'NONE',  ( 0.000000000000000000, 0.000000000000000000, 19.99999999999998934 ) ) ;
#18694 = CARTESIAN_POINT ( 'NONE',  ( -45.81425895439424067, 46.10914959592843587, 40.00000000000003553 ) ) ;
#18695 = CARTESIAN_POINT ( 'NONE',  ( -36.11269837220801548, 31.11269837220812207, 2.000000000000001776 ) ) ;
#18696 = CIRCLE ( 'NONE', #62477, 5.000000000000004441 ) ;
#18697 = CARTESIAN_POINT ( 'NONE',  ( 103.5849290181279230, 27.01613348792539071, 60.49401056488979833 ) ) ;
#18698 = CARTESIAN_POINT ( 'NONE',  ( -28.32746765835526048, 69.45586423092609607, 170.0000000000000000 ) ) ;
#18699 = AXIS2_PLACEMENT_3D ( 'NONE', #10537, #9522, #58384 ) ;
#18700 = CARTESIAN_POINT ( 'NONE',  ( 55.64941011647476898, 12.11006142851270617, -14.90257183315545397 ) ) ;
#18701 = VERTEX_POINT ( 'NONE', #6512 ) ;
#18702 = LINE ( 'NONE', #30298, #63729 ) ;
#18703 = CYLINDRICAL_SURFACE ( 'NONE', #21096, 4.999999999999990230 ) ;
#18704 = CARTESIAN_POINT ( 'NONE',  ( -82.32931163805226049, 23.75065981441937879, -22.32008095138030157 ) ) ;
#18705 = DIRECTION ( 'NONE',  ( -1.000000000000000000, -0.000000000000000000, -0.000000000000000000 ) ) ;
#18706 = PLANE ( 'NONE',  #50026 ) ;
#18707 = CARTESIAN_POINT ( 'NONE',  ( 8.581702583691640740, 6.376899981419158259, -94.58808349776735724 ) ) ;
#18708 = CARTESIAN_POINT ( 'NONE',  ( -23.95089599695169014, 9.496585844566151735, -70.15026316693982267 ) ) ;
#18709 = VECTOR ( 'NONE', #66024, 1000.000000000000000 ) ;
#18710 = ORIENTED_EDGE ( 'NONE', *, *, #21537, .F. ) ;
#18711 = DIRECTION ( 'NONE',  ( 1.000000000000000000, 0.000000000000000000, 0.000000000000000000 ) ) ;
#18712 = CARTESIAN_POINT ( 'NONE',  ( 0.000000000000000000, 10.00000000000000000, 0.000000000000000000 ) ) ;
#18713 = CARTESIAN_POINT ( 'NONE',  ( 37.46876540261053634, 9.179568636624027889, -77.21507226135139490 ) ) ;
#18714 = CARTESIAN_POINT ( 'NONE',  ( 204.6977192012829789, -170.0000000000000000, 90.39682191969680503 ) ) ;
#18715 = CARTESIAN_POINT ( 'NONE',  ( 210.5008983495071675, 116.4753531594350591, 68.30981121570347625 ) ) ;
#18716 = CARTESIAN_POINT ( 'NONE',  ( 79.14242532928582818, 17.00090225993928783, -69.65640399090251833 ) ) ;
#18717 = ORIENTED_EDGE ( 'NONE', *, *, #10824, .T. ) ;
#18718 = DIRECTION ( 'NONE',  ( 1.000000000000000000, 0.000000000000000000, 0.000000000000000000 ) ) ;
#18719 = CARTESIAN_POINT ( 'NONE',  ( -7.347286611336974360, -4.995646404165295706, -9.003039949738241177 ) ) ;
#18720 = EDGE_LOOP ( 'NONE', ( #36740, #1967, #18043, #22516, #63748, #15851 ) ) ;
#18721 = CARTESIAN_POINT ( 'NONE',  ( -78.66644367742111399, -170.0000000000000000, 45.41820113967312977 ) ) ;
#18722 = EDGE_LOOP ( 'NONE', ( #7175, #62608, #32869, #31796 ) ) ;
#18723 = CARTESIAN_POINT ( 'NONE',  ( -80.55742067659895156, 23.05042616197515315, -76.73329829129131952 ) ) ;
#18724 = CYLINDRICAL_SURFACE ( 'NONE', #42245, 7.500000000000013323 ) ;
#18725 = CARTESIAN_POINT ( 'NONE',  ( 94.02861641584115659, 23.15570573563315548, -71.41699682199956101 ) ) ;
#18726 = ORIENTED_EDGE ( 'NONE', *, *, #26052, .F. ) ;
#18727 = ORIENTED_EDGE ( 'NONE', *, *, #27059, .T. ) ;
#18728 = DIRECTION ( 'NONE',  ( 0.000000000000000000, 1.000000000000000000, 0.000000000000000000 ) ) ;
#18729 = CARTESIAN_POINT ( 'NONE',  ( -20.55634918610396866, 31.11269837220809009, 2.000000000000000000 ) ) ;
#18730 = CARTESIAN_POINT ( 'NONE',  ( 23.28785143291466397, 6.856621069835718174, 10.16897003589188841 ) ) ;
#18731 = ORIENTED_EDGE ( 'NONE', *, *, #33758, .T. ) ;
#18732 = PRODUCT_DEFINITION_SHAPE ( 'NONE', 'NONE',  #69609 ) ;
#18733 = ADVANCED_FACE ( 'NONE', ( #27959 ), #18461, .T. ) ;
#18734 = DIRECTION ( 'NONE',  ( 0.000000000000000000, -1.000000000000000000, 0.000000000000000000 ) ) ;
#18735 = AXIS2_PLACEMENT_3D ( 'NONE', #8908, #2330, #30705 ) ;
#18736 = CARTESIAN_POINT ( 'NONE',  ( 59.29474530993687154, 12.86968658439546509, -36.70420577007838858 ) ) ;
#18737 = CARTESIAN_POINT ( 'NONE',  ( -132.0870433264402948, 51.94057326482882075, -11.33156610799026609 ) ) ;
#18738 = CARTESIAN_POINT ( 'NONE',  ( 117.3110050642448101, 32.29133253383018598, -19.13666864001427470 ) ) ;
#18739 = CARTESIAN_POINT ( 'NONE',  ( 82.34401416830215226, 19.05992892018825557, -49.48157865267160105 ) ) ;
#18741 = ORIENTED_EDGE ( 'NONE', *, *, #63302, .T. ) ;
#18740 = FACE_OUTER_BOUND ( 'NONE', #25014, .T. ) ;
#18742 = ORIENTED_EDGE ( 'NONE', *, *, #26426, .F. ) ;
#18743 = EDGE_CURVE ( 'NONE', #33925, #28657, #24836, .T. ) ;
#18744 = VECTOR ( 'NONE', #1240, 1000.000000000000114 ) ;
#18745 = ORIENTED_EDGE ( 'NONE', *, *, #67407, .T. ) ;
#18746 = CARTESIAN_POINT ( 'NONE',  ( 290.0000000000000568, 0.000000000000000000, 0.000000000000000000 ) ) ;
#18747 = CARTESIAN_POINT ( 'NONE',  ( -55.05276343752910151, -170.0000000000000000, 64.66187836339484818 ) ) ;
#18748 = DIRECTION ( 'NONE',  ( 1.000000000000000000, 0.000000000000000000, 0.000000000000000000 ) ) ;
#18749 = LINE ( 'NONE', #40207, #63574 ) ;
#18750 = EDGE_CURVE ( 'NONE', #66549, #23198, #39287, .T. ) ;
#18751 = CIRCLE ( 'NONE', #34643, 498.0000000000000000 ) ;
#18752 = DIRECTION ( 'NONE',  ( 1.000000000000000000, 0.000000000000000000, 0.000000000000000000 ) ) ;
#18753 = CARTESIAN_POINT ( 'NONE',  ( -24.09190246691234805, 8.500289797445409690, -95.00000000000133582 ) ) ;
#18754 = CARTESIAN_POINT ( 'NONE',  ( 211.9552723536948520, 118.7100180530116518, 92.33883945253931813 ) ) ;
#18755 = CARTESIAN_POINT ( 'NONE',  ( -47.92160691800343386, 33.27200046441025449, 27.58472369410210945 ) ) ;
#18756 = CARTESIAN_POINT ( 'NONE',  ( -80.54915509118114869, 24.12810583352862182, 57.49897265118980982 ) ) ;
#18757 = DIRECTION ( 'NONE',  ( 1.000000000000000000, 0.000000000000000000, 0.000000000000000000 ) ) ;
#18758 = ORIENTED_EDGE ( 'NONE', *, *, #8619, .T. ) ;
#18759 = AXIS2_PLACEMENT_3D ( 'NONE', #21403, #16128, #37584 ) ;
#18760 = CARTESIAN_POINT ( 'NONE',  ( 8.679939806240508204, 7.383357464882122301, -13.76982068021760064 ) ) ;
#18761 = EDGE_LOOP ( 'NONE', ( #643, #37887, #885, #27656 ) ) ;
#18762 = ORIENTED_EDGE ( 'NONE', *, *, #23426, .F. ) ;
#18763 = EDGE_CURVE ( 'NONE', #21301, #13533, #46214, .T. ) ;
#18764 = CARTESIAN_POINT ( 'NONE',  ( 264.4165763529819628, -27.00000000000000355, 128.9999999999999716 ) ) ;
#18765 = CARTESIAN_POINT ( 'NONE',  ( 186.7642514597453101, 86.02880938169739977, -65.66567118133815484 ) ) ;
#18766 = CARTESIAN_POINT ( 'NONE',  ( -168.1839487819770511, 83.25723186408070831, 43.97232250669951981 ) ) ;
#18767 = LINE ( 'NONE', #10182, #25145 ) ;
#18768 = FACE_OUTER_BOUND ( 'NONE', #63805, .T. ) ;
#18769 = CARTESIAN_POINT ( 'NONE',  ( -104.5827168854524558, 33.96561401163044991, 4.021232942600325266 ) ) ;
#18770 = CARTESIAN_POINT ( 'NONE',  ( 444.9999999999999432, -35.00000000000000000, 2.000000000000000000 ) ) ;
#18771 = CARTESIAN_POINT ( 'NONE',  ( 128.0848616812662897, 38.04676222636084049, -38.70798055224722134 ) ) ;
#18772 = ORIENTED_EDGE ( 'NONE', *, *, #66585, .T. ) ;
#18773 = ORIENTED_EDGE ( 'NONE', *, *, #19891, .F. ) ;
#18774 = CARTESIAN_POINT ( 'NONE',  ( 437.3372781065085633, 395.0000000000001137, -136.4497041420117966 ) ) ;
#18775 = CARTESIAN_POINT ( 'NONE',  ( -8.811275908848671179, 6.956777180392053950, 3.320008556540252620 ) ) ;
#18776 = CARTESIAN_POINT ( 'NONE',  ( 3.318518101603014525, 7.321656987762867885, 5.929230630780102373E-15 ) ) ;
#18777 = CARTESIAN_POINT ( 'NONE',  ( -24.07146903340143140, 8.497560047608729406, -68.19585695038200868 ) ) ;
#18778 = CARTESIAN_POINT ( 'NONE',  ( 8.288104306525687193, 6.376394648992964598, 10.18357869276926309 ) ) ;
#18779 = EDGE_LOOP ( 'NONE', ( #4748, #51066, #19117, #26551 ) ) ;
#18780 = CARTESIAN_POINT ( 'NONE',  ( 46.23113030541875190, 10.41513832761375902, -66.85431394756601264 ) ) ;
#18781 = CARTESIAN_POINT ( 'NONE',  ( -58.33157376762797242, 16.63098604184965978, -62.81118730508888603 ) ) ;
#18782 = CARTESIAN_POINT ( 'NONE',  ( 181.0840389613909736, 78.60582251573005408, -63.06960825634327961 ) ) ;
#18783 = VECTOR ( 'NONE', #51679, 1000.000000000000000 ) ;
#18784 = LINE ( 'NONE', #67674, #7049 ) ;
#18785 = SURFACE_STYLE_USAGE ( .BOTH. , #28648 ) ;
#18786 = CARTESIAN_POINT ( 'NONE',  ( -165.9122696334864600, 79.44688201528255433, 9.386813235023986124 ) ) ;
#18787 = DIRECTION ( 'NONE',  ( -0.7071067811865476838, 0.000000000000000000, -0.7071067811865474617 ) ) ;
#18788 = DIRECTION ( 'NONE',  ( -0.000000000000000000, -0.000000000000000000, -1.000000000000000000 ) ) ;
#18789 = CARTESIAN_POINT ( 'NONE',  ( -0.3258398948454879207, 6.518608385615799250, 63.95880355785457994 ) ) ;
#18790 = ORIENTED_EDGE ( 'NONE', *, *, #10456, .T. ) ;
#18791 = B_SPLINE_CURVE_WITH_KNOTS ( 'NONE', 3,
 ( #37080, #63818, #10340, #4720, #26183, #53238, #26531, #26871, #46949, #69431, #9669, #21248, #42696, #41670, #64154, #48295, #127, #62787, #36052, #57507, #63128, #14929, #60273, #53926, #6096, #43031, #59554, #33894, #21932, #27910, #12435, #836, #32495, #49347, #48641, #55331, #1180, #32838, #59212, #54271, #17717, #484, #12088 ),
 .UNSPECIFIED., .F., .F.,
 ( 4, 2, 2, 2, 2, 2, 2, 2, 2, 2, 2, 2, 1, 2, 2, 2, 2, 2, 2, 2, 2, 4 ),
 ( 0.02358007599568759036, 0.02505677178601666347, 0.02579511968118119308, 0.02653346757634571923, 0.02801016336667479581, 0.02948685915700387239, 0.03022520705216840894, 0.03096355494733294550, 0.03244025073766201861, 0.03391694652799109866, 0.03539364231832017177, 0.03613199021348469098, 0.03687033810864921018, 0.03760868600381372939, 0.03834703389897824860, 0.03982372968930728008, 0.04130042547963631155, 0.04277712126996534303, 0.04351546916512986918, 0.04425381706029438145, 0.04573051285062339905, 0.04720720864095240971 ),
 .UNSPECIFIED. ) ;
#18792 = CARTESIAN_POINT ( 'NONE',  ( 276.9495076362458121, 21.63869423720476703, 3.975053342410747259 ) ) ;
#18793 = LINE ( 'NONE', #62041, #26239 ) ;
#18794 = DIRECTION ( 'NONE',  ( -0.000000000000000000, -1.000000000000000000, -0.000000000000000000 ) ) ;
#18795 = CARTESIAN_POINT ( 'NONE',  ( 427.4999999999999432, -18.06806526123148160, 0.000000000000000000 ) ) ;
#18796 = LINE ( 'NONE', #12838, #63686 ) ;
#18797 = AXIS2_PLACEMENT_3D ( 'NONE', #53563, #37742, #55572 ) ;
#18798 = EDGE_CURVE ( 'NONE', #5564, #52445, #25994, .T. ) ;
#18799 = CIRCLE ( 'NONE', #42345, 10.00000000000000178 ) ;
#18800 = VERTEX_POINT ( 'NONE', #67010 ) ;
#18801 = CARTESIAN_POINT ( 'NONE',  ( 50.98853755884140782, 395.0000000000004547, 96.05029585798814651 ) ) ;
#18802 = CARTESIAN_POINT ( 'NONE',  ( -5.355005115540905969, -6.145890662064667609, -0.08224679563972382701 ) ) ;
#18803 = EDGE_LOOP ( 'NONE', ( #23315, #46564, #66587 ) ) ;
#18804 = EDGE_CURVE ( 'NONE', #8633, #64962, #45182, .T. ) ;
#18805 = AXIS2_PLACEMENT_3D ( 'NONE', #68072, #67721, #25509 ) ;
#18806 = ORIENTED_EDGE ( 'NONE', *, *, #53038, .T. ) ;
#18807 = CARTESIAN_POINT ( 'NONE',  ( 0.000000000000000000, 0.000000000000000000, 0.000000000000000000 ) ) ;
#18808 = CARTESIAN_POINT ( 'NONE',  ( 151.3136733342017237, 54.26417151662144533, 41.20011332843551344 ) ) ;
#18809 = CARTESIAN_POINT ( 'NONE',  ( 8.485361335568063268, -170.0000000000000000, -95.00000000000133582 ) ) ;
#18810 = ORIENTED_EDGE ( 'NONE', *, *, #56622, .F. ) ;
#18811 = DIRECTION ( 'NONE',  ( 0.000000000000000000, 0.000000000000000000, 1.000000000000000000 ) ) ;
#18812 = LINE ( 'NONE', #56798, #12064 ) ;
#18813 = CARTESIAN_POINT ( 'NONE',  ( -1.088326810997879424, 6.545818265928947888, 7.438908920697859806 ) ) ;
#18814 = DIRECTION ( 'NONE',  ( 1.000000000000000000, 0.000000000000000000, 0.000000000000000000 ) ) ;
#18815 = DIRECTION ( 'NONE',  ( -0.000000000000000000, 1.000000000000000000, -0.000000000000000000 ) ) ;
#18816 = CARTESIAN_POINT ( 'NONE',  ( 155.1792092232399227, 55.88996826282357233, 83.43110084902221502 ) ) ;
#18817 = CARTESIAN_POINT ( 'NONE',  ( 136.9798231265810671, 43.34196232604180210, 3.331182321761577469 ) ) ;
#18818 = EDGE_CURVE ( 'NONE', #19443, #62318, #65340, .T. ) ;
#18819 = VERTEX_POINT ( 'NONE', #62049 ) ;
#18820 = ADVANCED_FACE ( 'NONE', ( #62405 ), #40948, .T. ) ;
#18821 = CARTESIAN_POINT ( 'NONE',  ( 117.6865880453676283, 32.48051379280607165, -44.47768925270803209 ) ) ;
#18822 = CARTESIAN_POINT ( 'NONE',  ( -71.97171223898807568, 20.94894057408424359, 14.49148078501619707 ) ) ;
#18823 = CARTESIAN_POINT ( 'NONE',  ( 46.64694836521739774, 9.462741877720617367, -45.07469269781585552 ) ) ;
#18824 = DIRECTION ( 'NONE',  ( 0.000000000000000000, -0.000000000000000000, 1.000000000000000000 ) ) ;
#18826 = ORIENTED_EDGE ( 'NONE', *, *, #25756, .T. ) ;
#18825 = CYLINDRICAL_SURFACE ( 'NONE', #9623, 7.500000000000020428 ) ;
#18827 = FACE_OUTER_BOUND ( 'NONE', #41459, .T. ) ;
#18828 = EDGE_CURVE ( 'NONE', #47781, #3682, #35328, .T. ) ;
#18829 = ORIENTED_EDGE ( 'NONE', *, *, #11809, .F. ) ;
#18830 = CARTESIAN_POINT ( 'NONE',  ( -145.9095871962850879, 61.18682730038539574, 71.65010240623834648 ) ) ;
#18831 = AXIS2_PLACEMENT_3D ( 'NONE', #13197, #44497, #22692 ) ;
#18832 = LINE ( 'NONE', #40289, #26636 ) ;
#18833 = DIRECTION ( 'NONE',  ( 0.3090169943749446757, 0.9510565162951544194, 0.000000000000000000 ) ) ;
#18834 = B_SPLINE_CURVE_WITH_KNOTS ( 'NONE', 3,
 ( #39237, #61030, #54697, #17778, #12500, #54339, #55393, #27621, #17055, #23415 ),
 .UNSPECIFIED., .F., .F.,
 ( 4, 2, 2, 2, 4 ),
 ( 0.000000000000000000, 0.002504193092414286771, 0.005008386184828573541, 0.007512579277242860745, 0.01001677236965714708 ),
 .UNSPECIFIED. ) ;
#18835 = CARTESIAN_POINT ( 'NONE',  ( 188.5645326065591689, 86.51153908883284771, -17.49986616938031503 ) ) ;
#18836 = CARTESIAN_POINT ( 'NONE',  ( 140.9169160367233360, 45.85398962664667977, -14.09481450478372544 ) ) ;
#18837 = AXIS2_PLACEMENT_3D ( 'NONE', #60022, #17462, #42560 ) ;
#18838 = CARTESIAN_POINT ( 'NONE',  ( -80.56139928459660382, 24.13290941644248022, -8.510312252193591220 ) ) ;
#18839 = CARTESIAN_POINT ( 'NONE',  ( -175.1895962157336726, 90.99110972060685754, -22.58887341897165513 ) ) ;
#18840 = CARTESIAN_POINT ( 'NONE',  ( -48.23766733091051861, 13.99378332280059034, 40.95827912834796081 ) ) ;
#18841 = ORIENTED_EDGE ( 'NONE', *, *, #35254, .F. ) ;
#18842 =( REPRESENTATION_RELATIONSHIP ('NONE','NONE', #40274, #50551 ) REPRESENTATION_RELATIONSHIP_WITH_TRANSFORMATION ( #53720 )SHAPE_REPRESENTATION_RELATIONSHIP( ) );
#18843 = ORIENTED_EDGE ( 'NONE', *, *, #60485, .T. ) ;
#18844 = ADVANCED_FACE ( 'NONE', ( #3316 ), #62755, .T. ) ;
#18845 = VECTOR ( 'NONE', #55827, 1000.000000000000000 ) ;
#18846 = CARTESIAN_POINT ( 'NONE',  ( 422.4999999999999432, -18.06806526123148160, -2.000000000000000000 ) ) ;
#18847 = PLANE ( 'NONE',  #59301 ) ;
#18849 = ADVANCED_FACE ( 'NONE', ( #34654 ), #56090, .T. ) ;
#18848 = CARTESIAN_POINT ( 'NONE',  ( -189.3111515777349894, 107.1887855376296983, 66.35551062646212017 ) ) ;
#18850 = EDGE_CURVE ( 'NONE', #29309, #15636, #44871, .T. ) ;
#18851 = COLOUR_RGB ( '',0.7921568627450980005, 0.8196078431372548767, 0.9333333333333333481 ) ;
#18852 = CARTESIAN_POINT ( 'NONE',  ( 186.6054783416232397, 84.37128553200975034, -48.82557464685664428 ) ) ;
#18853 = DIRECTION ( 'NONE',  ( -0.7071067811865474617, -0.7071067811865474617, 3.951729029292866070E-16 ) ) ;
#18854 = CARTESIAN_POINT ( 'NONE',  ( -24.19091603582230832, 8.513464105188679909, -40.87426144925215965 ) ) ;
#18855 = CARTESIAN_POINT ( 'NONE',  ( -17.50000000000002842, -18.06806526123148160, 0.000000000000000000 ) ) ;
#18856 = ORIENTED_EDGE ( 'NONE', *, *, #55915, .F. ) ;
#18857 = ORIENTED_EDGE ( 'NONE', *, *, #13881, .F. ) ;
#18858 = EDGE_LOOP ( 'NONE', ( #32028, #53768 ) ) ;
#18860 = CIRCLE ( 'NONE', #13242, 8.000000000000001776 ) ;
#18859 = CARTESIAN_POINT ( 'NONE',  ( 21.27121078971612889, 61.42097029141972087, 170.0000000000000000 ) ) ;
#18861 = CARTESIAN_POINT ( 'NONE',  ( -71.26082837647275880, 19.63751494688351684, 92.83733660865655679 ) ) ;
#18862 = CARTESIAN_POINT ( 'NONE',  ( -81.23297981660238065, 23.31577157498399089, 71.81404419543271445 ) ) ;
#18863 = CARTESIAN_POINT ( 'NONE',  ( 68.61679388097590504, 14.04192738700837140, -48.21445178305530987 ) ) ;
#18864 = CARTESIAN_POINT ( 'NONE',  ( -64.61430802170492882, 7.070445451047392638, 40.00000000000003553 ) ) ;
#18865 = CARTESIAN_POINT ( 'NONE',  ( -60.47589866267035319, 17.25153113855766307, 32.63091271826195339 ) ) ;
#18866 = LINE ( 'NONE', #18174, #13555 ) ;
#18867 = CARTESIAN_POINT ( 'NONE',  ( 59.94652978725886783, 13.01168383647461901, 44.16053422060780065 ) ) ;
#18868 = CARTESIAN_POINT ( 'NONE',  ( 32.56653645198905878, 7.618633747641397669, 87.99861145309087362 ) ) ;
#18869 =( NAMED_UNIT ( * ) SI_UNIT ( $, .STERADIAN. ) SOLID_ANGLE_UNIT ( ) );
#18870 = VERTEX_POINT ( 'NONE', #57473 ) ;
#18871 = CARTESIAN_POINT ( 'NONE',  ( -1.319107422865894774, 6.554467368239797587, -46.68092456214186114 ) ) ;
#18872 = CARTESIAN_POINT ( 'NONE',  ( -68.11501976657856972, 31.41506934893843805, 170.0000000000000000 ) ) ;
#18873 = CARTESIAN_POINT ( 'NONE',  ( -190.4968431727838833, 108.8425311198514862, -46.28873902368739124 ) ) ;
#18874 = CARTESIAN_POINT ( 'NONE',  ( 133.3996297101684547, 41.14871796345730104, -9.178760341931967659 ) ) ;
#18875 = DIRECTION ( 'NONE',  ( -1.000000000000000000, -1.110223024625118675E-14, 1.110223024625118675E-14 ) ) ;
#18876 = DIRECTION ( 'NONE',  ( -0.000000000000000000, 1.000000000000000000, -0.000000000000000000 ) ) ;
#18877 = CARTESIAN_POINT ( 'NONE',  ( 129.4887940973039804, 40.01039828304092794, -10.56306520635085988 ) ) ;
#18878 = VERTEX_POINT ( 'NONE', #30393 ) ;
#18879 = SHAPE_DEFINITION_REPRESENTATION ( #51752, #64096 ) ;
#18880 = FACE_OUTER_BOUND ( 'NONE', #40775, .T. ) ;
#18881 = CARTESIAN_POINT ( 'NONE',  ( -33.83721310978700814, 11.01869210665941878, -49.92765374023623082 ) ) ;
#18882 = FACE_OUTER_BOUND ( 'NONE', #42007, .T. ) ;
#18883 = CARTESIAN_POINT ( 'NONE',  ( -176.6810441562621747, 91.17854316950446503, 85.38946104415586547 ) ) ;
#18884 = ORIENTED_EDGE ( 'NONE', *, *, #19290, .T. ) ;
#18885 = CARTESIAN_POINT ( 'NONE',  ( -15.67984581960975632, -63.08044415722883969, 40.00000000000003553 ) ) ;
#18886 = EDGE_CURVE ( 'NONE', #9754, #18311, #48387, .T. ) ;
#18887 = CARTESIAN_POINT ( 'NONE',  ( -149.0732005398557760, 63.81212100765654327, -7.977722101697186652 ) ) ;
#18888 = CARTESIAN_POINT ( 'NONE',  ( -1.224646799147352468E-15, 19.13941707223175825, -5.803681084894614095 ) ) ;
#18889 = VERTEX_POINT ( 'NONE', #68041 ) ;
#18890 = AXIS2_PLACEMENT_3D ( 'NONE', #52843, #63770, #36343 ) ;
#18891 = EDGE_CURVE ( 'NONE', #65005, #66949, #21455, .T. ) ;
#18892 = CARTESIAN_POINT ( 'NONE',  ( 164.0474223553472370, 64.26366484389406253, 86.97719845451288734 ) ) ;
#18893 = EDGE_LOOP ( 'NONE', ( #63149, #58895, #41301, #56367 ) ) ;
#18894 = CARTESIAN_POINT ( 'NONE',  ( -62.06231780744543869, 17.72446026058426227, 13.65205514321663394 ) ) ;
#18895 = DIRECTION ( 'NONE',  ( 1.000000000000000000, 0.000000000000000000, 0.000000000000000000 ) ) ;
#18896 = VECTOR ( 'NONE', #31091, 1000.000000000000000 ) ;
#18897 = FACE_BOUND ( 'NONE', #66177, .T. ) ;
#18898 = CARTESIAN_POINT ( 'NONE',  ( -190.6985136298601731, 109.1272424661242582, 94.99999999999866418 ) ) ;
#18899 = VECTOR ( 'NONE', #32739, 1000.000000000000114 ) ;
#18900 = DIRECTION ( 'NONE',  ( 0.3090169943749446757, 0.9510565162951544194, 0.000000000000000000 ) ) ;
#18902 = ORIENTED_EDGE ( 'NONE', *, *, #65042, .T. ) ;
#18901 = CARTESIAN_POINT ( 'NONE',  ( 8.942470798084043437, 23.47701018505912174, 0.000000000000000000 ) ) ;
#18903 = ADVANCED_FACE ( 'NONE', ( #24777, #25130 ), #46563, .T. ) ;
#18904 = CARTESIAN_POINT ( 'NONE',  ( 62.04326772936978784, 12.44884401098615534, 29.86050463841740665 ) ) ;
#18905 = EDGE_CURVE ( 'NONE', #22148, #8320, #60773, .T. ) ;
#18906 = EDGE_LOOP ( 'NONE', ( #10211, #32487, #59363, #57100 ) ) ;
#18908 = VERTEX_POINT ( 'NONE', #58837 ) ;
#18907 = ADVANCED_FACE ( 'NONE', ( #25818 ), #15935, .F. ) ;
#18909 = CARTESIAN_POINT ( 'NONE',  ( -167.4860113959264822, 82.52233889531183308, 16.43299606317020078 ) ) ;
#18910 = CARTESIAN_POINT ( 'NONE',  ( 19.11168290073779730, 6.629794975642855803, -63.13554536250090621 ) ) ;
#18911 = EDGE_CURVE ( 'NONE', #69105, #40305, #109, .T. ) ;
#18913 = EDGE_LOOP ( 'NONE', ( #22387, #10672, #6363, #25179 ) ) ;
#18912 = CARTESIAN_POINT ( 'NONE',  ( -128.1282195935087884, 49.19720162550163423, 57.80142861109457186 ) ) ;
#18914 = DIRECTION ( 'NONE',  ( -0.000000000000000000, 1.000000000000000000, -0.000000000000000000 ) ) ;
#18915 = CARTESIAN_POINT ( 'NONE',  ( -25.80443741485380471, 9.749985135376009637, 42.69045884007576319 ) ) ;
#18916 = FACE_BOUND ( 'NONE', #46482, .T. ) ;
#18917 = ORIENTED_EDGE ( 'NONE', *, *, #23269, .F. ) ;
#18918 = CARTESIAN_POINT ( 'NONE',  ( 207.8398359204632868, 112.5208221429021336, -77.48374306908839060 ) ) ;
#18919 = CARTESIAN_POINT ( 'NONE',  ( 10.00000000000000178, -31.50328976398030534, 5.000000000000000000 ) ) ;
#18920 = CARTESIAN_POINT ( 'NONE',  ( -439.4229916354185548, 400.0000000000065370, -128.9497041420121093 ) ) ;
#18921 = CARTESIAN_POINT ( 'NONE',  ( -133.3923804760465543, 52.87100816290226390, 10.70811376284584426 ) ) ;
#18922 = DIRECTION ( 'NONE',  ( 0.9749279121818226201, 0.2225209339563184452, -2.254973782195817056E-16 ) ) ;
#18923 = ORIENTED_EDGE ( 'NONE', *, *, #48178, .T. ) ;
#18924 = ORIENTED_EDGE ( 'NONE', *, *, #32183, .F. ) ;
#18925 = CARTESIAN_POINT ( 'NONE',  ( -146.5230751932348880, 62.99205605665031271, -22.36346160708336228 ) ) ;
#18927 = EDGE_CURVE ( 'NONE', #46252, #21223, #31430, .T. ) ;
#18926 = CARTESIAN_POINT ( 'NONE',  ( -60.00000000000000000, 7.347880794884118356E-15, 5.000000000000000000 ) ) ;
#18928 = EDGE_CURVE ( 'NONE', #20719, #24611, #57458, .T. ) ;
#18929 = PLANE ( 'NONE',  #68154 ) ;
#18930 = CARTESIAN_POINT ( 'NONE',  ( -7.486743542470046364, 64.58150799671128084, 41.38025477438755928 ) ) ;
#18931 = EDGE_CURVE ( 'NONE', #7345, #53458, #37382, .T. ) ;
#18932 = CARTESIAN_POINT ( 'NONE',  ( -142.9728934044261734, 58.82891228489260982, 34.50119712044075015 ) ) ;
#18933 = CARTESIAN_POINT ( 'NONE',  ( 0.000000000000000000, 200.0000000000000000, 0.000000000000000000 ) ) ;
#18934 = CARTESIAN_POINT ( 'NONE',  ( -171.0758681675583830, 84.87997360100516175, -61.82834634754290448 ) ) ;
#18935 = EDGE_LOOP ( 'NONE', ( #24739, #32010, #62953, #47248 ) ) ;
#18936 = CARTESIAN_POINT ( 'NONE',  ( -103.2061297292849531, 34.38496953192503014, 30.56187840025431512 ) ) ;
#18937 = VERTEX_POINT ( 'NONE', #52862 ) ;
#18938 = CARTESIAN_POINT ( 'NONE',  ( 35.65775178405257151, 7.951994368745591402, 30.91065945747581267 ) ) ;
#18939 = CARTESIAN_POINT ( 'NONE',  ( 85.68197636629479064, 20.16141071296262766, 56.60131216792452591 ) ) ;
#18940 = VERTEX_POINT ( 'NONE', #5034 ) ;
#18941 = CARTESIAN_POINT ( 'NONE',  ( 186.2722199822850655, 84.01218714714249813, 42.24469577624778083 ) ) ;
#18942 = CARTESIAN_POINT ( 'NONE',  ( -189.4223925288096098, 107.3427006758676185, -67.23478617198331619 ) ) ;
#18943 = DIRECTION ( 'NONE',  ( -1.000000000000000000, 0.000000000000000000, 0.000000000000000000 ) ) ;
#18944 = CIRCLE ( 'NONE', #34720, 5.000000000000004441 ) ;
#18945 = LINE ( 'NONE', #34448, #61783 ) ;
#18946 = CARTESIAN_POINT ( 'NONE',  ( -3.000000000000006217, 0.000000000000000000, 0.000000000000000000 ) ) ;
#18947 = CARTESIAN_POINT ( 'NONE',  ( -14.56631729561072142, 8.434645566888205437, -39.59350022180603901 ) ) ;
#18948 = LINE ( 'NONE', #67487, #44976 ) ;
#18949 = COLOUR_RGB ( '',0.7921568627450980005, 0.8196078431372548767, 0.9333333333333333481 ) ;
#18950 = ORIENTED_EDGE ( 'NONE', *, *, #30921, .T. ) ;
#18951 = CARTESIAN_POINT ( 'NONE',  ( -108.0942684325822825, 35.83382830275052555, -91.46080949164959861 ) ) ;
#18952 = ORIENTED_EDGE ( 'NONE', *, *, #20397, .F. ) ;
#18953 = CARTESIAN_POINT ( 'NONE',  ( -65.36598343705435354, 0.000000000000000000, 41.38025477438755928 ) ) ;
#18954 = CARTESIAN_POINT ( 'NONE',  ( -59.96408504033279740, 17.10126854471815605, 70.35115488651923954 ) ) ;
#18955 = CARTESIAN_POINT ( 'NONE',  ( 109.9975424824652634, 22.00669820036271673, 401.6295345748408181 ) ) ;
#18956 = ORIENTED_EDGE ( 'NONE', *, *, #59924, .F. ) ;
#18957 = CARTESIAN_POINT ( 'NONE',  ( 32.64241790427570322, -7.194141594814827734, 6.893343212288940869 ) ) ;
#18958 = CARTESIAN_POINT ( 'NONE',  ( 150.2805372522807090, 53.51147386362153213, -68.31707538700877080 ) ) ;
#18959 = CARTESIAN_POINT ( 'NONE',  ( -95.88718821240200896, 29.65015105908826243, -19.60004368519706475 ) ) ;
#18960 = CARTESIAN_POINT ( 'NONE',  ( 134.3159642998340075, 41.70198410084975649, -51.02331093239570947 ) ) ;
#18961 = VERTEX_POINT ( 'NONE', #26497 ) ;
#18962 = DIRECTION ( 'NONE',  ( -1.000000000000000000, -9.989315170677461579E-15, -2.157629525789177834E-16 ) ) ;
#18963 = DIRECTION ( 'NONE',  ( -0.000000000000000000, 1.000000000000000000, -0.000000000000000000 ) ) ;
#18964 = CARTESIAN_POINT ( 'NONE',  ( -118.7011677090247588, 41.93687969120207981, 35.97862495719843423 ) ) ;
#18965 = CARTESIAN_POINT ( 'NONE',  ( -56.02027488966931656, 14.94257193099085512, -35.26346284988749602 ) ) ;
#18966 = ORIENTED_EDGE ( 'NONE', *, *, #45649, .T. ) ;
#18967 = CARTESIAN_POINT ( 'NONE',  ( -173.5372686962700755, 89.10569330281728639, -76.55650775521371543 ) ) ;
#18968 = CARTESIAN_POINT ( 'NONE',  ( 131.7631832018459761, 41.34383094671487413, 83.49070356861206221 ) ) ;
#18969 = B_SPLINE_CURVE_WITH_KNOTS ( 'NONE', 3,
 ( #39307, #55833, #33342, #50550, #55472, #60408, #65697, #18196, #49133, #38603, #54769, #50203, #32978, #66056, #22424, #6597, #12226, #33690, #22770, #2369, #44213, #44578, #23825, #39650, #66750, #12929, #2029, #17488, #55120, #23484, #61107, #6942, #34390, #11504, #17850, #6240, #28393, #49838, #60751, #27693, #1665, #43863, #12571 ),
 .UNSPECIFIED., .F., .F.,
 ( 4, 2, 2, 2, 2, 2, 2, 2, 1, 2, 2, 2, 2, 2, 2, 2, 2, 2, 2, 2, 2, 4 ),
 ( 1.734723475976807094E-18, 0.001466540241398116458, 0.002199810362097173819, 0.002933080482796231181, 0.004399620724194333761, 0.005866160965592434606, 0.007332701206990535452, 0.008065971327689585441, 0.008799241448388634562, 0.009532511569087683684, 0.01026578168978673281, 0.01173232193118487442, 0.01319886217258301256, 0.01466540241398115590, 0.01539867253468024319, 0.01613194265537933048, 0.01759848289677747729, 0.01906502313817561717, 0.01979829325887470098, 0.02053156337957378480, 0.02199810362097197325, 0.02346464386237015476 ),
 .UNSPECIFIED. ) ;
#18970 = CARTESIAN_POINT ( 'NONE',  ( 200.4590013143046576, 102.3556155835302945, -23.18599784113892781 ) ) ;
#18971 = DIRECTION ( 'NONE',  ( -1.000000000000000000, -1.387778780781446415E-16, 0.000000000000000000 ) ) ;
#18972 = EDGE_CURVE ( 'NONE', #21309, #66166, #58162, .T. ) ;
#18973 = LINE ( 'NONE', #40422, #35773 ) ;
#18974 = EDGE_LOOP ( 'NONE', ( #53039, #30160, #8689, #23492 ) ) ;
#18975 = CARTESIAN_POINT ( 'NONE',  ( 164.0298848570286339, 62.93631132702878972, -13.10447936278614023 ) ) ;
#18976 = CARTESIAN_POINT ( 'NONE',  ( 114.4640969196986191, 30.88424258798503530, -76.47100256968519716 ) ) ;
#18977 = DIRECTION ( 'NONE',  ( -0.000000000000000000, -0.000000000000000000, -1.000000000000000000 ) ) ;
#18978 = CARTESIAN_POINT ( 'NONE',  ( 187.1594815608683859, 84.97172738281348359, -93.01128905854854168 ) ) ;
#18979 = PLANE ( 'NONE',  #68949 ) ;
#18980 = ORIENTED_EDGE ( 'NONE', *, *, #62743, .T. ) ;
#18981 = EDGE_CURVE ( 'NONE', #61455, #7485, #69402, .T. ) ;
#18982 = CARTESIAN_POINT ( 'NONE',  ( 162.6205203824432317, 63.07332653227190633, -11.32221202892962708 ) ) ;
#18983 = VERTEX_POINT ( 'NONE', #32120 ) ;
#18984 = DIRECTION ( 'NONE',  ( -0.000000000000000000, -0.000000000000000000, -1.000000000000000000 ) ) ;
#18985 = CARTESIAN_POINT ( 'NONE',  ( 126.3481178384318611, 37.07182590705851055, 90.63207038995997777 ) ) ;
#18986 = EDGE_CURVE ( 'NONE', #38218, #55323, #36361, .T. ) ;
#18987 = CIRCLE ( 'NONE', #15618, 65.36598343705435354 ) ;
#18988 = CIRCLE ( 'NONE', #23513, 72.99999999999998579 ) ;
#18989 = EDGE_CURVE ( 'NONE', #34631, #37469, #12237, .T. ) ;
#18990 = ORIENTED_EDGE ( 'NONE', *, *, #41756, .T. ) ;
#18991 = CARTESIAN_POINT ( 'NONE',  ( -142.0062637385109952, 58.06920992247430746, -68.60690856511718039 ) ) ;
#18992 = CARTESIAN_POINT ( 'NONE',  ( -40.27405704175546930, -63.28161525591320924, 170.0000000000000000 ) ) ;
#18993 = CARTESIAN_POINT ( 'NONE',  ( 0.000000000000000000, 0.000000000000000000, 10.00000000000000000 ) ) ;
#18994 = CARTESIAN_POINT ( 'NONE',  ( 163.1265310614427051, 62.18610413911356005, -48.55550286496519163 ) ) ;
#18995 = ORIENTED_EDGE ( 'NONE', *, *, #66585, .F. ) ;
#18996 = CARTESIAN_POINT ( 'NONE',  ( -94.78138776532236420, 30.24234841992712930, 11.71057004227387210 ) ) ;
#18997 = CARTESIAN_POINT ( 'NONE',  ( 56.83393674870969647, 12.35044717442195150, 86.74189108956782945 ) ) ;
#18998 = DIRECTION ( 'NONE',  ( -1.000000000000000000, 0.000000000000000000, 0.000000000000000000 ) ) ;
#18999 = CARTESIAN_POINT ( 'NONE',  ( 85.67165909753197184, 20.15791549876372812, -9.022809353226582729 ) ) ;
#19000 = CYLINDRICAL_SURFACE ( 'NONE', #43736, 5.000000000000000888 ) ;
#19001 = FACE_OUTER_BOUND ( 'NONE', #64825, .T. ) ;
#19002 = CARTESIAN_POINT ( 'NONE',  ( 133.3990214534116205, 41.14886683286416513, -77.85737058891160700 ) ) ;
#19003 = VERTEX_POINT ( 'NONE', #27173 ) ;
#19004 = DIRECTION ( 'NONE',  ( 0.000000000000000000, -0.000000000000000000, -1.000000000000000000 ) ) ;
#19005 = CARTESIAN_POINT ( 'NONE',  ( 204.6977192012829789, -170.0000000000000000, 36.70772073876943153 ) ) ;
#19006 = VERTEX_POINT ( 'NONE', #1148 ) ;
#19007 = VECTOR ( 'NONE', #44631, 1000.000000000000000 ) ;
#19008 = CARTESIAN_POINT ( 'NONE',  ( -151.2511071212631464, 67.00426547928867649, -35.00508260455636389 ) ) ;
#19009 = CARTESIAN_POINT ( 'NONE',  ( 2.309976723937611442, -7.903938623646888928, -0.1306530452038232315 ) ) ;
#19010 = CARTESIAN_POINT ( 'NONE',  ( -35.17296606710973350, 11.25626711331309693, 31.19335591454689194 ) ) ;
#19011 = CARTESIAN_POINT ( 'NONE',  ( -154.7934364910360330, 68.79594655117531943, -63.83113484831022788 ) ) ;
#19012 = DIRECTION ( 'NONE',  ( -0.9959742939952397345, 0.08963930890342654279, 0.000000000000000000 ) ) ;
#19013 = EDGE_CURVE ( 'NONE', #61781, #53211, #19248, .T. ) ;
#19014 = CARTESIAN_POINT ( 'NONE',  ( -26.69131247781221106, -59.26697088777007849, 170.0000000000000000 ) ) ;
#19015 = CARTESIAN_POINT ( 'NONE',  ( 206.2980740120524388, 108.5619562183280067, -51.16432913298972807 ) ) ;
#19016 = CARTESIAN_POINT ( 'NONE',  ( 177.0075766083211590, 74.58167636505949361, 3.664334904826073824 ) ) ;
#19017 = CARTESIAN_POINT ( 'NONE',  ( -61.75629144857965258, 16.58190704077738076, 14.34543443704044741 ) ) ;
#19018 = EDGE_LOOP ( 'NONE', ( #60676, #40985, #10437, #34355 ) ) ;
#19019 = CARTESIAN_POINT ( 'NONE',  ( -96.77705718164445159, 31.18700926299573695, -37.39494439648063917 ) ) ;
#19020 = VERTEX_POINT ( 'NONE', #21901 ) ;
#19021 = CARTESIAN_POINT ( 'NONE',  ( 107.0477776024378613, 27.43148174916616000, -77.05657040992022644 ) ) ;
#19022 = DIRECTION ( 'NONE',  ( 0.000000000000000000, 0.000000000000000000, 1.000000000000000000 ) ) ;
#19023 = CARTESIAN_POINT ( 'NONE',  ( 42.70988075781783522, 8.862408058333489436, 57.50971735983328870 ) ) ;
#19024 = PLANE ( 'NONE',  #41354 ) ;
#19025 = CARTESIAN_POINT ( 'NONE',  ( -5.586713254917526683, 6.755371726299415513, 84.13907536519101882 ) ) ;
#19026 = CARTESIAN_POINT ( 'NONE',  ( -102.2801239173131194, 33.91021738430207222, -23.17002667451225406 ) ) ;
#19027 = CARTESIAN_POINT ( 'NONE',  ( 59.84413847313641810, 12.98802251483526149, -90.06398035839559668 ) ) ;
#19028 = CARTESIAN_POINT ( 'NONE',  ( -166.5704851812740230, 80.12110537694668722, 61.50361147337653023 ) ) ;
#19029 = ORIENTED_EDGE ( 'NONE', *, *, #31987, .F. ) ;
#19030 = ORIENTED_EDGE ( 'NONE', *, *, #58743, .T. ) ;
#19031 = CARTESIAN_POINT ( 'NONE',  ( 2.905661822261151883E-14, 15.55634918610403084, 85.00100000000000477 ) ) ;
#19032 = DIRECTION ( 'NONE',  ( -0.000000000000000000, -0.000000000000000000, -1.000000000000000000 ) ) ;
#19033 = CARTESIAN_POINT ( 'NONE',  ( 178.4027079424739100, 75.93756746109791322, -9.872868637179553986 ) ) ;
#19034 = CARTESIAN_POINT ( 'NONE',  ( 109.3154830994003390, 29.56170298203815960, 56.49859460758455754 ) ) ;
#19035 = DIRECTION ( 'NONE',  ( -0.000000000000000000, -0.000000000000000000, 1.000000000000000000 ) ) ;
#19036 = AXIS2_PLACEMENT_3D ( 'NONE', #905, #43793, #17059 ) ;
#19037 = CARTESIAN_POINT ( 'NONE',  ( 60.63380853769236722, 13.16344960520421559, -23.49203963615685353 ) ) ;
#19038 = ORIENTED_EDGE ( 'NONE', *, *, #21832, .T. ) ;
#19039 = CIRCLE ( 'NONE', #44900, 65.00000000000000000 ) ;
#19040 = DIRECTION ( 'NONE',  ( -1.000000000000000000, 0.000000000000000000, 0.000000000000000000 ) ) ;
#19041 = EDGE_CURVE ( 'NONE', #29324, #65564, #33858, .T. ) ;
#19042 = CARTESIAN_POINT ( 'NONE',  ( 23.03546163277112413, 7.848986635155161373, -41.07252390632271499 ) ) ;
#19043 = CARTESIAN_POINT ( 'NONE',  ( -149.5074843970971017, 65.50121172469319220, 45.72082123989907387 ) ) ;
#19044 = CARTESIAN_POINT ( 'NONE',  ( -422.6627218934914936, 399.9999999999998863, -146.4497041420118251 ) ) ;
#19045 = CARTESIAN_POINT ( 'NONE',  ( -125.8938041572051389, 47.69968343338778283, 30.61994787315706290 ) ) ;
#19046 = ADVANCED_FACE ( 'NONE', ( #32462 ), #6060, .T. ) ;
#19047 = EDGE_CURVE ( 'NONE', #47961, #58719, #7120, .T. ) ;
#19048 = EDGE_CURVE ( 'NONE', #41326, #44052, #11691, .T. ) ;
#19049 = VERTEX_POINT ( 'NONE', #43349 ) ;
#19050 = ORIENTED_EDGE ( 'NONE', *, *, #46516, .F. ) ;
#19051 = DIRECTION ( 'NONE',  ( 0.8584487936018655452, 0.5128992774059070170, 0.000000000000000000 ) ) ;
#19052 = CARTESIAN_POINT ( 'NONE',  ( 91.12448333640237763, 22.07449368110503229, -49.34459205181515529 ) ) ;
#19053 = LINE ( 'NONE', #13437, #1527 ) ;
#19054 = CARTESIAN_POINT ( 'NONE',  ( -173.5422248620772905, 89.11126078969415687, 18.97714401617738034 ) ) ;
#19055 = CARTESIAN_POINT ( 'NONE',  ( 10.00452960006446723, 6.384031490329864056, 86.38374501823878404 ) ) ;
#19056 = VECTOR ( 'NONE', #10421, 1000.000000000000000 ) ;
#19057 = CARTESIAN_POINT ( 'NONE',  ( 79.19132716134490124, 17.01584750883626995, -71.16104780385437323 ) ) ;
#19058 = VERTEX_POINT ( 'NONE', #59521 ) ;
#19059 = DIRECTION ( 'NONE',  ( -1.000000000000000000, 0.000000000000000000, 0.000000000000000000 ) ) ;
#19060 = CARTESIAN_POINT ( 'NONE',  ( 197.5344433744249102, 98.61756151884684130, -41.58120981647593339 ) ) ;
#19061 = ORIENTED_EDGE ( 'NONE', *, *, #55592, .T. ) ;
#19062 = CARTESIAN_POINT ( 'NONE',  ( 0.000000000000000000, 0.000000000000000000, 40.82842712474622004 ) ) ;
#19063 = EDGE_LOOP ( 'NONE', ( #29850, #41287, #48970, #1716 ) ) ;
#19064 = CARTESIAN_POINT ( 'NONE',  ( -82.32750425780474757, 23.74963782027935721, -62.89668749667942649 ) ) ;
#19065 = DIRECTION ( 'NONE',  ( 0.000000000000000000, 0.000000000000000000, 1.000000000000000000 ) ) ;
#19066 = LINE ( 'NONE', #40520, #63922 ) ;
#19067 = EDGE_CURVE ( 'NONE', #55170, #60171, #59649, .T. ) ;
#19068 = ORIENTED_EDGE ( 'NONE', *, *, #8491, .F. ) ;
#19069 = ADVANCED_FACE ( 'NONE', ( #64822 ), #27521, .T. ) ;
#19070 = VERTEX_POINT ( 'NONE', #33165 ) ;
#19071 = CARTESIAN_POINT ( 'NONE',  ( 12.46277766093406214, 6.416700641561361884, -36.27856315466706860 ) ) ;
#19072 = AXIS2_PLACEMENT_3D ( 'NONE', #583, #43823, #16752 ) ;
#19073 = DIRECTION ( 'NONE',  ( 0.7071067811865474617, -5.551115123125781716E-16, 0.7071067811865475727 ) ) ;
#19074 = CARTESIAN_POINT ( 'NONE',  ( 22.29513692215317988, 6.796052026456516515, 6.908320987580739647 ) ) ;
#19075 = ORIENTED_EDGE ( 'NONE', *, *, #33754, .T. ) ;
#19076 = CARTESIAN_POINT ( 'NONE',  ( -78.66644367742111399, 23.39876645725285798, -8.270900041254197532 ) ) ;
#19077 = CARTESIAN_POINT ( 'NONE',  ( 175.8947993867356843, 74.90689716047906188, -76.00546110050024140 ) ) ;
#19078 = CARTESIAN_POINT ( 'NONE',  ( 0.000000000000000000, 0.000000000000000000, 41.38025477438755928 ) ) ;
#19079 = CARTESIAN_POINT ( 'NONE',  ( 110.2429982417149432, 28.88204397445231564, -9.077886975189997543 ) ) ;
#19080 = CARTESIAN_POINT ( 'NONE',  ( 82.12277968641507186, 18.98848723477813039, -37.30662462622972697 ) ) ;
#19081 = DIRECTION ( 'NONE',  ( 0.000000000000000000, 0.000000000000000000, 1.000000000000000000 ) ) ;
#19082 = EDGE_LOOP ( 'NONE', ( #22472, #14411 ) ) ;
#19083 = VECTOR ( 'NONE', #68960, 1000.000000000000000 ) ;
#19084 = ORIENTED_EDGE ( 'NONE', *, *, #48395, .T. ) ;
#19085 = CARTESIAN_POINT ( 'NONE',  ( -16.04603987767271533, 64.68484515506864341, 34.48241823981440746 ) ) ;
#19086 = CYLINDRICAL_SURFACE ( 'NONE', #61889, 7.500000000000020428 ) ;
#19087 = PLANE ( 'NONE',  #34545 ) ;
#19088 = FACE_OUTER_BOUND ( 'NONE', #38833, .T. ) ;
#19089 = CARTESIAN_POINT ( 'NONE',  ( 198.3926538463958593, 98.07933330386025261, 13.96394819647072794 ) ) ;
#19090 = DIRECTION ( 'NONE',  ( 0.1342332658176522420, 0.9909497617679352555, -0.000000000000000000 ) ) ;
#19091 = CARTESIAN_POINT ( 'NONE',  ( 211.7299983131283057, 118.3604252729061130, 87.78175077331377452 ) ) ;
#19092 = CARTESIAN_POINT ( 'NONE',  ( 209.6698611676812050, 115.2210955123518659, 42.34078908743409642 ) ) ;
#19093 = DIRECTION ( 'NONE',  ( 0.000000000000000000, 0.000000000000000000, 1.000000000000000000 ) ) ;
#19094 = CARTESIAN_POINT ( 'NONE',  ( -12.39413342787891104, 7.231444436041488899, 43.58353802562231039 ) ) ;
#19095 = VERTEX_POINT ( 'NONE', #60583 ) ;
#19096 = CARTESIAN_POINT ( 'NONE',  ( 10.15118267943872077, 7.391905976536036427, -21.12758222051168033 ) ) ;
#19097 = ORIENTED_EDGE ( 'NONE', *, *, #12140, .T. ) ;
#19098 = CARTESIAN_POINT ( 'NONE',  ( 198.2545923567585646, 97.90679023593575891, -20.83074425647854611 ) ) ;
#19099 = ORIENTED_EDGE ( 'NONE', *, *, #46794, .T. ) ;
#19100 = CARTESIAN_POINT ( 'NONE',  ( -147.1538409485623333, 63.51600817366542628, 4.251635946998408855 ) ) ;
#19101 = CARTESIAN_POINT ( 'NONE',  ( 185.5412249395996014, 84.70425786166002524, -76.60579427066070934 ) ) ;
#19102 = CARTESIAN_POINT ( 'NONE',  ( -166.9992034932274976, 82.01285191063134050, 42.68440912882079630 ) ) ;
#19103 = CIRCLE ( 'NONE', #65146, 25.00000000000000355 ) ;
#19104 = CARTESIAN_POINT ( 'NONE',  ( -100.4262673593280368, 31.84860241619273680, -35.23214805985528386 ) ) ;
#19105 = CARTESIAN_POINT ( 'NONE',  ( 31.91375106836930087, 7.553354707452893280, -43.60781062558567811 ) ) ;
#19106 = CARTESIAN_POINT ( 'NONE',  ( -39.29440389294403246, -17.09499999999999886, 0.000000000000000000 ) ) ;
#19107 = CARTESIAN_POINT ( 'NONE',  ( 12.46490660984524723, 7.423426948220649635, -36.29097311990165053 ) ) ;
#19108 = CARTESIAN_POINT ( 'NONE',  ( 131.6005058089755551, 40.07838125795768036, -50.69123583781497189 ) ) ;
#19109 = ORIENTED_EDGE ( 'NONE', *, *, #16359, .F. ) ;
#19110 = EDGE_LOOP ( 'NONE', ( #44365, #56046 ) ) ;
#19111 = CARTESIAN_POINT ( 'NONE',  ( 186.9531721782180966, 86.23502673300468757, 85.81665300944044361 ) ) ;
#19112 = CARTESIAN_POINT ( 'NONE',  ( -15.32550079334879278, 7.496023944924839810, 10.52911393437325849 ) ) ;
#19113 = CARTESIAN_POINT ( 'NONE',  ( 4.000000000000012434, 6.928203230275504332, 0.000000000000000000 ) ) ;
#19114 = CARTESIAN_POINT ( 'NONE',  ( 51.85299110299497016, -39.21848821248376993, 3.061616997868437868E-16 ) ) ;
#19115 = UNCERTAINTY_MEASURE_WITH_UNIT (LENGTH_MEASURE( 1.000000000000000082E-05 ), #9698, 'distance_accuracy_value', 'NONE');
#19116 = CARTESIAN_POINT ( 'NONE',  ( 9.416656162223555171, 6.380306691996769253, 14.63415394072566400 ) ) ;
#19117 = ORIENTED_EDGE ( 'NONE', *, *, #68368, .T. ) ;
#19118 = ADVANCED_FACE ( 'NONE', ( #43691 ), #65169, .F. ) ;
#19119 = CARTESIAN_POINT ( 'NONE',  ( 39.88975917505626967, 9.487965272711658571, -77.46436805589148378 ) ) ;
#19120 = CARTESIAN_POINT ( 'NONE',  ( 0.000000000000000000, 0.000000000000000000, 0.000000000000000000 ) ) ;
#19121 = CARTESIAN_POINT ( 'NONE',  ( 198.8752826725510658, 100.3130050945023157, -75.40481520914208602 ) ) ;
#19122 = SHAPE_REPRESENTATION_RELATIONSHIP ( 'NONE' , 'NONE' ,  #50551, #49175 ) ;
#19123 = CARTESIAN_POINT ( 'NONE',  ( -180.2252811616041583, 95.40045830523430936, -39.79017893922387117 ) ) ;
#19124 = CARTESIAN_POINT ( 'NONE',  ( 107.0477776024379040, 27.43148174916616355, 3.477081361470783616 ) ) ;
#19125 = CARTESIAN_POINT ( 'NONE',  ( -170.2747214445850261, 84.01465441107043830, 18.42892912042381326 ) ) ;
#19126 = CARTESIAN_POINT ( 'NONE',  ( 108.3839814017204617, 21.48303375171747120, 4.742972355882020707 ) ) ;
#19127 = CARTESIAN_POINT ( 'NONE',  ( -51.34325167237332721, 13.71819364263220997, 71.18482817347160108 ) ) ;
#19128 = EDGE_CURVE ( 'NONE', #28008, #45254, #8009, .T. ) ;
#19129 = EDGE_CURVE ( 'NONE', #24552, #1734, #56311, .T. ) ;
#19130 = CARTESIAN_POINT ( 'NONE',  ( -2.190131154568196514, 6.589492063460817839, 59.50486936982123609 ) ) ;
#19131 = ORIENTED_EDGE ( 'NONE', *, *, #57502, .F. ) ;
#19132 = CARTESIAN_POINT ( 'NONE',  ( 100.0000000000000284, -5.000000000000000000, 21.42428528562851753 ) ) ;
#19133 = EDGE_CURVE ( 'NONE', #31627, #1172, #23072, .T. ) ;
#19134 = CARTESIAN_POINT ( 'NONE',  ( -129.4098618459771899, 48.85263848239745954, -75.88708462038850655 ) ) ;
#19135 = CARTESIAN_POINT ( 'NONE',  ( -109.7079446832839267, 37.86719386855317282, -70.42946416363754736 ) ) ;
#19136 = CARTESIAN_POINT ( 'NONE',  ( -49.43915770973590895, 13.24768844696976089, -37.71853435192636539 ) ) ;
#19137 = LINE ( 'NONE', #40591, #32394 ) ;
#19138 = AXIS2_PLACEMENT_3D ( 'NONE', #13793, #35251, #8531 ) ;
#19139 = DIRECTION ( 'NONE',  ( 0.000000000000000000, 0.000000000000000000, -1.000000000000000000 ) ) ;
#19140 = ORIENTED_EDGE ( 'NONE', *, *, #25181, .T. ) ;
#19141 = DIRECTION ( 'NONE',  ( 1.000000000000000000, 0.000000000000000000, 0.000000000000000000 ) ) ;
#19142 = CARTESIAN_POINT ( 'NONE',  ( -16.68907004672281502, -73.11959341363693454, 0.000000000000000000 ) ) ;
#19143 = ORIENTED_EDGE ( 'NONE', *, *, #15097, .T. ) ;
#19144 = ORIENTED_EDGE ( 'NONE', *, *, #49791, .T. ) ;
#19145 = DIRECTION ( 'NONE',  ( 1.000000000000000000, 0.000000000000000000, 0.000000000000000000 ) ) ;
#19146 = CARTESIAN_POINT ( 'NONE',  ( 150.5744176759382924, 53.72473166688034496, 33.94873877333132839 ) ) ;
#19147 = DIRECTION ( 'NONE',  ( 1.000000000000000000, 0.000000000000000000, 0.000000000000000000 ) ) ;
#19148 = ADVANCED_FACE ( 'NONE', ( #57051 ), #24698, .F. ) ;
#19149 = ORIENTED_EDGE ( 'NONE', *, *, #856, .T. ) ;
#19150 = CARTESIAN_POINT ( 'NONE',  ( 3.000000000000030198, 6.000000000000000000, -1.665334536937751377E-15 ) ) ;
#19151 = CARTESIAN_POINT ( 'NONE',  ( -179.5082312244189495, 94.53075638132055758, 7.537094676919972258 ) ) ;
#19152 = DIRECTION ( 'NONE',  ( 0.000000000000000000, -1.000000000000000000, 0.000000000000000000 ) ) ;
#19153 = VECTOR ( 'NONE', #18501, 1000.000000000000000 ) ;
#19154 = LINE ( 'NONE', #40608, #37651 ) ;
#19155 = CARTESIAN_POINT ( 'NONE',  ( -85.89078989036970313, 26.29712602777647845, 35.88770218881549567 ) ) ;
#19156 = CARTESIAN_POINT ( 'NONE',  ( 150.0625426684546255, 52.11349418987130377, 89.36692820587143160 ) ) ;
#19157 = CARTESIAN_POINT ( 'NONE',  ( 140.1999945597798671, 45.38880890490929687, 6.156068824733499589 ) ) ;
#19158 = ORIENTED_EDGE ( 'NONE', *, *, #29375, .F. ) ;
#19159 = LINE ( 'NONE', #67368, #8716 ) ;
#19160 = CARTESIAN_POINT ( 'NONE',  ( 13.14401442664831166, 6.430459733718342008, 71.38195679730273469 ) ) ;
#19161 = CARTESIAN_POINT ( 'NONE',  ( 45.90693067088656676, 9.344800815249319825, -39.35472096678888931 ) ) ;
#19162 = CARTESIAN_POINT ( 'NONE',  ( -72.73902111355396016, 21.21842696158244479, 87.00106551046614811 ) ) ;
#19164 = VERTEX_POINT ( 'NONE', #24354 ) ;
#19163 = DIRECTION ( 'NONE',  ( 0.000000000000000000, -1.000000000000000000, 0.000000000000000000 ) ) ;
#19165 = CARTESIAN_POINT ( 'NONE',  ( 86.15410276028860892, 19.25894675708890702, -50.82156419891174437 ) ) ;
#19166 = VECTOR ( 'NONE', #10709, 1000.000000000000000 ) ;
#19167 = ORIENTED_EDGE ( 'NONE', *, *, #38766, .F. ) ;
#19168 = FACE_OUTER_BOUND ( 'NONE', #27680, .T. ) ;
#19169 = CARTESIAN_POINT ( 'NONE',  ( -20.55634918610396866, 36.11269837220808654, 2.000000000000001776 ) ) ;
#19170 = CARTESIAN_POINT ( 'NONE',  ( -1.224646799147352468E-15, 0.000000000000000000, 0.000000000000000000 ) ) ;
#19171 = CARTESIAN_POINT ( 'NONE',  ( 181.0840389613909736, 78.60582251573003987, -9.380507075415925655 ) ) ;
#19172 = CARTESIAN_POINT ( 'NONE',  ( 10.55634918610397577, -31.11269837220809364, 2.000000000000001776 ) ) ;
#19173 = CARTESIAN_POINT ( 'NONE',  ( -85.75002235020438945, 26.23806300442548434, -13.29363553231531903 ) ) ;
#19174 = CARTESIAN_POINT ( 'NONE',  ( -180.3161328724957855, 97.10341277064810583, -13.22867699537820663 ) ) ;
#19175 = DIRECTION ( 'NONE',  ( 0.4738686624729966379, 0.8805955318567391110, 0.000000000000000000 ) ) ;
#19176 = EDGE_LOOP ( 'NONE', ( #52915, #67730, #44469, #49002, #51732 ) ) ;
#19177 = ORIENTED_EDGE ( 'NONE', *, *, #45579, .F. ) ;
#19178 = LINE ( 'NONE', #23165, #15176 ) ;
#19179 = CARTESIAN_POINT ( 'NONE',  ( 103.4696172145934554, 25.87254488218942328, 67.18619957088650096 ) ) ;
#19180 = DIRECTION ( 'NONE',  ( -0.000000000000000000, -0.000000000000000000, 1.000000000000000000 ) ) ;
#19181 = DIRECTION ( 'NONE',  ( 0.000000000000000000, 0.000000000000000000, -1.000000000000000000 ) ) ;
#19182 = EDGE_CURVE ( 'NONE', #24549, #22892, #67275, .T. ) ;
#19183 = CARTESIAN_POINT ( 'NONE',  ( 31.11269837220803325, -15.55634918610409656, 85.00100000000000477 ) ) ;
#19184 = CARTESIAN_POINT ( 'NONE',  ( 17.48889770758266948, 6.561062909825354339, 30.20590664838920603 ) ) ;
#19185 = CARTESIAN_POINT ( 'NONE',  ( -142.0103255789723846, 59.35140309638574507, 92.31801490858313741 ) ) ;
#19186 = VERTEX_POINT ( 'NONE', #8162 ) ;
#19187 = EDGE_LOOP ( 'NONE', ( #32911, #47972, #5189, #24006, #39056 ) ) ;
#19188 = ORIENTED_EDGE ( 'NONE', *, *, #11204, .T. ) ;
#19189 = DIRECTION ( 'NONE',  ( -0.000000000000000000, 1.000000000000000000, -0.000000000000000000 ) ) ;
#19190 = CARTESIAN_POINT ( 'NONE',  ( -82.53770812813169755, 23.83403279300014788, 58.33458210178376646 ) ) ;
#19191 = CARTESIAN_POINT ( 'NONE',  ( 70.45466089417030275, 14.52203022703029944, -42.23427169726421937 ) ) ;
#19192 = CARTESIAN_POINT ( 'NONE',  ( 23.93060502292675196, 7.646171227524815706, 0.000000000000000000 ) ) ;
#19193 = CARTESIAN_POINT ( 'NONE',  ( -58.97243502469717669, 16.81420332340174895, 44.21623767979525610 ) ) ;
#19194 = CIRCLE ( 'NONE', #59591, 4.999999999999997335 ) ;
#19195 = CARTESIAN_POINT ( 'NONE',  ( -37.05762690088739930, 11.60527003175538852, -74.63595191190708533 ) ) ;
#19196 = CARTESIAN_POINT ( 'NONE',  ( 33.76124497394584267, 7.742545529019362327, 69.22549252300315459 ) ) ;
#19197 = CARTESIAN_POINT ( 'NONE',  ( 42.00028371212653866, 8.760846226116838054, 84.03640436414383430 ) ) ;
#19198 = AXIS2_PLACEMENT_3D ( 'NONE', #15763, #11167, #16456 ) ;
#19199 = ORIENTED_EDGE ( 'NONE', *, *, #43310, .T. ) ;
#19200 = CARTESIAN_POINT ( 'NONE',  ( -0.3747453031323924044, 6.520267647591905025, -43.90647717188161181 ) ) ;
#19201 = PLANE ( 'NONE',  #59888 ) ;
#19202 = CARTESIAN_POINT ( 'NONE',  ( -120.1259246007803370, 42.81147313035990010, 16.09632390948472391 ) ) ;
#19203 = DIRECTION ( 'NONE',  ( 0.000000000000000000, 0.000000000000000000, 1.000000000000000000 ) ) ;
#19204 = CARTESIAN_POINT ( 'NONE',  ( 126.4083787442699958, 37.10531539900949838, -17.70407539275910480 ) ) ;
#19205 = CARTESIAN_POINT ( 'NONE',  ( 18.88468164817598449, 7.626722602998417422, -23.00979687325194334 ) ) ;
#19206 = DIRECTION ( 'NONE',  ( 0.000000000000000000, 0.000000000000000000, 1.000000000000000000 ) ) ;
#19207 = AXIS2_PLACEMENT_3D ( 'NONE', #24232, #44973, #13662 ) ;
#19208 = EDGE_CURVE ( 'NONE', #53253, #9716, #30674, .T. ) ;
#19209 = CIRCLE ( 'NONE', #1234, 200.0000000000000000 ) ;
#19210 = ORIENTED_EDGE ( 'NONE', *, *, #1044, .F. ) ;
#19211 = DIRECTION ( 'NONE',  ( 8.947834758491892820E-15, -3.957551866041645313E-15, 1.000000000000000000 ) ) ;
#19212 = ADVANCED_FACE ( 'NONE', ( #63360 ), #68628, .F. ) ;
#19213 = VECTOR ( 'NONE', #8888, 1000.000000000000000 ) ;
#19214 = CARTESIAN_POINT ( 'NONE',  ( 127.2358066117906787, 38.72257733469225371, -47.08406076428676812 ) ) ;
#19215 = CYLINDRICAL_SURFACE ( 'NONE', #39889, 2.999999999999999112 ) ;
#19216 = LINE ( 'NONE', #62127, #49140 ) ;
#19217 = DIRECTION ( 'NONE',  ( -1.000000000000000000, 0.000000000000000000, 0.000000000000000000 ) ) ;
#19218 = VERTEX_POINT ( 'NONE', #9199 ) ;
#19219 = ORIENTED_EDGE ( 'NONE', *, *, #65, .T. ) ;
#19220 = CARTESIAN_POINT ( 'NONE',  ( 0.000000000000000000, 5.000000000000000000, 85.00100000000000477 ) ) ;
#19221 = CARTESIAN_POINT ( 'NONE',  ( 311.8713128290285113, 190.0000000000000000, 346.5826552340383842 ) ) ;
#19222 = EDGE_LOOP ( 'NONE', ( #48524, #50912, #18790, #60327 ) ) ;
#19223 = CARTESIAN_POINT ( 'NONE',  ( 152.6935468464033079, 55.28251231414122913, 84.80687879366244886 ) ) ;
#19224 = ADVANCED_FACE ( 'NONE', ( #4955 ), #9897, .F. ) ;
#19225 = ORIENTED_EDGE ( 'NONE', *, *, #60905, .T. ) ;
#19226 = CARTESIAN_POINT ( 'NONE',  ( 132.0563630623057065, 41.51825634609597415, -77.65224337536834298 ) ) ;
#19227 = CARTESIAN_POINT ( 'NONE',  ( 2.905661822261151883E-14, 15.55634918610403084, 0.000000000000000000 ) ) ;
#19228 = PLANE ( 'NONE',  #4943 ) ;
#19229 = EDGE_CURVE ( 'NONE', #32664, #16864, #17196, .T. ) ;
#19230 = ADVANCED_FACE ( 'NONE', ( #9549 ), #15878, .T. ) ;
#19231 = DIRECTION ( 'NONE',  ( -1.000000000000000000, 0.000000000000000000, 0.000000000000000000 ) ) ;
#19232 = FACE_OUTER_BOUND ( 'NONE', #6807, .T. ) ;
#19234 = VERTEX_POINT ( 'NONE', #5636 ) ;
#19233 = DIRECTION ( 'NONE',  ( -0.000000000000000000, -0.000000000000000000, -1.000000000000000000 ) ) ;
#19235 = B_SPLINE_CURVE_WITH_KNOTS ( 'NONE', 3,
 ( #68111, #36432, #5105, #36785, #19917, #26565, #47660, #41373, #9021, #58228, #41021, #10043, #31500, #62476, #14293, #52933, #69114, #4421, #20940, #42396, #10374, #63858, #25886, #46984, #30464, #31172, #58557, #4084, #62826, #51916, #3723, #14629, #57548, #9352, #68444, #20250, #63172, #57886, #9705, #22324, #49033, #38148, #58906, #59588, #11404 ),
 .UNSPECIFIED., .F., .F.,
 ( 4, 2, 2, 1, 2, 2, 2, 2, 2, 2, 2, 2, 2, 2, 2, 2, 2, 2, 2, 2, 2, 2, 4 ),
 ( 0.02346057189573570387, 0.02492590417315496132, 0.02565857031186458831, 0.02639123645057421877, 0.02712390258928384923, 0.02785656872799347622, 0.02932190100541273367, 0.03005456714412236413, 0.03078723328283199112, 0.03225256556025124510, 0.03298523169896087903, 0.03371789783767050602, 0.03518323011508976000, 0.03664856239250902092, 0.03738122853121864098, 0.03811389466992827491, 0.03957922694734752889, 0.04104455922476678287, 0.04250989150218603685, 0.04324255764089565690, 0.04397522377960528389, 0.04544055605702453093, 0.04690588833444377798 ),
 .UNSPECIFIED. ) ;
#19236 = CARTESIAN_POINT ( 'NONE',  ( -2.487553394779416394, 7.609150130527738476, -91.32180055539627972 ) ) ;
#19237 = EDGE_LOOP ( 'NONE', ( #16625, #3551, #33054, #29358 ) ) ;
#19238 = ORIENTED_EDGE ( 'NONE', *, *, #19682, .T. ) ;
#19239 = CARTESIAN_POINT ( 'NONE',  ( -165.6404838346739155, 80.60836113891892296, 12.09496305903157243 ) ) ;
#19240 = APPLICATION_CONTEXT ( 'automotive_design' ) ;
#19241 = CARTESIAN_POINT ( 'NONE',  ( 22.81270948571149049, 6.827178363529885274, -67.22380911626287059 ) ) ;
#19243 = ORIENTED_EDGE ( 'NONE', *, *, #44037, .F. ) ;
#19242 = CARTESIAN_POINT ( 'NONE',  ( -133.0921934900200085, 52.65587531157186163, 67.08693232277423135 ) ) ;
#19244 = CARTESIAN_POINT ( 'NONE',  ( -98.60532234565044973, 32.07256199879358149, 85.16297041932693901 ) ) ;
#19245 = CIRCLE ( 'NONE', #14732, 65.36598343705435354 ) ;
#19246 = FACE_BOUND ( 'NONE', #59679, .T. ) ;
#19247 = VERTEX_POINT ( 'NONE', #21813 ) ;
#19248 = CIRCLE ( 'NONE', #5730, 89.99999999999998579 ) ;
#19249 = CARTESIAN_POINT ( 'NONE',  ( 175.8200436508851965, 74.83544132389157255, -92.05719928250275075 ) ) ;
#19250 = AXIS2_PLACEMENT_3D ( 'NONE', #10583, #59808, #64756 ) ;
#19251 = VECTOR ( 'NONE', #14010, 999.9999999999998863 ) ;
#19252 = CARTESIAN_POINT ( 'NONE',  ( 138.5943620234099569, 45.55242290395138127, 31.17580979822920639 ) ) ;
#19253 = CARTESIAN_POINT ( 'NONE',  ( 111.1865443042262029, 30.43181341527239070, 29.65596660664464679 ) ) ;
#19254 = DIRECTION ( 'NONE',  ( 0.000000000000000000, 0.000000000000000000, -1.000000000000000000 ) ) ;
#19255 = CARTESIAN_POINT ( 'NONE',  ( -29.70166638324878150, -57.83280658984300970, 170.0000000000000000 ) ) ;
#19256 = VERTEX_POINT ( 'NONE', #13285 ) ;
#19257 = VERTEX_POINT ( 'NONE', #65797 ) ;
#19258 = DIRECTION ( 'NONE',  ( 1.000000000000000000, 0.000000000000000000, 0.000000000000000000 ) ) ;
#19259 = AXIS2_PLACEMENT_3D ( 'NONE', #44083, #53935, #493 ) ;
#19260 = CARTESIAN_POINT ( 'NONE',  ( -48.12872802574198516, -43.70867239603780519, 170.0000000000000000 ) ) ;
#19261 = LINE ( 'NONE', #51289, #58746 ) ;
#19262 = CARTESIAN_POINT ( 'NONE',  ( -51.56239267699974960, 13.77339621164778727, -89.76365528998427123 ) ) ;
#19263 = CARTESIAN_POINT ( 'NONE',  ( -47.89046518825391985, 13.91124031206838296, -94.13781639831633186 ) ) ;
#19264 = EDGE_CURVE ( 'NONE', #59320, #68287, #8878, .T. ) ;
#19265 = CARTESIAN_POINT ( 'NONE',  ( -59.49248094505429663, 30.03746416324668900, 34.48241795236666718 ) ) ;
#19266 = CARTESIAN_POINT ( 'NONE',  ( 70.51522979775972999, 15.57935281015687146, -42.71848339722297538 ) ) ;
#19267 = CARTESIAN_POINT ( 'NONE',  ( -118.3918229753714968, 42.92682904595255877, 37.61031292237963441 ) ) ;
#19268 = CARTESIAN_POINT ( 'NONE',  ( 207.4696221732442325, 110.2206209205162111, 56.57135469275507234 ) ) ;
#19269 = ORIENTED_EDGE ( 'NONE', *, *, #56681, .T. ) ;
#19270 = CARTESIAN_POINT ( 'NONE',  ( 7.762887554996211747E-14, 51.66904755831208718, 2.000000000000001776 ) ) ;
#19271 = EDGE_LOOP ( 'NONE', ( #7620, #21554 ) ) ;
#19272 = ADVANCED_FACE ( 'NONE', ( #42914 ), #59444, .F. ) ;
#19273 = CARTESIAN_POINT ( 'NONE',  ( 79.62991792432430316, 18.20325130265939251, -94.18765078435455962 ) ) ;
#19274 = DIRECTION ( 'NONE',  ( 0.000000000000000000, 0.000000000000000000, 1.000000000000000000 ) ) ;
#19275 = ORIENTED_EDGE ( 'NONE', *, *, #65275, .F. ) ;
#19276 = DIRECTION ( 'NONE',  ( -0.8160245890732938934, -0.5780171883497599028, 0.000000000000000000 ) ) ;
#19277 = CARTESIAN_POINT ( 'NONE',  ( 64.38365952013991489, 38.46744580544303460, 0.000000000000000000 ) ) ;
#19278 = DIRECTION ( 'NONE',  ( -0.000000000000000000, -0.000000000000000000, -1.000000000000000000 ) ) ;
#19279 = CYLINDRICAL_SURFACE ( 'NONE', #37220, 4.999999999999990230 ) ;
#19280 = CARTESIAN_POINT ( 'NONE',  ( 36.09137906183515554, 8.001963043161770983, 3.835010927944524362 ) ) ;
#19281 = CARTESIAN_POINT ( 'NONE',  ( -7.825402957745085430, 7.899365992529248537, -35.41807073194381417 ) ) ;
#19282 = DIRECTION ( 'NONE',  ( 0.000000000000000000, 0.000000000000000000, 1.000000000000000000 ) ) ;
#19283 = VERTEX_POINT ( 'NONE', #5977 ) ;
#19284 = CARTESIAN_POINT ( 'NONE',  ( 0.000000000000000000, 9.237604307034018802, 1.301042606982603546E-15 ) ) ;
#19285 = ORIENTED_EDGE ( 'NONE', *, *, #25760, .T. ) ;
#19286 = CARTESIAN_POINT ( 'NONE',  ( -60.97727891098336528, 16.35024395194893287, 33.19213824417288095 ) ) ;
#19287 = DIRECTION ( 'NONE',  ( 1.734723475976807094E-16, 0.000000000000000000, 1.000000000000000000 ) ) ;
#19288 = CARTESIAN_POINT ( 'NONE',  ( 424.8372781065089612, 400.0000000000000568, -123.9497041420121235 ) ) ;
#19289 = ORIENTED_EDGE ( 'NONE', *, *, #43529, .F. ) ;
#19290 = EDGE_CURVE ( 'NONE', #18878, #11641, #64182, .T. ) ;
#19291 = DIRECTION ( 'NONE',  ( -0.9362348706397369824, -0.3513748240813435175, 0.000000000000000000 ) ) ;
#19292 = CARTESIAN_POINT ( 'NONE',  ( -14.55425570676089286, 7.423011834016143951, -66.44103785447590838 ) ) ;
#19293 = CARTESIAN_POINT ( 'NONE',  ( -35.99432170610150195, 10.38324794858010414, 31.73840043048652149 ) ) ;
#19294 = ADVANCED_FACE ( 'NONE', ( #17229 ), #38704, .F. ) ;
#19295 = CARTESIAN_POINT ( 'NONE',  ( 138.2204650371259333, 44.12203217345472694, -37.40497479428969285 ) ) ;
#19296 = EDGE_CURVE ( 'NONE', #50609, #4563, #6689, .T. ) ;
#19297 = ORIENTED_EDGE ( 'NONE', *, *, #23049, .F. ) ;
#19298 = ADVANCED_FACE ( 'NONE', ( #9731 ), #57912, .F. ) ;
#19299 = CARTESIAN_POINT ( 'NONE',  ( -155.5977325361978387, 70.88311713755702215, 69.44969795258840861 ) ) ;
#19300 = DIRECTION ( 'NONE',  ( 0.000000000000000000, 1.000000000000000000, 0.000000000000000000 ) ) ;
#19301 = CARTESIAN_POINT ( 'NONE',  ( 162.0862735437575566, 62.63196145447164298, 57.82334402139706953 ) ) ;
#19302 = VERTEX_POINT ( 'NONE', #29800 ) ;
#19303 = CARTESIAN_POINT ( 'NONE',  ( -180.3114074031036580, 97.09758726817788954, -71.21099496842563781 ) ) ;
#19304 = VECTOR ( 'NONE', #3756, 1000.000000000000000 ) ;
#19305 = CARTESIAN_POINT ( 'NONE',  ( 126.3749122082473377, 38.23888021981338170, 91.33587154719414514 ) ) ;
#19306 = PRODUCT_DEFINITION_SHAPE ( 'NONE', 'NONE',  #69581 ) ;
#19307 = CARTESIAN_POINT ( 'NONE',  ( 204.0485454264722023, 107.1608795776555922, -90.03598187893172167 ) ) ;
#19308 = VECTOR ( 'NONE', #58439, 1000.000000000000000 ) ;
#19310 = COLOUR_RGB ( '',0.7921568627450980005, 0.8196078431372548767, 0.9333333333333333481 ) ;
#19309 = DIRECTION ( 'NONE',  ( -1.000000000000000000, -0.000000000000000000, -0.000000000000000000 ) ) ;
#19311 = CARTESIAN_POINT ( 'NONE',  ( -422.6627218934912662, 399.9999999999998295, 113.5502958579882602 ) ) ;
#19312 = EDGE_CURVE ( 'NONE', #25377, #69123, #61798, .T. ) ;
#19313 = AXIS2_PLACEMENT_3D ( 'NONE', #24971, #55936, #7754 ) ;
#19314 = EDGE_LOOP ( 'NONE', ( #37356, #35762, #36812, #9506 ) ) ;
#19315 = CARTESIAN_POINT ( 'NONE',  ( 199.7278513351970162, 99.76879341361765796, 42.34380694319595761 ) ) ;
#19316 = CARTESIAN_POINT ( 'NONE',  ( 116.9200705848630264, 32.09536795999727588, -66.81303021653259577 ) ) ;
#19317 = CARTESIAN_POINT ( 'NONE',  ( 0.000000000000000000, 0.000000000000000000, 41.38025477438755928 ) ) ;
#19318 = CARTESIAN_POINT ( 'NONE',  ( 138.2136629441928903, 45.30947856186672595, 4.042827492293223024 ) ) ;
#19319 = DIRECTION ( 'NONE',  ( -0.7071067811865545671, 2.831068712794148784E-15, -0.7071067811865405783 ) ) ;
#19320 = CLOSED_SHELL ( 'NONE', ( #40021, #16014, #12469, #18035, #28178, #1644, #18820, #20155, #25382, #30202, #67285, #52018 ) ) ;
#19321 = EDGE_CURVE ( 'NONE', #36739, #65910, #39495, .T. ) ;
#19322 = ADVANCED_FACE ( 'NONE', ( #52624 ), #57571, .F. ) ;
#19323 = VERTEX_POINT ( 'NONE', #40685 ) ;
#19324 = EDGE_CURVE ( 'NONE', #54597, #6688, #24186, .T. ) ;
#19325 = CARTESIAN_POINT ( 'NONE',  ( 161.1112535418156426, 61.83422628788724751, -10.21864072077471874 ) ) ;
#19326 = ORIENTED_EDGE ( 'NONE', *, *, #26758, .F. ) ;
#19327 = LINE ( 'NONE', #23917, #25538 ) ;
#19328 = CARTESIAN_POINT ( 'NONE',  ( 140.1990463068371469, 45.38811834026235204, 94.71732886340767266 ) ) ;
#19330 = EDGE_LOOP ( 'NONE', ( #31956, #65786 ) ) ;
#19329 = CARTESIAN_POINT ( 'NONE',  ( 149.0250918491436778, 6.000000000000000000, -4.435653166495538535 ) ) ;
#19331 = CARTESIAN_POINT ( 'NONE',  ( 164.9547823171480161, 65.03046442419432083, -44.18386578002282761 ) ) ;
#19332 = CARTESIAN_POINT ( 'NONE',  ( 563.4809901518626702, 188.0000000000000000, 57.79371821540657095 ) ) ;
#19333 = CARTESIAN_POINT ( 'NONE',  ( 159.6593397521790507, 59.37286298965128140, -50.81150672396304913 ) ) ;
#19334 = ORIENTED_EDGE ( 'NONE', *, *, #53426, .T. ) ;
#19335 = CARTESIAN_POINT ( 'NONE',  ( -72.57286576968809300, 18.73210786364346703, 41.38025477438755928 ) ) ;
#19337 = B_SPLINE_CURVE_WITH_KNOTS ( 'NONE', 3,
 ( #22723, #1615, #55069, #7246, #28706, #40628, #67048, #3693, #51202, #51880, #29390, #52227, #68080, #56829, #62791, #2664, #18840, #56465, #67729, #19881, #3015, #25169, #29738, #24478, #50846, #24125, #39947, #14596, #45568, #61738, #30431, #41338, #40295, #36057, #57511, #9321, #19528, #40984, #45917, #30782, #35719, #62088, #67386, #62446 ),
 .UNSPECIFIED., .F., .F.,
 ( 4, 2, 2, 2, 2, 2, 2, 2, 2, 2, 2, 2, 2, 2, 2, 2, 2, 2, 2, 2, 2, 4 ),
 ( 0.000000000000000000, 0.001488594467279753288, 0.002232891700919617355, 0.002977188934559481422, 0.004465783401839182667, 0.005954377869118883913, 0.007442972336398583424, 0.008187269570038440553, 0.008931566803678297681, 0.01042016127095802928, 0.01190875573823776089, 0.01265305297187762842, 0.01339735020551749423, 0.01488594467279723971, 0.01563024190643711592, 0.01637453914007698866, 0.01786313360735673761, 0.01935172807463648656, 0.02009602530827635236, 0.02084032254191621816, 0.02232891700919592895, 0.02381751147647563974 ),
 .UNSPECIFIED. ) ;
#19336 = CARTESIAN_POINT ( 'NONE',  ( -126.8005235842505840, 47.09307471149450919, 45.57853283965476265 ) ) ;
#19338 = CARTESIAN_POINT ( 'NONE',  ( 150.3360255159550150, 53.55172128635252449, -95.00000000000133582 ) ) ;
#19339 = CARTESIAN_POINT ( 'NONE',  ( 79.19119222799091062, 18.06817527909836230, -15.48292693387985608 ) ) ;
#19340 = FACE_OUTER_BOUND ( 'NONE', #51925, .T. ) ;
#19341 = CARTESIAN_POINT ( 'NONE',  ( -34.06864996337441909, 10.03773626259441798, -62.63357253091302113 ) ) ;
#19342 =( REPRESENTATION_RELATIONSHIP ('NONE','NONE', #46031, #31639 ) REPRESENTATION_RELATIONSHIP_WITH_TRANSFORMATION ( #46991 )SHAPE_REPRESENTATION_RELATIONSHIP( ) );
#19343 = DIRECTION ( 'NONE',  ( -0.000000000000000000, -0.000000000000000000, 1.000000000000000000 ) ) ;
#19344 = ORIENTED_EDGE ( 'NONE', *, *, #56470, .F. ) ;
#19345 = CARTESIAN_POINT ( 'NONE',  ( -94.78138776532239262, 30.24234841992714351, 65.39967122320125270 ) ) ;
#19346 = CARTESIAN_POINT ( 'NONE',  ( -10.23531775138760835, 8.068923942586303966, 57.35362084251622150 ) ) ;
#19347 = ORIENTED_EDGE ( 'NONE', *, *, #13885, .T. ) ;
#19348 = VECTOR ( 'NONE', #47084, 999.9999999999998863 ) ;
#19349 = CARTESIAN_POINT ( 'NONE',  ( 155.7167524447090727, 57.56687707799950715, -9.474077844157728023 ) ) ;
#19350 = CARTESIAN_POINT ( 'NONE',  ( -46.66904755831212981, -10.55634918610397222, 0.000000000000000000 ) ) ;
#19351 = CARTESIAN_POINT ( 'NONE',  ( 109.7782172510783596, 29.77507867835875288, 29.61121420573730845 ) ) ;
#19352 = AXIS2_PLACEMENT_3D ( 'NONE', #39406, #38355, #60854 ) ;
#19353 = CARTESIAN_POINT ( 'NONE',  ( -7.825402957745081878, 7.899365992529270741, 30.11558103944718923 ) ) ;
#19354 = CARTESIAN_POINT ( 'NONE',  ( -452.6627218934913230, 1.665334536937734811E-13, 113.5502958579881749 ) ) ;
#19355 = LINE ( 'NONE', #19014, #53835 ) ;
#19356 = CARTESIAN_POINT ( 'NONE',  ( 157.4703587214989113, 57.65129005721576050, 71.25401806271709404 ) ) ;
#19357 = CARTESIAN_POINT ( 'NONE',  ( 175.8963338753313792, 73.51705463274393537, 15.38615084967059410 ) ) ;
#19358 = CARTESIAN_POINT ( 'NONE',  ( -58.76005811686688673, 15.70653557534867595, 17.51043486912802649 ) ) ;
#19359 = ORIENTED_EDGE ( 'NONE', *, *, #33892, .T. ) ;
#19360 = EDGE_CURVE ( 'NONE', #32729, #18015, #63193, .T. ) ;
#19361 = CARTESIAN_POINT ( 'NONE',  ( 1.667562369266825550, 64.99262834925669097, 0.000000000000000000 ) ) ;
#19362 = ORIENTED_EDGE ( 'NONE', *, *, #66181, .F. ) ;
#19363 = DIRECTION ( 'NONE',  ( -1.000000000000000000, 0.000000000000000000, 0.000000000000000000 ) ) ;
#19364 = CARTESIAN_POINT ( 'NONE',  ( 46.90208227351340753, 10.52324439420451085, -16.51717632370492339 ) ) ;
#19365 = CARTESIAN_POINT ( 'NONE',  ( 40.37438610703017616, 8.537526699166106070, 56.80551099547096072 ) ) ;
#19366 = DIRECTION ( 'NONE',  ( -0.000000000000000000, -0.000000000000000000, -1.000000000000000000 ) ) ;
#19367 = CARTESIAN_POINT ( 'NONE',  ( -1.700272545523339840, 6.569435498413836783, 86.96418197045451848 ) ) ;
#19368 = CARTESIAN_POINT ( 'NONE',  ( -109.6752351740181979, 37.84903014964774570, -14.39328408723732800 ) ) ;
#19369 = VERTEX_POINT ( 'NONE', #36115 ) ;
#19370 = CARTESIAN_POINT ( 'NONE',  ( 23.09119322872580682, -170.0000000000000000, -95.00000000000133582 ) ) ;
#19371 = CARTESIAN_POINT ( 'NONE',  ( -165.7143741370937278, 79.24519349471961505, 63.94847269051136607 ) ) ;
#19372 = ORIENTED_EDGE ( 'NONE', *, *, #17571, .F. ) ;
#19373 = ORIENTED_EDGE ( 'NONE', *, *, #24972, .T. ) ;
#19374 = EDGE_CURVE ( 'NONE', #17233, #11580, #36457, .T. ) ;
#19375 = CARTESIAN_POINT ( 'NONE',  ( -74.99999999999998579, 0.000000000000000000, 85.00000000000000000 ) ) ;
#19376 = CARTESIAN_POINT ( 'NONE',  ( -44.29440389294402536, 17.09499999999999886, 4.000000000000000000 ) ) ;
#19377 = CARTESIAN_POINT ( 'NONE',  ( 173.7246046907419554, 71.47482343504563573, -15.40631472208198005 ) ) ;
#19378 = CARTESIAN_POINT ( 'NONE',  ( 106.4072861358878157, 28.24787347451998087, 70.40525499941243481 ) ) ;
#19379 = DIRECTION ( 'NONE',  ( -0.000000000000000000, 1.000000000000000000, -0.000000000000000000 ) ) ;
#19380 = EDGE_CURVE ( 'NONE', #44589, #13782, #9041, .T. ) ;
#19381 = EDGE_CURVE ( 'NONE', #4738, #7351, #23780, .T. ) ;
#19382 = CARTESIAN_POINT ( 'NONE',  ( 58.47885130911549822, 12.69429933094348684, -22.36869975670756361 ) ) ;
#19383 = ORIENTED_EDGE ( 'NONE', *, *, #67534, .F. ) ;
#19384 = DIRECTION ( 'NONE',  ( -0.000000000000000000, 1.000000000000000000, -0.000000000000000000 ) ) ;
#19385 = ORIENTED_EDGE ( 'NONE', *, *, #8093, .T. ) ;
#19386 = CARTESIAN_POINT ( 'NONE',  ( 21.75198946226450403, 7.772524967554915953, -47.59311735406298993 ) ) ;
#19387 = CARTESIAN_POINT ( 'NONE',  ( -146.5309471467636513, 62.99917515507676313, 45.10861342454792577 ) ) ;
#19388 = CARTESIAN_POINT ( 'NONE',  ( 212.1983751099433277, 117.2326047784726910, 36.84905167329434050 ) ) ;
#19389 = FACE_BOUND ( 'NONE', #26201, .T. ) ;
#19390 = ORIENTED_EDGE ( 'NONE', *, *, #18430, .T. ) ;
#19391 = VERTEX_POINT ( 'NONE', #13962 ) ;
#19392 = CARTESIAN_POINT ( 'NONE',  ( 113.9728608271480965, -21.78879854653021297, -3.053399776244579478 ) ) ;
#19393 = LINE ( 'NONE', #46822, #31648 ) ;
#19394 = CARTESIAN_POINT ( 'NONE',  ( 32.09610685027467269, 8.582590950734788393, -71.67746533053700375 ) ) ;
#19395 = DIRECTION ( 'NONE',  ( 0.000000000000000000, 0.000000000000000000, 1.000000000000000000 ) ) ;
#19396 = CARTESIAN_POINT ( 'NONE',  ( 8.730760620888057488, 6.377258547620704654, 93.82534041452976226 ) ) ;
#19397 = EDGE_CURVE ( 'NONE', #40260, #19424, #46211, .T. ) ;
#19398 = CARTESIAN_POINT ( 'NONE',  ( 22.85407693638847348, 7.837765153256906814, 88.66769795570787949 ) ) ;
#19399 = AXIS2_PLACEMENT_3D ( 'NONE', #4120, #25588, #62520 ) ;
#19400 = ORIENTED_EDGE ( 'NONE', *, *, #32858, .F. ) ;
#19401 = EDGE_CURVE ( 'NONE', #16146, #41880, #3074, .T. ) ;
#19402 = CARTESIAN_POINT ( 'NONE',  ( 34.41143668122415988, 66.58502636910522199, 41.38025477438755928 ) ) ;
#19403 = CARTESIAN_POINT ( 'NONE',  ( 199.7291770695759965, 101.4092159658446946, -38.20255649232857564 ) ) ;
#19404 = ORIENTED_EDGE ( 'NONE', *, *, #28764, .T. ) ;
#19405 = CIRCLE ( 'NONE', #4789, 8.000000000000000000 ) ;
#19406 = CARTESIAN_POINT ( 'NONE',  ( 107.2081108419789359, 28.60378084105236240, -90.20802963420143783 ) ) ;
#19407 = EDGE_LOOP ( 'NONE', ( #26407, #55770, #17783, #43299 ) ) ;
#19408 = CARTESIAN_POINT ( 'NONE',  ( -78.66644367742111399, 22.32174330031318377, -76.96000122218160300 ) ) ;
#19409 = CARTESIAN_POINT ( 'NONE',  ( -56.97556689808916985, 16.24958672959847661, -8.618408225133944001 ) ) ;
#19410 = AXIS2_PLACEMENT_3D ( 'NONE', #49515, #34422, #38995 ) ;
#19411 = ORIENTED_EDGE ( 'NONE', *, *, #33057, .T. ) ;
#19412 = VECTOR ( 'NONE', #31215, 1000.000000000000000 ) ;
#19413 = ORIENTED_EDGE ( 'NONE', *, *, #22139, .F. ) ;
#19414 = LINE ( 'NONE', #66937, #65596 ) ;
#19415 = DIRECTION ( 'NONE',  ( -0.000000000000000000, -0.000000000000000000, -1.000000000000000000 ) ) ;
#19416 = CARTESIAN_POINT ( 'NONE',  ( 105.4134760436918299, 27.80903124201758558, 16.02569942440996087 ) ) ;
#19417 = ORIENTED_EDGE ( 'NONE', *, *, #37908, .F. ) ;
#19418 = CARTESIAN_POINT ( 'NONE',  ( -24.67506180694751450, 8.578306485686441718, 88.10122643889526728 ) ) ;
#19419 = CARTESIAN_POINT ( 'NONE',  ( 175.5498284945444709, 74.57669191966280664, -75.65732398570116857 ) ) ;
#19420 = FACE_OUTER_BOUND ( 'NONE', #33713, .T. ) ;
#19421 = DIRECTION ( 'NONE',  ( 1.063100223296055310E-16, 0.6427876096865404731, 0.7660444431189771253 ) ) ;
#19422 = CARTESIAN_POINT ( 'NONE',  ( 82.95856197793166587, 19.25847567427440765, -49.88006847027852331 ) ) ;
#19423 = CARTESIAN_POINT ( 'NONE',  ( -169.3509183217342127, 84.49925590041679868, -89.40419402843292573 ) ) ;
#19424 = VERTEX_POINT ( 'NONE', #24872 ) ;
#19426 = ORIENTED_EDGE ( 'NONE', *, *, #59193, .T. ) ;
#19425 = PRODUCT_RELATED_PRODUCT_CATEGORY ( 'part', '', ( #4024 ) ) ;
#19427 = FACE_OUTER_BOUND ( 'NONE', #3063, .T. ) ;
#19428 = CARTESIAN_POINT ( 'NONE',  ( -180.4355333984925096, 97.25072438123878271, 90.31203738677328374 ) ) ;
#19429 = CARTESIAN_POINT ( 'NONE',  ( 230.9999999999999432, -35.00000000000000000, -2.000000000000000000 ) ) ;
#19430 = CYLINDRICAL_SURFACE ( 'NONE', #20889, 7.500000000000027534 ) ;
#19431 = CARTESIAN_POINT ( 'NONE',  ( -37.98601804829807094, 14.28438006995819798, 82.99999999999997158 ) ) ;
#19432 = CARTESIAN_POINT ( 'NONE',  ( -27.40035611173194852, 8.962996713195352072, -90.17232150666276880 ) ) ;
#19433 = CARTESIAN_POINT ( 'NONE',  ( 210.9748732031754628, 117.1974929539830441, 86.27819310157629218 ) ) ;
#19434 = ADVANCED_FACE ( 'NONE', ( #14317 ), #13616, .F. ) ;
#19435 = CARTESIAN_POINT ( 'NONE',  ( 207.2640160519426047, 111.6867652229576322, 29.65748712772104767 ) ) ;
#19436 = FACE_OUTER_BOUND ( 'NONE', #19796, .T. ) ;
#19437 = CARTESIAN_POINT ( 'NONE',  ( -109.7793173546316723, 36.75648380851384900, 38.30271184306513277 ) ) ;
#19438 = ORIENTED_EDGE ( 'NONE', *, *, #42540, .T. ) ;
#19439 = EDGE_CURVE ( 'NONE', #26339, #41403, #66479, .T. ) ;
#19440 = CARTESIAN_POINT ( 'NONE',  ( 13.36262230781615301, 7.441298897118794997, -9.060692098087766766 ) ) ;
#19441 = EDGE_LOOP ( 'NONE', ( #64915, #32629, #11645, #58789 ) ) ;
#19442 = CARTESIAN_POINT ( 'NONE',  ( 197.5334904971816741, 97.00846725096933199, -14.74015068199268441 ) ) ;
#19443 = VERTEX_POINT ( 'NONE', #51940 ) ;
#19444 = CARTESIAN_POINT ( 'NONE',  ( -147.3669217311067428, 63.69361261596462498, 4.184853556603538749 ) ) ;
#19445 = AXIS2_PLACEMENT_3D ( 'NONE', #40135, #51725, #19363 ) ;
#19446 = CARTESIAN_POINT ( 'NONE',  ( 188.2091813586561386, 87.61952156613882892, -68.21099885728685308 ) ) ;
#19447 = CARTESIAN_POINT ( 'NONE',  ( -144.9412191745148277, 61.69548892475974355, 71.03477123040856611 ) ) ;
#19448 = CARTESIAN_POINT ( 'NONE',  ( 0.7145311798163248573, -4.618802153517011178, 8.000000000000000000 ) ) ;
#19449 = CARTESIAN_POINT ( 'NONE',  ( 39.40195752203891999, 8.409560354027407314, -35.61981746542776506 ) ) ;
#19450 = AXIS2_PLACEMENT_3D ( 'NONE', #30179, #4135, #8380 ) ;
#19451 = LINE ( 'NONE', #57095, #104 ) ;
#19452 = CARTESIAN_POINT ( 'NONE',  ( 14.80291736570133843, 7.477373894757625372, -35.56751837549798978 ) ) ;
#19453 = CARTESIAN_POINT ( 'NONE',  ( 128.0568017572569204, 38.03085713813910473, -48.30530462611437770 ) ) ;
#19454 = EDGE_LOOP ( 'NONE', ( #17019, #23571, #10383, #17440 ) ) ;
#19455 = AXIS2_PLACEMENT_3D ( 'NONE', #60770, #34051, #24201 ) ;
#19456 = ORIENTED_EDGE ( 'NONE', *, *, #47699, .T. ) ;
#19457 = EDGE_CURVE ( 'NONE', #60501, #30745, #47010, .T. ) ;
#19458 = VECTOR ( 'NONE', #14028, 1000.000000000000114 ) ;
#19459 = CARTESIAN_POINT ( 'NONE',  ( -31.11269837220801193, 36.11269837220812207, 85.00100000000000477 ) ) ;
#19460 = CARTESIAN_POINT ( 'NONE',  ( -35.06172898939804838, 15.49744344258353479, 13.32819299319722539 ) ) ;
#19461 = CARTESIAN_POINT ( 'NONE',  ( -28.13852122803041667, 9.072484007196644384, -76.41398812605804380 ) ) ;
#19462 = EDGE_CURVE ( 'NONE', #5114, #17560, #35665, .T. ) ;
#19463 = EDGE_CURVE ( 'NONE', #20755, #30529, #57469, .T. ) ;
#19464 = VECTOR ( 'NONE', #54996, 1000.000000000000000 ) ;
#19465 = CARTESIAN_POINT ( 'NONE',  ( 12.03194517566455701, 6.409266703743583093, 17.18016951692776217 ) ) ;
#19466 = CARTESIAN_POINT ( 'NONE',  ( 281.3012118866374180, 21.46131765974229566, -4.839032743736807696 ) ) ;
#19467 = FACE_OUTER_BOUND ( 'NONE', #24063, .T. ) ;
#19468 = CARTESIAN_POINT ( 'NONE',  ( 174.9042454172880241, 72.57746269938726869, -66.28938837206885637 ) ) ;
#19469 = CARTESIAN_POINT ( 'NONE',  ( 26.99999999999999645, 0.000000000000000000, 12.00000000000000000 ) ) ;
#19470 = CARTESIAN_POINT ( 'NONE',  ( 93.85846834761628088, 22.01563781856518887, -18.49024407162987416 ) ) ;
#19471 = CARTESIAN_POINT ( 'NONE',  ( -24.71645982722741408, 9.599558729461495687, 67.89525075705670076 ) ) ;
#19472 = DIRECTION ( 'NONE',  ( 5.294909809750763265E-16, 1.000000000000000000, 1.110223024625156171E-16 ) ) ;
#19473 = CARTESIAN_POINT ( 'NONE',  ( -54.57280099357648595, 14.55288945003961665, 57.16187836339484107 ) ) ;
#19474 = CARTESIAN_POINT ( 'NONE',  ( -0.3747453031323929595, 6.520267647591904137, 63.47172518997308543 ) ) ;
#19475 = ORIENTED_EDGE ( 'NONE', *, *, #15710, .T. ) ;
#19476 = CARTESIAN_POINT ( 'NONE',  ( 63.01563776193091826, 13.70579113808095073, -23.87614024170608218 ) ) ;
#19477 = CARTESIAN_POINT ( 'NONE',  ( 150.0980941434704903, 53.37942190380066876, 62.34908842616228242 ) ) ;
#19478 = CARTESIAN_POINT ( 'NONE',  ( -109.7156874346698316, 37.87149323084331343, -68.34337640632028865 ) ) ;
#19479 = CARTESIAN_POINT ( 'NONE',  ( -47.55360235114365963, 12.79819361309568215, -43.22893570361206628 ) ) ;
#19480 = CARTESIAN_POINT ( 'NONE',  ( -45.00000000000000000, 22.99999999999998579, 4.000000000000000000 ) ) ;
#19481 = DIRECTION ( 'NONE',  ( 1.000000000000000000, -0.000000000000000000, 0.000000000000000000 ) ) ;
#19482 = ORIENTED_EDGE ( 'NONE', *, *, #21650, .F. ) ;
#19483 = ADVANCED_FACE ( 'NONE', ( #19232 ), #32901, .F. ) ;
#19484 = SURFACE_STYLE_FILL_AREA ( #32889 ) ;
#19485 = CARTESIAN_POINT ( 'NONE',  ( -30.00000000000000355, -27.00000000000000355, 15.00000000000000000 ) ) ;
#19486 = VERTEX_POINT ( 'NONE', #16027 ) ;
#19487 = ORIENTED_EDGE ( 'NONE', *, *, #62836, .T. ) ;
#19488 = AXIS2_PLACEMENT_3D ( 'NONE', #10038, #63167, #30459 ) ;
#19489 = CARTESIAN_POINT ( 'NONE',  ( 9.737557066527559257, 200.0000000000000000, 2.275957463600584596 ) ) ;
#19490 = LINE ( 'NONE', #14225, #2938 ) ;
#19491 = CARTESIAN_POINT ( 'NONE',  ( -39.29440389294403246, -17.09499999999999886, 4.000000000000000000 ) ) ;
#19492 = ORIENTED_EDGE ( 'NONE', *, *, #16493, .T. ) ;
#19493 = DIRECTION ( 'NONE',  ( -0.000000000000000000, -0.000000000000000000, 1.000000000000000000 ) ) ;
#19494 = DIRECTION ( 'NONE',  ( 1.000000000000000000, 0.000000000000000000, 0.000000000000000000 ) ) ;
#19495 = CARTESIAN_POINT ( 'NONE',  ( 104.0290905220488469, -170.0000000000000000, 94.99999999999866418 ) ) ;
#19496 = AXIS2_PLACEMENT_3D ( 'NONE', #5929, #50254, #19274 ) ;
#19497 = CYLINDRICAL_SURFACE ( 'NONE', #69075, 5.000000000000004441 ) ;
#19498 = CARTESIAN_POINT ( 'NONE',  ( -84.23336401058611500, 25.60798568215573923, 42.96773630549936485 ) ) ;
#19499 = CARTESIAN_POINT ( 'NONE',  ( 8.000000000000007105, 249.8719672152120381, 94.99999999999866418 ) ) ;
#19500 = AXIS2_PLACEMENT_3D ( 'NONE', #36849, #46702, #62891 ) ;
#19501 = CARTESIAN_POINT ( 'NONE',  ( 141.0645618855930650, 45.95036951196543384, 8.026184627116476733 ) ) ;
#19502 = VECTOR ( 'NONE', #34413, 1000.000000000000000 ) ;
#19503 = ORIENTED_EDGE ( 'NONE', *, *, #41443, .F. ) ;
#19504 = CIRCLE ( 'NONE', #25149, 21.99999999999998579 ) ;
#19505 = LINE ( 'NONE', #50138, #36823 ) ;
#19506 = CIRCLE ( 'NONE', #61093, 65.00000000000000000 ) ;
#19507 = CARTESIAN_POINT ( 'NONE',  ( 12.03317402819681803, 6.409531826169462931, 57.86235655824060586 ) ) ;
#19508 = B_SPLINE_CURVE_WITH_KNOTS ( 'NONE', 3,
 ( #55061, #28333, #27637, #914, #1606, #22363, #22714, #50146, #1970, #11803, #43801, #38540, #44153, #23068, #37848, #11110, #44520, #65995, #23429, #44868, #59294, #32575, #46242, #30084, #3007, #56819, #40288, #29052, #50493, #45557, #51540, #3684, #24466, #67720, #25161, #3347, #46589, #18830, #24807, #2315, #13216, #30424, #12870, #7595, #61731, #18484, #13557, #45910 ),
 .UNSPECIFIED., .F., .F.,
 ( 4, 2, 2, 2, 2, 2, 2, 2, 2, 2, 2, 2, 2, 2, 2, 2, 2, 2, 2, 2, 2, 2, 2, 4 ),
 ( 0.02746511744866866542, 0.02914922134997094058, 0.03083332525127321228, 0.03251742915257548744, 0.03335948110322665278, 0.03420153305387781811, 0.03504358500452898345, 0.03588563695518015573, 0.03756974085648243783, 0.03841179280713359623, 0.03925384475778478238, 0.04009589670843596160, 0.04093794865908714081, 0.04262205256038945761, 0.04430615646169178135, 0.04514820841234293974, 0.04599026036299409814, 0.04767436426429639412, 0.04935846816559869010, 0.05020052011624982768, 0.05104257206690095833, 0.05272667596820322655, 0.05356872791885436413, 0.05441077986950550865 ),
 .UNSPECIFIED. ) ;
#19509 = CARTESIAN_POINT ( 'NONE',  ( -125.8938041572051389, 47.69968343338780414, 18.77539728269342945 ) ) ;
#19510 = CARTESIAN_POINT ( 'NONE',  ( -78.40344607829260326, 23.29806210341294914, 84.10570090962099243 ) ) ;
#19512 = ORIENTED_EDGE ( 'NONE', *, *, #10938, .F. ) ;
#19511 = DIRECTION ( 'NONE',  ( -1.000000000000000000, 0.000000000000000000, 0.000000000000000000 ) ) ;
#19513 = DIRECTION ( 'NONE',  ( -1.000000000000000000, -0.000000000000000000, -0.000000000000000000 ) ) ;
#19514 = ORIENTED_EDGE ( 'NONE', *, *, #11890, .T. ) ;
#19515 = AXIS2_PLACEMENT_3D ( 'NONE', #37439, #58546, #6121 ) ;
#19516 = EDGE_CURVE ( 'NONE', #43039, #58488, #10750, .T. ) ;
#19517 = ORIENTED_EDGE ( 'NONE', *, *, #14455, .T. ) ;
#19518 = CARTESIAN_POINT ( 'NONE',  ( 15.78827728214693416, -170.0000000000000000, -16.17439350822211352 ) ) ;
#19519 = LINE ( 'NONE', #68409, #23290 ) ;
#19520 = DIRECTION ( 'NONE',  ( -0.000000000000000000, -0.000000000000000000, -1.000000000000000000 ) ) ;
#19521 = DIRECTION ( 'NONE',  ( -0.000000000000000000, -0.000000000000000000, -1.000000000000000000 ) ) ;
#19522 = EDGE_CURVE ( 'NONE', #25277, #242, #547, .T. ) ;
#19523 = SHAPE_REPRESENTATION ( 'lock', ( #66832 ), #12941 ) ;
#19524 = CARTESIAN_POINT ( 'NONE',  ( -27.00000000000000355, -30.00000000000000355, 12.00000000000000000 ) ) ;
#19525 = DIRECTION ( 'NONE',  ( 0.000000000000000000, 0.000000000000000000, 1.000000000000000000 ) ) ;
#19526 = CARTESIAN_POINT ( 'NONE',  ( 17.45129144173298386, 7.566322476434613975, -89.38286583354187087 ) ) ;
#19527 = EDGE_CURVE ( 'NONE', #47684, #66948, #67617, .T. ) ;
#19528 = CARTESIAN_POINT ( 'NONE',  ( -51.34542473642581939, 14.75635007918829089, 31.29311869111193900 ) ) ;
#19529 = EDGE_LOOP ( 'NONE', ( #25599, #61255, #48711, #10755 ) ) ;
#19530 = EDGE_LOOP ( 'NONE', ( #68339, #9043 ) ) ;
#19531 = CARTESIAN_POINT ( 'NONE',  ( -103.2164890789475464, 34.39030697009940951, 18.63064823786974245 ) ) ;
#19532 = ADVANCED_FACE ( 'NONE', ( #16716 ), #4447, .F. ) ;
#19533 = CARTESIAN_POINT ( 'NONE',  ( -200.0000000000000000, 2.449293598294706434E-14, -7.000000000000000000 ) ) ;
#19534 = CARTESIAN_POINT ( 'NONE',  ( 164.9559213734325169, 63.71338633026441300, 64.29752433092906472 ) ) ;
#19535 = DIRECTION ( 'NONE',  ( -0.000000000000000000, -0.000000000000000000, -1.000000000000000000 ) ) ;
#19536 = LINE ( 'NONE', #3367, #62940 ) ;
#19537 = CARTESIAN_POINT ( 'NONE',  ( -452.6627218934913230, 1.665334536937734811E-13, 83.55029585798817493 ) ) ;
#19538 = CARTESIAN_POINT ( 'NONE',  ( 46.66904755831207297, -15.55634918610412853, 2.000000000000001776 ) ) ;
#19539 = ORIENTED_EDGE ( 'NONE', *, *, #61323, .F. ) ;
#19540 = EDGE_LOOP ( 'NONE', ( #63713, #12270, #61069, #48577, #4385, #63890, #50946, #25404, #56667, #38404, #17709 ) ) ;
#19541 = ORIENTED_EDGE ( 'NONE', *, *, #42231, .F. ) ;
#19542 = AXIS2_PLACEMENT_3D ( 'NONE', #24340, #66223, #67258 ) ;
#19543 = CARTESIAN_POINT ( 'NONE',  ( -153.6946616617039467, 69.16142959008689672, -21.70738820025326632 ) ) ;
#19544 = CARTESIAN_POINT ( 'NONE',  ( -79.14127775978546708, 22.50259208414362178, 57.26275173013681297 ) ) ;
#19545 = ADVANCED_FACE ( 'NONE', ( #68795 ), #10399, .F. ) ;
#19546 = CARTESIAN_POINT ( 'NONE',  ( 51.65020416916155455, -1.250000000000021760, 26.66469104408689006 ) ) ;
#19547 = DIRECTION ( 'NONE',  ( 0.9959742939952397345, -0.08963930890342655666, 0.000000000000000000 ) ) ;
#19548 = DIRECTION ( 'NONE',  ( 0.000000000000000000, 0.000000000000000000, 1.000000000000000000 ) ) ;
#19549 = AXIS2_PLACEMENT_3D ( 'NONE', #15987, #42716, #59574 ) ;
#19550 = LINE ( 'NONE', #26209, #36046 ) ;
#19551 = VECTOR ( 'NONE', #63420, 1000.000000000000000 ) ;
#19552 = CARTESIAN_POINT ( 'NONE',  ( 32.90878072717890035, 7.653588083204840409, 68.01993794000820515 ) ) ;
#19553 = CARTESIAN_POINT ( 'NONE',  ( 10.83418588031599228, 6.392467435475929882, -21.82701683438974882 ) ) ;
#19554 = ORIENTED_EDGE ( 'NONE', *, *, #25498, .T. ) ;
#19555 = CARTESIAN_POINT ( 'NONE',  ( -31.43908319763710679, -170.0000000000000000, 64.56100499665288339 ) ) ;
#19556 = DIRECTION ( 'NONE',  ( -9.729547286656084292E-15, -7.216449660064492742E-16, -1.000000000000000000 ) ) ;
#19557 = CARTESIAN_POINT ( 'NONE',  ( -118.3927673406137586, 41.74929850983304647, 11.51331731855512075 ) ) ;
#19558 = FACE_OUTER_BOUND ( 'NONE', #2123, .T. ) ;
#19559 = AXIS2_PLACEMENT_3D ( 'NONE', #11833, #34357, #60013 ) ;
#19560 = CARTESIAN_POINT ( 'NONE',  ( -44.99999999999998579, -25.00000000000000000, 2.000000000000015543 ) ) ;
#19561 = DIRECTION ( 'NONE',  ( 0.000000000000000000, 0.000000000000000000, -1.000000000000000000 ) ) ;
#19562 = DIRECTION ( 'NONE',  ( -0.000000000000000000, -0.000000000000000000, -1.000000000000000000 ) ) ;
#19563 = VECTOR ( 'NONE', #18464, 1000.000000000000000 ) ;
#19564 = AXIS2_PLACEMENT_3D ( 'NONE', #14047, #19319, #8787 ) ;
#19565 = VERTEX_POINT ( 'NONE', #47680 ) ;
#19567 = AXIS2_PLACEMENT_3D ( 'NONE', #54925, #60906, #28914 ) ;
#19566 = SHAPE_DEFINITION_REPRESENTATION ( #48392, #46031 ) ;
#19568 = CARTESIAN_POINT ( 'NONE',  ( 259.4165763529819060, 225.8585178651493948, 108.9999999999999858 ) ) ;
#19569 = CARTESIAN_POINT ( 'NONE',  ( 0.000000000000000000, 0.000000000000000000, -9.500000000000000000 ) ) ;
#19570 = CARTESIAN_POINT ( 'NONE',  ( 14.99999999999998579, 0.000000000000000000, 0.000000000000000000 ) ) ;
#19571 = CYLINDRICAL_SURFACE ( 'NONE', #42294, 125.0000000000000000 ) ;
#19572 = VERTEX_POINT ( 'NONE', #43444 ) ;
#19573 = ORIENTED_EDGE ( 'NONE', *, *, #1780, .F. ) ;
#19574 = DIRECTION ( 'NONE',  ( 1.000000000000000000, 0.000000000000000000, 0.000000000000000000 ) ) ;
#19575 = CARTESIAN_POINT ( 'NONE',  ( 201.9822477997853127, 104.3642793804899895, 2.860239141982756195 ) ) ;
#19576 = EDGE_LOOP ( 'NONE', ( #52961, #51215, #7528, #12119, #40259, #37087, #26916, #15681, #20765 ) ) ;
#19577 = CARTESIAN_POINT ( 'NONE',  ( 164.9669969155543185, 65.04083371431683247, 90.15876886485268926 ) ) ;
#19578 = VERTEX_POINT ( 'NONE', #47337 ) ;
#19579 = CARTESIAN_POINT ( 'NONE',  ( -58.33157376762795820, 16.63098604184964557, 17.72246446630213512 ) ) ;
#19580 = DIRECTION ( 'NONE',  ( 0.000000000000000000, 0.000000000000000000, 1.000000000000000000 ) ) ;
#19581 = CARTESIAN_POINT ( 'NONE',  ( -156.9262190792699414, 72.10659547035872663, 39.35937735580755970 ) ) ;
#19582 = CARTESIAN_POINT ( 'NONE',  ( -101.3602137809054540, 32.31558061113913993, 30.56121215972862615 ) ) ;
#19583 = DIRECTION ( 'NONE',  ( -0.000000000000000000, -0.000000000000000000, -1.000000000000000000 ) ) ;
#19585 = ORIENTED_EDGE ( 'NONE', *, *, #28499, .T. ) ;
#19584 = DIRECTION ( 'NONE',  ( 1.000000000000000000, 0.000000000000000000, 0.000000000000000000 ) ) ;
#19586 = EDGE_CURVE ( 'NONE', #28536, #53100, #60827, .T. ) ;
#19587 = CARTESIAN_POINT ( 'NONE',  ( 313.9975424824652350, 18.00000000000002842, 536.6193948016162949 ) ) ;
#19588 = EDGE_LOOP ( 'NONE', ( #43297, #40481, #48192, #23884 ) ) ;
#19589 = VERTEX_POINT ( 'NONE', #48358 ) ;
#19590 = CARTESIAN_POINT ( 'NONE',  ( 174.2538192999570299, 73.34752463892031926, 33.69852078121099481 ) ) ;
#19591 = VECTOR ( 'NONE', #59712, 1000.000000000000000 ) ;
#19592 = CARTESIAN_POINT ( 'NONE',  ( 21.75684465274325063, 6.764994602232766496, -65.29556045911284912 ) ) ;
#19593 = AXIS2_PLACEMENT_3D ( 'NONE', #33671, #54395, #38581 ) ;
#19595 = ORIENTED_EDGE ( 'NONE', *, *, #6848, .T. ) ;
#19594 = CARTESIAN_POINT ( 'NONE',  ( -130.1938957973835613, 50.61368074696269304, 58.80196259642822554 ) ) ;
#19596 = CARTESIAN_POINT ( 'NONE',  ( -101.7497140795961883, 33.63993131142439807, 84.22103294299186871 ) ) ;
#19597 = CYLINDRICAL_SURFACE ( 'NONE', #19399, 7.500000000000020428 ) ;
#19598 = AXIS2_PLACEMENT_3D ( 'NONE', #16348, #33238, #37113 ) ;
#19599 = EDGE_LOOP ( 'NONE', ( #59973, #54842, #54178, #10059 ) ) ;
#19600 = CARTESIAN_POINT ( 'NONE',  ( -59.95707852844800101, 16.05120821151901822, -21.56757814541855112 ) ) ;
#19601 = AXIS2_PLACEMENT_3D ( 'NONE', #43581, #32353, #37613 ) ;
#19602 = VECTOR ( 'NONE', #61461, 1000.000000000000000 ) ;
#19603 = EDGE_CURVE ( 'NONE', #22089, #47148, #32292, .T. ) ;
#19604 = CARTESIAN_POINT ( 'NONE',  ( -50.00000000000001421, -19.99999999999996447, 2.000000000000015543 ) ) ;
#19605 = CARTESIAN_POINT ( 'NONE',  ( 116.8917656767876565, 33.20682060519247614, 40.59075185124044793 ) ) ;
#19606 = VECTOR ( 'NONE', #49236, 1000.000000000000000 ) ;
#19607 = DIRECTION ( 'NONE',  ( 0.000000000000000000, 0.000000000000000000, 1.000000000000000000 ) ) ;
#19608 = CARTESIAN_POINT ( 'NONE',  ( -101.8191498210054959, 32.54686850610961812, -76.85912785543960979 ) ) ;
#19609 = VERTEX_POINT ( 'NONE', #60683 ) ;
#19610 = ORIENTED_EDGE ( 'NONE', *, *, #18202, .F. ) ;
#19611 = EDGE_CURVE ( 'NONE', #57474, #7362, #61377, .T. ) ;
#19612 = CARTESIAN_POINT ( 'NONE',  ( -143.3980294393559234, 60.45217072626395094, -19.82599328075919232 ) ) ;
#19613 = SPHERICAL_SURFACE ( 'NONE', #23333, 3.000000000000000000 ) ;
#19614 = CARTESIAN_POINT ( 'NONE',  ( 0.7145311798163216377, 4.618802153517004960, 7.999999999999998224 ) ) ;
#19615 = CARTESIAN_POINT ( 'NONE',  ( -52.14489132612000333, 13.92110435672092450, -89.48874280495719802 ) ) ;
#19616 = CARTESIAN_POINT ( 'NONE',  ( -50.48111445489777793, 14.53992017381783697, -90.45588132977169948 ) ) ;
#19617 = CYLINDRICAL_SURFACE ( 'NONE', #3435, 4.999999999999997335 ) ;
#19618 = CARTESIAN_POINT ( 'NONE',  ( 70.45451534980409747, 15.56315969138428557, -44.20839769585855805 ) ) ;
#19619 = DIRECTION ( 'NONE',  ( -1.000000000000000000, 0.000000000000000000, 0.000000000000000000 ) ) ;
#19620 = CARTESIAN_POINT ( 'NONE',  ( -170.2747214445849977, 84.01465441107040988, -62.10472265096723987 ) ) ;
#19621 = EDGE_LOOP ( 'NONE', ( #31353, #25365, #69298, #12441 ) ) ;
#19622 = CARTESIAN_POINT ( 'NONE',  ( -109.3386876948163575, 37.66246927061209959, 35.43368312552478017 ) ) ;
#19623 = ORIENTED_EDGE ( 'NONE', *, *, #9005, .F. ) ;
#19624 = CARTESIAN_POINT ( 'NONE',  ( -38.54881010929333485, 10.86689971295296786, 13.30968753690000383 ) ) ;
#19625 = CARTESIAN_POINT ( 'NONE',  ( 22.18075376363927020, -11.79626863379931656, 3.061616997868437868E-16 ) ) ;
#19626 = VERTEX_POINT ( 'NONE', #898 ) ;
#19627 = CARTESIAN_POINT ( 'NONE',  ( -30.00000000000000355, 26.99999999999999645, 12.00000000000000000 ) ) ;
#19628 = EDGE_CURVE ( 'NONE', #36796, #34795, #1592, .T. ) ;
#19629 = LINE ( 'NONE', #47050, #55807 ) ;
#19630 = CARTESIAN_POINT ( 'NONE',  ( 38.43102714813441878, 9.298961820315049920, 3.116234321035345811 ) ) ;
#19631 = CARTESIAN_POINT ( 'NONE',  ( -15.47041015649658391, 73.39774458108210808, 170.0000000000000000 ) ) ;
#19632 = CARTESIAN_POINT ( 'NONE',  ( 36.08729376665094435, 8.001156100723203934, 17.31492220065397447 ) ) ;
#19633 = CARTESIAN_POINT ( 'NONE',  ( -51.55432439150845170, 3.384920705045805001, 26.66469066592269144 ) ) ;
#19634 = CARTESIAN_POINT ( 'NONE',  ( -33.38294402636582703, 10.93918551420889962, -8.712282913815599272 ) ) ;
#19635 = ORIENTED_EDGE ( 'NONE', *, *, #61493, .F. ) ;
#19636 = CARTESIAN_POINT ( 'NONE',  ( -123.0640300519512635, 45.85328288118120810, -89.14461900415201967 ) ) ;
#19637 = VERTEX_POINT ( 'NONE', #23055 ) ;
#19638 = CARTESIAN_POINT ( 'NONE',  ( -31.73109799811232890, -21.50890718406003188, 13.32819397642332326 ) ) ;
#19639 = DIRECTION ( 'NONE',  ( -1.000000000000000000, 0.000000000000000000, 0.000000000000000000 ) ) ;
#19640 = CARTESIAN_POINT ( 'NONE',  ( -26.88245755577922580, 8.887394979218512958, 4.894357216155159840 ) ) ;
#19641 = ORIENTED_EDGE ( 'NONE', *, *, #23180, .T. ) ;
#19642 = LINE ( 'NONE', #18611, #34530 ) ;
#19643 = CARTESIAN_POINT ( 'NONE',  ( -15.27748264047829352, 7.491388194171920034, -68.78227764318798165 ) ) ;
#19644 = CARTESIAN_POINT ( 'NONE',  ( -35.17600017528511103, 10.23461991275926941, 31.20910972668009009 ) ) ;
#19645 = PRESENTATION_STYLE_ASSIGNMENT (( #24933 ) ) ;
#19646 = VECTOR ( 'NONE', #36400, 1000.000000000000000 ) ;
#19647 = ORIENTED_EDGE ( 'NONE', *, *, #20870, .T. ) ;
#19648 = CARTESIAN_POINT ( 'NONE',  ( 848.0071894358271720, 992.0915846175191746, 569.0068267248692564 ) ) ;
#19649 = LINE ( 'NONE', #41462, #46409 ) ;
#19650 = CARTESIAN_POINT ( 'NONE',  ( -124.1033713525885673, 45.32626312604506325, 45.40670476773291142 ) ) ;
#19651 = DIRECTION ( 'NONE',  ( -1.000000000000000000, 0.000000000000000000, 0.000000000000000000 ) ) ;
#19652 = VERTEX_POINT ( 'NONE', #6524 ) ;
#19654 = CARTESIAN_POINT ( 'NONE',  ( -180.3161328724958423, 97.10341277064809162, -66.91777817630556058 ) ) ;
#19653 = VECTOR ( 'NONE', #45564, 1000.000000000000000 ) ;
#19655 = AXIS2_PLACEMENT_3D ( 'NONE', #53954, #868, #32190 ) ;
#19656 = CARTESIAN_POINT ( 'NONE',  ( 126.3615183855829116, 38.23138460739041022, 90.24396629769827882 ) ) ;
#19657 = CARTESIAN_POINT ( 'NONE',  ( 111.1868021579657153, 29.32055685204860396, 44.56662876905394199 ) ) ;
#19658 = AXIS2_PLACEMENT_3D ( 'NONE', #10322, #63458, #20197 ) ;
#19659 = CARTESIAN_POINT ( 'NONE',  ( 6.400000000000000355, 4.618802153517001408, -8.000000000000000000 ) ) ;
#19660 = CIRCLE ( 'NONE', #42097, 125.0000000000000000 ) ;
#19661 = CARTESIAN_POINT ( 'NONE',  ( 0.000000000000000000, 0.000000000000000000, 2.000000000000001776 ) ) ;
#19662 = ORIENTED_EDGE ( 'NONE', *, *, #17869, .F. ) ;
#19663 = CARTESIAN_POINT ( 'NONE',  ( 204.6977192012829789, 106.3443248447423457, 44.20772073876944575 ) ) ;
#19664 = CARTESIAN_POINT ( 'NONE',  ( 56.67004931728209982, -170.0000000000000000, 94.99999999999866418 ) ) ;
#19665 = CARTESIAN_POINT ( 'NONE',  ( 187.6511924654682275, 87.00187850361886888, 33.17587653223696265 ) ) ;
#19666 = CARTESIAN_POINT ( 'NONE',  ( 181.4360341826970853, 78.96155396928541848, -89.91415884680696990 ) ) ;
#19667 = DIRECTION ( 'NONE',  ( -0.000000000000000000, -1.000000000000000000, -0.000000000000000000 ) ) ;
#19668 = ORIENTED_EDGE ( 'NONE', *, *, #32181, .F. ) ;
#19669 = EDGE_CURVE ( 'NONE', #50834, #28566, #8761, .T. ) ;
#19670 = CARTESIAN_POINT ( 'NONE',  ( 163.2911130186310515, 63.63047778106599139, -12.04342320290372470 ) ) ;
#19671 = EDGE_LOOP ( 'NONE', ( #37736, #47416, #9650, #43541 ) ) ;
#19672 = ADVANCED_FACE ( 'NONE', ( #33959 ), #65625, .F. ) ;
#19673 = DIRECTION ( 'NONE',  ( 0.000000000000000000, 0.000000000000000000, 1.000000000000000000 ) ) ;
#19674 = CARTESIAN_POINT ( 'NONE',  ( 138.5902997793499196, 44.35633795166239679, 84.84391433248465830 ) ) ;
#19676 = ORIENTED_EDGE ( 'NONE', *, *, #53199, .F. ) ;
#19675 = CARTESIAN_POINT ( 'NONE',  ( 155.7265855639938650, 57.57443315515123317, 2.757056929193004713 ) ) ;
#19677 = CARTESIAN_POINT ( 'NONE',  ( -146.1142527948576912, 61.35394402951023096, -62.46500431941766607 ) ) ;
#19678 = DIRECTION ( 'NONE',  ( 0.000000000000000000, 0.000000000000000000, 1.000000000000000000 ) ) ;
#19679 = CARTESIAN_POINT ( 'NONE',  ( 161.7209903610255139, 61.03262545641850068, -37.42759312634723301 ) ) ;
#19680 = EDGE_LOOP ( 'NONE', ( #24228, #66088, #67002, #49137 ) ) ;
#19681 = CARTESIAN_POINT ( 'NONE',  ( -95.63694837622352907, 30.64472169584718841, 14.66480637497265604 ) ) ;
#19682 = EDGE_CURVE ( 'NONE', #5387, #2906, #18834, .T. ) ;
#19683 = ADVANCED_FACE ( 'NONE', ( #39580 ), #44851, .T. ) ;
#19684 = CARTESIAN_POINT ( 'NONE',  ( -131.1078488676298832, 50.02394948559179255, 43.51637233646730607 ) ) ;
#19685 = FACE_OUTER_BOUND ( 'NONE', #28952, .T. ) ;
#19686 = VECTOR ( 'NONE', #5164, 1000.000000000000000 ) ;
#19687 = CARTESIAN_POINT ( 'NONE',  ( 82.12277968641507186, 18.98848723477811262, -10.46207403576605621 ) ) ;
#19688 = CARTESIAN_POINT ( 'NONE',  ( -7.825402957745085430, 7.899365992529248537, -35.41807073194381417 ) ) ;
#19689 = CARTESIAN_POINT ( 'NONE',  ( 155.7277429502854034, 56.30804678861343859, 56.44591023570471577 ) ) ;
#19690 = CARTESIAN_POINT ( 'NONE',  ( 89.88147981065577596, 21.62466191578946351, 43.98752394672685284 ) ) ;
#19691 = ORIENTED_EDGE ( 'NONE', *, *, #41605, .T. ) ;
#19692 = DIRECTION ( 'NONE',  ( 0.000000000000000000, -1.000000000000000000, 0.000000000000000000 ) ) ;
#19693 = CARTESIAN_POINT ( 'NONE',  ( -13.79190010541702982, 8.363435739308561878, 69.03078841869681526 ) ) ;
#19694 = ORIENTED_EDGE ( 'NONE', *, *, #67031, .F. ) ;
#19695 = EDGE_CURVE ( 'NONE', #48132, #29084, #45619, .T. ) ;
#19696 = CARTESIAN_POINT ( 'NONE',  ( -51.66904755831212981, -15.55634918610397222, 85.00100000000000477 ) ) ;
#19697 = CARTESIAN_POINT ( 'NONE',  ( 212.0779786303466210, 118.9010947973413437, -18.35900109281879367 ) ) ;
#19698 = VECTOR ( 'NONE', #24671, 1000.000000000000000 ) ;
#19699 = CIRCLE ( 'NONE', #35423, 125.0000000000000000 ) ;
#19700 = CARTESIAN_POINT ( 'NONE',  ( 103.8055367708241334, 27.11070767929348690, 40.99165044060047336 ) ) ;
#19701 = LINE ( 'NONE', #25343, #38879 ) ;
#19702 = CARTESIAN_POINT ( 'NONE',  ( 62.38297021405776377, 12.52668572540603975, 83.52147531495063504 ) ) ;
#19703 =( GEOMETRIC_REPRESENTATION_CONTEXT ( 3 ) GLOBAL_UNCERTAINTY_ASSIGNED_CONTEXT ( ( #55717 ) ) GLOBAL_UNIT_ASSIGNED_CONTEXT ( ( #18093, #66306, #23020 ) ) REPRESENTATION_CONTEXT ( 'NONE', 'WORKASPACE' ) );
#19704 = CARTESIAN_POINT ( 'NONE',  ( 185.7267155939802024, 84.90388481853132419, 4.069038840943626667 ) ) ;
#19705 = CARTESIAN_POINT ( 'NONE',  ( 212.0180052085437694, 116.9552462415714871, -42.16221012700841442 ) ) ;
#19706 = AXIS2_PLACEMENT_3D ( 'NONE', #9658, #52889, #26173 ) ;
#19707 = CARTESIAN_POINT ( 'NONE',  ( 180.2572128312846758, 77.77323980479702925, 2.497912692282359792 ) ) ;
#19708 = CARTESIAN_POINT ( 'NONE',  ( -57.65733424639442717, 15.39521790791522982, 18.01019561178333817 ) ) ;
#19709 = EDGE_LOOP ( 'NONE', ( #23921, #58750, #12272, #239 ) ) ;
#19711 = AXIS2_PLACEMENT_3D ( 'NONE', #29387, #50498, #66356 ) ;
#19710 = CARTESIAN_POINT ( 'NONE',  ( 181.0840389613909736, -170.0000000000000000, -51.22505766587963905 ) ) ;
#19712 = ORIENTED_EDGE ( 'NONE', *, *, #32634, .T. ) ;
#19713 = CARTESIAN_POINT ( 'NONE',  ( 103.0103829243728768, 25.67737053862327556, -68.21726512339051851 ) ) ;
#19714 = EDGE_CURVE ( 'NONE', #9829, #9227, #6950, .T. ) ;
#19715 = LINE ( 'NONE', #8828, #55640 ) ;
#19716 = DIRECTION ( 'NONE',  ( -0.000000000000000000, -0.000000000000000000, 1.000000000000000000 ) ) ;
#19717 = DIRECTION ( 'NONE',  ( -0.000000000000000000, -0.000000000000000000, -1.000000000000000000 ) ) ;
#19718 = CARTESIAN_POINT ( 'NONE',  ( -0.4222246928121727860, 6.521921806359222806, 92.54939115416705420 ) ) ;
#19719 = EDGE_CURVE ( 'NONE', #7482, #29309, #12107, .T. ) ;
#19720 = EDGE_CURVE ( 'NONE', #10221, #7307, #21308, .T. ) ;
#19721 = CARTESIAN_POINT ( 'NONE',  ( -858.3301948030079984, -622.0000000000060254, 10.00000000000000000 ) ) ;
#19722 = EDGE_LOOP ( 'NONE', ( #51427, #5587, #31709, #28222 ) ) ;
#19723 = CARTESIAN_POINT ( 'NONE',  ( -71.96390573417176029, 19.88067451234326910, 68.16606071164316916 ) ) ;
#19724 = CARTESIAN_POINT ( 'NONE',  ( 290.0000000000000568, 5.000000000000000888, 18.50000000000000000 ) ) ;
#19725 = EDGE_LOOP ( 'NONE', ( #15694, #62988, #52, #41722 ) ) ;
#19726 = VERTEX_POINT ( 'NONE', #9990 ) ;
#19727 = CARTESIAN_POINT ( 'NONE',  ( -151.2497169612549328, 65.66843968092749151, 45.56996481252021880 ) ) ;
#19728 = CARTESIAN_POINT ( 'NONE',  ( 16.54503815046451010, -18.74197728628616844, 0.000000000000000000 ) ) ;
#19729 = CARTESIAN_POINT ( 'NONE',  ( 176.4367926094704728, 74.03315361639846515, -22.77209446790686442 ) ) ;
#19730 = CARTESIAN_POINT ( 'NONE',  ( -36.11269837220804391, 20.55634918610409301, 2.000000000000001776 ) ) ;
#19731 = ORIENTED_EDGE ( 'NONE', *, *, #3187, .F. ) ;
#19732 = LINE ( 'NONE', #9182, #57010 ) ;
#19733 = ORIENTED_EDGE ( 'NONE', *, *, #53481, .T. ) ;
#19734 = CARTESIAN_POINT ( 'NONE',  ( 22.15943197741200521, 7.796127622097904997, -46.98355238114885424 ) ) ;
#19735 = CARTESIAN_POINT ( 'NONE',  ( 8.540564391411908929, 7.383006541823029956, 62.41466723577283204 ) ) ;
#19736 = CARTESIAN_POINT ( 'NONE',  ( 212.1931396682532807, 117.2245435827729239, 37.02143851943622366 ) ) ;
#19737 = FACE_BOUND ( 'NONE', #19082, .T. ) ;
#19738 = PRODUCT ( 'hex nut gradec_iso_ISO - 4034 - M10 - N', 'hex nut gradec_iso_ISO - 4034 - M10 - N', '', ( #62832 ) ) ;
#19739 = CIRCLE ( 'NONE', #2873, 74.95140232871122521 ) ;
#19740 = ORIENTED_EDGE ( 'NONE', *, *, #54789, .F. ) ;
#19741 = EDGE_LOOP ( 'NONE', ( #48806, #52788, #63849, #39047 ) ) ;
#19742 = CARTESIAN_POINT ( 'NONE',  ( 114.3366190915103289, -21.85805078441902793, -2.510101233139118815 ) ) ;
#19743 = CARTESIAN_POINT ( 'NONE',  ( -119.0183326251804345, 43.31072671377873462, 88.79436413878467249 ) ) ;
#19744 = CIRCLE ( 'NONE', #52282, 5.000000000000000888 ) ;
#19745 = CARTESIAN_POINT ( 'NONE',  ( 34.82939798935585429, 8.870855050008909615, -63.99916360883118926 ) ) ;
#19746 = LINE ( 'NONE', #57045, #8515 ) ;
#19747 = CARTESIAN_POINT ( 'NONE',  ( 21.33146652848267522, 6.741339414847635325, 86.14122630416260051 ) ) ;
#19748 = CARTESIAN_POINT ( 'NONE',  ( 23.18757945110744600, 7.858491809880083778, 89.93510652474785161 ) ) ;
#19749 = CIRCLE ( 'NONE', #18648, 65.00000000000000000 ) ;
#19750 = AXIS2_PLACEMENT_3D ( 'NONE', #52855, #51508, #3309 ) ;
#19751 = ORIENTED_EDGE ( 'NONE', *, *, #54869, .F. ) ;
#19752 =( GEOMETRIC_REPRESENTATION_CONTEXT ( 3 ) GLOBAL_UNCERTAINTY_ASSIGNED_CONTEXT ( ( #30370 ) ) GLOBAL_UNIT_ASSIGNED_CONTEXT ( ( #20501, #26481, #429 ) ) REPRESENTATION_CONTEXT ( 'NONE', 'WORKASPACE' ) );
#19753 = CYLINDRICAL_SURFACE ( 'NONE', #7848, 65.36598343705435354 ) ;
#19754 = VECTOR ( 'NONE', #12690, 1000.000000000000000 ) ;
#19755 = CARTESIAN_POINT ( 'NONE',  ( 197.9843579228224542, 99.18296459057403069, -40.47005908839251731 ) ) ;
#19756 = ORIENTED_EDGE ( 'NONE', *, *, #33768, .F. ) ;
#19757 = CARTESIAN_POINT ( 'NONE',  ( -86.15441609607630369, 25.31657638323078530, 10.57859359723828518 ) ) ;
#19758 = ORIENTED_EDGE ( 'NONE', *, *, #32916, .F. ) ;
#19759 = EDGE_CURVE ( 'NONE', #32766, #23774, #21564, .T. ) ;
#19760 = VECTOR ( 'NONE', #11912, 999.9999999999998863 ) ;
#19761 = CARTESIAN_POINT ( 'NONE',  ( -57.89360549284268842, 16.50663738101751221, -8.918089600607720158 ) ) ;
#19762 =( REPRESENTATION_RELATIONSHIP ('NONE','NONE', #40274, #34334 ) REPRESENTATION_RELATIONSHIP_WITH_TRANSFORMATION ( #46871 )SHAPE_REPRESENTATION_RELATIONSHIP( ) );
#19763 = VERTEX_POINT ( 'NONE', #53908 ) ;
#19764 = ORIENTED_EDGE ( 'NONE', *, *, #11332, .T. ) ;
#19765 = CARTESIAN_POINT ( 'NONE',  ( 8.540853903193186270, 6.376814430361480213, -41.07341765948896750 ) ) ;
#19766 = LINE ( 'NONE', #56710, #40477 ) ;
#19767 = CARTESIAN_POINT ( 'NONE',  ( 17.48889770758266593, 6.561062909825351674, 3.361356057925529939 ) ) ;
#19768 = ORIENTED_EDGE ( 'NONE', *, *, #12162, .T. ) ;
#19769 = EDGE_CURVE ( 'NONE', #69223, #10029, #63315, .T. ) ;
#19770 = EDGE_CURVE ( 'NONE', #59267, #44813, #31110, .T. ) ;
#19771 = EDGE_CURVE ( 'NONE', #64884, #10495, #31444, .T. ) ;
#19772 = CARTESIAN_POINT ( 'NONE',  ( -23.94826066252556274, 8.481232536276079870, 91.89930965450892586 ) ) ;
#19773 = CARTESIAN_POINT ( 'NONE',  ( 173.8576514579035290, 72.97529922124006418, -68.54141255106546282 ) ) ;
#19774 = CARTESIAN_POINT ( 'NONE',  ( 0.000000000000000000, 0.000000000000000000, 85.00000000000000000 ) ) ;
#19775 = CARTESIAN_POINT ( 'NONE',  ( 104.3805245147141818, 26.26278144139195447, -48.12669505167198736 ) ) ;
#19776 = B_SPLINE_CURVE_WITH_KNOTS ( 'NONE', 3,
 ( #3922, #29965, #51425, #20099, #3569, #3236, #14808, #57734, #8861, #19748, #41210, #9545, #19398, #40860, #53119, #58405, #15850, #16194, #48523, #36970, #42911, #5633, #27090, #25732, #64376, #37294, #20780, #53466, #26069, #20430, #15165, #47497, #68958, #42243, #5298, #26756, #47163, #68625, #41895, #10911, #32035, #53808, #63355, #36627, #32382, #31347, #63705, #10567, #9894, #58077, #15516, #31685, #10219, #58745, #52776, #59095 ),
 .UNSPECIFIED., .F., .F.,
 ( 4, 2, 2, 2, 2, 2, 2, 2, 2, 2, 2, 2, 2, 2, 2, 2, 2, 2, 2, 2, 2, 2, 2, 2, 2, 2, 2, 4 ),
 ( 0.000000000000000000, 0.001960836769587751254, 0.002941255154381627098, 0.003921673539175502508, 0.004902091923969378352, 0.005882510308763254196, 0.006862928693557130040, 0.007843347078351005017, 0.009804183847938715071, 0.01078460223273256663, 0.01176502061752641645, 0.01274543900232026801, 0.01372585738711412130, 0.01470627577190797113, 0.01568669415670182268, 0.01764753092628952580, 0.01960836769587722545, 0.02058878608067108915, 0.02156920446546494591, 0.02254962285025880267, 0.02353004123505265943, 0.02451045961984651966, 0.02549087800464037643, 0.02745171477422813505, 0.02843213315902201610, 0.02941255154381589368, 0.03039296992860977473, 0.03137338831340365231 ),
 .UNSPECIFIED. ) ;
#19777 = ADVANCED_FACE ( 'NONE', ( #64134 ), #45107, .T. ) ;
#19778 = DIRECTION ( 'NONE',  ( 0.000000000000000000, 0.000000000000000000, 1.000000000000000000 ) ) ;
#19779 = CARTESIAN_POINT ( 'NONE',  ( 45.82394788922869822, -46.11928342727429708, 0.000000000000000000 ) ) ;
#19780 = ORIENTED_EDGE ( 'NONE', *, *, #12054, .F. ) ;
#19781 = VERTEX_POINT ( 'NONE', #5728 ) ;
#19782 = CARTESIAN_POINT ( 'NONE',  ( 41.35041461497708326, 8.670465437677201237, 17.82849842206101343 ) ) ;
#19783 = CARTESIAN_POINT ( 'NONE',  ( 174.1348882614952629, 73.23561817543360064, 12.79949674401064996 ) ) ;
#19784 = DIRECTION ( 'NONE',  ( 1.387778780781445922E-16, -1.000000000000000000, -1.232595164407830946E-32 ) ) ;
#19785 = LINE ( 'NONE', #41247, #17514 ) ;
#19786 = CARTESIAN_POINT ( 'NONE',  ( 126.5710838895481913, 37.19597237024180458, 8.365867632742146398 ) ) ;
#19787 = CARTESIAN_POINT ( 'NONE',  ( -155.7495771807047333, 69.65980221699318520, 7.188372552036696561 ) ) ;
#19788 = CARTESIAN_POINT ( 'NONE',  ( 8.000000000000007105, 249.8719672152120381, 94.99999999999866418 ) ) ;
#19789 = CARTESIAN_POINT ( 'NONE',  ( 211.8345664497467169, 118.5225165986914106, 34.37992018911904779 ) ) ;
#19790 = CARTESIAN_POINT ( 'NONE',  ( -85.95621526752231034, 26.32462117888286457, 62.98115503426731010 ) ) ;
#19791 = CARTESIAN_POINT ( 'NONE',  ( -107.7893514267588273, 35.66840175773127442, 32.90635557035678715 ) ) ;
#19792 = ORIENTED_EDGE ( 'NONE', *, *, #11548, .T. ) ;
#19793 = VECTOR ( 'NONE', #14164, 1000.000000000000227 ) ;
#19794 = CONTEXT_DEPENDENT_SHAPE_REPRESENTATION ( #5374, #39497 ) ;
#19795 = DIRECTION ( 'NONE',  ( 1.387778780781446169E-16, -1.000000000000000000, -3.469446951953615421E-17 ) ) ;
#19796 = EDGE_LOOP ( 'NONE', ( #18467, #45686, #4130, #58678 ) ) ;
#19797 = DIRECTION ( 'NONE',  ( -1.000000000000000000, 0.000000000000000000, 0.000000000000000000 ) ) ;
#19798 = ORIENTED_EDGE ( 'NONE', *, *, #25580, .T. ) ;
#19799 = DIRECTION ( 'NONE',  ( -0.000000000000000000, -0.000000000000000000, -1.000000000000000000 ) ) ;
#19800 = CIRCLE ( 'NONE', #46751, 60.00000000000000000 ) ;
#19801 = B_SPLINE_CURVE_WITH_KNOTS ( 'NONE', 3,
 ( #58591, #42083, #9739, #41743, #68146, #62860, #15007, #9392, #26259, #42761, #5140, #15358, #64224, #47347, #58258, #20977, #68805, #10409, #36817, #26598, #48035, #57583, #63887, #10076, #20621, #31535, #47690, #37488, #69154, #19952, #31879, #4116, #42428, #30851, #52634, #58939, #41406, #15697, #32226, #20284, #63204, #31201, #10759, #52296, #37147, #69495 ),
 .UNSPECIFIED., .F., .F.,
 ( 4, 2, 2, 2, 2, 2, 2, 2, 2, 2, 2, 2, 2, 2, 2, 2, 2, 2, 2, 2, 2, 2, 4 ),
 ( 0.000000000000000000, 0.003736383952885354628, 0.005604575929328017847, 0.007472767905770679765, 0.008406863893992011158, 0.009340959882213341683, 0.01120915185865600794, 0.01214324784687734714, 0.01307734383509868981, 0.01401143982332003247, 0.01494553581154137514, 0.01587963179976271955, 0.01681372778798406048, 0.01774782377620540141, 0.01868191976442674582, 0.01961601575264808675, 0.02055011174086943115, 0.02148420772909077209, 0.02241830371731211302, 0.02428649569375482264, 0.02615468767019753227, 0.02802287964664024536, 0.02989107162308295151 ),
 .UNSPECIFIED. ) ;
#19802 = DIRECTION ( 'NONE',  ( 0.000000000000000000, 1.000000000000000000, 0.000000000000000000 ) ) ;
#19803 = CARTESIAN_POINT ( 'NONE',  ( 10.55634918610396511, -46.66904755831214402, 0.000000000000000000 ) ) ;
#19804 = DIRECTION ( 'NONE',  ( 0.000000000000000000, 0.000000000000000000, -1.000000000000000000 ) ) ;
#19805 = EDGE_CURVE ( 'NONE', #39302, #145, #2027, .T. ) ;
#19806 = ADVANCED_FACE ( 'NONE', ( #43702 ), #33536, .F. ) ;
#19807 = VECTOR ( 'NONE', #55029, 1000.000000000000000 ) ;
#19808 = VECTOR ( 'NONE', #53209, 1000.000000000000000 ) ;
#19809 = CARTESIAN_POINT ( 'NONE',  ( 34.45500533947588195, 7.817363290423887001, -37.46142013688670858 ) ) ;
#19810 = CARTESIAN_POINT ( 'NONE',  ( 63.74253542338254164, 39.54050679744534591, 170.0000000000000000 ) ) ;
#19811 = CARTESIAN_POINT ( 'NONE',  ( 111.9975424824652634, 170.0000000000000284, 354.1673509436691347 ) ) ;
#19812 = AXIS2_PLACEMENT_3D ( 'NONE', #6587, #27681, #60035 ) ;
#19813 = ADVANCED_FACE ( 'NONE', ( #50398 ), #50045, .F. ) ;
#19814 = CARTESIAN_POINT ( 'NONE',  ( 130.7531879853686121, 39.58149302537893277, -36.67985178847166594 ) ) ;
#19815 = EDGE_LOOP ( 'NONE', ( #26290, #49775, #10519, #19869 ) ) ;
#19816 = ORIENTED_EDGE ( 'NONE', *, *, #43225, .F. ) ;
#19817 = AXIS2_PLACEMENT_3D ( 'NONE', #58441, #37333, #32071 ) ;
#19818 = LINE ( 'NONE', #40919, #64191 ) ;
#19819 = LINE ( 'NONE', #14195, #62223 ) ;
#19820 = CARTESIAN_POINT ( 'NONE',  ( -31.43908319763709969, 9.591432048623765638, -77.16174795566554678 ) ) ;
#19821 = UNCERTAINTY_MEASURE_WITH_UNIT (LENGTH_MEASURE( 1.000000000000000082E-05 ), #69363, 'distance_accuracy_value', 'NONE');
#19822 = CARTESIAN_POINT ( 'NONE',  ( 15.78827728214693416, 6.500811158483328356, 18.17015708224157322 ) ) ;
#19823 = CARTESIAN_POINT ( 'NONE',  ( 45.04506994399699948, 10.22854084020124077, -74.92927396681155017 ) ) ;
#19824 = FACE_OUTER_BOUND ( 'NONE', #19979, .T. ) ;
#19825 = CARTESIAN_POINT ( 'NONE',  ( 175.3815143714021758, 73.02838262207001208, -65.69146865943324087 ) ) ;
#19826 =( NAMED_UNIT ( * ) SI_UNIT ( $, .STERADIAN. ) SOLID_ANGLE_UNIT ( ) );
#19827 = CARTESIAN_POINT ( 'NONE',  ( -85.61911145880966956, 26.18322756479841473, -93.48309464426087345 ) ) ;
#19828 = CARTESIAN_POINT ( 'NONE',  ( 65.35403040894466642, -1.250000000000021982, 43.58025477438756212 ) ) ;
#19829 = CARTESIAN_POINT ( 'NONE',  ( -26.88234027341226096, 9.904106450608205492, 58.58403535530551665 ) ) ;
#19830 = CARTESIAN_POINT ( 'NONE',  ( 109.6684666882775474, 21.42428528562853529, 5.000000000000007105 ) ) ;
#19831 = CARTESIAN_POINT ( 'NONE',  ( 65.02478361689730946, 37.39438481344068776, 170.0000000000000000 ) ) ;
#19832 = VERTEX_POINT ( 'NONE', #1506 ) ;
#19833 = CARTESIAN_POINT ( 'NONE',  ( 16.78635691501517613, 6.000000000000000000, -41.68900338898716740 ) ) ;
#19834 = CARTESIAN_POINT ( 'NONE',  ( -129.6165111262478717, 48.99406349865700605, -75.77339883365759476 ) ) ;
#19835 = CARTESIAN_POINT ( 'NONE',  ( -0.2498518584877217619, -33.42485110444322771, 6.893342931471429402 ) ) ;
#19836 = CARTESIAN_POINT ( 'NONE',  ( -51.13073217147959326, 13.66490163179657458, -36.31884843616727210 ) ) ;
#19837 = DIRECTION ( 'NONE',  ( 1.000000000000000000, 0.000000000000000000, 0.000000000000000000 ) ) ;
#19838 = CARTESIAN_POINT ( 'NONE',  ( -452.6627218934914367, 399.9999999999998863, -146.4497041420118251 ) ) ;
#19839 = ORIENTED_EDGE ( 'NONE', *, *, #37934, .T. ) ;
#19840 = SURFACE_STYLE_USAGE ( .BOTH. , #68040 ) ;
#19841 = CARTESIAN_POINT ( 'NONE',  ( -5.690023276062404101, -5.952467836904166809, -0.1306530452038198453 ) ) ;
#19842 = VERTEX_POINT ( 'NONE', #16633 ) ;
#19843 = VECTOR ( 'NONE', #23519, 1000.000000000000000 ) ;
#19844 = VERTEX_POINT ( 'NONE', #38089 ) ;
#19845 = EDGE_CURVE ( 'NONE', #41022, #18531, #6781, .T. ) ;
#19846 = CARTESIAN_POINT ( 'NONE',  ( 444.9999999999999432, 225.0000000000000000, 0.000000000000000000 ) ) ;
#19847 = CARTESIAN_POINT ( 'NONE',  ( 309.8720357909272707, 18.00000000000002842, 256.6193948016162381 ) ) ;
#19848 = PLANE ( 'NONE',  #56098 ) ;
#19849 = ORIENTED_EDGE ( 'NONE', *, *, #62963, .T. ) ;
#19850 = PLANE ( 'NONE',  #63041 ) ;
#19851 = CONICAL_SURFACE ( 'NONE', #20944, 65.00000000000000000, 0.7853981633974497223 ) ;
#19852 = DIRECTION ( 'NONE',  ( -1.000000000000000000, 0.000000000000000000, 0.000000000000000000 ) ) ;
#19853 = CYLINDRICAL_SURFACE ( 'NONE', #47661, 7.500000000000020428 ) ;
#19854 = FACE_OUTER_BOUND ( 'NONE', #27189, .T. ) ;
#19855 = CARTESIAN_POINT ( 'NONE',  ( 50.03867889673311709, 42.05760816978183669, 43.58025477438756212 ) ) ;
#19856 = VECTOR ( 'NONE', #2285, 1000.000000000000114 ) ;
#19857 = CARTESIAN_POINT ( 'NONE',  ( -25.48750459758502984, 9.705678256319565378, -20.56274929115669181 ) ) ;
#19858 = CARTESIAN_POINT ( 'NONE',  ( -30.62628708973294422, -68.47330165179167238, 170.0000000000000000 ) ) ;
#19859 = ADVANCED_FACE ( 'NONE', ( #44903 ), #12203, .T. ) ;
#19860 = EDGE_CURVE ( 'NONE', #5706, #29569, #46478, .T. ) ;
#19861 = ORIENTED_EDGE ( 'NONE', *, *, #28252, .F. ) ;
#19862 = CARTESIAN_POINT ( 'NONE',  ( 107.9342863085848450, 28.93180871323605530, -23.72930682673416314 ) ) ;
#19863 = CARTESIAN_POINT ( 'NONE',  ( 8.951900209438536038, 6.378066731449595572, 61.26501831331611214 ) ) ;
#19864 = EDGE_CURVE ( 'NONE', #8603, #51213, #40686, .T. ) ;
#19865 = CARTESIAN_POINT ( 'NONE',  ( 198.4059165548112276, 99.71594270191988585, 40.79851715686629632 ) ) ;
#19866 = ADVANCED_FACE ( 'NONE', ( #51092 ), #50787, .T. ) ;
#19867 = CARTESIAN_POINT ( 'NONE',  ( -74.08105192128697070, 21.69630190401540304, 85.63813808529961591 ) ) ;
#19869 = ORIENTED_EDGE ( 'NONE', *, *, #62745, .T. ) ;
#19868 = CARTESIAN_POINT ( 'NONE',  ( -36.11269837220801548, 31.11269837220812207, 0.000000000000000000 ) ) ;
#19870 = CARTESIAN_POINT ( 'NONE',  ( 69.48877314113907744, 15.30784187978995092, 41.10903227078659938 ) ) ;
#19871 = ORIENTED_EDGE ( 'NONE', *, *, #26539, .F. ) ;
#19872 = EDGE_CURVE ( 'NONE', #6225, #39573, #57397, .T. ) ;
#19873 = ORIENTED_EDGE ( 'NONE', *, *, #33614, .T. ) ;
#19874 =( NAMED_UNIT ( * ) PLANE_ANGLE_UNIT ( ) SI_UNIT ( $, .RADIAN. ) );
#19875 = LINE ( 'NONE', #41331, #21064 ) ;
#19876 = CARTESIAN_POINT ( 'NONE',  ( 199.7255144154429161, 99.76581417577203581, -76.30443167248331804 ) ) ;
#19877 = DIRECTION ( 'NONE',  ( -0.000000000000000000, 1.000000000000000000, -0.000000000000000000 ) ) ;
#19878 = CARTESIAN_POINT ( 'NONE',  ( -119.5267374018686297, 42.44190186039714519, 68.96077536236255412 ) ) ;
#19879 = CARTESIAN_POINT ( 'NONE',  ( -84.23336401058614342, 25.60798568215575344, -10.72136487542798555 ) ) ;
#19880 = DIRECTION ( 'NONE',  ( 1.000000000000000000, 0.000000000000000000, 0.000000000000000000 ) ) ;
#19881 = CARTESIAN_POINT ( 'NONE',  ( -47.60266343315662141, 13.84328785304053078, 38.81655012327907173 ) ) ;
#19882 = EDGE_LOOP ( 'NONE', ( #42252, #31669, #65286, #8303 ) ) ;
#19883 = ORIENTED_EDGE ( 'NONE', *, *, #41977, .T. ) ;
#19884 = DIRECTION ( 'NONE',  ( -1.000000000000000000, 0.000000000000000000, 0.000000000000000000 ) ) ;
#19885 = B_SPLINE_CURVE_WITH_KNOTS ( 'NONE', 3,
 ( #50596, #24227, #18939, #29486, #2417, #50949, #45674, #56568, #8390, #29835, #51306, #3115, #67478, #62187, #14005, #8744, #30191, #3452, #62548, #41434, #42118, #36848, #15390, #3797, #62890, #47380, #31916, #20314, #51980, #68834, #68178, #53343, #20659, #52327, #9080, #4150, #63576, #57614, #5175, #58286, #46700, #30531, #10107, #69187 ),
 .UNSPECIFIED., .F., .F.,
 ( 4, 2, 2, 2, 2, 2, 2, 2, 2, 2, 2, 2, 2, 2, 2, 2, 2, 2, 2, 2, 2, 4 ),
 ( 0.02416815208377490198, 0.02567033257376879693, 0.02642142281876574961, 0.02717251306376269882, 0.02867469355375655907, 0.02942578379875347705, 0.03017687404375039156, 0.03167905453374424141, 0.03318123502373808431, 0.03393232526873501270, 0.03468341551373193415, 0.03618559600372577012, 0.03693668624872267076, 0.03768777649371957139, 0.03918995698371340736, 0.04069213747370724332, 0.04219431796370107929, 0.04369649845369491525, 0.04444758869869185058, 0.04519867894368877204, 0.04670085943368265657, 0.04820303992367653417 ),
 .UNSPECIFIED. ) ;
#19886 = CARTESIAN_POINT ( 'NONE',  ( 103.9652201950894721, 26.08439499369982073, 68.06684849509201740 ) ) ;
#19887 = CARTESIAN_POINT ( 'NONE',  ( 112.8036877771481699, 30.08463150275148124, 83.74363904605614550 ) ) ;
#19888 = CARTESIAN_POINT ( 'NONE',  ( 8.000000000000000000, 1.572549600175622952, -9.431055444744870897 ) ) ;
#19889 = CARTESIAN_POINT ( 'NONE',  ( 181.9295719569814480, 79.46350097013164770, -51.18950099341775228 ) ) ;
#19890 = DIRECTION ( 'NONE',  ( -0.000000000000000000, 1.000000000000000000, -0.000000000000000000 ) ) ;
#19891 = EDGE_CURVE ( 'NONE', #18664, #61225, #61564, .T. ) ;
#19892 = CARTESIAN_POINT ( 'NONE',  ( -145.9251124924754208, 62.49975471021623008, 85.31446015602850252 ) ) ;
#19893 = ORIENTED_EDGE ( 'NONE', *, *, #60815, .F. ) ;
#19894 = PRODUCT_DEFINITION_SHAPE ( 'NONE', 'NONE',  #69617 ) ;
#19895 = EDGE_LOOP ( 'NONE', ( #2732, #35229, #2689, #47813 ) ) ;
#19896 = ORIENTED_EDGE ( 'NONE', *, *, #20532, .T. ) ;
#19897 = CIRCLE ( 'NONE', #53556, 164.5210298272983778 ) ;
#19898 = LINE ( 'NONE', #41692, #46498 ) ;
#19899 = PLANE ( 'NONE',  #64484 ) ;
#19900 = CARTESIAN_POINT ( 'NONE',  ( 133.8566784816069344, 42.60093787723652525, -51.02331093239568816 ) ) ;
#19901 = CARTESIAN_POINT ( 'NONE',  ( 104.9997958498911288, -22.00004639774357429, -0.3283548106454132198 ) ) ;
#19902 = AXIS2_PLACEMENT_3D ( 'NONE', #56585, #45335, #62564 ) ;
#19903 = CARTESIAN_POINT ( 'NONE',  ( -55.53456145826332602, 15.85318253404850353, 30.31732777293112946 ) ) ;
#19904 = CARTESIAN_POINT ( 'NONE',  ( -36.38071096718372388, 11.47804921491336216, -63.99874941106702408 ) ) ;
#19905 = DIRECTION ( 'NONE',  ( 0.9009688679024155933, 0.4338837391175656699, -0.000000000000000000 ) ) ;
#19906 = VECTOR ( 'NONE', #12853, 1000.000000000000000 ) ;
#19907 = CARTESIAN_POINT ( 'NONE',  ( 183.9887307715836471, 83.05100282186907634, 70.57129800896366589 ) ) ;
#19908 = CARTESIAN_POINT ( 'NONE',  ( 9.416656162223555171, 6.380306691996769253, -12.21039664973801209 ) ) ;
#19909 = ORIENTED_EDGE ( 'NONE', *, *, #32481, .F. ) ;
#19910 = VECTOR ( 'NONE', #44818, 1000.000000000000114 ) ;
#19911 = CARTESIAN_POINT ( 'NONE',  ( -5.885876544836656343, 6.772369038004115716, -50.16710263326163499 ) ) ;
#19912 = CARTESIAN_POINT ( 'NONE',  ( 188.5843222076478867, 86.53342480589837749, 63.94975097486255322 ) ) ;
#19913 = CARTESIAN_POINT ( 'NONE',  ( 7.347286611336963702, 4.995646404165275278, -0.4969600502617484983 ) ) ;
#19914 = FACE_OUTER_BOUND ( 'NONE', #10754, .T. ) ;
#19915 = CARTESIAN_POINT ( 'NONE',  ( 127.1040286383415889, 37.49395136275129659, -19.95267234602065898 ) ) ;
#19916 = CARTESIAN_POINT ( 'NONE',  ( 22.15926701483431316, 7.796117250416240374, -12.20938565424666500 ) ) ;
#19917 = CARTESIAN_POINT ( 'NONE',  ( 13.84704553156522167, 7.452804552247568992, 3.421577053668306334 ) ) ;
#19918 = VECTOR ( 'NONE', #38108, 1000.000000000000114 ) ;
#19919 = EDGE_LOOP ( 'NONE', ( #40783, #67233 ) ) ;
#19920 = DIRECTION ( 'NONE',  ( 1.000000000000000000, 1.850550996349095901E-16, 1.228197773518735191E-20 ) ) ;
#19921 = PRODUCT_CONTEXT ( 'NONE', #68260, 'mechanical' ) ;
#19922 = CARTESIAN_POINT ( 'NONE',  ( 129.1310456962234809, 39.80382822048400726, -49.36754109056038686 ) ) ;
#19923 = DIRECTION ( 'NONE',  ( 0.000000000000000000, 0.5000000000000013323, 0.8660254037844379305 ) ) ;
#19924 = CARTESIAN_POINT ( 'NONE',  ( 442.3372781065085633, 400.0000000000000568, -116.4497041420118393 ) ) ;
#19925 = CONTEXT_DEPENDENT_SHAPE_REPRESENTATION ( #31469, #64667 ) ;
#19926 = CARTESIAN_POINT ( 'NONE',  ( 186.5979919519638486, 85.84756789133378163, -38.63534547958833798 ) ) ;
#19927 = ORIENTED_EDGE ( 'NONE', *, *, #48623, .T. ) ;
#19928 = ORIENTED_EDGE ( 'NONE', *, *, #69410, .T. ) ;
#19929 = EDGE_CURVE ( 'NONE', #5910, #58406, #17070, .T. ) ;
#19930 = CARTESIAN_POINT ( 'NONE',  ( -142.9730935922299295, 58.82921737386681826, -11.77770370840645420 ) ) ;
#19931 = EDGE_CURVE ( 'NONE', #36547, #6792, #47341, .T. ) ;
#19932 = DIRECTION ( 'NONE',  ( -0.000000000000000000, -0.000000000000000000, 1.000000000000000000 ) ) ;
#19933 = EDGE_LOOP ( 'NONE', ( #24188, #34340, #56345, #65370 ) ) ;
#19934 = EDGE_CURVE ( 'NONE', #58934, #26154, #60156, .T. ) ;
#19935 = CARTESIAN_POINT ( 'NONE',  ( 155.4893034622222672, 57.39280319106983796, 83.35853011262113910 ) ) ;
#19936 = ORIENTED_EDGE ( 'NONE', *, *, #9610, .F. ) ;
#19937 = CARTESIAN_POINT ( 'NONE',  ( -58.97243502469717669, 16.81420332340175960, 17.37168708933159422 ) ) ;
#19938 = DIRECTION ( 'NONE',  ( -0.000000000000000000, -0.000000000000000000, -1.000000000000000000 ) ) ;
#19939 = DIRECTION ( 'NONE',  ( -1.000000000000000000, -0.000000000000000000, -0.000000000000000000 ) ) ;
#19940 = DIRECTION ( 'NONE',  ( 0.000000000000000000, 0.000000000000000000, -1.000000000000000000 ) ) ;
#19941 = DIRECTION ( 'NONE',  ( 0.000000000000000000, 0.000000000000000000, 1.000000000000000000 ) ) ;
#19943 = ORIENTED_EDGE ( 'NONE', *, *, #63021, .T. ) ;
#19942 = DIRECTION ( 'NONE',  ( 1.000000000000000000, 0.000000000000000000, 0.000000000000000000 ) ) ;
#19944 = AXIS2_PLACEMENT_3D ( 'NONE', #66915, #18711, #2878 ) ;
#19945 = DIRECTION ( 'NONE',  ( 0.000000000000000000, 0.000000000000000000, -1.000000000000000000 ) ) ;
#19946 = ORIENTED_EDGE ( 'NONE', *, *, #21796, .T. ) ;
#19947 = EDGE_LOOP ( 'NONE', ( #47444, #64728, #55279, #37389 ) ) ;
#19948 =( BOUNDED_CURVE ( )  B_SPLINE_CURVE ( 3, ( #24917, #18242, #45678, #3120 ),
 .UNSPECIFIED., .F., .F. ) 
 B_SPLINE_CURVE_WITH_KNOTS ( ( 4, 4 ),
 ( 3.140184917367546882E-16, 1.570796326794896780 ),
 .UNSPECIFIED. ) 
 CURVE ( )  GEOMETRIC_REPRESENTATION_ITEM ( )  RATIONAL_B_SPLINE_CURVE ( ( 1.000000000000000000, 0.8047378541243649375, 0.8047378541243649375, 1.000000000000000000 ) ) 
 REPRESENTATION_ITEM ( '' )  );
#19949 = AXIS2_PLACEMENT_3D ( 'NONE', #38572, #61077, #11839 ) ;
#19950 = CARTESIAN_POINT ( 'NONE',  ( -168.1811549361197820, 83.25427431521137578, 5.828879898275340921 ) ) ;
#19951 = EDGE_CURVE ( 'NONE', #39418, #33970, #22880, .T. ) ;
#19952 = CARTESIAN_POINT ( 'NONE',  ( -179.6470915626256897, 94.69856161161345653, -19.07391450275219924 ) ) ;
#19953 = AXIS2_PLACEMENT_3D ( 'NONE', #54843, #54134, #28829 ) ;
#19954 = EDGE_CURVE ( 'NONE', #14760, #48854, #17957, .T. ) ;
#19956 = ORIENTED_EDGE ( 'NONE', *, *, #50653, .T. ) ;
#19955 = CARTESIAN_POINT ( 'NONE',  ( -130.5811943660945360, 50.88295841537573949, 59.08986182251942409 ) ) ;
#19957 = CARTESIAN_POINT ( 'NONE',  ( -109.0191069781766657, 37.48620563201052391, 94.99999999999866418 ) ) ;
#19958 = FACE_BOUND ( 'NONE', #6502, .T. ) ;
#19959 = PRESENTATION_LAYER_ASSIGNMENT (  '', '', ( #44660 ) ) ;
#19960 = EDGE_LOOP ( 'NONE', ( #16873, #20474, #9121, #42355 ) ) ;
#19961 = VECTOR ( 'NONE', #55580, 1000.000000000000000 ) ;
#19962 = CARTESIAN_POINT ( 'NONE',  ( -62.49130718206700408, 16.80297926264071506, -16.86221752726308409 ) ) ;
#19963 = AXIS2_PLACEMENT_3D ( 'NONE', #41073, #49612, #17621 ) ;
#19964 = CARTESIAN_POINT ( 'NONE',  ( -130.5811943660945076, 50.88295841537573239, -75.13289112979900608 ) ) ;
#19965 = CARTESIAN_POINT ( 'NONE',  ( 117.6924004117966263, 33.61107268965020722, 36.09735895212963186 ) ) ;
#19966 = CARTESIAN_POINT ( 'NONE',  ( -31.86613124579579903, 10.09122387767404838, 6.893343212288924882 ) ) ;
#19967 = CARTESIAN_POINT ( 'NONE',  ( 70.51522979775974420, 15.57935281015687323, -69.56303398768666568 ) ) ;
#19968 = VERTEX_POINT ( 'NONE', #27101 ) ;
#19969 = ORIENTED_EDGE ( 'NONE', *, *, #53551, .T. ) ;
#19970 = CARTESIAN_POINT ( 'NONE',  ( -142.3260422482981085, 59.60034523324941347, -13.23360016362279090 ) ) ;
#19971 = CARTESIAN_POINT ( 'NONE',  ( -167.1534554062404254, 80.72263015867909530, -37.66204370233266729 ) ) ;
#19972 = FACE_OUTER_BOUND ( 'NONE', #21357, .T. ) ;
#19973 = CARTESIAN_POINT ( 'NONE',  ( -47.76873007799818538, 12.84869220385979460, -94.56435065590063971 ) ) ;
#19974 = CARTESIAN_POINT ( 'NONE',  ( 100.0000000000000284, -5.000000000000000000, 18.50000000000000000 ) ) ;
#19975 = DIRECTION ( 'NONE',  ( -0.000000000000000000, -0.000000000000000000, 1.000000000000000000 ) ) ;
#19976 = CARTESIAN_POINT ( 'NONE',  ( 63.01563776193091826, 12.67277567978500130, -35.72069083216973695 ) ) ;
#19977 = CARTESIAN_POINT ( 'NONE',  ( 112.3013380801408658, 400.0000000000066507, -123.9497041420121235 ) ) ;
#19978 = CARTESIAN_POINT ( 'NONE',  ( -172.3057147739577317, 86.22480007276995195, -76.52359078706952289 ) ) ;
#19979 = EDGE_LOOP ( 'NONE', ( #49154, #40536, #24862, #22436, #52944 ) ) ;
#19980 = CARTESIAN_POINT ( 'NONE',  ( -104.7956873821848660, 35.21322275870666374, 30.94966216072465670 ) ) ;
#19981 = VERTEX_POINT ( 'NONE', #5643 ) ;
#19982 = CARTESIAN_POINT ( 'NONE',  ( 79.98183030723785691, 18.31194381986301778, -93.43937185863195793 ) ) ;
#19983 = LINE ( 'NONE', #36155, #58793 ) ;
#19984 = ORIENTED_EDGE ( 'NONE', *, *, #6077, .T. ) ;
#19985 = CYLINDRICAL_SURFACE ( 'NONE', #36329, 4.250000000000000000 ) ;
#19986 = CARTESIAN_POINT ( 'NONE',  ( 46.39999999999999858, 5.616230220889761452E-16, -4.171999999999999709 ) ) ;
#19987 = CARTESIAN_POINT ( 'NONE',  ( 36.77024545412685796, 9.095083943590521969, 3.541950953158858884 ) ) ;
#19988 = CARTESIAN_POINT ( 'NONE',  ( 38.91493890549795509, 8.346224043800605230, 3.069283715499573351 ) ) ;
#19989 = DIRECTION ( 'NONE',  ( 1.000000000000000000, -0.000000000000000000, 0.000000000000000000 ) ) ;
#19990 = CARTESIAN_POINT ( 'NONE',  ( -34.74023699876257609, 11.17830703027882855, -22.72455885904352257 ) ) ;
#19991 = ORIENTED_EDGE ( 'NONE', *, *, #64631, .F. ) ;
#19992 = VECTOR ( 'NONE', #61456, 1000.000000000000000 ) ;
#19993 = PLANE ( 'NONE',  #10649 ) ;
#19994 = ORIENTED_EDGE ( 'NONE', *, *, #67890, .T. ) ;
#19995 = DIRECTION ( 'NONE',  ( 1.000000000000000000, 1.850550996349095901E-16, 1.228197773518735191E-20 ) ) ;
#19996 = CARTESIAN_POINT ( 'NONE',  ( 8.767814708128309320, 7.383611927972575373, -72.51365984521781627 ) ) ;
#19997 = CARTESIAN_POINT ( 'NONE',  ( -189.5325095384513645, 107.4952257375067433, 13.70762090391955823 ) ) ;
#19998 = DIRECTION ( 'NONE',  ( 0.000000000000000000, 0.000000000000000000, -1.000000000000000000 ) ) ;
#19999 = DIRECTION ( 'NONE',  ( -0.000000000000000000, -0.000000000000000000, -1.000000000000000000 ) ) ;
#20000 = CARTESIAN_POINT ( 'NONE',  ( -98.67723517640901321, 30.98797878696540309, -9.087774546891575156 ) ) ;
#20001 = VECTOR ( 'NONE', #58729, 1000.000000000000000 ) ;
#20002 = CARTESIAN_POINT ( 'NONE',  ( 157.2533363798600021, 58.75760182111577024, -51.12418429913766005 ) ) ;
#20003 = AXIS2_PLACEMENT_3D ( 'NONE', #14300, #50884, #45258 ) ;
#20004 = ORIENTED_EDGE ( 'NONE', *, *, #28054, .F. ) ;
#20005 = DIRECTION ( 'NONE',  ( 0.6000000000000030864, 2.886579864025407005E-15, 0.7999999999999978240 ) ) ;
#20006 = CYLINDRICAL_SURFACE ( 'NONE', #61035, 7.500000000000013323 ) ;
#20007 = DIRECTION ( 'NONE',  ( 0.000000000000000000, -0.000000000000000000, 1.000000000000000000 ) ) ;
#20008 = CARTESIAN_POINT ( 'NONE',  ( -122.3745688183166322, 44.21964839958061333, 44.75990178122122387 ) ) ;
#20009 = CARTESIAN_POINT ( 'NONE',  ( 125.0000000000000000, 0.000000000000000000, 5.000000000000000000 ) ) ;
#20010 = ORIENTED_EDGE ( 'NONE', *, *, #69155, .F. ) ;
#20011 = CARTESIAN_POINT ( 'NONE',  ( -177.1514380519392944, 93.28180884530864603, -62.71624474115134262 ) ) ;
#20012 = CARTESIAN_POINT ( 'NONE',  ( 127.7121523762017858, 38.99241938113798511, 94.99999999999866418 ) ) ;
#20013 = CARTESIAN_POINT ( 'NONE',  ( 203.3979956051160229, 106.2714448901421633, -90.12122811341167505 ) ) ;
#20014 = ADVANCED_FACE ( 'NONE', ( #17603 ), #48533, .T. ) ;
#20015 = DIRECTION ( 'NONE',  ( 0.000000000000000000, 0.000000000000000000, 1.000000000000000000 ) ) ;
#20016 = CIRCLE ( 'NONE', #68314, 65.36598343705435354 ) ;
#20017 = ADVANCED_FACE ( 'NONE', ( #369 ), #5987, .T. ) ;
#20018 = CARTESIAN_POINT ( 'NONE',  ( -123.6619986853277737, 45.04188181212062858, -62.09435052478287531 ) ) ;
#20019 = ORIENTED_EDGE ( 'NONE', *, *, #14255, .F. ) ;
#20020 = CARTESIAN_POINT ( 'NONE',  ( 197.3707490726350215, 96.80690576410106019, 38.34013995466353464 ) ) ;
#20021 = CARTESIAN_POINT ( 'NONE',  ( 116.0773578185793582, 31.67580513411752463, -75.00610128316866110 ) ) ;
#20022 = CARTESIAN_POINT ( 'NONE',  ( 184.3879440808140089, 83.47316703125159165, 43.54523204561664329 ) ) ;
#20024 = CARTESIAN_POINT ( 'NONE',  ( 139.6150621148398727, 46.20856238844174158, 14.99708312333219595 ) ) ;
#20023 = B_SPLINE_CURVE_WITH_KNOTS ( 'NONE', 3,
 ( #21816, #16886, #22174, #27438, #48527, #15855, #32730, #48876, #53815, #21472, #54157, #21147, #48191, #10572, #37649, #38347, #361, #37300, #65086, #5980, #27795, #49584, #43615, #53473, #59789, #11605, #33080, #54508, #5304, #42916, #49234, #11968, #43259, #22519, #38706, #58752, #16547, #1069, #32391, #32039, #5638, #17232, #43961, #65438 ),
 .UNSPECIFIED., .F., .F.,
 ( 4, 2, 2, 2, 2, 2, 2, 2, 2, 2, 2, 2, 2, 2, 2, 2, 2, 2, 2, 2, 2, 4 ),
 ( 0.02432640572110343971, 0.02583721026359365666, 0.02659261253483874779, 0.02734801480608383545, 0.02885881934857404546, 0.02961422161981916434, 0.03036962389106428670, 0.03188042843355452099, 0.03339123297604475182, 0.03414663524728984989, 0.03490203751853494796, 0.03641284206102511634, 0.03716824433227021440, 0.03792364660351530553, 0.03943445114600549473, 0.04094525568849567698, 0.04245606023098587312, 0.04396686477347605537, 0.04472226704472114650, 0.04547766931596623763, 0.04698847385845637131, 0.04849927840094650500 ),
 .UNSPECIFIED. ) ;
#20025 = ADVANCED_FACE ( 'NONE', ( #730 ), #43269, .F. ) ;
#20026 = DIRECTION ( 'NONE',  ( 1.000000000000000000, 0.000000000000000000, -0.000000000000000000 ) ) ;
#20027 = VERTEX_POINT ( 'NONE', #33786 ) ;
#20028 = DIRECTION ( 'NONE',  ( -0.000000000000000000, 1.000000000000000000, -0.000000000000000000 ) ) ;
#20029 = ORIENTED_EDGE ( 'NONE', *, *, #50041, .F. ) ;
#20030 = CARTESIAN_POINT ( 'NONE',  ( 68.63585058221465829, 15.08566240483131793, 59.16672110021340103 ) ) ;
#20031 = CARTESIAN_POINT ( 'NONE',  ( 128.9313739248989918, 38.52897977562246723, 85.03336623935274474 ) ) ;
#20032 = ADVANCED_FACE ( 'NONE', ( #17241 ), #38712, .F. ) ;
#20034 = ORIENTED_EDGE ( 'NONE', *, *, #57181, .F. ) ;
#20033 = FACE_BOUND ( 'NONE', #58971, .T. ) ;
#20035 = CARTESIAN_POINT ( 'NONE',  ( 0.000000000000000000, 0.000000000000000000, 0.000000000000000000 ) ) ;
#20036 = FACE_OUTER_BOUND ( 'NONE', #18446, .T. ) ;
#20037 = CARTESIAN_POINT ( 'NONE',  ( 117.4806398654733783, 33.50379325299404343, -45.45665458773512313 ) ) ;
#20038 = ORIENTED_EDGE ( 'NONE', *, *, #4822, .F. ) ;
#20039 = FACE_OUTER_BOUND ( 'NONE', #29408, .T. ) ;
#20040 = AXIS2_PLACEMENT_3D ( 'NONE', #43514, #16099, #58653 ) ;
#20041 = LINE ( 'NONE', #14753, #15221 ) ;
#20042 = ORIENTED_EDGE ( 'NONE', *, *, #11660, .T. ) ;
#20043 = CARTESIAN_POINT ( 'NONE',  ( 79.39764314491564789, 18.13166883367086157, -18.48108370271943102 ) ) ;
#20044 = CARTESIAN_POINT ( 'NONE',  ( -165.9992860119575084, 79.53569239468049545, 35.95263399248825209 ) ) ;
#20045 = CARTESIAN_POINT ( 'NONE',  ( 157.0336341255056425, 57.31169401067823088, 56.25401806271707272 ) ) ;
#20046 = CARTESIAN_POINT ( 'NONE',  ( 0.000000000000000000, 0.000000000000000000, 40.00000000000003553 ) ) ;
#20047 = ORIENTED_EDGE ( 'NONE', *, *, #8483, .T. ) ;
#20048 = VECTOR ( 'NONE', #17933, 1000.000000000000000 ) ;
#20049 = DIRECTION ( 'NONE',  ( 1.000000000000000000, 0.000000000000000000, 0.000000000000000000 ) ) ;
#20050 = EDGE_LOOP ( 'NONE', ( #58875, #59954, #34918, #17402 ) ) ;
#20051 = CARTESIAN_POINT ( 'NONE',  ( 153.8224167330182297, 56.12711234192239829, -10.22241626634837353 ) ) ;
#20052 = CARTESIAN_POINT ( 'NONE',  ( 205.5049354810107900, 109.1776577097391225, -24.48138044215792775 ) ) ;
#20053 = CARTESIAN_POINT ( 'NONE',  ( 103.1534365798308386, 26.83148826706846179, 39.61125415960676577 ) ) ;
#20054 = CARTESIAN_POINT ( 'NONE',  ( 30.12852347772543737, 100.0000000000000000, 133.5802547743875550 ) ) ;
#20055 = CARTESIAN_POINT ( 'NONE',  ( 56.31946197080010563, 11.21858957927811495, 87.60745826581978690 ) ) ;
#20056 = B_SPLINE_CURVE_WITH_KNOTS ( 'NONE', 3,
 ( #46635, #46982, #30462, #3721, #25201, #68109, #48329, #42731, #53275, #27592, #64539, #59942, #163, #42394, #53956, #15999, #54308, #59586, #58903, #870, #5785, #11065, #519, #20938, #17028, #10718, #64187, #26219, #21621, #22322, #32192, #53624, #5449, #63856, #11762, #37448, #43067, #69112, #32876, #48000, #15665, #58555, #43762, #21282, #10372 ),
 .UNSPECIFIED., .F., .F.,
 ( 4, 2, 2, 1, 2, 2, 2, 2, 2, 2, 2, 2, 2, 2, 2, 2, 2, 2, 2, 2, 2, 2, 4 ),
 ( 0.02345095402629352246, 0.02491692321306682514, 0.02564990780645347995, 0.02638289239984013129, 0.02711587699322678263, 0.02784886158661343744, 0.02931483077338673318, 0.03004781536677338799, 0.03078079996016004280, 0.03224676914693334895, 0.03297975374032000723, 0.03371273833370666551, 0.03517870752047992655, 0.03664467670725320148, 0.03737766130063985281, 0.03811064589402650415, 0.03957661508079982071, 0.04104258426757313033, 0.04250855345434643995, 0.04324153804773310517, 0.04397452264111975651, 0.04544049182789308000, 0.04690646101466640350 ),
 .UNSPECIFIED. ) ;
#20057 = CARTESIAN_POINT ( 'NONE',  ( 181.5079096844946491, 80.47139261082470796, 2.464043515047716681 ) ) ;
#20058 = CARTESIAN_POINT ( 'NONE',  ( 212.1983751099433846, 117.2326047784726910, -43.68460009809672329 ) ) ;
#20059 = CARTESIAN_POINT ( 'NONE',  ( 173.9288990958750105, 71.66475105971929338, 12.28611953004625335 ) ) ;
#20060 = ORIENTED_EDGE ( 'NONE', *, *, #25029, .F. ) ;
#20061 = DIRECTION ( 'NONE',  ( -0.000000000000000000, -0.000000000000000000, -1.000000000000000000 ) ) ;
#20062 = ORIENTED_EDGE ( 'NONE', *, *, #128, .T. ) ;
#20063 = CARTESIAN_POINT ( 'NONE',  ( -72.77296415263759854, 21.23032531836537018, 60.09768903209150182 ) ) ;
#20064 = CARTESIAN_POINT ( 'NONE',  ( 55.90910788310615231, 11.13585330978401089, -67.61777098659958085 ) ) ;
#20065 = CARTESIAN_POINT ( 'NONE',  ( -77.02372450489323796, 21.70271995013166233, 3.751895169942434993 ) ) ;
#20066 = CARTESIAN_POINT ( 'NONE',  ( 35.39413431650373099, 0.000000000000000000, 5.000000000000000000 ) ) ;
#20067 = CARTESIAN_POINT ( 'NONE',  ( -7.181048525087159184, 6.849049514988890586, 83.80408853790447665 ) ) ;
#20068 = CARTESIAN_POINT ( 'NONE',  ( -106.7004823116342180, 36.22460663120047286, -9.592053525173668049 ) ) ;
#20069 = B_SPLINE_CURVE_WITH_KNOTS ( 'NONE', 3,
 ( #60659, #35318, #2969, #18448, #29345, #33939, #24080, #18792, #1939, #61357, #7561, #45173, #29019, #44833, #50459, #13180, #51158, #30046, #40251, #51506, #67003, #24431, #61697, #23396, #46203, #39902, #66314, #28658, #34647, #34976, #56083, #2280, #12834, #56420, #7898, #50799 ),
 .UNSPECIFIED., .F., .F.,
 ( 4, 2, 2, 2, 2, 2, 2, 2, 2, 2, 2, 2, 2, 2, 2, 2, 2, 4 ),
 ( 0.000000000000000000, 0.0009802228717936478999, 0.001960445743587295800, 0.002940668615380943266, 0.003920891487174591600, 0.004901114358968239500, 0.005881337230761886532, 0.006371448666658678824, 0.006861560102555471982, 0.007841782974349056565, 0.008822005846142642882, 0.009802228717936227465, 0.01078245158972981205, 0.01176267446152339316, 0.01274289733331697774, 0.01372312020511056059, 0.01470334307690414517, 0.01568356594869772802 ),
 .UNSPECIFIED. ) ;
#20070 = ORIENTED_EDGE ( 'NONE', *, *, #62583, .F. ) ;
#20071 = EDGE_CURVE ( 'NONE', #24241, #34219, #13730, .T. ) ;
#20072 = CARTESIAN_POINT ( 'NONE',  ( -74.17694007417657076, 20.66176641130875424, 70.79032727487506804 ) ) ;
#20073 = CARTESIAN_POINT ( 'NONE',  ( 197.8053004231843772, 97.34590015073870006, -94.51308478323058182 ) ) ;
#20074 = ORIENTED_EDGE ( 'NONE', *, *, #41613, .F. ) ;
#20075 = VERTEX_POINT ( 'NONE', #22527 ) ;
#20076 = DIRECTION ( 'NONE',  ( 0.000000000000000000, 0.000000000000000000, -1.000000000000000000 ) ) ;
#20077 = CARTESIAN_POINT ( 'NONE',  ( 58.47673920847984874, 11.66523265296355305, -49.21114976423752552 ) ) ;
#20078 = CARTESIAN_POINT ( 'NONE',  ( 48.11816970607238630, 43.69944786994017960, 170.0000000000000000 ) ) ;
#20079 = DIRECTION ( 'NONE',  ( 0.7818314824680221431, 0.6234898018587432533, 2.500042656554810340E-16 ) ) ;
#20080 = CARTESIAN_POINT ( 'NONE',  ( 264.4165763529819628, 225.8585178651493948, 138.9999999999999716 ) ) ;
#20081 = ORIENTED_EDGE ( 'NONE', *, *, #29172, .F. ) ;
#20082 = CARTESIAN_POINT ( 'NONE',  ( -38.04732747637867618, 4.679373924310576527, 13.32819397642332326 ) ) ;
#20083 = ORIENTED_EDGE ( 'NONE', *, *, #39070, .T. ) ;
#20084 = CARTESIAN_POINT ( 'NONE',  ( 211.7451286015360949, 116.5372661580811524, 12.44640788307098767 ) ) ;
#20085 = DIRECTION ( 'NONE',  ( -0.000000000000000000, 1.000000000000000000, -0.000000000000000000 ) ) ;
#20086 = CARTESIAN_POINT ( 'NONE',  ( 209.6877167158270652, 113.4449353909247407, 42.31176391386135549 ) ) ;
#20087 = CARTESIAN_POINT ( 'NONE',  ( 15.78827728214693416, 6.500811158483322139, -89.20804527961313113 ) ) ;
#20088 = EDGE_CURVE ( 'NONE', #65524, #62136, #28144, .T. ) ;
#20089 = EDGE_CURVE ( 'NONE', #47734, #38085, #48663, .T. ) ;
#20090 = ORIENTED_EDGE ( 'NONE', *, *, #61247, .T. ) ;
#20091 = CIRCLE ( 'NONE', #32441, 25.12245591505646303 ) ;
#20092 = ORIENTED_EDGE ( 'NONE', *, *, #43084, .F. ) ;
#20093 = CARTESIAN_POINT ( 'NONE',  ( 114.9673805781175133, -21.99252023018708968, 0.6578219585121953816 ) ) ;
#20094 = CARTESIAN_POINT ( 'NONE',  ( -118.4463605755664446, 42.96013650986014909, 92.75845490717212272 ) ) ;
#20095 = CARTESIAN_POINT ( 'NONE',  ( -165.7699288023689803, 79.30174988963861438, -16.88298621586212889 ) ) ;
#20096 = LINE ( 'NONE', #67950, #2887 ) ;
#20097 = EDGE_CURVE ( 'NONE', #57426, #56594, #67673, .T. ) ;
#20098 = CARTESIAN_POINT ( 'NONE',  ( 22.82910978135140212, 6.828162702325536237, 93.80883881146230863 ) ) ;
#20099 = CARTESIAN_POINT ( 'NONE',  ( 23.10675661028717087, 7.853421165986156360, 92.87640639569337964 ) ) ;
#20100 = MECHANICAL_DESIGN_GEOMETRIC_PRESENTATION_REPRESENTATION (  '', ( #40332 ), #38058 ) ;
#20101 = ORIENTED_EDGE ( 'NONE', *, *, #18594, .T. ) ;
#20102 = CARTESIAN_POINT ( 'NONE',  ( 73.43826238111391547, 0.000000000000000000, 26.24939009510892518 ) ) ;
#20103 = CARTESIAN_POINT ( 'NONE',  ( -96.00016893459647349, 29.70347032303887858, 68.97150621174834839 ) ) ;
#20104 = ORIENTED_EDGE ( 'NONE', *, *, #56299, .T. ) ;
#20105 = CARTESIAN_POINT ( 'NONE',  ( -86.15275984831841072, 25.31588180512565600, 11.59364235127147680 ) ) ;
#20106 = ORIENTED_EDGE ( 'NONE', *, *, #60738, .F. ) ;
#20107 = CARTESIAN_POINT ( 'NONE',  ( -56.73868929054667376, 16.18382781951278915, -8.559674830497424836 ) ) ;
#20109 = ORIENTED_EDGE ( 'NONE', *, *, #59984, .T. ) ;
#20108 = EDGE_CURVE ( 'NONE', #24269, #27416, #22180, .T. ) ;
#20110 = ORIENTED_EDGE ( 'NONE', *, *, #35090, .T. ) ;
#20111 = CARTESIAN_POINT ( 'NONE',  ( 69.68177367721139603, 20.52767805628179332, 170.0000000000000000 ) ) ;
#20112 = ADVANCED_FACE ( 'NONE', ( #11613 ), #55225, .T. ) ;
#20114 = EDGE_CURVE ( 'NONE', #16433, #47695, #64748, .T. ) ;
#20113 = CARTESIAN_POINT ( 'NONE',  ( -108.9643850519886001, 37.45603458068514158, -92.79426669927697446 ) ) ;
#20115 = CARTESIAN_POINT ( 'NONE',  ( 22.30016284075436417, 6.796348835713779124, 14.42317800662865146 ) ) ;
#20116 = EDGE_LOOP ( 'NONE', ( #47534, #5599, #14221, #65561 ) ) ;
#20117 = CARTESIAN_POINT ( 'NONE',  ( -38.04017048906806053, 10.76841555971077469, 87.83049671292886273 ) ) ;
#20118 = CARTESIAN_POINT ( 'NONE',  ( 174.9099402067542997, 73.96774984027643995, -66.30337972617925857 ) ) ;
#20119 = DIRECTION ( 'NONE',  ( -1.000000000000000000, 0.000000000000000000, 0.000000000000000000 ) ) ;
#20120 = CARTESIAN_POINT ( 'NONE',  ( 109.3047266816501235, 28.44977739115299897, -50.87832046748908965 ) ) ;
#20121 = CARTESIAN_POINT ( 'NONE',  ( 85.68197636629479064, 20.16141071296263831, -50.77689019393022818 ) ) ;
#20122 = CARTESIAN_POINT ( 'NONE',  ( -54.03875030502680943, 7.289021226777605002E-15, 2.000000000000001776 ) ) ;
#20123 = EDGE_LOOP ( 'NONE', ( #60111, #9552, #12672, #68997, #58996, #47267, #65608, #9635, #8455 ) ) ;
#20124 = DIRECTION ( 'NONE',  ( -0.000000000000000000, -0.000000000000000000, -1.000000000000000000 ) ) ;
#20125 = CARTESIAN_POINT ( 'NONE',  ( -83.13046924527391468, 25.15778674529014936, -75.49169951200217099 ) ) ;
#20126 = CARTESIAN_POINT ( 'NONE',  ( 174.4978817191264966, 73.57770570413210010, 6.365850984605415874 ) ) ;
#20127 = DIRECTION ( 'NONE',  ( 0.000000000000000000, 1.000000000000000000, 0.000000000000000000 ) ) ;
#20128 = CARTESIAN_POINT ( 'NONE',  ( 15.78827728214693416, 6.500811158483327468, -35.51894409868578606 ) ) ;
#20129 = DIRECTION ( 'NONE',  ( -1.000000000000000000, 0.000000000000000000, 1.387778780781445182E-16 ) ) ;
#20130 = CARTESIAN_POINT ( 'NONE',  ( -154.6171773099879374, 68.63761944777704116, 16.87154224365831467 ) ) ;
#20131 = CARTESIAN_POINT ( 'NONE',  ( -118.6727642982647239, 43.09863379477472733, -71.35525363643188257 ) ) ;
#20132 = CARTESIAN_POINT ( 'NONE',  ( 204.6977192012829789, 108.0580384837235073, 44.20772073876944575 ) ) ;
#20133 = CARTESIAN_POINT ( 'NONE',  ( -80.31482177285907653, 24.03632224640839254, 57.44225315143493305 ) ) ;
#20134 = FACE_OUTER_BOUND ( 'NONE', #34376, .T. ) ;
#20135 = ORIENTED_EDGE ( 'NONE', *, *, #36037, .T. ) ;
#20136 = CARTESIAN_POINT ( 'NONE',  ( -53.51212025488904800, 15.31378391224928315, 84.15964359628104319 ) ) ;
#20137 = ORIENTED_EDGE ( 'NONE', *, *, #2103, .T. ) ;
#20138 = DIRECTION ( 'NONE',  ( 1.000000000000000000, 0.000000000000000000, 0.000000000000000000 ) ) ;
#20139 = EDGE_LOOP ( 'NONE', ( #48631, #29658, #17355, #59448 ) ) ;
#20140 = CIRCLE ( 'NONE', #36963, 65.36598343705435354 ) ;
#20141 = B_SPLINE_CURVE_WITH_KNOTS ( 'NONE', 3,
 ( #9630, #31088, #52528, #4351, #41973, #54942, #23306, #11333, #32803, #65517, #38424, #59172, #50021, #32456, #28210, #21890, #43685, #10992, #27513, #1855, #59514, #18018, #54233, #17312, #38783, #48602, #439, #16615, #60230, #44392, #22248, #60575, #59868, #38072, #49657, #44033, #54593, #11684, #7113, #12043, #27165, #6054, #43342, #65161 ),
 .UNSPECIFIED., .F., .F.,
 ( 4, 2, 2, 2, 2, 2, 2, 2, 2, 2, 2, 2, 2, 2, 2, 2, 2, 2, 2, 2, 2, 4 ),
 ( 6.938893903907228378E-18, 0.001488594467279747650, 0.002232891700919627329, 0.002977188934559507009, 0.004465783401839248587, 0.005954377869118990599, 0.007442972336398733478, 0.008187269570038610556, 0.008931566803678486766, 0.01042016127095824786, 0.01190875573823800895, 0.01265305297187786955, 0.01339735020551772841, 0.01488594467279744440, 0.01563024190643729980, 0.01637453914007715866, 0.01786313360735687292, 0.01935172807463658370, 0.02009602530827643563, 0.02084032254191628408, 0.02232891700919596364, 0.02381751147647563627 ),
 .UNSPECIFIED. ) ;
#20142 = CARTESIAN_POINT ( 'NONE',  ( 16.77104078056616743, 7.540619757007628543, -62.41212509805560416 ) ) ;
#20143 = FACE_OUTER_BOUND ( 'NONE', #22508, .T. ) ;
#20144 = CARTESIAN_POINT ( 'NONE',  ( 21.77974805481932918, -62.98608706026495696, 34.48241823983692456 ) ) ;
#20145 = CARTESIAN_POINT ( 'NONE',  ( -439.4229916354183842, 388.0000000000020464, 91.05029585799266556 ) ) ;
#20147 = CARTESIAN_POINT ( 'NONE',  ( 141.3586046882815026, 47.34625111366350581, -44.03220709178651049 ) ) ;
#20146 = CIRCLE ( 'NONE', #48232, 5.000000000000170530 ) ;
#20148 = CARTESIAN_POINT ( 'NONE',  ( 33.44983424733137412, 7.709709042132400825, -38.53006481374713843 ) ) ;
#20149 = EDGE_CURVE ( 'NONE', #51034, #10115, #23835, .T. ) ;
#20150 = CARTESIAN_POINT ( 'NONE',  ( 8.679939806240508204, 7.383357464882124077, -40.61437127068128916 ) ) ;
#20151 = DIRECTION ( 'NONE',  ( 0.000000000000000000, 0.000000000000000000, 1.000000000000000000 ) ) ;
#20152 = CARTESIAN_POINT ( 'NONE',  ( -120.5002574492098972, 44.22930148497321312, -10.35167903076605000 ) ) ;
#20153 = EDGE_LOOP ( 'NONE', ( #42491, #47555, #19177, #45122 ) ) ;
#20154 = EDGE_LOOP ( 'NONE', ( #26387, #4613, #65940, #10571 ) ) ;
#20155 = ADVANCED_FACE ( 'NONE', ( #6350 ), #27803, .F. ) ;
#20156 = CARTESIAN_POINT ( 'NONE',  ( 70.65683382808231272, -25.18281821780013274, 170.0000000000000000 ) ) ;
#20157 = DIRECTION ( 'NONE',  ( -1.000000000000000000, 0.000000000000000000, 0.000000000000000000 ) ) ;
#20158 = CARTESIAN_POINT ( 'NONE',  ( -31.43908319763709969, 9.591432048623762086, -62.16174795566551836 ) ) ;
#20159 = AXIS2_PLACEMENT_3D ( 'NONE', #26012, #63977, #47439 ) ;
#20160 = CARTESIAN_POINT ( 'NONE',  ( 8.336031647119268584, 6.376437040857334537, 11.64877837691457607 ) ) ;
#20161 = CARTESIAN_POINT ( 'NONE',  ( 43.35536254672140188, 9.973606330917814233, -76.34245829030946595 ) ) ;
#20162 = CARTESIAN_POINT ( 'NONE',  ( 33.08881014127219089, 4.734317623318680113, 6.893343212288931099 ) ) ;
#20163 = DIRECTION ( 'NONE',  ( 0.000000000000000000, 0.000000000000000000, 1.000000000000000000 ) ) ;
#20164 = CARTESIAN_POINT ( 'NONE',  ( -177.5259994307673423, 92.16784265327252967, -48.30003138184611089 ) ) ;
#20165 = CARTESIAN_POINT ( 'NONE',  ( -40.27405704175544088, -63.28161525591325187, 43.58025477438756923 ) ) ;
#20166 = CARTESIAN_POINT ( 'NONE',  ( -27.70185240367227664, 10.02491413133431131, 58.05382884042261082 ) ) ;
#20167 = DIRECTION ( 'NONE',  ( 0.000000000000000000, 0.000000000000000000, 1.000000000000000000 ) ) ;
#20168 = EDGE_CURVE ( 'NONE', #20075, #40730, #24281, .T. ) ;
#20169 = CARTESIAN_POINT ( 'NONE',  ( -51.35181696773308602, 13.72007042346227479, 58.12010125874579103 ) ) ;
#20170 = EDGE_CURVE ( 'NONE', #20616, #29587, #5371, .T. ) ;
#20171 = ADVANCED_FACE ( 'NONE', ( #18296 ), #55242, .T. ) ;
#20172 = VERTEX_POINT ( 'NONE', #45377 ) ;
#20173 = CARTESIAN_POINT ( 'NONE',  ( -9.744241498306646321, -37.07486245478190057, 13.32819397642333392 ) ) ;
#20174 = CARTESIAN_POINT ( 'NONE',  ( 0.000000000000000000, 0.000000000000000000, 0.000000000000000000 ) ) ;
#20175 = CARTESIAN_POINT ( 'NONE',  ( 156.5890478960376697, 58.24007662587948175, 71.21522256953024055 ) ) ;
#20176 = CARTESIAN_POINT ( 'NONE',  ( -103.2164890789475606, 34.39030697009940951, -61.90300353352128582 ) ) ;
#20177 = CARTESIAN_POINT ( 'NONE',  ( 0.000000000000000000, 0.000000000000000000, 41.38025477438755928 ) ) ;
#20178 = CARTESIAN_POINT ( 'NONE',  ( -17.50000000000002842, 207.5000000000000284, 378.0000000000000000 ) ) ;
#20179 = CARTESIAN_POINT ( 'NONE',  ( 311.9975424824652350, 295.8720703627916464, 535.5371946177799600 ) ) ;
#20180 = ORIENTED_EDGE ( 'NONE', *, *, #38441, .T. ) ;
#20181 = CARTESIAN_POINT ( 'NONE',  ( -61.38706483483509402, 16.47181058798476272, 68.68523971831442054 ) ) ;
#20182 = ORIENTED_EDGE ( 'NONE', *, *, #57804, .F. ) ;
#20183 = EDGE_LOOP ( 'NONE', ( #2314, #17880 ) ) ;
#20184 = CARTESIAN_POINT ( 'NONE',  ( -417.6627218934913230, 179.4906275429376308, -144.4497041420118819 ) ) ;
#20185 = DIRECTION ( 'NONE',  ( 0.000000000000000000, 1.000000000000000000, 0.000000000000000000 ) ) ;
#20186 = FACE_OUTER_BOUND ( 'NONE', #49621, .T. ) ;
#20187 = ORIENTED_EDGE ( 'NONE', *, *, #2155, .F. ) ;
#20188 = AXIS2_PLACEMENT_3D ( 'NONE', #43013, #21236, #26514 ) ;
#20189 = LINE ( 'NONE', #63102, #10895 ) ;
#20190 = CARTESIAN_POINT ( 'NONE',  ( -52.73319225379862019, -53.34578647582125654, 43.58025477438756212 ) ) ;
#20191 = CARTESIAN_POINT ( 'NONE',  ( 60.63380853769237433, 13.16344960520421914, -50.33659022662053673 ) ) ;
#20192 = EDGE_CURVE ( 'NONE', #27636, #52661, #61560, .T. ) ;
#20194 = ADVANCED_FACE ( 'NONE', ( #50650 ), #53031, .T. ) ;
#20193 = CARTESIAN_POINT ( 'NONE',  ( -85.95621526752228192, 26.32462117888284681, 36.13660444380358427 ) ) ;
#20195 = AXIS2_PLACEMENT_3D ( 'NONE', #56694, #45796, #61627 ) ;
#20196 = CARTESIAN_POINT ( 'NONE',  ( -30.46002654261637588, 10.45132580906818021, -23.42440563520737129 ) ) ;
#20197 = DIRECTION ( 'NONE',  ( -1.000000000000000000, 0.000000000000000000, 0.000000000000000000 ) ) ;
#20198 = EDGE_CURVE ( 'NONE', #6856, #47821, #34839, .T. ) ;
#20199 = ORIENTED_EDGE ( 'NONE', *, *, #18202, .T. ) ;
#20200 = DIRECTION ( 'NONE',  ( 0.000000000000000000, -1.000000000000000000, 0.000000000000000000 ) ) ;
#20201 = CARTESIAN_POINT ( 'NONE',  ( 8.683531412707433006, 6.377173148747124820, 66.77437832024716613 ) ) ;
#20202 = CARTESIAN_POINT ( 'NONE',  ( -24.95029760921699591, 9.631514785009935409, 33.94725700252100609 ) ) ;
#20203 = CARTESIAN_POINT ( 'NONE',  ( 204.3091227790962989, 107.5190503136782638, 44.20772073876946706 ) ) ;
#20204 = CARTESIAN_POINT ( 'NONE',  ( -71.35453793101461883, 20.73435672776740191, 89.90586990597532235 ) ) ;
#20206 = VERTEX_POINT ( 'NONE', #63971 ) ;
#20205 = DIRECTION ( 'NONE',  ( 0.000000000000000000, 0.000000000000000000, 1.000000000000000000 ) ) ;
#20207 = CARTESIAN_POINT ( 'NONE',  ( 68.62997155117722059, 15.08415013720828668, 42.30982577549439583 ) ) ;
#20208 = ORIENTED_EDGE ( 'NONE', *, *, #30117, .F. ) ;
#20209 = AXIS2_PLACEMENT_3D ( 'NONE', #10947, #55246, #1097 ) ;
#20210 = ORIENTED_EDGE ( 'NONE', *, *, #67936, .T. ) ;
#20211 = CARTESIAN_POINT ( 'NONE',  ( 113.4402889550712956, 31.50582881646778333, -63.46592719120694426 ) ) ;
#20212 = CARTESIAN_POINT ( 'NONE',  ( 2.129405171194437063, -25.03204795498853841, 0.000000000000000000 ) ) ;
#20213 = DIRECTION ( 'NONE',  ( -0.000000000000000000, -0.000000000000000000, -1.000000000000000000 ) ) ;
#20214 = CARTESIAN_POINT ( 'NONE',  ( 31.11269837220806522, -6.375108774214766072E-14, 2.000000000000001776 ) ) ;
#20215 = DIRECTION ( 'NONE',  ( 0.000000000000000000, 0.000000000000000000, 1.000000000000000000 ) ) ;
#20216 = CARTESIAN_POINT ( 'NONE',  ( -85.36298448216592760, 26.07611629625833771, -12.35578000808629184 ) ) ;
#20217 = DIRECTION ( 'NONE',  ( 0.000000000000000000, 0.000000000000000000, 1.000000000000000000 ) ) ;
#20218 = CARTESIAN_POINT ( 'NONE',  ( -151.2410113808308552, 65.66338888995502998, -49.62284842420343978 ) ) ;
#20219 = ORIENTED_EDGE ( 'NONE', *, *, #8191, .T. ) ;
#20220 = ORIENTED_EDGE ( 'NONE', *, *, #61365, .T. ) ;
#20221 = DIRECTION ( 'NONE',  ( -0.000000000000000000, -0.000000000000000000, 1.000000000000000000 ) ) ;
#20222 = CARTESIAN_POINT ( 'NONE',  ( -452.6627218934912662, 364.9999999999998295, 113.5502958579879760 ) ) ;
#20223 = CARTESIAN_POINT ( 'NONE',  ( 116.9223627093533509, 32.09655261207334576, 87.37230592524522876 ) ) ;
#20224 = CONICAL_SURFACE ( 'NONE', #32571, 65.00000000000000000, 0.7853981633974497223 ) ;
#20225 = FACE_OUTER_BOUND ( 'NONE', #68492, .T. ) ;
#20226 = CARTESIAN_POINT ( 'NONE',  ( -19.46539569203835640, 15.68752276659279943, 0.000000000000000000 ) ) ;
#20227 = CARTESIAN_POINT ( 'NONE',  ( 417.3372781065083359, 395.0000000000041496, 83.55029585798409641 ) ) ;
#20228 = LINE ( 'NONE', #9331, #5983 ) ;
#20229 = ORIENTED_EDGE ( 'NONE', *, *, #59719, .T. ) ;
#20230 = ORIENTED_EDGE ( 'NONE', *, *, #51610, .F. ) ;
#20231 = VERTEX_POINT ( 'NONE', #42174 ) ;
#20232 = EDGE_CURVE ( 'NONE', #57073, #10801, #31286, .T. ) ;
#20233 = DIRECTION ( 'NONE',  ( -1.000000000000000000, 0.000000000000000000, 0.000000000000000000 ) ) ;
#20234 = CARTESIAN_POINT ( 'NONE',  ( 174.1355634792904254, 71.85737575453710235, -94.55186492391756303 ) ) ;
#20235 = CARTESIAN_POINT ( 'NONE',  ( 109.3475734619033659, -21.43178884250801275, 4.968175626252066657 ) ) ;
#20236 = DIRECTION ( 'NONE',  ( 0.000000000000000000, 0.000000000000000000, 1.000000000000000000 ) ) ;
#20237 = FACE_OUTER_BOUND ( 'NONE', #26458, .T. ) ;
#20238 = CIRCLE ( 'NONE', #15770, 25.12245591505646303 ) ;
#20239 = CARTESIAN_POINT ( 'NONE',  ( 184.3879440808139805, 83.47316703125162007, 70.38978263608034069 ) ) ;
#20240 = CARTESIAN_POINT ( 'NONE',  ( 46.58610174774756985, 9.452965170565081010, 88.92390424605549981 ) ) ;
#20241 = SHAPE_REPRESENTATION_RELATIONSHIP ( 'NONE' , 'NONE' ,  #19523, #10569 ) ;
#20242 = ORIENTED_EDGE ( 'NONE', *, *, #49797, .T. ) ;
#20243 = CARTESIAN_POINT ( 'NONE',  ( 22.51849650178395734, 7.817407610814552044, 13.98895852407905949 ) ) ;
#20244 = CARTESIAN_POINT ( 'NONE',  ( 20.86596583059835552, 36.13760021380633702, 13.79046340968177908 ) ) ;
#20245 = CARTESIAN_POINT ( 'NONE',  ( 15.55634918610411610, 46.66904755831205875, 0.000000000000000000 ) ) ;
#20246 = DIRECTION ( 'NONE',  ( 1.000000000000000000, 0.000000000000000000, 0.000000000000000000 ) ) ;
#20247 = CARTESIAN_POINT ( 'NONE',  ( 133.3990214534116774, 41.14886683286415803, -24.16826940798425838 ) ) ;
#20248 = ADVANCED_FACE ( 'NONE', ( #15450 ), #58012, .T. ) ;
#20249 = LINE ( 'NONE', #25548, #8514 ) ;
#20250 = CARTESIAN_POINT ( 'NONE',  ( 11.20486344102687504, 7.403248964808827104, 16.62706366644169620 ) ) ;
#20251 = EDGE_CURVE ( 'NONE', #7998, #12593, #63143, .T. ) ;
#20252 = B_SPLINE_CURVE_WITH_KNOTS ( 'NONE', 3,
 ( #38371, #5330, #42941, #64411, #10942, #44340, #38730, #1093, #16220, #22199, #64762, #32413, #59816, #386, #11631, #33105, #53838, #49609, #60174, #10590, #745, #5657, #27463, #27117, #6003, #54891, #27822, #48212, #54541, #37, #37674, #6368, #65825, #43287, #11995, #43637, #21842, #1442, #17258, #48907, #65114, #17619, #22895, #59121 ),
 .UNSPECIFIED., .F., .F.,
 ( 4, 2, 2, 2, 2, 2, 2, 2, 2, 2, 2, 2, 2, 2, 2, 2, 2, 2, 2, 2, 2, 4 ),
 ( 0.02908143158676655682, 0.03095422299093871302, 0.03282701439511086922, 0.03469980579928302888, 0.03657259720345518855, 0.03844538860762734822, 0.04031818001179950095, 0.04125457571388553568, 0.04219097141597157041, 0.04312736711805760514, 0.04359556496910062251, 0.04406376282014363988, 0.04500015852222963991, 0.04593655422431563301, 0.04687294992640163305, 0.04780934562848762615, 0.04968213703265959846, 0.05155492843683157078, 0.05342771984100353616, 0.05530051124517551542, 0.05717330264934748080, 0.05904609405351945312 ),
 .UNSPECIFIED. ) ;
#20253 = EDGE_CURVE ( 'NONE', #38528, #65730, #57320, .T. ) ;
#20254 = VERTEX_POINT ( 'NONE', #21400 ) ;
#20255 = CARTESIAN_POINT ( 'NONE',  ( 188.4937788906148626, 86.43336847120863808, 11.16285860195706547 ) ) ;
#20256 = APPLICATION_PROTOCOL_DEFINITION ( 'draft international standard', 'automotive_design', 1998, #3532 ) ;
#20257 = VECTOR ( 'NONE', #25524, 1000.000000000000000 ) ;
#20258 = CARTESIAN_POINT ( 'NONE',  ( 181.0840389613909736, 78.60582251573003987, 44.30859410551141764 ) ) ;
#20259 = CARTESIAN_POINT ( 'NONE',  ( -21.93488243476846478, -35.49895327440580672, 13.79046412364926333 ) ) ;
#20260 = CARTESIAN_POINT ( 'NONE',  ( 41.80536115778102868, 8.734184316430667394, -77.07306109708069641 ) ) ;
#20261 = CARTESIAN_POINT ( 'NONE',  ( 187.8973304652193121, 87.27378997243174297, -46.87199284111774489 ) ) ;
#20262 = ORIENTED_EDGE ( 'NONE', *, *, #30667, .T. ) ;
#20263 = ORIENTED_EDGE ( 'NONE', *, *, #40347, .T. ) ;
#20264 = CARTESIAN_POINT ( 'NONE',  ( -144.2029146819478456, 59.80706661873674790, -10.14434587346329941 ) ) ;
#20265 = CARTESIAN_POINT ( 'NONE',  ( -68.11501976657856972, 31.41506934893843805, 170.0000000000000000 ) ) ;
#20266 = EDGE_LOOP ( 'NONE', ( #62457, #30578, #48710, #26934 ) ) ;
#20267 = CARTESIAN_POINT ( 'NONE',  ( 113.4493678088378346, 30.39339414805073858, 70.75222796080394971 ) ) ;
#20268 = EDGE_LOOP ( 'NONE', ( #7912, #29670, #42435, #16415 ) ) ;
#20269 = LINE ( 'NONE', #31188, #42423 ) ;
#20270 = CARTESIAN_POINT ( 'NONE',  ( 46.66904755831207297, -15.55634918610412853, 0.000000000000000000 ) ) ;
#20271 = B_SPLINE_CURVE_WITH_KNOTS ( 'NONE', 3,
 ( #20934, #58551, #10368, #31834 ),
 .UNSPECIFIED., .F., .F.,
 ( 4, 4 ),
 ( 0.1259919275528363081, 0.1829744153748759372 ),
 .UNSPECIFIED. ) ;
#20272 = CARTESIAN_POINT ( 'NONE',  ( -15.55634918610408945, -31.11269837220804035, 2.000000000000001776 ) ) ;
#20273 = VECTOR ( 'NONE', #49190, 1000.000000000000000 ) ;
#20274 = CARTESIAN_POINT ( 'NONE',  ( -94.84390436305045569, 29.16104988397310649, 39.02940028697720010 ) ) ;
#20275 = DIRECTION ( 'NONE',  ( -0.000000000000000000, 1.000000000000000000, -0.000000000000000000 ) ) ;
#20277 = ORIENTED_EDGE ( 'NONE', *, *, #18668, .T. ) ;
#20276 = LINE ( 'NONE', #29446, #66835 ) ;
#20278 = EDGE_CURVE ( 'NONE', #22871, #60851, #4732, .T. ) ;
#20279 = CARTESIAN_POINT ( 'NONE',  ( 254.4165763529819344, -27.00000000000000355, 128.9999999999999716 ) ) ;
#20280 = ORIENTED_EDGE ( 'NONE', *, *, #37541, .F. ) ;
#20281 = EDGE_LOOP ( 'NONE', ( #37278, #60625, #30752, #12668, #20539, #41970, #18810, #40398, #2655, #33761, #63561, #57088, #68848, #68555, #2199, #64811, #31459, #25249, #59345, #46386, #286, #58587, #63518, #7742, #50002, #34406, #13133, #11899, #54738, #31033, #27385, #13289, #199, #10105, #47474, #7792, #55812, #18357, #40839, #54854, #25541, #399, #12259, #67096, #11456, #17846, #6000, #328, #53511, #67037, #22984, #25385, #13119, #16307, #30866, #41677, #67961, #67914, #26810, #53976, #3980, #57386, #62090, #37072, #22605, #5589, #30235, #58414, #7781, #1438, #49355, #28087, #5216, #8343, #43184, #35787, #28207, #56033, #66348, #7999, #43612, #63451, #42804, #27688, #29484, #32087, #35128, #20038, #66450, #21606, #59894, #34253, #38893, #4818, #44610, #39374, #7954, #29111, #47637, #36139, #53897, #64557, #57727 ) ) ;
#20282 = CARTESIAN_POINT ( 'NONE',  ( -123.4531143159639441, 44.90777521523904880, -22.66459338198712103 ) ) ;
#20283 = DIRECTION ( 'NONE',  ( -1.000000000000000000, 0.000000000000000000, 0.000000000000000000 ) ) ;
#20284 = CARTESIAN_POINT ( 'NONE',  ( -176.3896317155480062, 90.84057090619018027, -22.13191603966969012 ) ) ;
#20286 = ORIENTED_EDGE ( 'NONE', *, *, #40501, .T. ) ;
#20285 = CARTESIAN_POINT ( 'NONE',  ( -133.3316503378477762, 52.82738260200863323, 63.86119459864413272 ) ) ;
#20287 = CARTESIAN_POINT ( 'NONE',  ( -107.7144780656001330, 36.77195912774744357, 86.50315365870005735 ) ) ;
#20288 = DIRECTION ( 'NONE',  ( -1.000000000000000000, 0.000000000000000000, 0.000000000000000000 ) ) ;
#20289 = ORIENTED_EDGE ( 'NONE', *, *, #64654, .F. ) ;
#20290 = DIRECTION ( 'NONE',  ( -1.000000000000000000, 0.000000000000000000, 0.000000000000000000 ) ) ;
#20291 = CARTESIAN_POINT ( 'NONE',  ( -133.1640943168118554, 52.70734926280009347, -67.39673842532138792 ) ) ;
#20292 = CARTESIAN_POINT ( 'NONE',  ( 60.23839536713451537, 12.04563565271882908, -89.93993854489507100 ) ) ;
#20293 = DIRECTION ( 'NONE',  ( -0.000000000000000000, -1.000000000000000000, 0.000000000000000000 ) ) ;
#20294 = CARTESIAN_POINT ( 'NONE',  ( 64.94098077424392557, 14.16208887966257102, -77.33007373951066654 ) ) ;
#20295 = ORIENTED_EDGE ( 'NONE', *, *, #47994, .T. ) ;
#20296 = EDGE_LOOP ( 'NONE', ( #45452, #35267, #18193, #39783 ) ) ;
#20297 = VECTOR ( 'NONE', #61330, 1000.000000000000000 ) ;
#20298 = CARTESIAN_POINT ( 'NONE',  ( 181.9406741394861911, 79.47484497224795064, -63.10656098916969370 ) ) ;
#20299 = CARTESIAN_POINT ( 'NONE',  ( -169.1005390226459326, 82.76152663947085841, -35.86510333151966279 ) ) ;
#20300 = CARTESIAN_POINT ( 'NONE',  ( 111.9975424824652634, 172.0000000000000284, 536.6193948016162949 ) ) ;
#20301 = CARTESIAN_POINT ( 'NONE',  ( 103.1695711638930817, 26.83837309506524704, -72.81073785818523447 ) ) ;
#20302 = CARTESIAN_POINT ( 'NONE',  ( -73.80418150970713498, 21.59712875466422588, 32.18635260252404606 ) ) ;
#20303 = DIRECTION ( 'NONE',  ( 0.000000000000000000, -1.000000000000000000, -2.184185950696548891E-33 ) ) ;
#20304 = CARTESIAN_POINT ( 'NONE',  ( 66.73467315386238852, 14.60276727483218906, -36.68961546505575200 ) ) ;
#20305 = DIRECTION ( 'NONE',  ( -1.000000000000000000, -0.000000000000000000, 0.000000000000000000 ) ) ;
#20306 = CARTESIAN_POINT ( 'NONE',  ( -171.4867114763004281, 85.32693843184998173, -76.38800489763023904 ) ) ;
#20308 = ORIENTED_EDGE ( 'NONE', *, *, #22057, .F. ) ;
#20307 = EDGE_CURVE ( 'NONE', #18940, #52822, #10498, .T. ) ;
#20309 = CARTESIAN_POINT ( 'NONE',  ( -107.0584934212648420, 35.27493744466473657, -9.868436795408833007 ) ) ;
#20310 = ORIENTED_EDGE ( 'NONE', *, *, #43551, .T. ) ;
#20311 = AXIS2_PLACEMENT_3D ( 'NONE', #5406, #65188, #11713 ) ;
#20312 = CARTESIAN_POINT ( 'NONE',  ( -180.5312359056721618, 95.77409857860999409, -94.70578744242111213 ) ) ;
#20313 = EDGE_CURVE ( 'NONE', #17237, #67632, #68888, .T. ) ;
#20314 = CARTESIAN_POINT ( 'NONE',  ( 79.37778929114111293, 18.12554302172301490, 66.03557851574602466 ) ) ;
#20315 = CARTESIAN_POINT ( 'NONE',  ( 0.000000000000000000, 0.000000000000000000, 170.0000000000000000 ) ) ;
#20316 = CARTESIAN_POINT ( 'NONE',  ( -189.2826425734429279, 107.1493800926106275, -68.08208096063634684 ) ) ;
#20317 = CARTESIAN_POINT ( 'NONE',  ( 410.0000000000000000, 190.0000000000000000, 0.000000000000000000 ) ) ;
#20318 = LINE ( 'NONE', #14363, #24893 ) ;
#20319 = DIRECTION ( 'NONE',  ( -0.000000000000000000, -1.000000000000000000, -0.000000000000000000 ) ) ;
#20320 = FACE_OUTER_BOUND ( 'NONE', #47499, .T. ) ;
#20321 = AXIS2_PLACEMENT_3D ( 'NONE', #4396, #36753, #36062 ) ;
#20322 = CARTESIAN_POINT ( 'NONE',  ( -38.92718193365331558, 11.96647478777219931, -15.48328760661300052 ) ) ;
#20323 = ORIENTED_EDGE ( 'NONE', *, *, #34312, .T. ) ;
#20324 = CARTESIAN_POINT ( 'NONE',  ( 149.0250918491436494, 0.000000000000000000, -46.68900338898718161 ) ) ;
#20325 = ORIENTED_EDGE ( 'NONE', *, *, #31005, .T. ) ;
#20326 = FACE_OUTER_BOUND ( 'NONE', #59021, .T. ) ;
#20327 = PRESENTATION_STYLE_ASSIGNMENT (( #47392 ) ) ;
#20328 = CARTESIAN_POINT ( 'NONE',  ( -189.7334103489410495, 107.7745063523401257, 8.881755487159328055 ) ) ;
#20329 = DIRECTION ( 'NONE',  ( 0.000000000000000000, 1.000000000000000000, -0.000000000000000000 ) ) ;
#20330 = CARTESIAN_POINT ( 'NONE',  ( -14.55390976651257873, 7.422979442794215288, -73.08496616077771080 ) ) ;
#20331 = CARTESIAN_POINT ( 'NONE',  ( -101.3492134984965531, 32.31003911421601060, -8.213220048528352635 ) ) ;
#20332 = CARTESIAN_POINT ( 'NONE',  ( 156.5890478960376413, 58.24007662587944623, -36.16297979232447091 ) ) ;
#20333 = EDGE_CURVE ( 'NONE', #55323, #39717, #29669, .T. ) ;
#20334 = EDGE_CURVE ( 'NONE', #54975, #64346, #46310, .T. ) ;
#20335 = ORIENTED_EDGE ( 'NONE', *, *, #42565, .T. ) ;
#20336 = DIRECTION ( 'NONE',  ( -0.9999999288524208385, -0.0003772202979824376039, -2.172995263545127176E-16 ) ) ;
#20337 = LINE ( 'NONE', #29509, #19458 ) ;
#20338 = CARTESIAN_POINT ( 'NONE',  ( 175.0696098417091378, 74.11936424544842339, -21.36851627469916082 ) ) ;
#20339 = CARTESIAN_POINT ( 'NONE',  ( 64.98797965777978902, 1.249999999999979350, 170.0000000000000000 ) ) ;
#20340 = DIRECTION ( 'NONE',  ( 0.8584487936018727616, -0.5128992774058949156, 0.000000000000000000 ) ) ;
#20341 = ORIENTED_EDGE ( 'NONE', *, *, #1502, .F. ) ;
#20342 = CARTESIAN_POINT ( 'NONE',  ( -179.2128128997734962, 95.75254520622995358, -73.46006140737962653 ) ) ;
#20343 = CARTESIAN_POINT ( 'NONE',  ( -2.355184675731021304, 6.596450510445342807, -21.21029824059963786 ) ) ;
#20344 = CARTESIAN_POINT ( 'NONE',  ( 113.4351684956570523, 30.38657459074490319, 30.30815483564448343 ) ) ;
#20345 = LINE ( 'NONE', #2797, #41653 ) ;
#20346 = CARTESIAN_POINT ( 'NONE',  ( -27.00000000000000355, -30.00000000000000355, 15.00000000000000000 ) ) ;
#20347 = ORIENTED_EDGE ( 'NONE', *, *, #58421, .F. ) ;
#20348 = CARTESIAN_POINT ( 'NONE',  ( 199.7255144154428592, 99.76581417577200739, 31.07377068937141473 ) ) ;
#20349 = CARTESIAN_POINT ( 'NONE',  ( 116.5096233816161941, 31.89062767870469983, -74.39514096115526343 ) ) ;
#20350 = CARTESIAN_POINT ( 'NONE',  ( 188.5651904823862424, 88.01586411309099844, 37.41956129399849829 ) ) ;
#20351 = DIRECTION ( 'NONE',  ( 0.000000000000000000, 0.000000000000000000, 1.000000000000000000 ) ) ;
#20352 = DIRECTION ( 'NONE',  ( 1.000000000000000000, -0.000000000000000000, -0.000000000000000000 ) ) ;
#20353 = AXIS2_PLACEMENT_3D ( 'NONE', #12131, #17034, #49392 ) ;
#20354 = AXIS2_PLACEMENT_3D ( 'NONE', #14561, #56428, #61705 ) ;
#20355 = EDGE_LOOP ( 'NONE', ( #57247, #41936, #42444, #59571 ) ) ;
#20356 = CARTESIAN_POINT ( 'NONE',  ( 174.6307688320643479, 73.70327352127002030, 59.82234444106918403 ) ) ;
#20357 = CIRCLE ( 'NONE', #1286, 24.99999999999985434 ) ;
#20358 = EDGE_LOOP ( 'NONE', ( #40227, #3870 ) ) ;
#20359 = CARTESIAN_POINT ( 'NONE',  ( -109.3553681454883844, 36.52260784104392854, -45.05470719201598229 ) ) ;
#20360 = CARTESIAN_POINT ( 'NONE',  ( 136.3708086338960470, 42.96321442892168818, 83.62629360459338557 ) ) ;
#20361 = CARTESIAN_POINT ( 'NONE',  ( -62.53989795537026453, 16.81768094534200131, 38.32257745060478982 ) ) ;
#20363 = ORIENTED_EDGE ( 'NONE', *, *, #41155, .T. ) ;
#20362 = CARTESIAN_POINT ( 'NONE',  ( 151.8005253678161921, 54.62151558044536159, 5.128849957095197531 ) ) ;
#20364 = CARTESIAN_POINT ( 'NONE',  ( 160.9099843287285125, 61.67000084894969092, -50.30479636640266961 ) ) ;
#20365 = VECTOR ( 'NONE', #63322, 1000.000000000000000 ) ;
#20366 = DIRECTION ( 'NONE',  ( -0.000000000000000000, 1.000000000000000000, -0.000000000000000000 ) ) ;
#20367 = DIRECTION ( 'NONE',  ( 0.9909497617679352555, -0.1342332658176522697, 5.102127870520022769E-18 ) ) ;
#20368 = EDGE_LOOP ( 'NONE', ( #51086, #8149, #47190 ) ) ;
#20369 = FACE_OUTER_BOUND ( 'NONE', #35571, .T. ) ;
#20370 = CARTESIAN_POINT ( 'NONE',  ( -149.5074843970971301, 64.17983161892345834, -49.81283053149198992 ) ) ;
#20371 = ORIENTED_EDGE ( 'NONE', *, *, #55486, .T. ) ;
#20372 = LINE ( 'NONE', #53058, #21885 ) ;
#20373 = CARTESIAN_POINT ( 'NONE',  ( -180.6215424137752450, 97.48070480470856580, 38.62763768963357336 ) ) ;
#20374 = CARTESIAN_POINT ( 'NONE',  ( 150.8925291903903769, 52.71218673668931132, 60.11153687441628080 ) ) ;
#20375 = CARTESIAN_POINT ( 'NONE',  ( 400.0000000000000000, 0.000000000000000000, 0.000000000000000000 ) ) ;
#20376 = EDGE_LOOP ( 'NONE', ( #9332, #50137, #63981, #48731 ) ) ;
#20377 = CARTESIAN_POINT ( 'NONE',  ( 45.89268866913128875, 10.36133864615985622, 14.33506431777695056 ) ) ;
#20378 = ORIENTED_EDGE ( 'NONE', *, *, #19931, .F. ) ;
#20379 = CARTESIAN_POINT ( 'NONE',  ( 154.0515132159917471, 56.29926936869308918, -23.47126196184992253 ) ) ;
#20380 = ADVANCED_FACE ( 'NONE', ( #17509 ), #285, .F. ) ;
#20381 = CARTESIAN_POINT ( 'NONE',  ( 210.9631450001600683, 117.1791136960929265, -21.14097324130973377 ) ) ;
#20382 = CARTESIAN_POINT ( 'NONE',  ( 102.7446498997619955, 26.65764321315730001, 36.57460656155974021 ) ) ;
#20383 = CARTESIAN_POINT ( 'NONE',  ( -156.0171627975467743, 69.90368824761765154, -65.42354838375587178 ) ) ;
#20384 = PLANE ( 'NONE',  #53870 ) ;
#20385 = CARTESIAN_POINT ( 'NONE',  ( 188.5653887627527752, 88.01608521313129074, 9.354702516507275689 ) ) ;
#20386 = CARTESIAN_POINT ( 'NONE',  ( 211.5066273949819333, 116.1727691518061789, -47.01952303312400971 ) ) ;
#20387 = EDGE_CURVE ( 'NONE', #27523, #68787, #38985, .T. ) ;
#20388 = DIRECTION ( 'NONE',  ( -1.000000000000000000, -0.000000000000000000, -0.000000000000000000 ) ) ;
#20389 = ORIENTED_EDGE ( 'NONE', *, *, #63127, .T. ) ;
#20390 = DIRECTION ( 'NONE',  ( -0.6910626489868685329, 0.7227948638273878901, 0.000000000000000000 ) ) ;
#20392 = VERTEX_POINT ( 'NONE', #1342 ) ;
#20391 = EDGE_CURVE ( 'NONE', #47218, #22681, #23151, .T. ) ;
#20393 = CARTESIAN_POINT ( 'NONE',  ( -73.10086105983764071, 21.34631349770505082, 69.81410049433821996 ) ) ;
#20394 = CARTESIAN_POINT ( 'NONE',  ( 61.33627421985469397, 12.28939706835343237, -62.75169496998579888 ) ) ;
#20395 = SURFACE_STYLE_USAGE ( .BOTH. , #3534 ) ;
#20396 = DIRECTION ( 'NONE',  ( 1.850371928290090422E-16, -1.000000000000000000, -1.110223024625156294E-16 ) ) ;
#20397 = EDGE_CURVE ( 'NONE', #20568, #27916, #32999, .T. ) ;
#20398 = CARTESIAN_POINT ( 'NONE',  ( -0.4830416248186119588, 6.524023950717643849, 92.86839907411122397 ) ) ;
#20399 = AXIS2_PLACEMENT_3D ( 'NONE', #68953, #3565, #29959 ) ;
#20400 = CARTESIAN_POINT ( 'NONE',  ( -109.7079446832838983, 37.86719386855315861, -16.74036298271016321 ) ) ;
#20401 = VERTEX_POINT ( 'NONE', #44598 ) ;
#20402 = AXIS2_PLACEMENT_3D ( 'NONE', #62507, #3412, #40349 ) ;
#20403 = CARTESIAN_POINT ( 'NONE',  ( -78.66644367742109978, 22.32174330031321574, 72.26275173013684139 ) ) ;
#20404 = LINE ( 'NONE', #30978, #20666 ) ;
#20405 = ORIENTED_EDGE ( 'NONE', *, *, #21832, .F. ) ;
#20406 = ORIENTED_EDGE ( 'NONE', *, *, #29864, .F. ) ;
#20407 = CARTESIAN_POINT ( 'NONE',  ( -152.9119739516381458, 67.12135129037712034, 31.52259186888439046 ) ) ;
#20408 = CARTESIAN_POINT ( 'NONE',  ( 56.19513604272050600, 11.19349063094192509, -40.09155741990996802 ) ) ;
#20410 = CARTESIAN_POINT ( 'NONE',  ( 447.3372781065089612, 365.0000000000064233, -146.4497041420121377 ) ) ;
#20409 = CIRCLE ( 'NONE', #59705, 8.000000000000000000 ) ;
#20411 = AXIS2_PLACEMENT_3D ( 'NONE', #45171, #7558, #46201 ) ;
#20412 = CARTESIAN_POINT ( 'NONE',  ( -22.15007195153847164, -31.28689791206514670, 13.32819397642333037 ) ) ;
#20413 = LINE ( 'NONE', #53098, #1623 ) ;
#20414 = EDGE_CURVE ( 'NONE', #36166, #902, #43540, .T. ) ;
#20415 = VECTOR ( 'NONE', #40095, 1000.000000000000000 ) ;
#20416 = VERTEX_POINT ( 'NONE', #32654 ) ;
#20417 = CARTESIAN_POINT ( 'NONE',  ( -131.6253556217205016, 51.61436399519948282, 33.25658671114208431 ) ) ;
#20418 = EDGE_LOOP ( 'NONE', ( #25518, #324, #28874, #25819 ) ) ;
#20419 = CARTESIAN_POINT ( 'NONE',  ( 212.1707951106656935, 117.1901534358505614, 10.52110880440418939 ) ) ;
#20420 = CARTESIAN_POINT ( 'NONE',  ( -142.9843132609582597, 60.12226089556227748, 41.93116989061249456 ) ) ;
#20421 = CARTESIAN_POINT ( 'NONE',  ( 209.6525588430077960, 113.3929734759396837, 31.07261694010716013 ) ) ;
#20422 = CARTESIAN_POINT ( 'NONE',  ( -74.52723870109949189, 7.962625360374199879, 41.38025477438755928 ) ) ;
#20423 = ORIENTED_EDGE ( 'NONE', *, *, #15515, .T. ) ;
#20424 = EDGE_LOOP ( 'NONE', ( #29848, #3306, #37004, #50191 ) ) ;
#20425 = CARTESIAN_POINT ( 'NONE',  ( 113.0494652463580536, -21.63856170200817530, -3.975743201777092839 ) ) ;
#20426 = CARTESIAN_POINT ( 'NONE',  ( -133.1325180892867479, 52.68453899796251250, 89.73671469607783990 ) ) ;
#20427 = DIRECTION ( 'NONE',  ( 0.000000000000000000, 0.000000000000000000, 1.000000000000000000 ) ) ;
#20428 = CARTESIAN_POINT ( 'NONE',  ( 47.99999999999997158, 19.99999999999996447, 0.000000000000000000 ) ) ;
#20429 = CARTESIAN_POINT ( 'NONE',  ( 20.62507889231323688, 6.703605479764012998, 85.46244512927005132 ) ) ;
#20430 = CARTESIAN_POINT ( 'NONE',  ( 15.13717264782866145, 7.486582872045924653, 83.70339063347323361 ) ) ;
#20431 = ORIENTED_EDGE ( 'NONE', *, *, #48100, .T. ) ;
#20432 = DIRECTION ( 'NONE',  ( -0.000000000000000000, 0.000000000000000000, 1.000000000000000000 ) ) ;
#20433 = CARTESIAN_POINT ( 'NONE',  ( 203.1414537950835779, 105.9225671689748367, -36.47858528242302611 ) ) ;
#20434 = EDGE_LOOP ( 'NONE', ( #3517, #59421, #50911, #42790 ) ) ;
#20435 = CARTESIAN_POINT ( 'NONE',  ( -81.00507684688702170, 23.22613445438389235, 18.20370096348767319 ) ) ;
#20436 = VERTEX_POINT ( 'NONE', #65015 ) ;
#20437 = CARTESIAN_POINT ( 'NONE',  ( -125.8938041572051389, -170.0000000000000000, 30.61994787315706290 ) ) ;
#20438 = EDGE_LOOP ( 'NONE', ( #53088, #33098, #33087, #38795 ) ) ;
#20439 = VECTOR ( 'NONE', #1061, 1000.000000000000000 ) ;
#20440 = ORIENTED_EDGE ( 'NONE', *, *, #68411, .F. ) ;
#20441 = CARTESIAN_POINT ( 'NONE',  ( -118.7011544766493500, 43.11604763363182968, 13.41670242813880876 ) ) ;
#20442 = CARTESIAN_POINT ( 'NONE',  ( -180.0179082103088319, 95.14811732286298707, 68.12739521910877727 ) ) ;
#20443 = CARTESIAN_POINT ( 'NONE',  ( 128.4224537826254675, 38.23837035195749223, 69.04676071552452754 ) ) ;
#20444 = AXIS2_PLACEMENT_3D ( 'NONE', #2472, #40106, #13377 ) ;
#20445 = ORIENTED_EDGE ( 'NONE', *, *, #45032, .T. ) ;
#20446 = B_SPLINE_CURVE_WITH_KNOTS ( 'NONE', 3,
 ( #66085, #1347, #22801, #65727, #17876, #33716, #40370, #68156, #29127, #3430, #8722, #45295, #66780, #19605, #14340, #46680, #51961, #30508, #25244, #35092, #19965, #13637, #13305, #41416, #24556, #8015, #62163, #41066, #30172, #56544, #29818, #40707, #3772, #19253, #50577, #62525 ),
 .UNSPECIFIED., .F., .F.,
 ( 4, 2, 2, 2, 2, 2, 2, 2, 2, 2, 2, 2, 2, 2, 2, 2, 2, 4 ),
 ( 3.469446951953614189E-18, 0.001545474820159074576, 0.003090949640318145682, 0.004636424460477216354, 0.006181899280636287894, 0.007727374100795359434, 0.008500111510874878290, 0.009272848920954396279, 0.01081832374111341144, 0.01236379856127242660, 0.01390927338143144350, 0.01545474820159046039, 0.01700022302174947555, 0.01854569784190849072, 0.02009117266206750935, 0.02163664748222652451, 0.02318212230238554314, 0.02472759712254455483 ),
 .UNSPECIFIED. ) ;
#20447 = ADVANCED_FACE ( 'NONE', ( #55140 ), #16125, .F. ) ;
#20448 = PRODUCT_DEFINITION_SHAPE ( 'NONE', 'NONE',  #69615 ) ;
#20449 = AXIS2_PLACEMENT_3D ( 'NONE', #21067, #5223, #43187 ) ;
#20450 = CARTESIAN_POINT ( 'NONE',  ( -37.14089062983303080, 10.59660406339133942, 86.49034957900197185 ) ) ;
#20451 = DIRECTION ( 'NONE',  ( -0.000000000000000000, -0.000000000000000000, -1.000000000000000000 ) ) ;
#20452 = CARTESIAN_POINT ( 'NONE',  ( -443.8115333961470128, 394.8687311169578606, -126.5269779445883387 ) ) ;
#20453 = CARTESIAN_POINT ( 'NONE',  ( 45.57199999999999562, 6.123233995736766282E-16, -5.000000000000000000 ) ) ;
#20454 = CIRCLE ( 'NONE', #50796, 200.0000000000000000 ) ;
#20455 = CARTESIAN_POINT ( 'NONE',  ( -24.33435124463266419, 8.532637995283112176, 40.13176205844700206 ) ) ;
#20456 = CARTESIAN_POINT ( 'NONE',  ( -146.1201263095600780, 62.66021356509617135, -62.46206482111294633 ) ) ;
#20457 = VERTEX_POINT ( 'NONE', #6965 ) ;
#20458 = VECTOR ( 'NONE', #22087, 1000.000000000000000 ) ;
#20459 = CYLINDRICAL_SURFACE ( 'NONE', #44391, 125.0000000000000000 ) ;
#20460 = CARTESIAN_POINT ( 'NONE',  ( -83.51110947562230535, 25.31252704029285283, -75.19045686144863794 ) ) ;
#20461 = CARTESIAN_POINT ( 'NONE',  ( -7.825402957745085430, 6.891034867348153625, -89.10717191287116634 ) ) ;
#20462 = FACE_OUTER_BOUND ( 'NONE', #26175, .T. ) ;
#20463 = LINE ( 'NONE', #35272, #46748 ) ;
#20464 = CARTESIAN_POINT ( 'NONE',  ( 130.7260704202055024, 39.56565398554880630, 3.334336834773580005 ) ) ;
#20465 = CARTESIAN_POINT ( 'NONE',  ( 36.19799081159146681, 8.014391982702079531, -90.02455723444843727 ) ) ;
#20466 = CARTESIAN_POINT ( 'NONE',  ( -120.5002574492099114, 44.22930148497321312, -64.04078021169341639 ) ) ;
#20467 = EDGE_CURVE ( 'NONE', #50282, #53754, #59748, .T. ) ;
#20468 = CARTESIAN_POINT ( 'NONE',  ( 39.40195752203891999, 9.424259417798145577, 71.75838489642698903 ) ) ;
#20469 = CARTESIAN_POINT ( 'NONE',  ( 164.3577270662354124, 63.21061577643033758, 7.084215918832702741 ) ) ;
#20470 = CARTESIAN_POINT ( 'NONE',  ( -105.4589068214114178, 34.42476264325678414, 31.20975402820559808 ) ) ;
#20471 = ORIENTED_EDGE ( 'NONE', *, *, #67850, .T. ) ;
#20472 = CONTEXT_DEPENDENT_SHAPE_REPRESENTATION ( #19762, #61416 ) ;
#20473 = CARTESIAN_POINT ( 'NONE',  ( -47.88727290496198208, 13.91049128144765490, 93.81492665685888710 ) ) ;
#20474 = ORIENTED_EDGE ( 'NONE', *, *, #36518, .F. ) ;
#20475 = DIRECTION ( 'NONE',  ( -0.000000000000000000, -0.000000000000000000, 1.000000000000000000 ) ) ;
#20476 = ORIENTED_EDGE ( 'NONE', *, *, #6664, .T. ) ;
#20477 = CYLINDRICAL_SURFACE ( 'NONE', #7403, 7.500000000000020428 ) ;
#20478 = DIRECTION ( 'NONE',  ( 0.000000000000000000, 0.000000000000000000, 1.000000000000000000 ) ) ;
#20479 = CARTESIAN_POINT ( 'NONE',  ( -168.7329347389695897, 83.83901812802763232, 32.22089368191161185 ) ) ;
#20480 = EDGE_CURVE ( 'NONE', #48193, #58381, #6261, .T. ) ;
#20481 = CARTESIAN_POINT ( 'NONE',  ( -15.55634918610411077, -41.66904755831209428, 2.000000000000001776 ) ) ;
#20482 = CARTESIAN_POINT ( 'NONE',  ( 140.9141742510256563, 47.05414327990549594, -46.11397078288850082 ) ) ;
#20483 = CARTESIAN_POINT ( 'NONE',  ( 34.83825437341841535, 7.859462995505741567, -49.09150060942670990 ) ) ;
#20484 = CARTESIAN_POINT ( 'NONE',  ( 0.01678220609566017166, 0.7854258609844448902, -8.000000000000000000 ) ) ;
#20485 = CARTESIAN_POINT ( 'NONE',  ( 31.11269837220809364, 20.55634918610396866, 2.000000000000001776 ) ) ;
#20486 = LINE ( 'NONE', #48236, #52102 ) ;
#20487 = VERTEX_POINT ( 'NONE', #646 ) ;
#20488 = ORIENTED_EDGE ( 'NONE', *, *, #21051, .T. ) ;
#20489 = LINE ( 'NONE', #20156, #34987 ) ;
#20490 = PRESENTATION_STYLE_ASSIGNMENT (( #57446 ) ) ;
#20491 = CARTESIAN_POINT ( 'NONE',  ( -170.2951623264597458, 85.51757001115473145, -8.407365705316680149 ) ) ;
#20492 = ADVANCED_FACE ( 'NONE', ( #27362 ), #59375, .F. ) ;
#20493 = UNCERTAINTY_MEASURE_WITH_UNIT (LENGTH_MEASURE( 1.000000000000000082E-05 ), #46034, 'distance_accuracy_value', 'NONE');
#20494 = CONICAL_SURFACE ( 'NONE', #28381, 74.95140232871122521, 0.8777644062502172329 ) ;
#20495 = ADVANCED_FACE ( 'NONE', ( #38270 ), #32317, .T. ) ;
#20496 = DIRECTION ( 'NONE',  ( -1.000000000000000000, 0.000000000000000000, 0.000000000000000000 ) ) ;
#20497 = FACE_OUTER_BOUND ( 'NONE', #36320, .T. ) ;
#20498 = PLANE ( 'NONE',  #18890 ) ;
#20499 = CARTESIAN_POINT ( 'NONE',  ( 177.2011275744679324, 74.76848439756734876, -76.99017118353420130 ) ) ;
#20500 = AXIS2_PLACEMENT_3D ( 'NONE', #41062, #20288, #30502 ) ;
#20501 =( LENGTH_UNIT ( ) NAMED_UNIT ( * ) SI_UNIT ( .MILLI., .METRE. ) );
#20502 = CARTESIAN_POINT ( 'NONE',  ( -178.2427210808090479, 93.01567669683340966, -47.69625270927920013 ) ) ;
#20503 = LINE ( 'NONE', #14880, #48624 ) ;
#20504 = CARTESIAN_POINT ( 'NONE',  ( -452.6627218934859798, 395.0000000000064801, -136.4497041420121661 ) ) ;
#20505 = FACE_OUTER_BOUND ( 'NONE', #8522, .T. ) ;
#20506 = CARTESIAN_POINT ( 'NONE',  ( 16.78635691501517613, 6.000000000000000000, -14.43565316649550034 ) ) ;
#20507 = ORIENTED_EDGE ( 'NONE', *, *, #11642, .F. ) ;
#20508 = DIRECTION ( 'NONE',  ( -0.000000000000000000, -0.000000000000000000, 1.000000000000000000 ) ) ;
#20509 = DIRECTION ( 'NONE',  ( -0.8090169943749422332, -0.5877852522924802425, 0.000000000000000000 ) ) ;
#20510 = LINE ( 'NONE', #69032, #20654 ) ;
#20511 = CARTESIAN_POINT ( 'NONE',  ( 0.1230226671131348926, -25.12215469714591976, 3.061616997868437868E-16 ) ) ;
#20512 = FACE_OUTER_BOUND ( 'NONE', #21296, .T. ) ;
#20513 = CARTESIAN_POINT ( 'NONE',  ( -0.3234390959946896738, 7.525307474706613320, 91.58024944812166268 ) ) ;
#20514 = ORIENTED_EDGE ( 'NONE', *, *, #61635, .T. ) ;
#20515 = DIRECTION ( 'NONE',  ( -0.5508969814521065267, 0.8345732537212999791, 0.000000000000000000 ) ) ;
#20516 = CARTESIAN_POINT ( 'NONE',  ( 74.62299871641495486, 5.461138973199026303, 41.38025477438755928 ) ) ;
#20517 = EDGE_LOOP ( 'NONE', ( #12973, #57054, #56981 ) ) ;
#20518 = ORIENTED_EDGE ( 'NONE', *, *, #14609, .F. ) ;
#20519 = CARTESIAN_POINT ( 'NONE',  ( 38.76018190153303067, 9.341091693823624809, 83.62323164182360813 ) ) ;
#20520 = CARTESIAN_POINT ( 'NONE',  ( 39.40195752203892710, -170.0000000000000000, 64.25838489642696061 ) ) ;
#20521 = CARTESIAN_POINT ( 'NONE',  ( -5.767955557622883589E-14, -26.11269837220806522, 85.00100000000000477 ) ) ;
#20522 = VERTEX_POINT ( 'NONE', #27022 ) ;
#20523 = CARTESIAN_POINT ( 'NONE',  ( 112.3013380801406811, 400.0000000000077307, 101.0502958579874644 ) ) ;
#20524 = DIRECTION ( 'NONE',  ( -0.7071067811865477948, 2.775557561562891967E-17, -0.7071067811865473507 ) ) ;
#20525 = CARTESIAN_POINT ( 'NONE',  ( 35.65685430025423841, 7.951642554322390311, -9.758845964438441101 ) ) ;
#20526 = DIRECTION ( 'NONE',  ( 0.7071067811865474617, 0.7071067811865474617, 0.000000000000000000 ) ) ;
#20527 = CARTESIAN_POINT ( 'NONE',  ( -6.686525924292787693, 5.377136764700155780, -9.183279549040166856 ) ) ;
#20528 = CARTESIAN_POINT ( 'NONE',  ( 93.09528872995971938, 21.72934119836186184, 41.04433854226019918 ) ) ;
#20529 = EDGE_CURVE ( 'NONE', #4522, #58728, #59717, .T. ) ;
#20530 = EDGE_LOOP ( 'NONE', ( #38873, #49255 ) ) ;
#20532 = EDGE_CURVE ( 'NONE', #45386, #20826, #60068, .T. ) ;
#20531 = DIRECTION ( 'NONE',  ( 0.000000000000000000, -1.000000000000000000, 0.000000000000000000 ) ) ;
#20533 = CARTESIAN_POINT ( 'NONE',  ( 13.84120792123769128, 6.445822122644895735, 57.09985721401838532 ) ) ;
#20534 = CARTESIAN_POINT ( 'NONE',  ( 7.762887554996211747E-14, 46.66904755831208718, 2.000000000000001776 ) ) ;
#20535 = CARTESIAN_POINT ( 'NONE',  ( 197.4121679705848180, 98.46451029407253941, 34.92010124187357434 ) ) ;
#20536 = CARTESIAN_POINT ( 'NONE',  ( -71.21425542757401672, 20.68582981242713359, 92.51412664241122741 ) ) ;
#20538 = ORIENTED_EDGE ( 'NONE', *, *, #43359, .T. ) ;
#20537 = DIRECTION ( 'NONE',  ( -1.000000000000000000, 0.000000000000000000, 0.000000000000000000 ) ) ;
#20539 = ORIENTED_EDGE ( 'NONE', *, *, #21591, .F. ) ;
#20540 = AXIS2_PLACEMENT_3D ( 'NONE', #63404, #15207, #36669 ) ;
#20541 = ORIENTED_EDGE ( 'NONE', *, *, #16159, .T. ) ;
#20542 = AXIS2_PLACEMENT_3D ( 'NONE', #57252, #67467, #40715 ) ;
#20543 = CARTESIAN_POINT ( 'NONE',  ( 116.5100763992442836, 33.01539745157281658, -66.13966895617740249 ) ) ;
#20544 = CARTESIAN_POINT ( 'NONE',  ( 8.000000000000007105, 249.8719672152120381, 94.99999999999866418 ) ) ;
#20545 = CARTESIAN_POINT ( 'NONE',  ( 203.9181091394788155, 105.2759068139671683, -63.17048162308529413 ) ) ;
#20546 = EDGE_CURVE ( 'NONE', #23006, #41527, #65723, .T. ) ;
#20547 = CARTESIAN_POINT ( 'NONE',  ( -14.86595946518020739, 20.25193917588078563, 3.061616997868437868E-16 ) ) ;
#20548 = AXIS2_PLACEMENT_3D ( 'NONE', #42129, #42805, #53011 ) ;
#20549 = EDGE_CURVE ( 'NONE', #31339, #29832, #12859, .T. ) ;
#20550 = CARTESIAN_POINT ( 'NONE',  ( 204.6977192012829789, -170.0000000000000000, -16.98138044215791354 ) ) ;
#20551 = FACE_OUTER_BOUND ( 'NONE', #33044, .T. ) ;
#20552 = CARTESIAN_POINT ( 'NONE',  ( 21.64175105888077510, 7.766279958615638357, -92.00052844524886098 ) ) ;
#20553 = VECTOR ( 'NONE', #30303, 1000.000000000000000 ) ;
#20554 = CARTESIAN_POINT ( 'NONE',  ( -154.0718453320783681, 68.14976693162391541, -48.26858095381671632 ) ) ;
#20555 = EDGE_LOOP ( 'NONE', ( #31678, #53853, #57976, #67186 ) ) ;
#20556 = ORIENTED_EDGE ( 'NONE', *, *, #35558, .F. ) ;
#20557 = ADVANCED_FACE ( 'NONE', ( #2735, #24202, #66080, #17872, #62157, #67457, #3426, #19246, #7676, #35087, #40701, #51617, #39330, #60771, #45645, #2391, #12597, #34052, #66773, #55493, #34755, #7325, #28780, #18564, #40018, #8007, #67124, #18916, #19958, #9053, #14332, #57588, #68151, #32484, #36128, #5738 ), #4464, .F. ) ;
#20558 = DIRECTION ( 'NONE',  ( 1.000000000000000000, 0.000000000000000000, 0.000000000000000000 ) ) ;
#20559 = CARTESIAN_POINT ( 'NONE',  ( -85.95621526752229613, 26.32462117888285746, -44.39704732758743688 ) ) ;
#20560 = VECTOR ( 'NONE', #10344, 1000.000000000000000 ) ;
#20561 = CARTESIAN_POINT ( 'NONE',  ( 105.4886448962878660, 26.74369472770962020, 84.99022211379437408 ) ) ;
#20562 = EDGE_CURVE ( 'NONE', #31187, #7482, #36822, .T. ) ;
#20563 = CARTESIAN_POINT ( 'NONE',  ( -156.1477286774994298, 71.38742644140636173, 14.87326405071225111 ) ) ;
#20564 = FACE_BOUND ( 'NONE', #34264, .T. ) ;
#20565 = DIRECTION ( 'NONE',  ( 1.000000000000000000, 0.000000000000000000, 0.000000000000000000 ) ) ;
#20566 = LINE ( 'NONE', #31479, #67785 ) ;
#20567 = ORIENTED_EDGE ( 'NONE', *, *, #61583, .T. ) ;
#20568 = VERTEX_POINT ( 'NONE', #27194 ) ;
#20569 = ORIENTED_EDGE ( 'NONE', *, *, #15242, .T. ) ;
#20570 =( NAMED_UNIT ( * ) SI_UNIT ( $, .STERADIAN. ) SOLID_ANGLE_UNIT ( ) );
#20571 = DIRECTION ( 'NONE',  ( 0.000000000000000000, 1.000000000000000000, -0.000000000000000000 ) ) ;
#20572 = CARTESIAN_POINT ( 'NONE',  ( 105.2579757425518210, -21.94246241598115432, 1.618793836905549233 ) ) ;
#20573 = EDGE_CURVE ( 'NONE', #29607, #19726, #68810, .T. ) ;
#20574 = LINE ( 'NONE', #51904, #5693 ) ;
#20575 = EDGE_CURVE ( 'NONE', #66330, #15601, #4783, .T. ) ;
#20576 = CARTESIAN_POINT ( 'NONE',  ( -34.39099631177280969, 10.00000000000000000, -17.00000000000000711 ) ) ;
#20577 = EDGE_CURVE ( 'NONE', #12758, #56665, #62865, .T. ) ;
#20578 = ADVANCED_FACE ( 'NONE', ( #20625 ), #31206, .F. ) ;
#20579 = FACE_BOUND ( 'NONE', #51834, .T. ) ;
#20580 = CARTESIAN_POINT ( 'NONE',  ( 10.13846145460683168, 6.385368868491634764, -11.21767487839372279 ) ) ;
#20581 = CARTESIAN_POINT ( 'NONE',  ( 20.35964562795320276, 7.697260051881319676, 16.63611903121913826 ) ) ;
#20582 = CARTESIAN_POINT ( 'NONE',  ( 186.6054783416232112, 84.37128553200973613, 58.55262771499806718 ) ) ;
#20583 = CARTESIAN_POINT ( 'NONE',  ( -118.9468627709229196, 42.08677365399179848, 14.11409130223153774 ) ) ;
#20584 = CARTESIAN_POINT ( 'NONE',  ( 70.11438327604405174, 14.43198353181101368, -67.63221911897893790 ) ) ;
#20585 = CARTESIAN_POINT ( 'NONE',  ( 47.99999999999997158, 19.99999999999996447, 0.000000000000000000 ) ) ;
#20586 = CARTESIAN_POINT ( 'NONE',  ( 23.04797191264876588, 7.849755664016359269, -18.12056745251717871 ) ) ;
#20587 = DIRECTION ( 'NONE',  ( -0.000000000000000000, -0.000000000000000000, 1.000000000000000000 ) ) ;
#20588 = EDGE_LOOP ( 'NONE', ( #8378, #56058, #30527, #59030 ) ) ;
#20590 = CARTESIAN_POINT ( 'NONE',  ( 188.2988323915788840, 86.21831227955483712, 12.03370908765665170 ) ) ;
#20589 = AXIS2_PLACEMENT_3D ( 'NONE', #35462, #28806, #67827 ) ;
#20591 = APPLICATION_PROTOCOL_DEFINITION ( 'draft international standard', 'automotive_design', 1998, #10707 ) ;
#20592 = CARTESIAN_POINT ( 'NONE',  ( 174.6127059037622189, 72.30368563770912260, 32.97823390021704881 ) ) ;
#20593 = CARTESIAN_POINT ( 'NONE',  ( 0.000000000000000000, 0.000000000000000000, -7.000000000000000000 ) ) ;
#20594 = CARTESIAN_POINT ( 'NONE',  ( -104.1225399044495816, 34.86084180570099278, -49.78854814781668381 ) ) ;
#20595 = CARTESIAN_POINT ( 'NONE',  ( 182.7745872728868335, 81.77554423487160307, -36.36768213514671544 ) ) ;
#20596 = ORIENTED_EDGE ( 'NONE', *, *, #32094, .F. ) ;
#20597 = VECTOR ( 'NONE', #32601, 1000.000000000000000 ) ;
#20598 = ORIENTED_EDGE ( 'NONE', *, *, #49061, .T. ) ;
#20599 = LINE ( 'NONE', #37823, #53809 ) ;
#20600 = CIRCLE ( 'NONE', #17176, 65.00000000000000000 ) ;
#20601 = CARTESIAN_POINT ( 'NONE',  ( 175.0857681883884140, 72.74906374897946648, 94.99999999999866418 ) ) ;
#20602 = ORIENTED_EDGE ( 'NONE', *, *, #211, .T. ) ;
#20603 = VECTOR ( 'NONE', #17225, 1000.000000000000000 ) ;
#20604 = CARTESIAN_POINT ( 'NONE',  ( 112.1012908502484464, 29.75117929736500955, 56.68578264432271396 ) ) ;
#20605 = ORIENTED_EDGE ( 'NONE', *, *, #17546, .F. ) ;
#20606 = CARTESIAN_POINT ( 'NONE',  ( -419.7337897053564006, 395.0000000000001705, 80.62136366985323832 ) ) ;
#20607 = PLANE ( 'NONE',  #64326 ) ;
#20608 = B_SPLINE_CURVE_WITH_KNOTS ( 'NONE', 3,
 ( #53012, #9784, #4501, #36861, #69539, #58302 ),
 .UNSPECIFIED., .F., .F.,
 ( 4, 2, 4 ),
 ( 0.03218953612796877223, 0.06469846386257063764, 0.09720739159717248223 ),
 .UNSPECIFIED. ) ;
#20609 = DIRECTION ( 'NONE',  ( -0.000000000000000000, 1.000000000000000000, -0.000000000000000000 ) ) ;
#20610 = AXIS2_PLACEMENT_3D ( 'NONE', #10274, #16246, #32086 ) ;
#20611 = CARTESIAN_POINT ( 'NONE',  ( 158.2025576483179066, 58.22064626730321635, -89.81328548006500512 ) ) ;
#20612 = CARTESIAN_POINT ( 'NONE',  ( 86.62931800182293784, 19.42108912189597092, -50.82156419891174437 ) ) ;
#20614 = EDGE_LOOP ( 'NONE', ( #36570, #12598, #64745 ) ) ;
#20613 = CARTESIAN_POINT ( 'NONE',  ( 412.3372781065085633, 179.4906275429376024, -144.4497041420117682 ) ) ;
#20615 = CARTESIAN_POINT ( 'NONE',  ( -15.67984581961064450, 63.08044415722863363, 73.58025477438756923 ) ) ;
#20616 = VERTEX_POINT ( 'NONE', #67798 ) ;
#20617 = VERTEX_POINT ( 'NONE', #42089 ) ;
#20619 = ADVANCED_FACE ( 'NONE', ( #35789 ), #19597, .F. ) ;
#20618 = CARTESIAN_POINT ( 'NONE',  ( -119.6995109608660783, 42.54844499216735443, -19.80530726453818957 ) ) ;
#20620 = PLANE ( 'NONE',  #43711 ) ;
#20621 = CARTESIAN_POINT ( 'NONE',  ( -180.4654253355436992, 95.69358270527510513, -16.91796665578175052 ) ) ;
#20623 = ORIENTED_EDGE ( 'NONE', *, *, #52639, .F. ) ;
#20622 = LINE ( 'NONE', #42085, #34332 ) ;
#20624 = DIRECTION ( 'NONE',  ( 0.000000000000000000, 1.000000000000000000, -0.000000000000000000 ) ) ;
#20625 = FACE_OUTER_BOUND ( 'NONE', #22316, .T. ) ;
#20626 = VERTEX_POINT ( 'NONE', #47025 ) ;
#20627 = B_SPLINE_CURVE_WITH_KNOTS ( 'NONE', 3,
 ( #10260, #48560, #47532, #5339, #394, #26794, #48220, #45, #57771, #4310, #47201, #64419, #68659, #15202, #16230, #20469, #9930, #52817, #68995, #20820, #42279, #54549, #28887, #39098, #2157, #6012, #1811, #27472, #22208, #23610, #55253, #54899, #33116, #43997, #6723, #48915, #65475, #23265, #6376, #32762, #753, #11639, #28168, #27830 ),
 .UNSPECIFIED., .F., .F.,
 ( 4, 2, 2, 2, 2, 2, 2, 2, 2, 2, 2, 2, 2, 2, 2, 2, 2, 2, 2, 2, 2, 4 ),
 ( 0.02638217555535139064, 0.02805347641364862310, 0.02972477727194585209, 0.03139607813024308108, 0.03306737898854031354, 0.03390302941768895406, 0.03473867984683759458, 0.03640998070513487561, 0.03724563113428349531, 0.03808128156343210807, 0.03891693199258072083, 0.03975258242172934053, 0.04058823285087795329, 0.04142388328002657299, 0.04225953370917518576, 0.04309518413832380546, 0.04476648499662103098, 0.04643778585491824956, 0.04810908671321547508, 0.04978038757151270061, 0.05145168842980992613, 0.05312298928810715165 ),
 .UNSPECIFIED. ) ;
#20628 = CARTESIAN_POINT ( 'NONE',  ( -59.36813706141739289, 15.88103696331960890, -9.732856487797739931 ) ) ;
#20629 = ADVANCED_FACE ( 'NONE', ( #3767 ), #41411, .F. ) ;
#20630 = ADVANCED_FACE ( 'NONE', ( #36473 ), #57927, .F. ) ;
#20631 = EDGE_CURVE ( 'NONE', #51945, #17566, #52640, .T. ) ;
#20632 = CARTESIAN_POINT ( 'NONE',  ( -128.9843070188473177, 49.78011598923035308, -76.10710841746416122 ) ) ;
#20634 = CARTESIAN_POINT ( 'NONE',  ( -64.18058723658654685, 10.37664328995176888, 0.000000000000000000 ) ) ;
#20633 = VECTOR ( 'NONE', #17576, 1000.000000000000000 ) ;
#20635 = CARTESIAN_POINT ( 'NONE',  ( -131.6399667378751133, 51.62465701391629835, 16.12153412855955636 ) ) ;
#20636 = CARTESIAN_POINT ( 'NONE',  ( -96.76159256735191150, 30.06445763698411255, -64.25652613276936620 ) ) ;
#20637 = ORIENTED_EDGE ( 'NONE', *, *, #23312, .F. ) ;
#20638 = ORIENTED_EDGE ( 'NONE', *, *, #60121, .T. ) ;
#20639 = EDGE_CURVE ( 'NONE', #8876, #42865, #11020, .T. ) ;
#20640 = AXIS2_PLACEMENT_3D ( 'NONE', #11390, #49018, #1202 ) ;
#20641 = CARTESIAN_POINT ( 'NONE',  ( 185.1802655733641245, 82.84606286178498635, -64.27098958697960995 ) ) ;
#20642 = CARTESIAN_POINT ( 'NONE',  ( -166.2028193222419077, 79.74385139484274987, -45.12230103603525322 ) ) ;
#20643 = CARTESIAN_POINT ( 'NONE',  ( -125.8938041572051389, -170.0000000000000000, -42.41370389823394760 ) ) ;
#20644 = ADVANCED_FACE ( 'NONE', ( #45390 ), #45743, .F. ) ;
#20645 = AXIS2_PLACEMENT_3D ( 'NONE', #23971, #66903, #13420 ) ;
#20646 = CARTESIAN_POINT ( 'NONE',  ( 105.2529848321548229, 27.73895015262023023, -75.87138210954954332 ) ) ;
#20647 = CARTESIAN_POINT ( 'NONE',  ( -72.77296415263764118, 21.23032531836537018, 33.25313844162783283 ) ) ;
#20648 = CARTESIAN_POINT ( 'NONE',  ( 79.38459371357853911, 17.07499996355401350, 39.21690604770069655 ) ) ;
#20649 = CARTESIAN_POINT ( 'NONE',  ( 64.69738688745236743, 14.10375742873388027, -35.90769066738622683 ) ) ;
#20650 = VECTOR ( 'NONE', #12538, 1000.000000000000000 ) ;
#20651 = CARTESIAN_POINT ( 'NONE',  ( -118.4106078162223525, 42.93830006159888057, 38.68969896642374096 ) ) ;
#20652 = CARTESIAN_POINT ( 'NONE',  ( -137.3060924980642596, 138.4631249211268482, 10.00000000000000000 ) ) ;
#20653 = ORIENTED_EDGE ( 'NONE', *, *, #45268, .T. ) ;
#20655 = CARTESIAN_POINT ( 'NONE',  ( -108.6909373351217454, 36.15835109565441741, -19.59438147849856549 ) ) ;
#20654 = VECTOR ( 'NONE', #63785, 1000.000000000000000 ) ;
#20656 = ORIENTED_EDGE ( 'NONE', *, *, #51955, .T. ) ;
#20657 = CARTESIAN_POINT ( 'NONE',  ( 85.05043445648591671, 19.94792874060193100, -89.63462324852685015 ) ) ;
#20658 = VECTOR ( 'NONE', #12936, 1000.000000000000000 ) ;
#20659 = CARTESIAN_POINT ( 'NONE',  ( 81.04027388895740103, 18.64386073872848115, 69.08189960584093114 ) ) ;
#20660 = DIRECTION ( 'NONE',  ( -0.000000000000000000, -0.000000000000000000, -1.000000000000000000 ) ) ;
#20661 = DIRECTION ( 'NONE',  ( 0.000000000000000000, 0.000000000000000000, 1.000000000000000000 ) ) ;
#20662 = FACE_OUTER_BOUND ( 'NONE', #4988, .T. ) ;
#20663 = DIRECTION ( 'NONE',  ( 0.000000000000000000, 0.000000000000000000, -1.000000000000000000 ) ) ;
#20664 = CARTESIAN_POINT ( 'NONE',  ( 31.90217595456442368, 7.552213897210514837, -69.47029962155583860 ) ) ;
#20665 = CARTESIAN_POINT ( 'NONE',  ( -48.12872802574267439, 43.70867239603707333, 170.0000000000000000 ) ) ;
#20666 = VECTOR ( 'NONE', #32008, 1000.000000000000000 ) ;
#20667 = CARTESIAN_POINT ( 'NONE',  ( 0.000000000000000000, 0.000000000000000000, 43.58025477438756212 ) ) ;
#20668 = EDGE_CURVE ( 'NONE', #49023, #52035, #29494, .T. ) ;
#20669 = EDGE_LOOP ( 'NONE', ( #15832, #41567, #61041, #19896 ) ) ;
#20670 = FACE_OUTER_BOUND ( 'NONE', #6818, .T. ) ;
#20671 = ORIENTED_EDGE ( 'NONE', *, *, #8979, .T. ) ;
#20672 = CARTESIAN_POINT ( 'NONE',  ( 55.91133443650747381, 12.16263767238153726, 61.70338409828477921 ) ) ;
#20673 = CARTESIAN_POINT ( 'NONE',  ( 14.81290967676422454, 7.477658233646010011, -77.31609961694144317 ) ) ;
#20675 = EDGE_CURVE ( 'NONE', #40831, #988, #63182, .T. ) ;
#20674 = CARTESIAN_POINT ( 'NONE',  ( 5.737557066527558369, 188.0000000000000000, 2.275957463600585040 ) ) ;
#20676 = ADVANCED_BREP_SHAPE_REPRESENTATION ( '', ( #41290, #66832 ), #19752 ) ;
#20677 = LINE ( 'NONE', #15060, #16521 ) ;
#20678 = CARTESIAN_POINT ( 'NONE',  ( -55.90340863576495423, 14.91086451836061677, -88.94171492579830840 ) ) ;
#20679 = DIRECTION ( 'NONE',  ( -0.000000000000000000, -0.000000000000000000, 1.000000000000000000 ) ) ;
#20680 = CARTESIAN_POINT ( 'NONE',  ( 150.2941978382489197, 53.52137138947629325, -45.82117147580458294 ) ) ;
#20681 = ORIENTED_EDGE ( 'NONE', *, *, #66289, .T. ) ;
#20682 = DIRECTION ( 'NONE',  ( -1.000000000000000000, -2.206925868997230195E-16, -4.649058915617843013E-16 ) ) ;
#20683 = CARTESIAN_POINT ( 'NONE',  ( -149.9475539515598825, 65.87716206616011050, 72.56537183036279259 ) ) ;
#20684 = CARTESIAN_POINT ( 'NONE',  ( 0.000000000000000000, 8.000000000000000000, 0.000000000000000000 ) ) ;
#20685 = DIRECTION ( 'NONE',  ( 0.000000000000000000, -1.000000000000000000, 0.000000000000000000 ) ) ;
#20686 = CARTESIAN_POINT ( 'NONE',  ( -129.3970594949620079, 50.06339481638098476, -49.06162375837405420 ) ) ;
#20687 = ORIENTED_EDGE ( 'NONE', *, *, #34883, .T. ) ;
#20688 = DIRECTION ( 'NONE',  ( -0.000000000000000000, 1.000000000000000000, -0.000000000000000000 ) ) ;
#20689 = CARTESIAN_POINT ( 'NONE',  ( 94.02921784728462740, 22.08005910033070762, 65.30351108513647773 ) ) ;
#20690 = CARTESIAN_POINT ( 'NONE',  ( 200.8303160266298732, 102.8412051751308667, -10.54118182323272634 ) ) ;
#20691 = CARTESIAN_POINT ( 'NONE',  ( -146.9398925983290951, 62.03096887829646988, 84.84101267915092137 ) ) ;
#20692 = AXIS2_PLACEMENT_3D ( 'NONE', #44864, #67038, #24464 ) ;
#20693 = DIRECTION ( 'NONE',  ( 1.000000000000000000, 0.000000000000000000, -2.220446049250313081E-16 ) ) ;
#20694 = ORIENTED_EDGE ( 'NONE', *, *, #45759, .T. ) ;
#20695 = CARTESIAN_POINT ( 'NONE',  ( 198.2545923567585362, 97.90679023593578734, 32.85835692444881317 ) ) ;
#20696 = FACE_OUTER_BOUND ( 'NONE', #18082, .T. ) ;
#20697 = VECTOR ( 'NONE', #42304, 1000.000000000000000 ) ;
#20698 = CARTESIAN_POINT ( 'NONE',  ( 188.4920037102894526, 87.93425473911918289, 38.01812594245322430 ) ) ;
#20699 = CARTESIAN_POINT ( 'NONE',  ( 164.0105905242218398, 64.23277447906893656, 6.384859283288245813 ) ) ;
#20700 = CARTESIAN_POINT ( 'NONE',  ( -101.8140949286062238, 33.67224128592400945, 45.51907450641512298 ) ) ;
#20701 = B_SPLINE_CURVE_WITH_KNOTS ( 'NONE', 3,
 ( #25187, #67400, #19546, #21193 ),
 .UNSPECIFIED., .F., .F.,
 ( 4, 4 ),
 ( 0.1259919275528358362, 0.1829744153748746882 ),
 .UNSPECIFIED. ) ;
#20702 = VECTOR ( 'NONE', #44644, 1000.000000000000000 ) ;
#20703 = ORIENTED_EDGE ( 'NONE', *, *, #288, .F. ) ;
#20704 = CIRCLE ( 'NONE', #60005, 25.12245591505646303 ) ;
#20705 = EDGE_CURVE ( 'NONE', #2210, #37473, #34853, .T. ) ;
#20706 = CARTESIAN_POINT ( 'NONE',  ( 173.8623159076319382, 72.97967239795016781, 61.60855493920503534 ) ) ;
#20707 = VECTOR ( 'NONE', #3487, 1000.000000000000000 ) ;
#20708 = ORIENTED_EDGE ( 'NONE', *, *, #5773, .F. ) ;
#20710 = ADVANCED_FACE ( 'NONE', ( #50667 ), #40121, .F. ) ;
#20709 = CARTESIAN_POINT ( 'NONE',  ( -109.6660553119435377, 36.69391917620600196, -41.18609763443000560 ) ) ;
#20711 = CARTESIAN_POINT ( 'NONE',  ( 64.69649025047539226, 13.06878919510322312, -77.37851346046119261 ) ) ;
#20712 = VECTOR ( 'NONE', #47007, 1000.000000000000000 ) ;
#20713 = DIRECTION ( 'NONE',  ( 0.000000000000000000, 0.000000000000000000, 1.000000000000000000 ) ) ;
#20715 = VERTEX_POINT ( 'NONE', #3871 ) ;
#20714 = DIRECTION ( 'NONE',  ( -0.6910626489868685329, 0.7227948638273878901, 0.000000000000000000 ) ) ;
#20716 = CARTESIAN_POINT ( 'NONE',  ( -174.7800083645696532, 88.99302808536934606, 30.99548995540544638 ) ) ;
#20717 = CARTESIAN_POINT ( 'NONE',  ( -5.000000000000026645, -15.55634918610403616, 85.00100000000000477 ) ) ;
#20718 = CARTESIAN_POINT ( 'NONE',  ( 114.6659427952414347, 32.10199811723106933, -37.34674998934434598 ) ) ;
#20719 = VERTEX_POINT ( 'NONE', #62620 ) ;
#20720 = B_SPLINE_CURVE_WITH_KNOTS ( 'NONE', 3,
 ( #67513, #43173, #37559, #58319, #57988, #64650, #69222, #52694, #37211, #16105, #53379, #10138, #4861, #15764, #48431, #63952, #25650, #59012, #9807, #42154, #31597, #68544, #10828, #268, #53727, #58662, #36884, #32297, #15077, #10479, #5549, #27002, #31267, #21723, #16457, #37912, #36539, #53037, #68869, #4521, #41814, #25984, #59357 ),
 .UNSPECIFIED., .F., .F.,
 ( 4, 2, 2, 2, 2, 2, 2, 2, 2, 2, 2, 1, 2, 2, 2, 2, 2, 2, 2, 2, 2, 4 ),
 ( 0.02515559250233026511, 0.02674001423437960545, 0.02753222510040427562, 0.02832443596642894579, 0.02990885769847835204, 0.03149327943052775830, 0.03307770116257716109, 0.03386991202860185901, 0.03466212289462655693, 0.03624654462667591809, 0.03703875549270058826, 0.03783096635872525842, 0.03862317722474992859, 0.03941538809077459876, 0.04099980982282395992, 0.04258423155487331413, 0.04337644242089799818, 0.04416865328692266834, 0.04575307501897196011, 0.04733749675102125187, 0.04892191848307053670, 0.05050634021511982846 ),
 .UNSPECIFIED. ) ;
#20721 = CARTESIAN_POINT ( 'NONE',  ( 447.3372781065083927, 395.0000000000043769, 103.5502958579838264 ) ) ;
#20722 = EDGE_CURVE ( 'NONE', #54708, #12059, #35881, .T. ) ;
#20723 = DIRECTION ( 'NONE',  ( -0.7071067811865473507, -1.232595164407830946E-32, 0.7071067811865476838 ) ) ;
#20724 = CARTESIAN_POINT ( 'NONE',  ( 140.9169160367233076, 45.85398962664667977, 66.43883726660729394 ) ) ;
#20725 = CARTESIAN_POINT ( 'NONE',  ( -171.0758681675584683, 84.87997360100517596, 45.54985601431179276 ) ) ;
#20726 = CARTESIAN_POINT ( 'NONE',  ( -31.43908319763709969, 9.591432048623762086, -62.16174795566551836 ) ) ;
#20727 = EDGE_CURVE ( 'NONE', #25681, #40373, #15114, .T. ) ;
#20728 = CARTESIAN_POINT ( 'NONE',  ( 87.11239765416381431, 20.65008247340817604, 44.71208757247934074 ) ) ;
#20729 = ORIENTED_EDGE ( 'NONE', *, *, #1666, .T. ) ;
#20731 = EDGE_CURVE ( 'NONE', #48266, #33282, #246, .T. ) ;
#20730 = CARTESIAN_POINT ( 'NONE',  ( 230.9999999999999432, -57.00000000000007816, -2.000000000000000000 ) ) ;
#20732 = ORIENTED_EDGE ( 'NONE', *, *, #34405, .T. ) ;
#20733 = CARTESIAN_POINT ( 'NONE',  ( 35.54014968547571129, -66.04466488925490353, 43.58025477438756212 ) ) ;
#20734 = CARTESIAN_POINT ( 'NONE',  ( -57.54234552050026963, 15.36296824409563477, 84.42464098905453795 ) ) ;
#20735 = LINE ( 'NONE', #42192, #25687 ) ;
#20736 = CARTESIAN_POINT ( 'NONE',  ( -156.9910258076866114, 70.79617246506502681, -69.73103036517183284 ) ) ;
#20737 = CARTESIAN_POINT ( 'NONE',  ( -4.999999999999922728, 46.66904755831208718, 2.000000000000000000 ) ) ;
#20738 = FACE_OUTER_BOUND ( 'NONE', #31244, .T. ) ;
#20739 = CARTESIAN_POINT ( 'NONE',  ( 206.7099580236350107, 109.1417833474364585, -36.58928946998770471 ) ) ;
#20740 = CARTESIAN_POINT ( 'NONE',  ( -31.11269837220812207, -31.11269837220801193, 85.00100000000000477 ) ) ;
#20741 = ORIENTED_EDGE ( 'NONE', *, *, #54438, .F. ) ;
#20742 = CIRCLE ( 'NONE', #30901, 5.000000000000000888 ) ;
#20743 = DIRECTION ( 'NONE',  ( -0.000000000000000000, 0.000000000000000000, -1.000000000000000000 ) ) ;
#20744 = ORIENTED_EDGE ( 'NONE', *, *, #6603, .T. ) ;
#20745 = CARTESIAN_POINT ( 'NONE',  ( -452.6627218934913230, 399.9999999999997726, 113.5502958579881891 ) ) ;
#20746 = CARTESIAN_POINT ( 'NONE',  ( 205.5004956747122833, 107.4493581495447785, -78.13833085385769550 ) ) ;
#20747 = CARTESIAN_POINT ( 'NONE',  ( 55.76298701799386492, 11.10663440745151398, -68.09037621486923797 ) ) ;
#20748 = CARTESIAN_POINT ( 'NONE',  ( 154.4165763529819628, 225.8585178651493663, 129.0000000000000000 ) ) ;
#20749 = CARTESIAN_POINT ( 'NONE',  ( 0.000000000000000000, 0.000000000000000000, -0.5776712190230133270 ) ) ;
#20750 = FACE_OUTER_BOUND ( 'NONE', #38432, .T. ) ;
#20751 = CARTESIAN_POINT ( 'NONE',  ( 161.1112535418156710, 61.83422628788726882, -63.90774190170210289 ) ) ;
#20752 = ORIENTED_EDGE ( 'NONE', *, *, #8743, .T. ) ;
#20753 = CARTESIAN_POINT ( 'NONE',  ( 209.3223706822284100, 0.000000000000000000, 277.8007638641562380 ) ) ;
#20754 = CARTESIAN_POINT ( 'NONE',  ( 64.99999999999998579, 0.000000000000000000, -1.127570259384924454E-14 ) ) ;
#20755 = VERTEX_POINT ( 'NONE', #40805 ) ;
#20756 = ADVANCED_FACE ( 'NONE', ( #3518 ), #67900, .F. ) ;
#20757 = VERTEX_POINT ( 'NONE', #26362 ) ;
#20758 = CIRCLE ( 'NONE', #43183, 19.99999999999998934 ) ;
#20759 = DIRECTION ( 'NONE',  ( -1.000000000000000000, 0.000000000000000000, 0.000000000000000000 ) ) ;
#20760 = FACE_OUTER_BOUND ( 'NONE', #16623, .T. ) ;
#20761 = DIRECTION ( 'NONE',  ( -0.000000000000000000, 0.000000000000000000, -1.000000000000000000 ) ) ;
#20762 = FILL_AREA_STYLE_COLOUR ( '', #19310 ) ;
#20763 = VECTOR ( 'NONE', #3049, 1000.000000000000114 ) ;
#20764 = DIRECTION ( 'NONE',  ( 1.000000000000000000, 0.000000000000000000, 0.000000000000000000 ) ) ;
#20765 = ORIENTED_EDGE ( 'NONE', *, *, #17307, .F. ) ;
#20766 = CARTESIAN_POINT ( 'NONE',  ( 0.000000000000000000, 0.000000000000000000, 30.00000000000000000 ) ) ;
#20767 = ORIENTED_EDGE ( 'NONE', *, *, #46997, .T. ) ;
#20768 = CARTESIAN_POINT ( 'NONE',  ( 205.0999694062793992, 106.8955893716604919, 2.363170148305747009 ) ) ;
#20769 = DIRECTION ( 'NONE',  ( 0.000000000000000000, -0.000000000000000000, -1.000000000000000000 ) ) ;
#20770 = CARTESIAN_POINT ( 'NONE',  ( -3.255961059272213465, 7.643453059677441708, 70.42757466837964841 ) ) ;
#20771 = CARTESIAN_POINT ( 'NONE',  ( -3.841371665203041630E-11, 0.000000000000000000, 0.000000000000000000 ) ) ;
#20772 = B_SPLINE_CURVE_WITH_KNOTS ( 'NONE', 3,
 ( #63677, #36601, #19727, #67930, #41185, #62647, #41875, #14454, #30289, #57362, #58383, #68933, #53093, #15491, #14103, #42217, #35909, #36943, #25367, #51738, #58049, #30633, #41529, #10192, #8839, #69287, #3543, #40832, #52079, #62291, #3899, #68271, #35563, #57022, #47139, #57708, #62981, #20407, #9521, #36252, #52427, #4250, #25710, #68601 ),
 .UNSPECIFIED., .F., .F.,
 ( 4, 2, 2, 2, 2, 2, 2, 2, 2, 2, 2, 2, 2, 2, 2, 2, 2, 2, 2, 2, 2, 4 ),
 ( 1.387778780781445676E-17, 0.003433139681083872442, 0.004291424601354786560, 0.005149709521625698942, 0.006866279362167435237, 0.007724564282438299914, 0.008582849202709161990, 0.009441134122980024065, 0.01029941904325088614, 0.01201598888379266233, 0.01373255872433443679, 0.01459084364460531621, 0.01544912856487619217, 0.01630741348514706812, 0.01716569840541794581, 0.01888226824595971506, 0.02059883808650148432, 0.02145712300677240711, 0.02231540792704332990, 0.02403197776758510262, 0.02574854760812687188, 0.02746511744866864460 ),
 .UNSPECIFIED. ) ;
#20773 = ORIENTED_EDGE ( 'NONE', *, *, #35345, .T. ) ;
#20774 = EDGE_LOOP ( 'NONE', ( #6609, #50155, #54092, #64691 ) ) ;
#20775 = CARTESIAN_POINT ( 'NONE',  ( 113.0516338319616665, -21.63887047452759305, 3.974065166673112603 ) ) ;
#20776 = CARTESIAN_POINT ( 'NONE',  ( -120.2269354400981598, 44.05870085693242544, 86.88615135046399018 ) ) ;
#20777 = CARTESIAN_POINT ( 'NONE',  ( -78.66644367742111399, -170.0000000000000000, -61.96000122218157458 ) ) ;
#20778 = LINE ( 'NONE', #31682, #5186 ) ;
#20779 = PLANE ( 'NONE',  #28501 ) ;
#20780 = CARTESIAN_POINT ( 'NONE',  ( 17.10503398861595770, 7.553194056991637595, 83.81298706601685922 ) ) ;
#20781 = ORIENTED_EDGE ( 'NONE', *, *, #18364, .F. ) ;
#20782 = CARTESIAN_POINT ( 'NONE',  ( -86.05211524933166345, 26.36495896184001708, -95.00000000000133582 ) ) ;
#20783 = CARTESIAN_POINT ( 'NONE',  ( -94.78109144324895396, 29.13179392050636807, 64.57839755988879915 ) ) ;
#20784 = ADVANCED_FACE ( 'NONE', ( #63984 ), #43899, .T. ) ;
#20785 = ORIENTED_EDGE ( 'NONE', *, *, #29169, .T. ) ;
#20786 = CARTESIAN_POINT ( 'NONE',  ( -86.10361028793437299, 25.29528064050657576, 10.07196939449881512 ) ) ;
#20787 = ORIENTED_EDGE ( 'NONE', *, *, #25121, .T. ) ;
#20788 = AXIS2_PLACEMENT_3D ( 'NONE', #40529, #3943, #41914 ) ;
#20789 = EDGE_CURVE ( 'NONE', #21469, #63543, #55567, .T. ) ;
#20790 = ORIENTED_EDGE ( 'NONE', *, *, #5904, .T. ) ;
#20792 = EDGE_CURVE ( 'NONE', #48097, #8872, #64290, .T. ) ;
#20791 = MANIFOLD_SOLID_BREP ( 'Shell1', #42893 ) ;
#20793 = ORIENTED_EDGE ( 'NONE', *, *, #53042, .T. ) ;
#20794 = CARTESIAN_POINT ( 'NONE',  ( 8.670103207226933506, 6.377073801252349128, -45.43205147905846530 ) ) ;
#20795 = CARTESIAN_POINT ( 'NONE',  ( -173.5394735271661375, 87.59446374803708579, 57.66624519710470054 ) ) ;
#20796 = CARTESIAN_POINT ( 'NONE',  ( 22.53041628628729498, 6.810083298012986397, 13.99219147001824126 ) ) ;
#20797 = CIRCLE ( 'NONE', #36576, 245.3095347406803342 ) ;
#20798 = AXIS2_PLACEMENT_3D ( 'NONE', #51587, #14973, #24853 ) ;
#20799 = VERTEX_POINT ( 'NONE', #47799 ) ;
#20800 = AXIS2_PLACEMENT_3D ( 'NONE', #31615, #44940, #2386 ) ;
#20801 = CARTESIAN_POINT ( 'NONE',  ( -36.44526830929234507, 10.46676546085014969, 85.81153421141065962 ) ) ;
#20802 = DIRECTION ( 'NONE',  ( -0.5508969814520944253, -0.8345732537213078617, 0.000000000000000000 ) ) ;
#20803 = VECTOR ( 'NONE', #54886, 1000.000000000000000 ) ;
#20804 = CARTESIAN_POINT ( 'NONE',  ( -42.02161712141799654, -26.09918303830819042, 30.00000000000000000 ) ) ;
#20805 = EDGE_CURVE ( 'NONE', #2387, #50015, #54446, .T. ) ;
#20806 = CARTESIAN_POINT ( 'NONE',  ( 103.1567541746301941, 25.73937982110323119, -45.93086059415202982 ) ) ;
#20807 = CARTESIAN_POINT ( 'NONE',  ( 138.5684226926155702, 45.53585076428269218, -64.51278046548689815 ) ) ;
#20809 = EDGE_CURVE ( 'NONE', #25475, #33258, #26701, .T. ) ;
#20808 = CARTESIAN_POINT ( 'NONE',  ( -142.0860844253782886, 59.41107357617637064, -70.27677374158945156 ) ) ;
#20810 = VERTEX_POINT ( 'NONE', #22109 ) ;
#20811 = CARTESIAN_POINT ( 'NONE',  ( 24.79066879238609644, 3.228426989449657114, 0.000000000000000000 ) ) ;
#20812 = CARTESIAN_POINT ( 'NONE',  ( -83.69370847062539553, 25.38703975185371675, -75.03095722555288205 ) ) ;
#20813 = CARTESIAN_POINT ( 'NONE',  ( 173.9405361758639117, 73.05302209498822208, 12.26640283032960532 ) ) ;
#20814 = CARTESIAN_POINT ( 'NONE',  ( -118.5151419614604436, 43.00218563933588456, -41.04416846843501787 ) ) ;
#20815 = CARTESIAN_POINT ( 'NONE',  ( -79.61235761536667610, 23.76245710489569518, 3.618273565636886069 ) ) ;
#20816 = CARTESIAN_POINT ( 'NONE',  ( 154.4165763529819628, 225.8585178651493663, 108.9999999999999858 ) ) ;
#20817 = CARTESIAN_POINT ( 'NONE',  ( 33.34472344659697285, 7.698735568503753512, -92.36667317427755108 ) ) ;
#20818 = CARTESIAN_POINT ( 'NONE',  ( 197.3914575603701280, 98.43856781875066986, 92.14791230178799708 ) ) ;
#20819 = CARTESIAN_POINT ( 'NONE',  ( 70.45466089417031696, 14.52203022703029056, 11.45482948366315945 ) ) ;
#20820 = CARTESIAN_POINT ( 'NONE',  ( 164.8407099662995563, 63.61629583487395223, 8.649268911586283082 ) ) ;
#20822 = DIRECTION ( 'NONE',  ( 0.000000000000000000, 0.000000000000000000, 1.000000000000000000 ) ) ;
#20821 = B_SPLINE_CURVE_WITH_KNOTS ( 'NONE', 3,
 ( #39325, #1337, #34410, #28774, #60767, #12592, #61475, #23499, #11883, #34048, #43878, #7672, #33707, #66425, #54791, #55853, #55489, #55135, #17505, #2731, #38621, #28060, #65363, #61122, #50917, #38981, #50567, #18217, #22791, #17146, #34750, #60064, #23847, #6613, #60428, #12244, #13294, #56186, #44231, #45286, #33361, #66769, #18560, #49499, #6960 ),
 .UNSPECIFIED., .F., .F.,
 ( 4, 2, 2, 1, 2, 2, 2, 2, 2, 2, 2, 2, 2, 2, 2, 2, 2, 2, 2, 2, 2, 2, 4 ),
 ( 0.02346464386237015476, 0.02493212228186624663, 0.02566586149161429603, 0.02639960070136234196, 0.02713333991111039137, 0.02786707912085843730, 0.02933455754035455693, 0.03006829675010262021, 0.03080203595985067655, 0.03226951437934676148, 0.03300325358909482476, 0.03373699279884288804, 0.03520447121833901460, 0.03667194963783514117, 0.03740568884758317669, 0.03813942805733121916, 0.03960690647682733878, 0.04107438489632345840, 0.04254186331581957803, 0.04327560252556764131, 0.04400934173531570459, 0.04547682015481182422, 0.04694429857430794384 ),
 .UNSPECIFIED. ) ;
#20823 = ORIENTED_EDGE ( 'NONE', *, *, #2613, .F. ) ;
#20824 = CONTEXT_DEPENDENT_SHAPE_REPRESENTATION ( #62909, #60830 ) ;
#20825 = CARTESIAN_POINT ( 'NONE',  ( -52.90268453104089730, 15.15480697857591252, 84.31435017214288052 ) ) ;
#20826 = VERTEX_POINT ( 'NONE', #4896 ) ;
#20827 = DIRECTION ( 'NONE',  ( -1.000000000000000000, 0.000000000000000000, 0.000000000000000000 ) ) ;
#20828 = ORIENTED_EDGE ( 'NONE', *, *, #47858, .T. ) ;
#20829 = CARTESIAN_POINT ( 'NONE',  ( 23.03546163277112768, 7.848986635155163150, -67.91707449678644082 ) ) ;
#20830 = DIRECTION ( 'NONE',  ( 1.697894969632809662E-16, -1.110223024625155801E-16, 1.000000000000000000 ) ) ;
#20831 = CARTESIAN_POINT ( 'NONE',  ( 0.000000000000000000, 0.000000000000000000, 0.000000000000000000 ) ) ;
#20832 = CARTESIAN_POINT ( 'NONE',  ( 66.72974708835175761, 13.56459745268606554, -22.91045958329191734 ) ) ;
#20833 = CARTESIAN_POINT ( 'NONE',  ( 209.9999999999999716, -57.00000000000007816, 93.99999999999998579 ) ) ;
#20834 = CARTESIAN_POINT ( 'NONE',  ( -50.53243683205840853, 14.55237037207940531, -63.55645086763099272 ) ) ;
#20835 = CARTESIAN_POINT ( 'NONE',  ( 154.4550750032601627, 55.34393534448157226, -36.75316982753754758 ) ) ;
#20836 = CARTESIAN_POINT ( 'NONE',  ( -440.1146514826276075, 388.0000000000064801, -133.9016337311480243 ) ) ;
#20837 = CARTESIAN_POINT ( 'NONE',  ( -118.9668643994984052, 43.27909474462862960, -12.68187660284936413 ) ) ;
#20838 = ORIENTED_EDGE ( 'NONE', *, *, #36474, .T. ) ;
#20839 = VERTEX_POINT ( 'NONE', #21757 ) ;
#20840 = VECTOR ( 'NONE', #45212, 1000.000000000000000 ) ;
#20841 = DIRECTION ( 'NONE',  ( 0.4112000000000004540, 0.9115451497320358198, -0.000000000000000000 ) ) ;
#20842 = CARTESIAN_POINT ( 'NONE',  ( 444.9999999999999432, -35.00000000000000000, -2.000000000000000000 ) ) ;
#20843 = CARTESIAN_POINT ( 'NONE',  ( 15.55634918610403261, -3.079134169858832593E-14, 0.000000000000000000 ) ) ;
#20844 = VECTOR ( 'NONE', #62363, 1000.000000000000114 ) ;
#20845 = CARTESIAN_POINT ( 'NONE',  ( 447.3372781065085633, 400.0000000000000568, -146.4497041420117966 ) ) ;
#20846 = DIRECTION ( 'NONE',  ( 0.000000000000000000, 0.000000000000000000, 1.000000000000000000 ) ) ;
#20847 = VECTOR ( 'NONE', #50536, 1000.000000000000000 ) ;
#20848 = VECTOR ( 'NONE', #10993, 1000.000000000000000 ) ;
#20849 = CARTESIAN_POINT ( 'NONE',  ( 184.3879440808140657, 83.47316703125159165, -10.14386913531070711 ) ) ;
#20850 = CARTESIAN_POINT ( 'NONE',  ( 174.1364721914477514, 71.85829564941447245, -73.40901879464566093 ) ) ;
#20851 = DIRECTION ( 'NONE',  ( -0.7071067811865507924, 8.659560562354892183E-17, -0.7071067811865441310 ) ) ;
#20852 = LINE ( 'NONE', #42312, #16117 ) ;
#20854 = CARTESIAN_POINT ( 'NONE',  ( 11.30618213853385967, 74.15344055032308290, 170.0000000000000000 ) ) ;
#20853 = B_SPLINE_CURVE_WITH_KNOTS ( 'NONE', 3,
 ( #68452, #69473, #21292, #57894, #42739, #20260, #31179, #52606, #49740, #32202, #174, #54678, #60314, #38154, #32885, #21630, #26913, #43077, #17038, #28301, #23038, #1570, #53633, #6506, #11772, #48339, #64550, #22679, #17396, #44484, #55027, #33597, #65964, #59594, #17762, #65603, #16699, #16358, #39216, #27600, #11073, #64902, #27954, #49041, #5796 ),
 .UNSPECIFIED., .F., .F.,
 ( 4, 2, 2, 2, 2, 2, 2, 2, 2, 2, 2, 2, 2, 1, 2, 2, 2, 2, 2, 2, 2, 2, 4 ),
 ( 0.02352719711393053484, 0.02499986300757012572, 0.02573619595438991076, 0.02647252890120969232, 0.02794519479484923810, 0.02941786068848878388, 0.03015419363530857239, 0.03089052658212835742, 0.03236319247576796565, 0.03309952542258779579, 0.03383585836940762592, 0.03530852426304727926, 0.03604485720986710939, 0.03678119015668693953, 0.03751752310350676967, 0.03825385605032659980, 0.03972652194396622538, 0.04119918783760584402, 0.04267185373124546266, 0.04340818667806528586, 0.04414451962488510905, 0.04561718551852474157, 0.04708985141216438797 ),
 .UNSPECIFIED. ) ;
#20855 = DIRECTION ( 'NONE',  ( -0.000000000000000000, -0.000000000000000000, -1.000000000000000000 ) ) ;
#20856 = AXIS2_PLACEMENT_3D ( 'NONE', #4169, #3474, #63258 ) ;
#20857 = CARTESIAN_POINT ( 'NONE',  ( -422.6627218934914936, 394.9999999999956799, 83.55029585799226766 ) ) ;
#20858 = VECTOR ( 'NONE', #12508, 1000.000000000000000 ) ;
#20859 = AXIS2_PLACEMENT_3D ( 'NONE', #58700, #10518, #10867 ) ;
#20860 = EDGE_LOOP ( 'NONE', ( #31174, #15858, #11109, #49182 ) ) ;
#20861 = CARTESIAN_POINT ( 'NONE',  ( -173.1211646369891355, 87.12891641440857882, 72.66624519710475738 ) ) ;
#20862 = DIRECTION ( 'NONE',  ( -1.000000000000000000, 0.000000000000000000, 0.000000000000000000 ) ) ;
#20863 = CARTESIAN_POINT ( 'NONE',  ( 154.4435090467313785, 56.59612921827832110, 70.61996015326239728 ) ) ;
#20864 = CARTESIAN_POINT ( 'NONE',  ( -142.6736406357357794, 59.87555372585265445, 94.99999999999866418 ) ) ;
#20865 = DIRECTION ( 'NONE',  ( -0.000000000000000000, 1.000000000000000000, -0.000000000000000000 ) ) ;
#20866 = CARTESIAN_POINT ( 'NONE',  ( -0.7847733590455667763, 7.541558926123923534, 88.69980130832604459 ) ) ;
#20867 = VERTEX_POINT ( 'NONE', #69260 ) ;
#20868 = DIRECTION ( 'NONE',  ( 1.000000000000000000, 0.000000000000000000, -0.000000000000000000 ) ) ;
#20869 = CARTESIAN_POINT ( 'NONE',  ( 0.08224679563971343255, 7.710515798486365036, 2.644994884459111351 ) ) ;
#20870 = EDGE_CURVE ( 'NONE', #69450, #12534, #37360, .T. ) ;
#20871 = ORIENTED_EDGE ( 'NONE', *, *, #44553, .F. ) ;
#20872 = ORIENTED_EDGE ( 'NONE', *, *, #13906, .T. ) ;
#20873 = CARTESIAN_POINT ( 'NONE',  ( 46.86855270197328593, 10.51779196975806840, 91.88407132189860249 ) ) ;
#20874 = LINE ( 'NONE', #42333, #16429 ) ;
#20875 = ADVANCED_FACE ( 'NONE', ( #64679 ), #43550, .F. ) ;
#20876 = CARTESIAN_POINT ( 'NONE',  ( 135.3597199823648225, 43.52062712031425207, -89.85493311428349728 ) ) ;
#20877 = ORIENTED_EDGE ( 'NONE', *, *, #67680, .T. ) ;
#20878 = B_SPLINE_CURVE_WITH_KNOTS ( 'NONE', 3,
 ( #3566, #61273, #13097, #45790, #18713, #40857, #30308, #18361, #8509, #40165, #29960, #51422, #62309, #67598, #34563, #7478, #46470, #66918, #57044, #67949, #19394, #29266, #8858, #39468, #2534, #12744, #66570, #28928, #39818, #50714, #58073, #10564, #9891, #25729, #36624, #19745, #48182, #63003, #26066, #68955, #9192, #36967, #47494, #31002, #57381 ),
 .UNSPECIFIED., .F., .F.,
 ( 4, 2, 2, 2, 2, 2, 2, 2, 2, 2, 2, 2, 2, 1, 2, 2, 2, 2, 2, 2, 2, 2, 4 ),
 ( 0.02356759485890611364, 0.02503765354686408873, 0.02577268289084306413, 0.02650771223482203606, 0.02797777092277998687, 0.02944782961073793767, 0.03018285895471693736, 0.03091788829869593358, 0.03238794698665397459, 0.03312297633063299857, 0.03385800567461202254, 0.03532806436257011212, 0.03606309370654915691, 0.03679812305052820171, 0.03753315239450724650, 0.03826818173848629129, 0.03973824042644441557, 0.04120829911440254678, 0.04267835780236067800, 0.04341338714633974361, 0.04414841649031881615, 0.04561847517827696125, 0.04708853386623510634 ),
 .UNSPECIFIED. ) ;
#20879 = DIRECTION ( 'NONE',  ( -1.000000000000000000, 0.000000000000000000, 0.000000000000000000 ) ) ;
#20880 = CARTESIAN_POINT ( 'NONE',  ( -5.401648928593173693, 6.744888135494081283, 17.88536589262118071 ) ) ;
#20881 = ADVANCED_FACE ( 'NONE', ( #53409 ), #59388, .T. ) ;
#20882 = CARTESIAN_POINT ( 'NONE',  ( 34.84173759613683075, 7.859847277726514925, -10.30082682987506715 ) ) ;
#20883 = CARTESIAN_POINT ( 'NONE',  ( 174.1348882614952629, 73.23561817543362906, -40.88960443691671998 ) ) ;
#20884 = CARTESIAN_POINT ( 'NONE',  ( 164.2089238023960718, 63.08603653844363635, 87.28623637339566699 ) ) ;
#20885 = LINE ( 'NONE', #25835, #568 ) ;
#20886 = PRODUCT_DEFINITION_SHAPE ( 'NONE', 'NONE',  #57716 ) ;
#20887 = ORIENTED_EDGE ( 'NONE', *, *, #12473, .T. ) ;
#20888 = CARTESIAN_POINT ( 'NONE',  ( -2.000000000000000000, 0.000000000000000000, -0.000000000000000000 ) ) ;
#20889 = AXIS2_PLACEMENT_3D ( 'NONE', #67985, #52812, #31379 ) ;
#20890 = CARTESIAN_POINT ( 'NONE',  ( 417.3372781065086201, 399.9999999999998863, 108.5502958579882034 ) ) ;
#20891 = B_SPLINE_CURVE_WITH_KNOTS ( 'NONE', 3,
 ( #58434, #47882, #69346, #35623, #57075, #27464, #59817, #11632, #10591, #43288, #32063, #16912, #65115, #38 ),
 .UNSPECIFIED., .F., .F.,
 ( 4, 2, 2, 2, 2, 2, 4 ),
 ( 0.000000000000000000, 0.001279364114800584686, 0.002558728229601169371, 0.003838092344401753623, 0.005117456459202338742, 0.007676184688803516787, 0.01023491291840469483 ),
 .UNSPECIFIED. ) ;
#20893 = EDGE_CURVE ( 'NONE', #17738, #53526, #21600, .T. ) ;
#20892 = CARTESIAN_POINT ( 'NONE',  ( 11.21312910819262676, 7.403355431336992254, 31.55132192236441568 ) ) ;
#20894 = CARTESIAN_POINT ( 'NONE',  ( 198.2581645178918279, 99.52881771501679964, 40.56300693318002715 ) ) ;
#20895 = CARTESIAN_POINT ( 'NONE',  ( -85.31879956968585077, 26.05747381080316316, 88.08442089185827228 ) ) ;
#20896 = AXIS2_PLACEMENT_3D ( 'NONE', #37604, #44267, #16501 ) ;
#20898 = EDGE_LOOP ( 'NONE', ( #47431, #46905, #14989, #35358 ) ) ;
#20897 = CARTESIAN_POINT ( 'NONE',  ( 21.77974794783310486, 62.98608673099827371, 34.48241795236666007 ) ) ;
#20899 = EDGE_LOOP ( 'NONE', ( #32470, #43497, #34862, #15714 ) ) ;
#20900 = VECTOR ( 'NONE', #62759, 1000.000000000000000 ) ;
#20901 = VERTEX_POINT ( 'NONE', #44560 ) ;
#20902 = CARTESIAN_POINT ( 'NONE',  ( 117.7442255600443133, 33.63739995216997158, -70.76590447690840335 ) ) ;
#20903 = CARTESIAN_POINT ( 'NONE',  ( -440.1146514826276643, 388.0000000000064801, -133.9016337311480243 ) ) ;
#20904 = CARTESIAN_POINT ( 'NONE',  ( 307.2575771313985342, 170.0000000000000284, 256.6193948016162381 ) ) ;
#20905 = AXIS2_PLACEMENT_3D ( 'NONE', #5200, #22066, #28032 ) ;
#20907 = CARTESIAN_POINT ( 'NONE',  ( -190.6985136298602015, 109.1272424661243434, -10.81538671745452795 ) ) ;
#20906 = VECTOR ( 'NONE', #16906, 1000.000000000000000 ) ;
#20908 = CARTESIAN_POINT ( 'NONE',  ( -8.810383862755523765, 7.965311326754778598, -8.622074896589690951 ) ) ;
#20909 = CARTESIAN_POINT ( 'NONE',  ( -52.13778968636795241, 39.42540649521991014, 6.377659838150125914E-18 ) ) ;
#20910 = CARTESIAN_POINT ( 'NONE',  ( 70.34686579112866411, -18.11777090454118877, 43.58025477438756923 ) ) ;
#20911 = AXIS2_PLACEMENT_3D ( 'NONE', #50593, #2414, #10104 ) ;
#20912 = CARTESIAN_POINT ( 'NONE',  ( -190.6985136298602015, 109.1272424661243434, -64.50448789838189612 ) ) ;
#20913 = EDGE_LOOP ( 'NONE', ( #55879, #67851, #35947, #26878 ) ) ;
#20914 = ORIENTED_EDGE ( 'NONE', *, *, #6659, .F. ) ;
#20915 = CARTESIAN_POINT ( 'NONE',  ( 70.51583798635768119, 15.57951509147424041, -16.61804899806768532 ) ) ;
#20916 = CARTESIAN_POINT ( 'NONE',  ( -83.13046924527391468, 25.15778674529016357, -48.64714892153850201 ) ) ;
#20917 = CARTESIAN_POINT ( 'NONE',  ( 107.7734915886500460, 27.75592479571297488, 83.71111518197675139 ) ) ;
#20918 = CARTESIAN_POINT ( 'NONE',  ( -156.0209085498132140, 71.27066046086522988, 7.619205632352728408 ) ) ;
#20919 = CARTESIAN_POINT ( 'NONE',  ( 28.03046679490049797, 26.14935035984741774, 13.32819299319723960 ) ) ;
#20920 = FACE_OUTER_BOUND ( 'NONE', #24665, .T. ) ;
#20921 = CARTESIAN_POINT ( 'NONE',  ( -147.4686369529070191, 63.77742835114294451, 84.67161332027325216 ) ) ;
#20922 = ORIENTED_EDGE ( 'NONE', *, *, #67681, .F. ) ;
#20923 = ORIENTED_EDGE ( 'NONE', *, *, #18535, .T. ) ;
#20924 = ORIENTED_EDGE ( 'NONE', *, *, #48453, .T. ) ;
#20925 = DIRECTION ( 'NONE',  ( -0.2225209339563184452, 0.9749279121818226201, 0.000000000000000000 ) ) ;
#20926 = CARTESIAN_POINT ( 'NONE',  ( 34.45972925205163762, 8.830088223935224079, -48.78227442661408020 ) ) ;
#20927 = CARTESIAN_POINT ( 'NONE',  ( 104.6432117441986520, 26.37618165085906341, -92.10548344321300362 ) ) ;
#20928 = CARTESIAN_POINT ( 'NONE',  ( -36.37371824399144060, 10.45334302951138206, 58.89140364663110461 ) ) ;
#20929 = CYLINDRICAL_SURFACE ( 'NONE', #19515, 7.500000000000020428 ) ;
#20930 = EDGE_LOOP ( 'NONE', ( #20180, #1452, #59956, #47111 ) ) ;
#20931 = CARTESIAN_POINT ( 'NONE',  ( 35.44781468922823109, 7.928097401423693569, 57.88074027180304881 ) ) ;
#20932 = CARTESIAN_POINT ( 'NONE',  ( 12.46277766093406214, 6.416700641561363661, -9.434012564203385409 ) ) ;
#20933 = ADVANCED_FACE ( 'NONE', ( #32329 ), #16485, .T. ) ;
#20934 = CARTESIAN_POINT ( 'NONE',  ( 4.590321433068643486, 24.57496590315240681, 0.000000000000000000 ) ) ;
#20935 = CARTESIAN_POINT ( 'NONE',  ( 184.3941060377211443, 82.01604625189463604, 56.90855055168082544 ) ) ;
#20936 = PLANE ( 'NONE',  #49968 ) ;
#20937 = CARTESIAN_POINT ( 'NONE',  ( -81.23297981660238065, 23.31577157498399089, -35.56415816642201833 ) ) ;
#20938 = CARTESIAN_POINT ( 'NONE',  ( 23.28785143291466042, 6.856621069835718174, 63.85807121681927612 ) ) ;
#20939 = FACE_OUTER_BOUND ( 'NONE', #39388, .T. ) ;
#20940 = CARTESIAN_POINT ( 'NONE',  ( 8.767814708128309320, 7.383611927972575373, 8.019991926173236862 ) ) ;
#20941 = EDGE_CURVE ( 'NONE', #60552, #65236, #56204, .T. ) ;
#20942 = VECTOR ( 'NONE', #33017, 1000.000000000000000 ) ;
#20943 = ORIENTED_EDGE ( 'NONE', *, *, #29255, .T. ) ;
#20944 = AXIS2_PLACEMENT_3D ( 'NONE', #18338, #39801, #61257 ) ;
#20945 = CARTESIAN_POINT ( 'NONE',  ( 188.2076037774874635, 86.11782719225436722, 7.600624286963005183 ) ) ;
#20946 = PRODUCT_CONTEXT ( 'NONE', #13005, 'mechanical' ) ;
#20947 = CARTESIAN_POINT ( 'NONE',  ( -190.6985136298601731, 109.1272424661242582, 94.99999999999866418 ) ) ;
#20948 = DIRECTION ( 'NONE',  ( 0.000000000000000000, 0.8660254037844379305, -0.5000000000000013323 ) ) ;
#20949 = FACE_OUTER_BOUND ( 'NONE', #29473, .T. ) ;
#20950 = CARTESIAN_POINT ( 'NONE',  ( 55.91494169499919309, 12.16343363043255543, -67.63797929442789325 ) ) ;
#20951 = EDGE_LOOP ( 'NONE', ( #64924, #7459, #60403, #28308 ) ) ;
#20952 = AXIS2_PLACEMENT_3D ( 'NONE', #52522, #58149, #63777 ) ;
#20953 = ORIENTED_EDGE ( 'NONE', *, *, #18423, .T. ) ;
#20954 = EDGE_LOOP ( 'NONE', ( #62874, #66371, #11247, #2377 ) ) ;
#20955 = EDGE_CURVE ( 'NONE', #39170, #22725, #44086, .T. ) ;
#20956 = CARTESIAN_POINT ( 'NONE',  ( -28.13266652174640470, 9.071935854491409046, -9.236353854820380960 ) ) ;
#20957 = CARTESIAN_POINT ( 'NONE',  ( 197.3756653044963230, 98.41886189307120958, 8.231045378275350544 ) ) ;
#20958 = EDGE_CURVE ( 'NONE', #25468, #68538, #34766, .T. ) ;
#20959 = VERTEX_POINT ( 'NONE', #44253 ) ;
#20960 = AXIS2_PLACEMENT_3D ( 'NONE', #43222, #47469, #4916 ) ;
#20961 = CARTESIAN_POINT ( 'NONE',  ( 60.58000000000000540, -36.09918303830819752, 15.41169613715280562 ) ) ;
#20962 = VERTEX_POINT ( 'NONE', #65733 ) ;
#20963 = DIRECTION ( 'NONE',  ( -0.000000000000000000, 0.000000000000000000, 1.000000000000000000 ) ) ;
#20964 = CARTESIAN_POINT ( 'NONE',  ( 131.6005058089754982, 40.07838125795770168, 29.84241593357604216 ) ) ;
#20965 = DIRECTION ( 'NONE',  ( -0.5508969814520944253, -0.8345732537213078617, 0.000000000000000000 ) ) ;
#20966 = EDGE_CURVE ( 'NONE', #47585, #29324, #34067, .T. ) ;
#20967 = DIRECTION ( 'NONE',  ( -1.000000000000000000, 0.000000000000000000, 0.000000000000000000 ) ) ;
#20968 = DIRECTION ( 'NONE',  ( 1.000000000000000000, 0.000000000000000000, 0.000000000000000000 ) ) ;
#20970 = VERTEX_POINT ( 'NONE', #66092 ) ;
#20969 = FACE_OUTER_BOUND ( 'NONE', #19725, .T. ) ;
#20971 = CARTESIAN_POINT ( 'NONE',  ( -62.97854483871577713, 16.08424353203677271, 40.00000000000003553 ) ) ;
#20972 = ORIENTED_EDGE ( 'NONE', *, *, #7402, .F. ) ;
#20973 = ORIENTED_EDGE ( 'NONE', *, *, #5607, .T. ) ;
#20974 = CARTESIAN_POINT ( 'NONE',  ( -119.2682179969168175, 42.28333404791700190, -12.01608118964443861 ) ) ;
#20975 = CARTESIAN_POINT ( 'NONE',  ( 31.11269837220812562, 31.11269837220800483, 2.000000000000001776 ) ) ;
#20976 = EDGE_CURVE ( 'NONE', #11268, #61262, #7686, .T. ) ;
#20977 = CARTESIAN_POINT ( 'NONE',  ( -180.2252811616041868, 95.40045830523435200, -12.94562834876021107 ) ) ;
#20978 = PLANE ( 'NONE',  #60062 ) ;
#20980 = VERTEX_POINT ( 'NONE', #50585 ) ;
#20979 = CARTESIAN_POINT ( 'NONE',  ( -142.6264002846223775, 58.55577336362199503, -45.30821067346655440 ) ) ;
#20981 = CARTESIAN_POINT ( 'NONE',  ( -109.7058324133404454, 37.86601138638052788, 92.81177118499459766 ) ) ;
#20982 = EDGE_CURVE ( 'NONE', #47734, #13320, #29134, .T. ) ;
#20983 = EDGE_CURVE ( 'NONE', #29324, #64675, #44612, .T. ) ;
#20984 = VERTEX_POINT ( 'NONE', #39000 ) ;
#20985 = B_SPLINE_CURVE_WITH_KNOTS ( 'NONE', 3,
 ( #58796, #47899, #5350, #64087 ),
 .UNSPECIFIED., .F., .F.,
 ( 4, 4 ),
 ( 9.900409499072286585E-07, 0.05658314289920114010 ),
 .UNSPECIFIED. ) ;
#20986 = DIRECTION ( 'NONE',  ( -0.000000000000000000, -1.000000000000000000, -0.000000000000000000 ) ) ;
#20987 = FACE_OUTER_BOUND ( 'NONE', #5925, .T. ) ;
#20988 = CARTESIAN_POINT ( 'NONE',  ( -95.05323930133205579, 30.36974142673411592, 66.93429615280686562 ) ) ;
#20989 = AXIS2_PLACEMENT_3D ( 'NONE', #41441, #52334, #62896 ) ;
#20990 = CARTESIAN_POINT ( 'NONE',  ( -129.6079169496900931, 50.20899308323960497, -62.73827057211200753 ) ) ;
#20991 = CARTESIAN_POINT ( 'NONE',  ( 55.86967469797618691, 11.12799771593089559, -94.59437614483285017 ) ) ;
#20992 = CARTESIAN_POINT ( 'NONE',  ( -100.4262673593280226, 31.84860241619275101, 18.45695312107208252 ) ) ;
#20993 = CARTESIAN_POINT ( 'NONE',  ( -98.46684543088107944, 30.88557736720390778, -62.89638174071533427 ) ) ;
#20994 = ORIENTED_EDGE ( 'NONE', *, *, #62728, .T. ) ;
#20995 = ADVANCED_FACE ( 'NONE', ( #17524 ), #29475, .F. ) ;
#20996 = ORIENTED_EDGE ( 'NONE', *, *, #1850, .T. ) ;
#20997 = AXIS2_PLACEMENT_3D ( 'NONE', #63509, #19562, #4759 ) ;
#20998 = CYLINDRICAL_SURFACE ( 'NONE', #65260, 85.31295361348101380 ) ;
#20999 = CARTESIAN_POINT ( 'NONE',  ( -166.5704851812740515, 80.12110537694670143, -45.87459088847822386 ) ) ;
#21000 = LINE ( 'NONE', #10430, #34027 ) ;
#21001 = CIRCLE ( 'NONE', #38941, 24.69999999999999929 ) ;
#21002 = DIRECTION ( 'NONE',  ( 0.000000000000000000, 0.000000000000000000, 1.000000000000000000 ) ) ;
#21003 = CARTESIAN_POINT ( 'NONE',  ( -78.19438069111009781, 23.21811806230640585, 30.41820113967310846 ) ) ;
#21004 = CARTESIAN_POINT ( 'NONE',  ( -72.21889834709581635, 21.03534256744170960, -65.59680318578142533 ) ) ;
#21005 = ORIENTED_EDGE ( 'NONE', *, *, #31784, .T. ) ;
#21006 = VECTOR ( 'NONE', #35469, 1000.000000000000000 ) ;
#21007 = CARTESIAN_POINT ( 'NONE',  ( 447.3372781065085633, 400.0000000000000568, -146.4497041420118251 ) ) ;
#21008 = CARTESIAN_POINT ( 'NONE',  ( -120.1346137380982526, 44.00127440773568566, 33.30914571746500741 ) ) ;
#21009 = CARTESIAN_POINT ( 'NONE',  ( 208.9781236209186659, 112.4006213943319636, 69.72746670309929584 ) ) ;
#21010 = EDGE_LOOP ( 'NONE', ( #22173, #19482 ) ) ;
#21011 = CARTESIAN_POINT ( 'NONE',  ( -65.36598343705435354, 0.000000000000000000, 41.38025477438755928 ) ) ;
#21012 = ORIENTED_EDGE ( 'NONE', *, *, #66879, .T. ) ;
#21014 = AXIS2_PLACEMENT_3D ( 'NONE', #998, #44602, #66082 ) ;
#21013 = CARTESIAN_POINT ( 'NONE',  ( -14.94265033805046095, 7.459411036484911328, -45.33398552347500754 ) ) ;
#21015 = DIRECTION ( 'NONE',  ( 0.000000000000000000, 0.000000000000000000, 1.000000000000000000 ) ) ;
#21016 = CARTESIAN_POINT ( 'NONE',  ( 92.95016907945942819, 22.74936990452175678, 60.01214966832145592 ) ) ;
#21017 = CARTESIAN_POINT ( 'NONE',  ( 56.42997683260104225, 32.25922681454270702, 170.0000000000000000 ) ) ;
#21018 = FACE_OUTER_BOUND ( 'NONE', #8135, .T. ) ;
#21019 = CARTESIAN_POINT ( 'NONE',  ( 34.45500533947588195, 7.817363290423888778, -64.30597072735039887 ) ) ;
#21020 = CARTESIAN_POINT ( 'NONE',  ( -94.83091526606385457, 30.26550147229323073, -70.37511245693397655 ) ) ;
#21021 = CARTESIAN_POINT ( 'NONE',  ( -32.41898580403140784, 10.77423026598439648, -8.520716206325841924 ) ) ;
#21022 = ORIENTED_EDGE ( 'NONE', *, *, #50010, .T. ) ;
#21023 = LINE ( 'NONE', #54748, #58950 ) ;
#21025 = ORIENTED_EDGE ( 'NONE', *, *, #50272, .F. ) ;
#21024 = EDGE_CURVE ( 'NONE', #28566, #26321, #26133, .T. ) ;
#21026 = CARTESIAN_POINT ( 'NONE',  ( 42.02161712141799654, -16.09918303830818687, 30.00000000000000000 ) ) ;
#21027 = CARTESIAN_POINT ( 'NONE',  ( 12.47451846520757002, 7.423604437114563304, -76.59618454708339641 ) ) ;
#21028 = CARTESIAN_POINT ( 'NONE',  ( -190.3061188229049208, 108.5745819235681751, 15.45852572812942327 ) ) ;
#21029 = DIRECTION ( 'NONE',  ( -1.000000000000000000, 0.000000000000000000, 0.000000000000000000 ) ) ;
#21030 = CARTESIAN_POINT ( 'NONE',  ( -1.857619870843140619, 6.575690665396233925, 42.18455459037815558 ) ) ;
#21031 = CARTESIAN_POINT ( 'NONE',  ( 210.6189312023034574, 116.6550319566545539, 94.99999999999866418 ) ) ;
#21032 = CARTESIAN_POINT ( 'NONE',  ( 151.6178224291901131, 54.48737267587416966, -38.92713886945099233 ) ) ;
#21033 = EDGE_CURVE ( 'NONE', #45819, #37504, #60081, .T. ) ;
#21034 = VERTEX_POINT ( 'NONE', #12260 ) ;
#21035 = DIRECTION ( 'NONE',  ( 4.104355744161125585E-15, -4.104355744161082987E-15, 1.000000000000000000 ) ) ;
#21036 = CARTESIAN_POINT ( 'NONE',  ( -189.4248691432192970, 107.3461292335514656, -16.99913809175565405 ) ) ;
#21037 = CARTESIAN_POINT ( 'NONE',  ( 175.5498284945444709, 74.57669191966280664, -21.96822280477383060 ) ) ;
#21038 = CARTESIAN_POINT ( 'NONE',  ( -108.5248383251030333, 37.21456094989614627, 60.70243158702523090 ) ) ;
#21039 = ITEM_DEFINED_TRANSFORMATION ( 'NONE', 'NONE', #51251,  #66832 ) ;
#21040 = LINE ( 'NONE', #36526, #17526 ) ;
#21041 = ORIENTED_EDGE ( 'NONE', *, *, #35296, .T. ) ;
#21042 = DIRECTION ( 'NONE',  ( 1.000000000000000000, 1.387778780781444936E-16, 0.000000000000000000 ) ) ;
#21043 = CARTESIAN_POINT ( 'NONE',  ( -2.866724795119724778, 6.618578306599219196, -10.42539455610338806 ) ) ;
#21044 = VECTOR ( 'NONE', #59014, 1000.000000000000000 ) ;
#21045 = EDGE_CURVE ( 'NONE', #7345, #32729, #28428, .T. ) ;
#21046 = CARTESIAN_POINT ( 'NONE',  ( 197.9868529032975744, 99.18611233336805810, -20.34206310618822755 ) ) ;
#21047 = CARTESIAN_POINT ( 'NONE',  ( -142.0345488537072072, 58.09133413710082294, 91.24922763633107081 ) ) ;
#21048 = EDGE_CURVE ( 'NONE', #14098, #13609, #35526, .T. ) ;
#21049 = AXIS2_PLACEMENT_3D ( 'NONE', #52923, #69106, #52253 ) ;
#21050 = DIRECTION ( 'NONE',  ( 1.000000000000000000, 0.000000000000000000, 0.000000000000000000 ) ) ;
#21051 = EDGE_CURVE ( 'NONE', #9638, #29599, #12607, .T. ) ;
#21052 = ORIENTED_EDGE ( 'NONE', *, *, #51856, .F. ) ;
#21053 = DIRECTION ( 'NONE',  ( 0.000000000000000000, 1.000000000000000000, 2.184185950696548891E-33 ) ) ;
#21054 = CARTESIAN_POINT ( 'NONE',  ( 80.16761386260783695, 18.37011649821945269, 6.527426858061783577 ) ) ;
#21055 = CIRCLE ( 'NONE', #22145, 4.999999999999997335 ) ;
#21056 = CARTESIAN_POINT ( 'NONE',  ( 164.8433205901839358, 64.93586312665800619, 11.46758294457424654 ) ) ;
#21057 = CARTESIAN_POINT ( 'NONE',  ( 31.11269837220809364, 20.55634918610396866, 0.000000000000000000 ) ) ;
#21058 = AXIS2_PLACEMENT_3D ( 'NONE', #194, #22701, #21654 ) ;
#21059 = ORIENTED_EDGE ( 'NONE', *, *, #47316, .F. ) ;
#21060 = VECTOR ( 'NONE', #10932, 1000.000000000000000 ) ;
#21061 = B_SPLINE_CURVE_WITH_KNOTS ( 'NONE', 3,
 ( #59930, #27933, #49722, #1550, #6485, #39880, #38852, #49372, #1204, #61341, #13161, #55004, #39537, #66631, #18427, #45150, #23709, #22657, #44098, #23011, #17015, #55715, #65581, #17743, #55357, #17374, #43747, #60296, #33580, #44464, #50440, #28274, #12114, #34626, #7541, #7879, #39200, #33918, #65224, #60990, #6826, #12812, #65945, #29329 ),
 .UNSPECIFIED., .F., .F.,
 ( 4, 2, 2, 2, 2, 2, 2, 2, 2, 2, 2, 2, 2, 2, 2, 2, 2, 2, 2, 2, 2, 4 ),
 ( 1.440969542111313559E-17, 0.001482469635030006592, 0.002223704452545002298, 0.002964939270059997571, 0.004447408905089988117, 0.005929878540119976928, 0.007412348175149966606, 0.008153582992664965348, 0.008894817810179967560, 0.01037728744520997198, 0.01185975708023997814, 0.01260099189775498556, 0.01334222671526999297, 0.01482469635030000607, 0.01556593116781501175, 0.01630716598533001743, 0.01778963562036001839, 0.01927210525539002628, 0.02001334007290502676, 0.02075457489042003070, 0.02223704452545005247, 0.02371951416048007424 ),
 .UNSPECIFIED. ) ;
#21062 = CARTESIAN_POINT ( 'NONE',  ( 174.1348882614952629, 73.23561817543360064, 66.48859792493803411 ) ) ;
#21063 = ORIENTED_EDGE ( 'NONE', *, *, #17155, .T. ) ;
#21064 = VECTOR ( 'NONE', #51541, 1000.000000000000000 ) ;
#21065 = CARTESIAN_POINT ( 'NONE',  ( -105.8879439778144445, 34.65133284149107595, -49.10708695906607346 ) ) ;
#21066 = CARTESIAN_POINT ( 'NONE',  ( 69.08240197259638649, 14.16210831900840716, -74.48173343371692567 ) ) ;
#21067 = CARTESIAN_POINT ( 'NONE',  ( 0.000000000000000000, 0.000000000000000000, 0.000000000000000000 ) ) ;
#21069 = ORIENTED_EDGE ( 'NONE', *, *, #45579, .T. ) ;
#21068 = CARTESIAN_POINT ( 'NONE',  ( 151.1700480242206197, 54.15904440870136938, 14.14223021667874569 ) ) ;
#21070 = CARTESIAN_POINT ( 'NONE',  ( -178.0633751203918393, 92.80295726428047942, 43.96776513697549404 ) ) ;
#21071 = CARTESIAN_POINT ( 'NONE',  ( 0.000000000000000000, 0.000000000000000000, 0.000000000000000000 ) ) ;
#21072 = EDGE_CURVE ( 'NONE', #47842, #60292, #25934, .T. ) ;
#21073 = EDGE_CURVE ( 'NONE', #55324, #10027, #45209, .T. ) ;
#21074 = CARTESIAN_POINT ( 'NONE',  ( 117.4711568421289627, 33.49899443629671936, -41.35662267546008763 ) ) ;
#21075 = ORIENTED_EDGE ( 'NONE', *, *, #7047, .F. ) ;
#21076 = ADVANCED_FACE ( 'NONE', ( #24564 ), #4476, .F. ) ;
#21077 = CARTESIAN_POINT ( 'NONE',  ( -65.36598343705435354, 0.000000000000000000, 41.38025477438755928 ) ) ;
#21078 = CARTESIAN_POINT ( 'NONE',  ( 137.4117721579687554, 43.61242559081432546, 70.47591696582985321 ) ) ;
#21079 = CARTESIAN_POINT ( 'NONE',  ( -166.5686015187718283, 80.11916873959171426, 41.98092334962779404 ) ) ;
#21080 = CARTESIAN_POINT ( 'NONE',  ( -37.38781680082736614, 10.64362327909142181, -74.25552192898616966 ) ) ;
#21081 = CARTESIAN_POINT ( 'NONE',  ( 0.000000000000000000, 0.000000000000000000, 5.000000000000000000 ) ) ;
#21082 = ORIENTED_EDGE ( 'NONE', *, *, #30023, .T. ) ;
#21083 = CARTESIAN_POINT ( 'NONE',  ( 45.35621884287174765, 10.27694987765648271, 5.982729125893944122 ) ) ;
#21084 = ORIENTED_EDGE ( 'NONE', *, *, #48041, .T. ) ;
#21085 = EDGE_LOOP ( 'NONE', ( #29214, #27170, #33901, #48224 ) ) ;
#21086 = CARTESIAN_POINT ( 'NONE',  ( 209.3223706822284100, 0.000000000000000000, 31.44247402469554942 ) ) ;
#21087 = CARTESIAN_POINT ( 'NONE',  ( 212.1488570093001726, 119.0116247937291405, -17.85290917965843605 ) ) ;
#21088 = PRESENTATION_STYLE_ASSIGNMENT (( #5247 ) ) ;
#21089 = CARTESIAN_POINT ( 'NONE',  ( -157.0077369422017739, 70.81157624963286423, -69.43848245219707849 ) ) ;
#21090 = AXIS2_PLACEMENT_3D ( 'NONE', #30067, #57143, #14568 ) ;
#21091 = CARTESIAN_POINT ( 'NONE',  ( -109.2503638244981232, 36.46497529133068127, 88.92031527522445344 ) ) ;
#21092 = DIRECTION ( 'NONE',  ( 0.000000000000000000, -0.9999993111447558203, 0.001173758924898823551 ) ) ;
#21093 = CARTESIAN_POINT ( 'NONE',  ( 207.8675797643809631, 110.7908513421271977, -37.01557826710286037 ) ) ;
#21094 = DIRECTION ( 'NONE',  ( -0.000000000000000000, 1.000000000000000000, -0.000000000000000000 ) ) ;
#21095 = ORIENTED_EDGE ( 'NONE', *, *, #4372, .F. ) ;
#21096 = AXIS2_PLACEMENT_3D ( 'NONE', #24338, #28917, #7100 ) ;
#21097 = DIRECTION ( 'NONE',  ( -0.000000000000000000, -0.000000000000000000, -1.000000000000000000 ) ) ;
#21098 = VERTEX_POINT ( 'NONE', #36143 ) ;
#21099 = CARTESIAN_POINT ( 'NONE',  ( -71.17984086584780812, 20.67393782512345624, 65.27769819161431997 ) ) ;
#21100 =( REPRESENTATION_RELATIONSHIP ('NONE','NONE', #40274, #22184 ) REPRESENTATION_RELATIONSHIP_WITH_TRANSFORMATION ( #57427 )SHAPE_REPRESENTATION_RELATIONSHIP( ) );
#21101 = CARTESIAN_POINT ( 'NONE',  ( 188.2950202724320263, 86.21411212788220269, 34.72575518757594182 ) ) ;
#21102 = CARTESIAN_POINT ( 'NONE',  ( 417.3372781065086201, 0.000000000000000000, -146.4497041420118251 ) ) ;
#21103 = CIRCLE ( 'NONE', #50326, 22.00000000000000355 ) ;
#21104 = CARTESIAN_POINT ( 'NONE',  ( -76.78936026062118003, 21.61552955137052479, 3.808395977436665358 ) ) ;
#21105 = CARTESIAN_POINT ( 'NONE',  ( -33.12535873119978191, 9.874205581139028354, -89.19521348031341290 ) ) ;
#21106 = CARTESIAN_POINT ( 'NONE',  ( 21.43750346857338229, 7.754771113113082315, 42.47208553991309543 ) ) ;
#21107 = CARTESIAN_POINT ( 'NONE',  ( 197.5213143501814272, 96.99325216816036743, 88.17819802051872102 ) ) ;
#21108 = CIRCLE ( 'NONE', #42434, 74.95140232871122521 ) ;
#21109 = DIRECTION ( 'NONE',  ( -1.000000000000000000, 0.000000000000000000, 0.000000000000000000 ) ) ;
#21110 = ORIENTED_EDGE ( 'NONE', *, *, #63250, .F. ) ;
#21111 = CARTESIAN_POINT ( 'NONE',  ( -76.10397364431022993, 21.36211154336727702, 57.71004732640698620 ) ) ;
#21112 = FACE_OUTER_BOUND ( 'NONE', #19187, .T. ) ;
#21113 = ORIENTED_EDGE ( 'NONE', *, *, #22875, .F. ) ;
#21114 = ORIENTED_EDGE ( 'NONE', *, *, #31124, .F. ) ;
#21115 = DIRECTION ( 'NONE',  ( 1.000000000000000000, -0.000000000000000000, -0.000000000000000000 ) ) ;
#21116 = CARTESIAN_POINT ( 'NONE',  ( 57.39674746172462250, 11.43903079040058834, -38.22885664779096970 ) ) ;
#21117 = CARTESIAN_POINT ( 'NONE',  ( 25.97682081077775251, -21.03539584665513829, 6.893342938366318506 ) ) ;
#21118 = LINE ( 'NONE', #26733, #23790 ) ;
#21119 = AXIS2_PLACEMENT_3D ( 'NONE', #52480, #58105, #25766 ) ;
#21120 = ADVANCED_FACE ( 'NONE', ( #41765, #62877, #47366, #31221, #46688, #56912 ), #57938, .T. ) ;
#21121 = CARTESIAN_POINT ( 'NONE',  ( 410.0000000000000000, 190.0000000000000000, 0.000000000000000000 ) ) ;
#21122 = VERTEX_POINT ( 'NONE', #68164 ) ;
#21123 = ORIENTED_EDGE ( 'NONE', *, *, #23233, .T. ) ;
#21124 = CARTESIAN_POINT ( 'NONE',  ( -125.8938041572051389, 47.69968343338778283, 30.61994787315706290 ) ) ;
#21125 = ORIENTED_EDGE ( 'NONE', *, *, #28010, .F. ) ;
#21126 = CARTESIAN_POINT ( 'NONE',  ( -36.11269837220809364, -10.55634918610397932, 2.000000000000001776 ) ) ;
#21127 = DIRECTION ( 'NONE',  ( -0.000000000000000000, -0.000000000000000000, -1.000000000000000000 ) ) ;
#21128 = CARTESIAN_POINT ( 'NONE',  ( 59.72526569420001152, 11.93313563009888689, 70.91484602205103727 ) ) ;
#21129 = CARTESIAN_POINT ( 'NONE',  ( -22.50000000000000355, 207.5000000000000284, 20.00000000000000000 ) ) ;
#21130 = EDGE_CURVE ( 'NONE', #41110, #14174, #8729, .T. ) ;
#21131 = DIRECTION ( 'NONE',  ( 0.8584487936018655452, 0.5128992774059070170, 0.000000000000000000 ) ) ;
#21132 = SURFACE_SIDE_STYLE ('',( #69306 ) ) ;
#21133 = EDGE_CURVE ( 'NONE', #40777, #18538, #27267, .T. ) ;
#21134 = ORIENTED_EDGE ( 'NONE', *, *, #66760, .T. ) ;
#21135 = EDGE_CURVE ( 'NONE', #59365, #28423, #5916, .T. ) ;
#21136 = ORIENTED_EDGE ( 'NONE', *, *, #19463, .F. ) ;
#21137 = CARTESIAN_POINT ( 'NONE',  ( 442.3372781065085633, 390.0000000000001137, 108.5502958579883170 ) ) ;
#21138 = PLANE ( 'NONE',  #57516 ) ;
#21139 = CARTESIAN_POINT ( 'NONE',  ( -165.9992860119575084, 79.53569239468046703, -17.73646718843910008 ) ) ;
#21140 = CARTESIAN_POINT ( 'NONE',  ( 135.6651581599209919, 42.52720121194706593, -77.65019136801915067 ) ) ;
#21141 = CARTESIAN_POINT ( 'NONE',  ( 204.6977192012829789, 106.3443248447423599, 56.05227132923312183 ) ) ;
#21142 = CARTESIAN_POINT ( 'NONE',  ( -189.7334103489410211, 107.7745063523401114, -71.65189628423172508 ) ) ;
#21143 = ORIENTED_EDGE ( 'NONE', *, *, #47164, .T. ) ;
#21144 = CARTESIAN_POINT ( 'NONE',  ( -95.52163045714284806, 29.47808868198295329, 61.60217047910855825 ) ) ;
#21145 = VERTEX_POINT ( 'NONE', #18926 ) ;
#21147 = CARTESIAN_POINT ( 'NONE',  ( -73.81689110552360944, 20.53332132481498462, 32.19181849619675972 ) ) ;
#21146 = AXIS2_PLACEMENT_3D ( 'NONE', #12651, #39039, #18620 ) ;
#21148 = ORIENTED_EDGE ( 'NONE', *, *, #4327, .F. ) ;
#21149 = AXIS2_PLACEMENT_3D ( 'NONE', #19661, #41121, #66838 ) ;
#21150 = ORIENTED_EDGE ( 'NONE', *, *, #7309, .T. ) ;
#21151 = CARTESIAN_POINT ( 'NONE',  ( -119.6801029354224681, 43.71909921132878907, 7.067823973529548276 ) ) ;
#21152 = CARTESIAN_POINT ( 'NONE',  ( -179.8996803435689174, 95.00451760716447325, 68.38766948947770175 ) ) ;
#21153 = AXIS2_PLACEMENT_3D ( 'NONE', #33630, #54352, #6178 ) ;
#21154 = CARTESIAN_POINT ( 'NONE',  ( 126.4324872316703363, 37.11876756822026380, 64.95086461873292194 ) ) ;
#21155 = ORIENTED_EDGE ( 'NONE', *, *, #2481, .F. ) ;
#21156 = EDGE_CURVE ( 'NONE', #40373, #63617, #35801, .T. ) ;
#21157 = CARTESIAN_POINT ( 'NONE',  ( 63.01563776193091826, 13.70579113808096849, 17.96841034875761878 ) ) ;
#21158 = CARTESIAN_POINT ( 'NONE',  ( 152.8558173410469578, 54.14978343559394602, 42.84179159303089790 ) ) ;
#21159 = DIRECTION ( 'NONE',  ( -0.000000000000000000, -0.000000000000000000, -1.000000000000000000 ) ) ;
#21160 = FACE_OUTER_BOUND ( 'NONE', #5536, .T. ) ;
#21161 = CARTESIAN_POINT ( 'NONE',  ( -26.88245755577923291, 8.887394979218516511, 31.73890780661882971 ) ) ;
#21162 = DIRECTION ( 'NONE',  ( -0.8496664383351307803, 0.000000000000000000, 0.5273205320930463014 ) ) ;
#21163 = ORIENTED_EDGE ( 'NONE', *, *, #25181, .F. ) ;
#21164 = FACE_BOUND ( 'NONE', #31960, .T. ) ;
#21165 = PLANE ( 'NONE',  #35418 ) ;
#21166 = CARTESIAN_POINT ( 'NONE',  ( -79.62207341875657107, 23.76621716825509623, -62.00572262374755894 ) ) ;
#21167 = CARTESIAN_POINT ( 'NONE',  ( 174.4912080999799002, 73.57140295268877139, 13.55010776019312679 ) ) ;
#21168 = CARTESIAN_POINT ( 'NONE',  ( -20.55634918610408945, -31.11269837220804035, 85.00100000000000477 ) ) ;
#21169 = CARTESIAN_POINT ( 'NONE',  ( -85.89078989036968892, 26.29712602777652464, 9.043151598351821363 ) ) ;
#21170 = CARTESIAN_POINT ( 'NONE',  ( 0.000000000000000000, 0.000000000000000000, 0.000000000000000000 ) ) ;
#21171 = CARTESIAN_POINT ( 'NONE',  ( 37.36225457415450535, 8.152725941243264884, -89.57965209093477199 ) ) ;
#21172 = CARTESIAN_POINT ( 'NONE',  ( -118.4709174626548531, 42.97515378817185905, -68.15209134257274570 ) ) ;
#21173 = CARTESIAN_POINT ( 'NONE',  ( 63.98009977735162579, 12.89803120691695959, 3.014776002286982948 ) ) ;
#21174 = CARTESIAN_POINT ( 'NONE',  ( -85.66184035008924980, 26.20110535976566624, 67.47910982318403228 ) ) ;
#21175 = CARTESIAN_POINT ( 'NONE',  ( 93.32228019177713918, 22.88890999585039410, -19.87069863458034291 ) ) ;
#21176 = VERTEX_POINT ( 'NONE', #25603 ) ;
#21177 = ITEM_DEFINED_TRANSFORMATION ( 'NONE', 'NONE', #21950,  #39895 ) ;
#21178 = ORIENTED_EDGE ( 'NONE', *, *, #40498, .T. ) ;
#21179 = LINE ( 'NONE', #9590, #63285 ) ;
#21180 = ORIENTED_EDGE ( 'NONE', *, *, #19133, .T. ) ;
#21181 = CARTESIAN_POINT ( 'NONE',  ( 22.28700331106866983, 7.803633676228379557, -66.11158134317128088 ) ) ;
#21182 = CARTESIAN_POINT ( 'NONE',  ( -452.6627218934914936, 364.9999999999953957, 113.5502958579925945 ) ) ;
#21183 = CARTESIAN_POINT ( 'NONE',  ( -144.7530445311634821, 61.54314312182903990, 59.25981816036905059 ) ) ;
#21184 = CARTESIAN_POINT ( 'NONE',  ( 230.9999999999999432, -2.000000000000001776, 72.99999999999998579 ) ) ;
#21185 = LINE ( 'NONE', #26805, #50842 ) ;
#21186 = CARTESIAN_POINT ( 'NONE',  ( -52.00092620775817664, 14.92276858858357436, -76.41618673138754048 ) ) ;
#21187 = DIRECTION ( 'NONE',  ( -0.000000000000000000, -0.000000000000000000, -1.000000000000000000 ) ) ;
#21188 = CARTESIAN_POINT ( 'NONE',  ( -122.3994536713185539, 45.42826354555015911, -8.928800194678888857 ) ) ;
#21189 = ORIENTED_EDGE ( 'NONE', *, *, #48017, .F. ) ;
#21190 = EDGE_CURVE ( 'NONE', #41559, #54229, #47498, .T. ) ;
#21191 = ORIENTED_EDGE ( 'NONE', *, *, #57402, .F. ) ;
#21192 = EDGE_CURVE ( 'NONE', #27437, #60955, #9758, .T. ) ;
#21193 = CARTESIAN_POINT ( 'NONE',  ( 64.98797965777978902, -1.250000000000021760, 40.00000000000003553 ) ) ;
#21194 = CARTESIAN_POINT ( 'NONE',  ( -306.1215797690288696, 161.1948386903797825, 0.000000000000000000 ) ) ;
#21195 = DIRECTION ( 'NONE',  ( -0.5407162030609373726, -0.6444004775717707689, 0.5407162030609373726 ) ) ;
#21196 = EDGE_CURVE ( 'NONE', #14640, #37433, #68495, .T. ) ;
#21197 = CARTESIAN_POINT ( 'NONE',  ( 128.0786479395874267, 39.20070012600677956, -92.41263896547152967 ) ) ;
#21198 = DIRECTION ( 'NONE',  ( 1.000000000000000000, 0.000000000000000000, -0.000000000000000000 ) ) ;
#21199 = CIRCLE ( 'NONE', #60511, 10.00000000000000000 ) ;
#21200 = CARTESIAN_POINT ( 'NONE',  ( 89.88147981065577596, 21.62466191578948127, 17.14297335626316254 ) ) ;
#21201 = CARTESIAN_POINT ( 'NONE',  ( -15.08468253268399728, 7.472949889606720575, 62.51227595438552243 ) ) ;
#21202 = CARTESIAN_POINT ( 'NONE',  ( 210.0055645826032844, 115.7254585628714239, 4.541385688506491825 ) ) ;
#21203 =( LENGTH_UNIT ( ) NAMED_UNIT ( * ) SI_UNIT ( .MILLI., .METRE. ) );
#21204 = CARTESIAN_POINT ( 'NONE',  ( -85.85317205159077503, 26.28128351165222298, -94.11325662453201346 ) ) ;
#21205 = CARTESIAN_POINT ( 'NONE',  ( 46.76970795284345428, 9.482505412758889918, -14.81013751142722867 ) ) ;
#21206 = CARTESIAN_POINT ( 'NONE',  ( 205.0999694062793424, 106.8955893716604777, -24.48138044215792064 ) ) ;
#21207 = CARTESIAN_POINT ( 'NONE',  ( 108.6977768404062914, 21.46141967451380950, -4.838576272177880000 ) ) ;
#21208 = EDGE_CURVE ( 'NONE', #50651, #43728, #42978, .T. ) ;
#21209 = CARTESIAN_POINT ( 'NONE',  ( 157.4703587214989398, 58.92748579479259519, 71.25401806271709404 ) ) ;
#21210 = EDGE_CURVE ( 'NONE', #65730, #16433, #19261, .T. ) ;
#21211 = VERTEX_POINT ( 'NONE', #45997 ) ;
#21212 = EDGE_CURVE ( 'NONE', #27636, #26875, #64329, .T. ) ;
#21213 = LINE ( 'NONE', #63082, #61616 ) ;
#21214 = CARTESIAN_POINT ( 'NONE',  ( 92.52113039222224700, 22.58921125235803729, -38.65466082921378188 ) ) ;
#21215 = CARTESIAN_POINT ( 'NONE',  ( 99.99999999999997158, 6.000000000000000000, -25.00000000000000000 ) ) ;
#21216 = LINE ( 'NONE', #21891, #20848 ) ;
#21217 = CARTESIAN_POINT ( 'NONE',  ( 150.4544126017350720, 52.39556706174411715, 7.400449090205046154 ) ) ;
#21218 = CARTESIAN_POINT ( 'NONE',  ( -3.540478021920604679, 7.657046766457612286, 85.14064472492238167 ) ) ;
#21219 = ADVANCED_FACE ( 'NONE', ( #19972 ), #3438, .T. ) ;
#21220 = ORIENTED_EDGE ( 'NONE', *, *, #58272, .F. ) ;
#21221 = CARTESIAN_POINT ( 'NONE',  ( 57.30278335769541087, 48.40406511297401693, 170.0000000000000000 ) ) ;
#21222 = CARTESIAN_POINT ( 'NONE',  ( -62.45176220516618315, 16.79101814080731714, 65.91410335926558162 ) ) ;
#21223 = VERTEX_POINT ( 'NONE', #19614 ) ;
#21224 = ORIENTED_EDGE ( 'NONE', *, *, #25519, .T. ) ;
#21225 = CARTESIAN_POINT ( 'NONE',  ( 41.05177318205839754, 9.645271888559822315, 83.77932428570838397 ) ) ;
#21226 = LINE ( 'NONE', #37387, #58941 ) ;
#21227 = CARTESIAN_POINT ( 'NONE',  ( 137.8343364920582133, 45.06871843100040564, -90.84222727415109944 ) ) ;
#21228 = EDGE_LOOP ( 'NONE', ( #40945, #53294, #30734, #29017 ) ) ;
#21229 = CARTESIAN_POINT ( 'NONE',  ( -59.56523643198715234, 15.93788386494078502, -63.56521738332754268 ) ) ;
#21230 = CARTESIAN_POINT ( 'NONE',  ( 39.40195752203892710, 8.409560354027385998, -8.775266874964067654 ) ) ;
#21231 = CARTESIAN_POINT ( 'NONE',  ( 175.0696098417091662, 74.11936424544846602, -48.21306686516284401 ) ) ;
#21232 = CARTESIAN_POINT ( 'NONE',  ( -7.345652830558753621, 4.996589667937373136, -9.003584543331209389 ) ) ;
#21233 = CARTESIAN_POINT ( 'NONE',  ( 88.52345267551655184, 20.07594890262053866, 29.95123874579921619 ) ) ;
#21234 = ORIENTED_EDGE ( 'NONE', *, *, #15473, .F. ) ;
#21235 = DIRECTION ( 'NONE',  ( -0.000000000000000000, -0.000000000000000000, -1.000000000000000000 ) ) ;
#21236 = DIRECTION ( 'NONE',  ( -0.000000000000000000, 1.000000000000000000, -0.000000000000000000 ) ) ;
#21237 = FACE_OUTER_BOUND ( 'NONE', #41375, .T. ) ;
#21238 = CARTESIAN_POINT ( 'NONE',  ( 198.7123879174244223, 100.1053816708572555, 32.18029401982719406 ) ) ;
#21239 = VECTOR ( 'NONE', #47346, 1000.000000000000000 ) ;
#21240 = CARTESIAN_POINT ( 'NONE',  ( -83.27963540317796287, 25.21826204940221317, 85.68556430999879581 ) ) ;
#21242 = EDGE_LOOP ( 'NONE', ( #6841, #44152, #19143, #19873, #19514, #60481, #47390, #24560, #20488 ) ) ;
#21241 = DIRECTION ( 'NONE',  ( 0.000000000000000000, 0.000000000000000000, 1.000000000000000000 ) ) ;
#21243 = ORIENTED_EDGE ( 'NONE', *, *, #31936, .T. ) ;
#21244 = ORIENTED_EDGE ( 'NONE', *, *, #16902, .T. ) ;
#21245 = CARTESIAN_POINT ( 'NONE',  ( 116.0822834687217266, 32.80169113915576418, -65.53445419630700997 ) ) ;
#21246 = DIRECTION ( 'NONE',  ( -1.000000000000000000, 3.344045254895050726E-17, -1.337618101958020291E-16 ) ) ;
#21247 = DIRECTION ( 'NONE',  ( -1.000000000000000000, -0.000000000000000000, -1.334402673828313339E-16 ) ) ;
#21248 = CARTESIAN_POINT ( 'NONE',  ( -36.89224332184166855, 11.57404295377975956, 59.40614351394950177 ) ) ;
#21249 = CARTESIAN_POINT ( 'NONE',  ( -10.23531775138760480, 8.068923942586298637, -23.18003092887482453 ) ) ;
#21250 = CARTESIAN_POINT ( 'NONE',  ( 152.6560521232696033, 54.00248515670894989, -76.22471660518338865 ) ) ;
#21251 = CARTESIAN_POINT ( 'NONE',  ( -24.09190246691234805, 9.515371887976103338, -95.00000000000133582 ) ) ;
#21252 = DIRECTION ( 'NONE',  ( -0.000000000000000000, 1.000000000000000000, -0.000000000000000000 ) ) ;
#21253 = VERTEX_POINT ( 'NONE', #41074 ) ;
#21254 = VERTEX_POINT ( 'NONE', #51968 ) ;
#21255 = CARTESIAN_POINT ( 'NONE',  ( 64.08056813503695537, 12.89932471814515225, 41.38025477438755928 ) ) ;
#21256 = CARTESIAN_POINT ( 'NONE',  ( 0.000000000000000000, 0.000000000000000000, 380.0000000000000000 ) ) ;
#21257 = CARTESIAN_POINT ( 'NONE',  ( 107.1706323048065599, 27.48610522718908911, 83.95080517049565572 ) ) ;
#21258 = CARTESIAN_POINT ( 'NONE',  ( 115.7612476187724013, 32.64200929566222698, -11.47492610996905782 ) ) ;
#21259 = ADVANCED_FACE ( 'NONE', ( #47713 ), #16407, .F. ) ;
#21260 = DIRECTION ( 'NONE',  ( -0.000000000000000000, -1.000000000000000000, -0.000000000000000000 ) ) ;
#21261 = DIRECTION ( 'NONE',  ( -0.000000000000000000, -0.000000000000000000, 1.000000000000000000 ) ) ;
#21262 = CARTESIAN_POINT ( 'NONE',  ( -190.6985136298602015, 109.1272424661243434, -91.34903848884556510 ) ) ;
#21263 = ORIENTED_EDGE ( 'NONE', *, *, #23846, .T. ) ;
#21264 = ORIENTED_EDGE ( 'NONE', *, *, #6364, .T. ) ;
#21265 = EDGE_CURVE ( 'NONE', #63094, #69498, #11462, .T. ) ;
#21266 = ORIENTED_EDGE ( 'NONE', *, *, #21265, .F. ) ;
#21267 = CARTESIAN_POINT ( 'NONE',  ( -151.2511071212631748, 67.00426547928871912, -8.160532014092686026 ) ) ;
#21268 = ADVANCED_FACE ( 'NONE', ( #64250 ), #37167, .F. ) ;
#21269 = CARTESIAN_POINT ( 'NONE',  ( 33.75794032130627187, 8.754084575552404601, -38.15644254858585782 ) ) ;
#21270 = B_SPLINE_CURVE_WITH_KNOTS ( 'NONE', 3,
 ( #47454, #30962, #58361, #4226, #47121, #52735 ),
 .UNSPECIFIED., .F., .F.,
 ( 4, 2, 4 ),
 ( 0.03218947840871067695, 0.06469842185262320022, 0.09720736529653573044 ),
 .UNSPECIFIED. ) ;
#21271 = EDGE_CURVE ( 'NONE', #42749, #16065, #222, .T. ) ;
#21272 = DIRECTION ( 'NONE',  ( -0.04486483035051862939, 0.9989930665413143673, 0.000000000000000000 ) ) ;
#21273 = CIRCLE ( 'NONE', #3311, 2.999999999999981792 ) ;
#21274 = CARTESIAN_POINT ( 'NONE',  ( 203.9228889538745193, 106.9879579748728702, 56.08195001833964710 ) ) ;
#21275 = EDGE_LOOP ( 'NONE', ( #48937, #6067, #1645, #32059, #28609 ) ) ;
#21276 = CARTESIAN_POINT ( 'NONE',  ( 183.1873354889583538, 82.20882912211250471, 56.44120003221799209 ) ) ;
#21277 = CARTESIAN_POINT ( 'NONE',  ( -156.0300823189602113, 69.91528270335481920, 61.32471221532804861 ) ) ;
#21278 = CARTESIAN_POINT ( 'NONE',  ( -7.825402957745087207, 6.891034867348159842, -35.41807073194381417 ) ) ;
#21279 = CARTESIAN_POINT ( 'NONE',  ( 184.3994103300443328, 82.02159554764423888, 70.39554651480847269 ) ) ;
#21280 = CARTESIAN_POINT ( 'NONE',  ( -439.4229916354183274, 388.0000000000020464, 101.0502958579930066 ) ) ;
#21281 = CARTESIAN_POINT ( 'NONE',  ( -86.15441609607631790, 25.31657638323081727, -43.11050758368907054 ) ) ;
#21282 = CARTESIAN_POINT ( 'NONE',  ( 16.28371206594635368, 6.516665886438621769, 71.85925826316893961 ) ) ;
#21283 = DIRECTION ( 'NONE',  ( -1.000000000000000000, 0.000000000000000000, 0.000000000000000000 ) ) ;
#21284 = CARTESIAN_POINT ( 'NONE',  ( 8.848532605049241440, 6.377649401037235322, -66.98796475424842356 ) ) ;
#21285 = EDGE_CURVE ( 'NONE', #62629, #53534, #48059, .T. ) ;
#21286 = AXIS2_PLACEMENT_3D ( 'NONE', #50484, #12158, #57152 ) ;
#21287 = ORIENTED_EDGE ( 'NONE', *, *, #9693, .F. ) ;
#21288 = CARTESIAN_POINT ( 'NONE',  ( -31.43908319763710679, -170.0000000000000000, 37.71645440618917888 ) ) ;
#21289 = ITEM_DEFINED_TRANSFORMATION ( 'NONE', 'NONE', #12993,  #66832 ) ;
#21290 = CARTESIAN_POINT ( 'NONE',  ( 176.6258282025055166, 74.21441092921637050, 30.77301370930646840 ) ) ;
#21291 = DIRECTION ( 'NONE',  ( -0.000000000000000000, 1.000000000000000000, -0.000000000000000000 ) ) ;
#21292 = CARTESIAN_POINT ( 'NONE',  ( 40.37438610703016906, 8.537526699166111399, -77.41724195684747656 ) ) ;
#21293 = AXIS2_PLACEMENT_3D ( 'NONE', #39648, #54767, #34030 ) ;
#21294 = DIRECTION ( 'NONE',  ( -1.000000000000000000, 0.000000000000000000, 0.000000000000000000 ) ) ;
#21295 = ORIENTED_EDGE ( 'NONE', *, *, #53514, .F. ) ;
#21296 = EDGE_LOOP ( 'NONE', ( #63587, #24238, #110, #66143 ) ) ;
#21297 = DIRECTION ( 'NONE',  ( 0.000000000000000000, 0.000000000000000000, -1.000000000000000000 ) ) ;
#21298 = CARTESIAN_POINT ( 'NONE',  ( 174.6746562023443801, 72.36198225676386642, 94.41010371319214300 ) ) ;
#21299 = ORIENTED_EDGE ( 'NONE', *, *, #14837, .F. ) ;
#21300 = CARTESIAN_POINT ( 'NONE',  ( 116.1021807117072058, 31.68810634233422974, 68.66407567072008078 ) ) ;
#21301 = VERTEX_POINT ( 'NONE', #43128 ) ;
#21302 = CARTESIAN_POINT ( 'NONE',  ( 132.9453095272139649, 42.04754713161464252, -62.86786152285933582 ) ) ;
#21303 = CARTESIAN_POINT ( 'NONE',  ( 128.0568017572569488, 38.03085713813911184, 32.22834714527665056 ) ) ;
#21304 = LINE ( 'NONE', #37478, #9526 ) ;
#21305 = CARTESIAN_POINT ( 'NONE',  ( 84.66625268040917263, 18.76025835477234693, -89.76113623899809113 ) ) ;
#21306 = CARTESIAN_POINT ( 'NONE',  ( -119.1064753703575718, -170.0000000000000000, 94.99999999999866418 ) ) ;
#21307 = DIRECTION ( 'NONE',  ( 0.000000000000000000, 0.000000000000000000, 1.000000000000000000 ) ) ;
#21308 = B_SPLINE_CURVE_WITH_KNOTS ( 'NONE', 3,
 ( #13544, #46930, #62420, #34666, #29717, #68393, #51860, #19156, #14574, #56103, #40610, #2640, #35698, #8264, #8621, #14237, #25144, #45542, #51179, #67025, #18816, #24453, #35343, #56802, #45894, #67365, #459, #52877, #10321, #9648, #43007, #58174, #52546, #53567, #5046, #63803, #20884, #47947, #32475, #48279, #11011, #21913, #15266, #4705, #26853, #64483, #41993, #58851, #43362, #69416, #107, #36729 ),
 .UNSPECIFIED., .F., .F.,
 ( 4, 2, 2, 2, 2, 2, 2, 2, 2, 2, 2, 2, 2, 2, 2, 2, 2, 2, 2, 2, 2, 2, 2, 2, 2, 4 ),
 ( 0.000000000000000000, 0.002274976238400359084, 0.004549952476800718168, 0.005687440596000920695, 0.006824928715201121487, 0.007962416834401324015, 0.009099904953601524807, 0.01023739307280172733, 0.01137488119200192986, 0.01364985743040229675, 0.01592483366880266538, 0.01706232178800288005, 0.01819980990720309125, 0.02047478614560356569, 0.02274976238400404360, 0.02388725050320428950, 0.02502473862240453192, 0.02729971486080498902, 0.02843720298000524879, 0.02957469109920550163, 0.03071217921840575446, 0.03184966733760600383, 0.03298715545680625666, 0.03412464357600650949, 0.03526213169520676233, 0.03639961981440701516 ),
 .UNSPECIFIED. ) ;
#21309 = VERTEX_POINT ( 'NONE', #54370 ) ;
#21310 = ORIENTED_EDGE ( 'NONE', *, *, #26122, .T. ) ;
#21311 = DIRECTION ( 'NONE',  ( -1.850371928290090422E-16, 1.000000000000000000, 1.110223024625156171E-16 ) ) ;
#21312 = FACE_BOUND ( 'NONE', #9365, .T. ) ;
#21313 = CARTESIAN_POINT ( 'NONE',  ( -149.5074843970970733, 65.50121172469319220, -34.81283053149196149 ) ) ;
#21314 = CARTESIAN_POINT ( 'NONE',  ( -169.1116812882276861, 84.24296059722695418, -62.70237070590246731 ) ) ;
#21316 = ORIENTED_EDGE ( 'NONE', *, *, #19770, .F. ) ;
#21315 = CARTESIAN_POINT ( 'NONE',  ( -144.2188519266539970, 59.82027639618911508, -47.63651262692244615 ) ) ;
#21317 = CARTESIAN_POINT ( 'NONE',  ( -7.825402957745087207, -170.0000000000000000, -8.573520141480127421 ) ) ;
#21318 = AXIS2_PLACEMENT_3D ( 'NONE', #54018, #60004, #38559 ) ;
#21319 = VERTEX_POINT ( 'NONE', #63564 ) ;
#21321 = ADVANCED_FACE ( 'NONE', ( #59647, #38206 ), #42447, .T. ) ;
#21320 = DIRECTION ( 'NONE',  ( -1.000000000000000000, -0.000000000000000000, -0.000000000000000000 ) ) ;
#21322 = FACE_OUTER_BOUND ( 'NONE', #56192, .T. ) ;
#21323 = CARTESIAN_POINT ( 'NONE',  ( 80.17205177205136124, 17.31791394718354837, -20.30016712999428918 ) ) ;
#21324 = CARTESIAN_POINT ( 'NONE',  ( -128.9863978264384627, 49.78205252558956317, -62.42159899320021310 ) ) ;
#21325 = DIRECTION ( 'NONE',  ( -0.000000000000000000, -0.000000000000000000, -1.000000000000000000 ) ) ;
#21326 = CARTESIAN_POINT ( 'NONE',  ( -95.50384525802328994, 29.46973564057716999, 14.39913645707428280 ) ) ;
#21327 = CARTESIAN_POINT ( 'NONE',  ( -95.21430597939259144, 29.33390900154318004, -71.92457073492782627 ) ) ;
#21328 = VERTEX_POINT ( 'NONE', #10094 ) ;
#21329 = VERTEX_POINT ( 'NONE', #58615 ) ;
#21330 = CARTESIAN_POINT ( 'NONE',  ( 181.0840389613909736, 78.60582251573003987, -78.06960825634331513 ) ) ;
#21331 = CARTESIAN_POINT ( 'NONE',  ( 69.77839676787858991, 27.52340539440040956, 170.0000000000000000 ) ) ;
#21332 = CARTESIAN_POINT ( 'NONE',  ( -165.7689197919845014, 79.30072199592278537, -40.70117905480101683 ) ) ;
#21333 = FACE_OUTER_BOUND ( 'NONE', #52946, .T. ) ;
#21334 = VECTOR ( 'NONE', #41898, 1000.000000000000000 ) ;
#21335 = CARTESIAN_POINT ( 'NONE',  ( 109.7782172510783454, 29.77507867835874933, -77.76698815611737814 ) ) ;
#21336 = CARTESIAN_POINT ( 'NONE',  ( -78.18897186942402300, 23.21604822208489338, 45.41820113967314398 ) ) ;
#21337 = CARTESIAN_POINT ( 'NONE',  ( 82.14449817946434962, 17.93919511903895625, 43.22844623160558086 ) ) ;
#21338 = FACE_OUTER_BOUND ( 'NONE', #63270, .T. ) ;
#21339 = CARTESIAN_POINT ( 'NONE',  ( 42.71680114082827373, 9.880016734137544887, -36.37429557171203243 ) ) ;
#21340 = CARTESIAN_POINT ( 'NONE',  ( 99.71998884745383407, 190.0000000000000000, 7.478223336038896996 ) ) ;
#21341 = ORIENTED_EDGE ( 'NONE', *, *, #28865, .T. ) ;
#21342 = CARTESIAN_POINT ( 'NONE',  ( 204.6977192012829789, 108.0580384837234931, -9.481380442157895772 ) ) ;
#21343 = EDGE_CURVE ( 'NONE', #61832, #28258, #27299, .T. ) ;
#21344 = ORIENTED_EDGE ( 'NONE', *, *, #40258, .F. ) ;
#21345 = CARTESIAN_POINT ( 'NONE',  ( -9.525868120571905351, 7.007646177566255297, -35.60930802222527092 ) ) ;
#21346 = CARTESIAN_POINT ( 'NONE',  ( -33.97702052856965338, 17.74986603947969144, 13.32819397642332504 ) ) ;
#21347 = CARTESIAN_POINT ( 'NONE',  ( 88.53025347111699261, 21.14438024052374132, 56.78577616652550830 ) ) ;
#21348 = CARTESIAN_POINT ( 'NONE',  ( 110.2429982417149432, 29.99119854320847267, 2.766663615273645682 ) ) ;
#21349 = DIRECTION ( 'NONE',  ( 1.000000000000000000, 0.000000000000000000, 0.000000000000000000 ) ) ;
#21350 = CARTESIAN_POINT ( 'NONE',  ( 31.95008798096003844, 7.556925044648910905, -68.98185651406271290 ) ) ;
#21351 = CARTESIAN_POINT ( 'NONE',  ( 15.78827728214693416, 7.507518794609589818, -50.51894409868581448 ) ) ;
#21352 = ADVANCED_FACE ( 'NONE', ( #6198 ), #43473, .T. ) ;
#21353 = VECTOR ( 'NONE', #47885, 1000.000000000000000 ) ;
#21354 = DIRECTION ( 'NONE',  ( -1.000000000000000000, 0.000000000000000000, 0.000000000000000000 ) ) ;
#21355 = ORIENTED_EDGE ( 'NONE', *, *, #34936, .F. ) ;
#21356 = CARTESIAN_POINT ( 'NONE',  ( 35.38849253846352383, 46.38061039241811301, 27.58472369417912162 ) ) ;
#21357 = EDGE_LOOP ( 'NONE', ( #9766, #43430, #29429, #40306 ) ) ;
#21358 = LINE ( 'NONE', #4500, #25046 ) ;
#21359 = CARTESIAN_POINT ( 'NONE',  ( 8.540564391411901823, 7.383006541823028179, -71.80808571654557682 ) ) ;
#21360 = DIRECTION ( 'NONE',  ( 1.000000000000000000, -0.000000000000000000, 0.000000000000000000 ) ) ;
#21361 = CARTESIAN_POINT ( 'NONE',  ( 0.000000000000000000, 0.000000000000000000, 2.499999999999999556 ) ) ;
#21362 = CARTESIAN_POINT ( 'NONE',  ( -4.955782654901479845, 6.720825733572404204, 30.67341288399633115 ) ) ;
#21363 = CARTESIAN_POINT ( 'NONE',  ( -97.47339919287394139, 30.40512551257286944, -9.891953464162076770 ) ) ;
#21364 = CARTESIAN_POINT ( 'NONE',  ( 93.47266763748514506, 22.94549330578766089, 87.81307861244059154 ) ) ;
#21365 = EDGE_CURVE ( 'NONE', #66442, #42365, #55394, .T. ) ;
#21366 = ORIENTED_EDGE ( 'NONE', *, *, #4574, .T. ) ;
#21367 = DIRECTION ( 'NONE',  ( 0.9108602745606099171, 0.4127148655274851530, -6.798829950883235577E-15 ) ) ;
#21368 = AXIS2_PLACEMENT_3D ( 'NONE', #14186, #51127, #51478 ) ;
#21369 = CARTESIAN_POINT ( 'NONE',  ( 8.000000000000001776, -3.867591403079185142, -9.002324684675414801 ) ) ;
#21371 = EDGE_CURVE ( 'NONE', #5465, #65127, #37510, .T. ) ;
#21370 = CARTESIAN_POINT ( 'NONE',  ( -133.3149301983942507, 51.57857650535024163, 12.39399621277310004 ) ) ;
#21372 = EDGE_CURVE ( 'NONE', #67311, #47553, #21000, .T. ) ;
#21373 = CARTESIAN_POINT ( 'NONE',  ( -105.8683518445188980, 35.77995342500074827, 58.26050255926607235 ) ) ;
#21374 = ITEM_DEFINED_TRANSFORMATION ( 'NONE', 'NONE', #17531,  #66832 ) ;
#21375 = CARTESIAN_POINT ( 'NONE',  ( -133.3220917939969752, 52.82057604964900577, -41.34405810791972868 ) ) ;
#21376 = VERTEX_POINT ( 'NONE', #69172 ) ;
#21377 = LINE ( 'NONE', #59687, #31146 ) ;
#21378 = CARTESIAN_POINT ( 'NONE',  ( 92.21267147730743829, 21.40196534721317434, 69.08802095801497956 ) ) ;
#21379 =( NAMED_UNIT ( * ) PLANE_ANGLE_UNIT ( ) SI_UNIT ( $, .RADIAN. ) );
#21380 = CARTESIAN_POINT ( 'NONE',  ( -145.9244519207070141, 61.19885883688223771, 85.31486399595573289 ) ) ;
#21381 = LINE ( 'NONE', #64296, #25682 ) ;
#21382 = ORIENTED_EDGE ( 'NONE', *, *, #8011, .T. ) ;
#21383 = DIRECTION ( 'NONE',  ( 1.000000000000000000, -0.000000000000000000, 0.000000000000000000 ) ) ;
#21384 = CARTESIAN_POINT ( 'NONE',  ( 79.33384730094452664, 18.11203072455030849, 8.609877271889105899 ) ) ;
#21385 = CYLINDRICAL_SURFACE ( 'NONE', #53308, 246.3582898394607241 ) ;
#21386 = CARTESIAN_POINT ( 'NONE',  ( -125.8938041572051389, -170.0000000000000000, -23.06915330777029638 ) ) ;
#21387 = VECTOR ( 'NONE', #3411, 1000.000000000000000 ) ;
#21388 = ORIENTED_EDGE ( 'NONE', *, *, #50363, .T. ) ;
#21389 = CARTESIAN_POINT ( 'NONE',  ( -149.5074843970970733, 65.50121172469317798, -61.65738112195564469 ) ) ;
#21390 = ORIENTED_EDGE ( 'NONE', *, *, #58327, .T. ) ;
#21391 = CARTESIAN_POINT ( 'NONE',  ( 56.42997683260146857, -32.25922681454192542, 170.0000000000000000 ) ) ;
#21392 = CARTESIAN_POINT ( 'NONE',  ( 66.72974708835175761, 13.56459745268607087, -76.59956076421927662 ) ) ;
#21393 = LINE ( 'NONE', #63964, #8115 ) ;
#21394 = B_SPLINE_CURVE_WITH_KNOTS ( 'NONE', 3,
 ( #6959, #49857, #60766, #50222, #1688, #27710, #991, #12591, #55487, #65361, #33359, #6612, #12949, #51950, #2730, #14327, #46671, #13972, #3763, #40011, #61472, #50915 ),
 .UNSPECIFIED., .F., .F.,
 ( 4, 2, 2, 2, 2, 2, 2, 2, 2, 2, 4 ),
 ( 0.000000000000000000, 0.001288289306256240390, 0.002576578612512480781, 0.003864867918768720954, 0.005153157225024961562, 0.006441446531281201301, 0.007085591184409312064, 0.007729735837537421092, 0.009018025143793640883, 0.009662169796921762921, 0.01030631445004988149 ),
 .UNSPECIFIED. ) ;
#21396 = ORIENTED_EDGE ( 'NONE', *, *, #56242, .F. ) ;
#21395 = CARTESIAN_POINT ( 'NONE',  ( 51.39999999999999858, 0.000000000000000000, 0.000000000000000000 ) ) ;
#21397 = CARTESIAN_POINT ( 'NONE',  ( -177.1540936177023298, 91.73126115633628785, 31.98316566157747332 ) ) ;
#21398 = CIRCLE ( 'NONE', #52829, 4.250000000000000000 ) ;
#21399 = DIRECTION ( 'NONE',  ( -0.000000000000000000, -0.000000000000000000, -1.000000000000000000 ) ) ;
#21400 = CARTESIAN_POINT ( 'NONE',  ( 55.46196446482127840, -34.59309596431295120, 43.58025477438756212 ) ) ;
#21401 = ORIENTED_EDGE ( 'NONE', *, *, #26599, .F. ) ;
#21402 = ADVANCED_FACE ( 'NONE', ( #31551 ), #10778, .T. ) ;
#21403 = CARTESIAN_POINT ( 'NONE',  ( 0.000000000000000000, 0.000000000000000000, -20.00000000000000000 ) ) ;
#21404 = ADVANCED_BREP_SHAPE_REPRESENTATION ( '', ( #65110, #18036, #66832 ), #17430 ) ;
#21405 = EDGE_CURVE ( 'NONE', #68305, #68932, #31899, .T. ) ;
#21406 = LINE ( 'NONE', #64319, #34265 ) ;
#21407 = CARTESIAN_POINT ( 'NONE',  ( -173.1211646369891355, 88.63826465341151106, 30.82169460664101734 ) ) ;
#21408 = CARTESIAN_POINT ( 'NONE',  ( 126.4318266066171930, 38.27072266789465971, 62.76314339832654809 ) ) ;
#21409 = ORIENTED_EDGE ( 'NONE', *, *, #18655, .F. ) ;
#21410 = ORIENTED_EDGE ( 'NONE', *, *, #788, .T. ) ;
#21411 = EDGE_LOOP ( 'NONE', ( #55505, #18773 ) ) ;
#21412 = VECTOR ( 'NONE', #50867, 1000.000000000000000 ) ;
#21413 = CARTESIAN_POINT ( 'NONE',  ( -36.11269837220801548, 31.11269837220812207, 85.00100000000000477 ) ) ;
#21414 = CARTESIAN_POINT ( 'NONE',  ( -47.66823188586783289, 12.82507252420411881, 92.85681623549952235 ) ) ;
#21415 = DIRECTION ( 'NONE',  ( -0.000000000000000000, -0.000000000000000000, -1.000000000000000000 ) ) ;
#21416 = DIRECTION ( 'NONE',  ( -2.168404344971009361E-16, 0.000000000000000000, 1.000000000000000000 ) ) ;
#21417 = CARTESIAN_POINT ( 'NONE',  ( 69.97872708500212013, 14.39620413031757629, 93.80885834994377603 ) ) ;
#21418 = DIRECTION ( 'NONE',  ( -0.000000000000000000, -0.000000000000000000, -1.000000000000000000 ) ) ;
#21419 = EDGE_CURVE ( 'NONE', #19763, #31093, #21679, .T. ) ;
#21420 = CARTESIAN_POINT ( 'NONE',  ( -132.2199390322348336, 50.80243550247265460, 69.02423031754652527 ) ) ;
#21421 = DIRECTION ( 'NONE',  ( 0.000000000000000000, -0.000000000000000000, -1.000000000000000000 ) ) ;
#21422 = ADVANCED_FACE ( 'NONE', ( #21333 ), #26957, .T. ) ;
#21423 = EDGE_LOOP ( 'NONE', ( #45279, #34765 ) ) ;
#21424 = CARTESIAN_POINT ( 'NONE',  ( -100.6199109870225641, 33.06995330681461098, -88.87768113824378702 ) ) ;
#21425 = ORIENTED_EDGE ( 'NONE', *, *, #67351, .T. ) ;
#21426 = CARTESIAN_POINT ( 'NONE',  ( -78.18897186942403721, 23.21604822208489338, 72.26275173013684139 ) ) ;
#21427 = CARTESIAN_POINT ( 'NONE',  ( 212.1962110267000128, 117.2292732107321171, -71.04714369557829912 ) ) ;
#21428 = EDGE_CURVE ( 'NONE', #64962, #40175, #32250, .T. ) ;
#21429 = CARTESIAN_POINT ( 'NONE',  ( 56.19211641164837800, 11.19288081156168602, -73.18788659422385479 ) ) ;
#21430 = CARTESIAN_POINT ( 'NONE',  ( -76.31381168750409927, 21.43908608416555239, 18.21112609344433864 ) ) ;
#21431 = CARTESIAN_POINT ( 'NONE',  ( -20.55634918610411077, -41.66904755831209428, 85.00100000000000477 ) ) ;
#21432 = CARTESIAN_POINT ( 'NONE',  ( 112.3013380801406669, 395.0000000000010800, 91.05029585798746439 ) ) ;
#21433 = EDGE_CURVE ( 'NONE', #3016, #60863, #53120, .T. ) ;
#21434 = DIRECTION ( 'NONE',  ( 0.000000000000000000, 0.000000000000000000, 1.000000000000000000 ) ) ;
#21435 = ORIENTED_EDGE ( 'NONE', *, *, #47078, .F. ) ;
#21436 = DIRECTION ( 'NONE',  ( 0.000000000000000000, -1.000000000000000000, 0.000000000000000000 ) ) ;
#21437 = CARTESIAN_POINT ( 'NONE',  ( 45.82394788922869822, -46.11928342727429708, 41.38025477438755928 ) ) ;
#21438 = ORIENTED_EDGE ( 'NONE', *, *, #14115, .T. ) ;
#21439 = ORIENTED_EDGE ( 'NONE', *, *, #25240, .T. ) ;
#21440 = CARTESIAN_POINT ( 'NONE',  ( -24.61094659556678010, 9.585225265507407499, -66.54939687623127043 ) ) ;
#21441 = CARTESIAN_POINT ( 'NONE',  ( 56.53635105806414174, 11.26263375223564012, -47.00625827598132389 ) ) ;
#21442 = SURFACE_STYLE_USAGE ( .BOTH. , #60477 ) ;
#21443 = CARTESIAN_POINT ( 'NONE',  ( 109.9975424824652634, 171.8183490441642221, 533.9018882243740336 ) ) ;
#21444 = ADVANCED_FACE ( 'NONE', ( #7253 ), #6895, .F. ) ;
#21445 = VERTEX_POINT ( 'NONE', #66703 ) ;
#21446 = AXIS2_PLACEMENT_3D ( 'NONE', #60287, #64868, #12102 ) ;
#21447 = ORIENTED_EDGE ( 'NONE', *, *, #64711, .T. ) ;
#21448 = ADVANCED_FACE ( 'NONE', ( #12886 ), #25091, .T. ) ;
#21449 = EDGE_CURVE ( 'NONE', #52445, #22995, #23445, .T. ) ;
#21450 = EDGE_CURVE ( 'NONE', #22781, #23405, #60976, .T. ) ;
#21451 = LINE ( 'NONE', #64357, #42382 ) ;
#21452 = EDGE_LOOP ( 'NONE', ( #19400, #29325 ) ) ;
#21453 = DIRECTION ( 'NONE',  ( 1.387778780781445429E-16, -1.000000000000000000, -3.081487911019577365E-33 ) ) ;
#21454 = CARTESIAN_POINT ( 'NONE',  ( -145.5195986658808920, 62.16746116576786818, 31.86476147939222514 ) ) ;
#21455 = CIRCLE ( 'NONE', #63033, 5.000000000000004441 ) ;
#21456 = LINE ( 'NONE', #4937, #56600 ) ;
#21457 = CARTESIAN_POINT ( 'NONE',  ( -6.843910203392214342, 7.836697961436722260, 71.91164237052761621 ) ) ;
#21458 = CIRCLE ( 'NONE', #43888, 4.999999999999990230 ) ;
#21459 = DIRECTION ( 'NONE',  ( 1.000000000000000000, 0.000000000000000000, 0.000000000000000000 ) ) ;
#21460 = EDGE_LOOP ( 'NONE', ( #15282, #53884, #62575, #61572, #1954, #40214, #43773, #53919, #22993 ) ) ;
#21461 = ORIENTED_EDGE ( 'NONE', *, *, #7661, .T. ) ;
#21462 = CARTESIAN_POINT ( 'NONE',  ( -1.310872448937999701, 8.480771745766400471, -0.3173508448886568911 ) ) ;
#21463 = LINE ( 'NONE', #42907, #54066 ) ;
#21464 = DIRECTION ( 'NONE',  ( -0.000000000000000000, -0.000000000000000000, 1.000000000000000000 ) ) ;
#21465 = CYLINDRICAL_SURFACE ( 'NONE', #64682, 7.500000000000013323 ) ;
#21466 = DIRECTION ( 'NONE',  ( 0.000000000000000000, 1.000000000000000000, 0.000000000000000000 ) ) ;
#21467 = VECTOR ( 'NONE', #1804, 1000.000000000000000 ) ;
#21468 = CARTESIAN_POINT ( 'NONE',  ( -189.8071159312682710, 107.8771087123619736, -71.83549201025891762 ) ) ;
#21469 = VERTEX_POINT ( 'NONE', #56128 ) ;
#21470 = CARTESIAN_POINT ( 'NONE',  ( -98.46684543088103680, 30.88557736720386515, 71.32637121160307458 ) ) ;
#21471 = ORIENTED_EDGE ( 'NONE', *, *, #26592, .F. ) ;
#21472 = CARTESIAN_POINT ( 'NONE',  ( -74.40004226286974642, 20.74218500375952345, 31.74512071546088521 ) ) ;
#21473 = ORIENTED_EDGE ( 'NONE', *, *, #45094, .F. ) ;
#21474 = EDGE_LOOP ( 'NONE', ( #13696, #62459, #1950, #30513 ) ) ;
#21475 = CARTESIAN_POINT ( 'NONE',  ( -118.8392474096542628, 43.20060570451235549, 8.676164318946312903 ) ) ;
#21476 = CARTESIAN_POINT ( 'NONE',  ( -180.6213815675304488, 95.88446356933842196, 64.85668927554371521 ) ) ;
#21477 = CARTESIAN_POINT ( 'NONE',  ( 126.4754729582248416, 37.14269484129876275, 65.21006343432689789 ) ) ;
#21478 = ORIENTED_EDGE ( 'NONE', *, *, #31218, .F. ) ;
#21479 = DIRECTION ( 'NONE',  ( 0.000000000000000000, 0.000000000000000000, -1.000000000000000000 ) ) ;
#21480 = ADVANCED_FACE ( 'NONE', ( #60368 ), #17812, .F. ) ;
#21481 = DIRECTION ( 'NONE',  ( 0.8584487936018727616, -0.5128992774058949156, 0.000000000000000000 ) ) ;
#21482 = CARTESIAN_POINT ( 'NONE',  ( 69.83617901654358207, 15.39919709983075258, 34.18378910825896355 ) ) ;
#21483 = DIRECTION ( 'NONE',  ( 1.000000000000000000, 0.000000000000000000, 0.000000000000000000 ) ) ;
#21484 = CARTESIAN_POINT ( 'NONE',  ( -28.32746765835430836, -69.45586423092646555, 170.0000000000000000 ) ) ;
#21485 = CARTESIAN_POINT ( 'NONE',  ( 31.11269837220809364, 15.55634918610396866, 2.000000000000001776 ) ) ;
#21486 = CARTESIAN_POINT ( 'NONE',  ( -27.48703802937315288, 8.975952825337598640, 44.09546302086310732 ) ) ;
#21487 = CARTESIAN_POINT ( 'NONE',  ( -143.2587158300142107, 60.34092810886537706, -65.00150092923556144 ) ) ;
#21488 = ORIENTED_EDGE ( 'NONE', *, *, #5770, .T. ) ;
#21489 = VECTOR ( 'NONE', #32532, 1000.000000000000000 ) ;
#21490 = FACE_BOUND ( 'NONE', #63417, .T. ) ;
#21491 = DIRECTION ( 'NONE',  ( -1.000000000000000000, 0.000000000000000000, 0.000000000000000000 ) ) ;
#21492 = DIRECTION ( 'NONE',  ( 0.000000000000000000, 0.000000000000000000, -1.000000000000000000 ) ) ;
#21494 = CARTESIAN_POINT ( 'NONE',  ( -84.49322488516129681, 0.000000000000000000, 43.58025477438756212 ) ) ;
#21493 = AXIS2_PLACEMENT_3D ( 'NONE', #41734, #19583, #62145 ) ;
#21495 = CARTESIAN_POINT ( 'NONE',  ( 410.0000000000000000, 190.0000000000000000, 380.0000000000000000 ) ) ;
#21496 = CARTESIAN_POINT ( 'NONE',  ( -64.83840629396348731, 4.580509716059292913, 40.00000000000003553 ) ) ;
#21497 = CARTESIAN_POINT ( 'NONE',  ( 6.526941389886052214, 24.13294503563511029, 0.000000000000000000 ) ) ;
#21498 = CARTESIAN_POINT ( 'NONE',  ( -46.66904755831212981, -10.55634918610397222, 2.000000000000001776 ) ) ;
#21499 = EDGE_CURVE ( 'NONE', #16122, #25612, #54728, .T. ) ;
#21500 = CARTESIAN_POINT ( 'NONE',  ( -119.6801029354225108, 43.71909921132878907, -73.46582779786149331 ) ) ;
#21502 = LINE ( 'NONE', #16229, #45626 ) ;
#21501 = VECTOR ( 'NONE', #25333, 1000.000000000000000 ) ;
#21503 = AXIS2_PLACEMENT_3D ( 'NONE', #11744, #33915, #64877 ) ;
#21504 = CARTESIAN_POINT ( 'NONE',  ( -83.15209219203885027, 25.16621997697721724, 70.79312038800895834 ) ) ;
#21505 = CARTESIAN_POINT ( 'NONE',  ( 42.03341093683043539, 9.782505851509640138, -89.78263700018763416 ) ) ;
#21506 = EDGE_LOOP ( 'NONE', ( #56840, #37913, #65256, #5715 ) ) ;
#21507 = LINE ( 'NONE', #26797, #52044 ) ;
#21508 = ORIENTED_EDGE ( 'NONE', *, *, #36424, .F. ) ;
#21509 = DIRECTION ( 'NONE',  ( -0.000000000000000000, 1.000000000000000000, -0.000000000000000000 ) ) ;
#21510 = EDGE_LOOP ( 'NONE', ( #30673, #53406, #47090, #18727 ) ) ;
#21511 = B_SPLINE_CURVE_WITH_KNOTS ( 'NONE', 3,
 ( #65156, #60223, #18965, #40762, #39131, #61860, #48947, #60570, #22241, #43680, #22941, #16950, #27862, #38414, #46037, #59859, #11679, #54936, #33151, #33508, #28565, #29868, #1846, #54587, #23302, #6412, #49304, #44748, #22588, #17305, #56593, #40413, #44028, #3147, #13685, #44383, #65873, #35141, #8415, #12039, #24604, #67504, #65507, #6756, #1480, #30558, #31260 ),
 .UNSPECIFIED., .F., .F.,
 ( 4, 2, 2, 2, 2, 2, 2, 2, 2, 2, 2, 2, 1, 2, 2, 2, 2, 2, 2, 2, 2, 2, 2, 4 ),
 ( 0.000000000000000000, 0.001493793014771564818, 0.002240689522157346576, 0.002987586029543128335, 0.004481379044314701826, 0.005228275551700484018, 0.005975172059086265343, 0.007468965073857845340, 0.008215861581243648348, 0.008962758088629452224, 0.01045655110340105130, 0.01120344761078684304, 0.01195034411817263130, 0.01269724062555842130, 0.01344413713294421130, 0.01493793014771577221, 0.01568482665510154486, 0.01643172316248732098, 0.01792551617725886975, 0.01941930919203041853, 0.02016620569941620159, 0.02091310220680198464, 0.02240689522157354036, 0.02390068823634509954 ),
 .UNSPECIFIED. ) ;
#21512 = ADVANCED_FACE ( 'NONE', ( #28713 ), #60710, .T. ) ;
#21513 = CARTESIAN_POINT ( 'NONE',  ( 39.40195752203892710, -170.0000000000000000, 44.91383430596327742 ) ) ;
#21514 = CARTESIAN_POINT ( 'NONE',  ( 112.4855833589208629, 31.04769103621673310, 83.63625584413014735 ) ) ;
#21515 = CARTESIAN_POINT ( 'NONE',  ( 410.0000000000000000, 0.000000000000000000, 0.000000000000000000 ) ) ;
#21516 = CARTESIAN_POINT ( 'NONE',  ( 70.46452034227870342, 14.52462608639673292, -17.38126288549829113 ) ) ;
#21517 = VECTOR ( 'NONE', #29572, 1000.000000000000227 ) ;
#21518 = CARTESIAN_POINT ( 'NONE',  ( 135.0005116824454490, 43.29964618809726318, -50.93914690418067437 ) ) ;
#21519 = CARTESIAN_POINT ( 'NONE',  ( -47.55316895016325418, 13.83165595246917157, -69.05820636316589400 ) ) ;
#21520 = DIRECTION ( 'NONE',  ( -0.000000000000000000, -0.000000000000000000, -1.000000000000000000 ) ) ;
#21521 = DIRECTION ( 'NONE',  ( 0.000000000000000000, 0.000000000000000000, 1.000000000000000000 ) ) ;
#21522 = EDGE_LOOP ( 'NONE', ( #4725, #15252, #36070, #43614 ) ) ;
#21523 = ORIENTED_EDGE ( 'NONE', *, *, #51917, .F. ) ;
#21524 = CARTESIAN_POINT ( 'NONE',  ( 37.70910994512002645, 9.209110272746707793, 56.94781516157431156 ) ) ;
#21525 = CARTESIAN_POINT ( 'NONE',  ( 184.0270137565624964, 83.08990924474782958, 83.57409603390661346 ) ) ;
#21526 = LINE ( 'NONE', #15912, #7203 ) ;
#21527 = DIRECTION ( 'NONE',  ( -2.921639538487254261E-16, -1.134144525784205431E-35, -1.000000000000000000 ) ) ;
#21528 = VERTEX_POINT ( 'NONE', #1987 ) ;
#21529 = EDGE_CURVE ( 'NONE', #68932, #4035, #51481, .T. ) ;
#21530 = CARTESIAN_POINT ( 'NONE',  ( 91.67776154311745529, 22.27748043241296472, 15.91940090679946174 ) ) ;
#21531 = CARTESIAN_POINT ( 'NONE',  ( -10.46803069297985900, 7.077485182625207649, 71.48343882395781179 ) ) ;
#21532 = CARTESIAN_POINT ( 'NONE',  ( 212.0075063341774069, 118.7912820769029594, 8.154294459840707887 ) ) ;
#21533 = DIRECTION ( 'NONE',  ( 0.000000000000000000, 0.000000000000000000, -1.000000000000000000 ) ) ;
#21534 = CARTESIAN_POINT ( 'NONE',  ( 46.90222083990963142, 9.503928413859229707, -16.03507805835512556 ) ) ;
#21535 = CARTESIAN_POINT ( 'NONE',  ( 0.000000000000000000, 0.000000000000000000, 7.000000000000000000 ) ) ;
#21536 = CARTESIAN_POINT ( 'NONE',  ( -452.6627218934913230, 399.9999999999998863, 113.5502958579881749 ) ) ;
#21537 = EDGE_CURVE ( 'NONE', #43634, #66845, #12184, .T. ) ;
#21538 = LINE ( 'NONE', #10985, #64735 ) ;
#21539 = ORIENTED_EDGE ( 'NONE', *, *, #48256, .T. ) ;
#21540 = CARTESIAN_POINT ( 'NONE',  ( 129.1052153257904251, 39.78893484542955861, 15.98927307743317350 ) ) ;
#21541 = CARTESIAN_POINT ( 'NONE',  ( 91.67776154311745529, 22.27748043241296472, -37.76970027412789932 ) ) ;
#21542 = AXIS2_PLACEMENT_3D ( 'NONE', #45788, #55639, #67266 ) ;
#21543 = DIRECTION ( 'NONE',  ( 0.000000000000000000, 0.000000000000000000, -1.000000000000000000 ) ) ;
#21544 = LINE ( 'NONE', #32804, #36577 ) ;
#21545 = CARTESIAN_POINT ( 'NONE',  ( 150.7926588734435427, 52.63999027731879465, 13.48961824798760745 ) ) ;
#21546 = CARTESIAN_POINT ( 'NONE',  ( -14.86245480583235690, 8.462548703819992468, 88.69022230593746770 ) ) ;
#21547 = VECTOR ( 'NONE', #35867, 1000.000000000000000 ) ;
#21548 = ORIENTED_EDGE ( 'NONE', *, *, #5009, .T. ) ;
#21549 = CARTESIAN_POINT ( 'NONE',  ( 62.04664474957769471, 12.44961624115901522, 17.92119150936918004 ) ) ;
#21550 = CARTESIAN_POINT ( 'NONE',  ( 6.400000000000000355, 0.000000000000000000, 0.000000000000000000 ) ) ;
#21551 = ORIENTED_EDGE ( 'NONE', *, *, #63129, .T. ) ;
#21552 = CIRCLE ( 'NONE', #30565, 65.00000000000000000 ) ;
#21553 = AXIS2_PLACEMENT_3D ( 'NONE', #53097, #9179, #4925 ) ;
#21554 = ORIENTED_EDGE ( 'NONE', *, *, #13522, .T. ) ;
#21555 = DIRECTION ( 'NONE',  ( -0.9009688679024218105, 0.4338837391175526248, 0.000000000000000000 ) ) ;
#21556 = LINE ( 'NONE', #42672, #47852 ) ;
#21557 = CARTESIAN_POINT ( 'NONE',  ( 90.91356992076214283, 21.99794663086830937, -64.00549692677411429 ) ) ;
#21558 = ORIENTED_EDGE ( 'NONE', *, *, #15706, .F. ) ;
#21559 = VECTOR ( 'NONE', #30939, 1000.000000000000000 ) ;
#21560 = CARTESIAN_POINT ( 'NONE',  ( -56.96214175905167565, 15.20165595797839586, -62.30395517612640077 ) ) ;
#21561 = CLOSED_SHELL ( 'NONE', ( #53740, #29963, #1832, #53099 ) ) ;
#21562 = CARTESIAN_POINT ( 'NONE',  ( -0.5178428571329638519, 7.532057582089302095, 12.47706993293499522 ) ) ;
#21563 = CARTESIAN_POINT ( 'NONE',  ( 174.2468109002382732, 73.34092405459590225, -40.63028982688571489 ) ) ;
#21564 = LINE ( 'NONE', #14908, #158 ) ;
#21565 = CARTESIAN_POINT ( 'NONE',  ( 34.76618902119821541, -54.93755186520709799, 43.58025477438756923 ) ) ;
#21566 = ADVANCED_FACE ( 'NONE', ( #17087 ), #49761, .T. ) ;
#21567 = ORIENTED_EDGE ( 'NONE', *, *, #25102, .T. ) ;
#21568 = CARTESIAN_POINT ( 'NONE',  ( -47.94960849910474110, 13.92522873833625141, -40.25875785308206645 ) ) ;
#21569 = ADVANCED_FACE ( 'NONE', ( #23086 ), #61406, .F. ) ;
#21570 = CARTESIAN_POINT ( 'NONE',  ( 0.000000000000000000, 0.000000000000000000, 15.70156211871650775 ) ) ;
#21571 = CARTESIAN_POINT ( 'NONE',  ( 8.336237313193160858, 7.382629160459399209, 38.49233202133056864 ) ) ;
#21572 = LINE ( 'NONE', #1168, #58505 ) ;
#21573 = FACE_OUTER_BOUND ( 'NONE', #52217, .T. ) ;
#21575 = EDGE_LOOP ( 'NONE', ( #62682, #36983, #35955, #40340 ) ) ;
#21574 = FACE_OUTER_BOUND ( 'NONE', #11700, .T. ) ;
#21576 = ORIENTED_EDGE ( 'NONE', *, *, #47700, .F. ) ;
#21577 = ORIENTED_EDGE ( 'NONE', *, *, #61694, .T. ) ;
#21578 = CARTESIAN_POINT ( 'NONE',  ( -4.707385604365774134E-15, -6.732211846623389562, 4.339467034331192963 ) ) ;
#21579 = CARTESIAN_POINT ( 'NONE',  ( -51.99406906667273631, 13.88268392809765217, 44.66953586812910260 ) ) ;
#21580 = CARTESIAN_POINT ( 'NONE',  ( -2.645453300864630819E-14, -15.55634918610403616, 2.000000000000001776 ) ) ;
#21581 = CARTESIAN_POINT ( 'NONE',  ( 60.00000000000000000, 7.347880794884118356E-15, -5.000000000000000000 ) ) ;
#21582 = EDGE_CURVE ( 'NONE', #9188, #10959, #1275, .T. ) ;
#21583 = CARTESIAN_POINT ( 'NONE',  ( -62.54086041493278714, 17.86944394914986489, -42.22520487807840084 ) ) ;
#21584 = CARTESIAN_POINT ( 'NONE',  ( 3.000000000000028866, 0.000000000000000000, -3.000000000000030198 ) ) ;
#21585 = CARTESIAN_POINT ( 'NONE',  ( 149.9838583332407893, 52.05699766415858676, -70.99723250371756933 ) ) ;
#21586 = CARTESIAN_POINT ( 'NONE',  ( 19.75784582661440680, 6.660183274347839522, -9.806260835590238756 ) ) ;
#21587 = EDGE_LOOP ( 'NONE', ( #11226, #23255, #14120, #11818 ) ) ;
#21588 = CARTESIAN_POINT ( 'NONE',  ( -156.6819053601226415, 70.51177710383656461, -40.05411599417865176 ) ) ;
#21589 = ORIENTED_EDGE ( 'NONE', *, *, #13101, .T. ) ;
#21591 = EDGE_CURVE ( 'NONE', #45287, #13481, #27777, .T. ) ;
#21590 =( REPRESENTATION_RELATIONSHIP ('NONE','NONE', #40274, #64096 ) REPRESENTATION_RELATIONSHIP_WITH_TRANSFORMATION ( #60745 )SHAPE_REPRESENTATION_RELATIONSHIP( ) );
#21592 = ORIENTED_EDGE ( 'NONE', *, *, #39554, .F. ) ;
#21593 = EDGE_CURVE ( 'NONE', #47929, #17237, #9311, .T. ) ;
#21594 = FACE_OUTER_BOUND ( 'NONE', #64207, .T. ) ;
#21595 = VECTOR ( 'NONE', #48867, 999.9999999999998863 ) ;
#21596 = CARTESIAN_POINT ( 'NONE',  ( -82.33596576276353574, 24.83688096733770934, -36.05641134141605164 ) ) ;
#21597 = CARTESIAN_POINT ( 'NONE',  ( -24.07713913638673731, 9.513388522963451166, 92.87435816855477810 ) ) ;
#21598 = CARTESIAN_POINT ( 'NONE',  ( -153.6994314938756077, 69.16570456337670691, 17.61204298921591516 ) ) ;
#21599 = ADVANCED_FACE ( 'NONE', ( #62798 ), #45573, .T. ) ;
#21600 = CIRCLE ( 'NONE', #14878, 24.99999999999985434 ) ;
#21601 = FACE_BOUND ( 'NONE', #12605, .T. ) ;
#21602 = CARTESIAN_POINT ( 'NONE',  ( 22.29513692215318343, 6.796052026456514739, 33.75287157804441307 ) ) ;
#21603 = DIRECTION ( 'NONE',  ( 0.000000000000000000, 0.000000000000000000, 1.000000000000000000 ) ) ;
#21604 = VERTEX_POINT ( 'NONE', #35726 ) ;
#21605 = VERTEX_POINT ( 'NONE', #40300 ) ;
#21606 = ORIENTED_EDGE ( 'NONE', *, *, #46598, .F. ) ;
#21607 = AXIS2_PLACEMENT_3D ( 'NONE', #23866, #66793, #18581 ) ;
#21608 = CARTESIAN_POINT ( 'NONE',  ( -152.9143627383494959, 68.46626892668653852, -8.771231553591714913 ) ) ;
#21609 = CARTESIAN_POINT ( 'NONE',  ( 32.66883187925819954, 8.640402022338109944, -46.46001169007210763 ) ) ;
#21610 = B_SPLINE_CURVE_WITH_KNOTS ( 'NONE', 3,
 ( #23372, #45851, #39878, #55713, #28995, #45148 ),
 .UNSPECIFIED., .F., .F.,
 ( 4, 2, 4 ),
 ( 2.380731629582122378E-07, 0.002336973833157555101, 0.004673709593152151377 ),
 .UNSPECIFIED. ) ;
#21611 = CARTESIAN_POINT ( 'NONE',  ( -34.51918258780366955, 10.11719938103012417, 57.71828778730281329 ) ) ;
#21612 = DIRECTION ( 'NONE',  ( 0.000000000000000000, 1.000000000000000000, 0.000000000000000000 ) ) ;
#21613 = VERTEX_POINT ( 'NONE', #68422 ) ;
#21614 = CARTESIAN_POINT ( 'NONE',  ( 181.5079096844946491, 80.47139261082472217, 56.15314469597509373 ) ) ;
#21615 = LINE ( 'NONE', #27938, #56259 ) ;
#21616 = SHAPE_REPRESENTATION_RELATIONSHIP ( 'NONE' , 'NONE' ,  #55473, #60914 ) ;
#21617 = CARTESIAN_POINT ( 'NONE',  ( 23.28809538736928531, 7.864824219997530008, 11.16234900110744732 ) ) ;
#21618 = CARTESIAN_POINT ( 'NONE',  ( 106.0171289417044136, 26.97542621030656207, 16.46741202603713816 ) ) ;
#21619 = CARTESIAN_POINT ( 'NONE',  ( 56.74421265833604622, -32.44697398030825752, 41.38025477438755928 ) ) ;
#21620 = CARTESIAN_POINT ( 'NONE',  ( -85.35127931077731489, 24.98147633333001494, -46.02518267684259001 ) ) ;
#21622 = ADVANCED_FACE ( 'NONE', ( #20225 ), #67392, .F. ) ;
#21621 = CARTESIAN_POINT ( 'NONE',  ( 22.89634831467700593, 6.832298124325686395, 66.76462710434758208 ) ) ;
#21623 = PLANE ( 'NONE',  #41096 ) ;
#21624 = CARTESIAN_POINT ( 'NONE',  ( 8.288104306525687193, 6.376394648992966374, -70.35007307862180426 ) ) ;
#21625 = ORIENTED_EDGE ( 'NONE', *, *, #19695, .T. ) ;
#21626 = CARTESIAN_POINT ( 'NONE',  ( -417.6627218934913230, 219.4906275429376308, -144.4497041420118819 ) ) ;
#21627 = APPLICATION_PROTOCOL_DEFINITION ( 'draft international standard', 'automotive_design', 1998, #14326 ) ;
#21628 = CARTESIAN_POINT ( 'NONE',  ( 173.5843421840238250, 71.34465141434345981, 37.11183576288200925 ) ) ;
#21629 = DIRECTION ( 'NONE',  ( -0.000000000000000000, 1.000000000000000000, -0.000000000000000000 ) ) ;
#21630 = CARTESIAN_POINT ( 'NONE',  ( 45.90128843543705983, 9.343910238294478532, -73.73932652712356628 ) ) ;
#21631 = CARTESIAN_POINT ( 'NONE',  ( 56.29445224195347919, 12.24017809212661767, -73.42969269962038936 ) ) ;
#21632 = ORIENTED_EDGE ( 'NONE', *, *, #62427, .F. ) ;
#21633 = VERTEX_POINT ( 'NONE', #57176 ) ;
#21634 = LINE ( 'NONE', #43083, #29135 ) ;
#21635 = CARTESIAN_POINT ( 'NONE',  ( 198.7129816317746815, 100.1061386900356354, 14.39133888418318463 ) ) ;
#21636 = VERTEX_POINT ( 'NONE', #57519 ) ;
#21637 = ORIENTED_EDGE ( 'NONE', *, *, #36373, .F. ) ;
#21638 = CARTESIAN_POINT ( 'NONE',  ( 115.7561705820728832, 31.51689401996054940, 58.84795663990033177 ) ) ;
#21639 = ORIENTED_EDGE ( 'NONE', *, *, #41118, .T. ) ;
#21640 = CARTESIAN_POINT ( 'NONE',  ( 116.6436511186860798, 33.08230081168869674, 67.87302575006638961 ) ) ;
#21641 = CARTESIAN_POINT ( 'NONE',  ( 266.9165763529819628, 242.0000000000000000, 128.9999999999999716 ) ) ;
#21642 = CARTESIAN_POINT ( 'NONE',  ( 134.3135005523731706, 42.87884033955813834, 56.36529494589373712 ) ) ;
#21643 = DIRECTION ( 'NONE',  ( 0.000000000000000000, -1.000000000000000000, 0.000000000000000000 ) ) ;
#21644 = VECTOR ( 'NONE', #27096, 1000.000000000000000 ) ;
#21646 = ADVANCED_FACE ( 'NONE', ( #62452 ), #51209, .F. ) ;
#21645 = CARTESIAN_POINT ( 'NONE',  ( 161.0127366078917532, 60.45848280706938738, -90.69197953650788691 ) ) ;
#21647 = CARTESIAN_POINT ( 'NONE',  ( 91.11342358617756076, 21.00000175105273570, -49.33836006142978903 ) ) ;
#21648 = AXIS2_PLACEMENT_3D ( 'NONE', #60000, #61059, #49443 ) ;
#21649 = DIRECTION ( 'NONE',  ( 1.000000000000000000, -0.000000000000000000, -0.000000000000000000 ) ) ;
#21650 = EDGE_CURVE ( 'NONE', #31540, #33414, #63244, .T. ) ;
#21651 = EDGE_LOOP ( 'NONE', ( #54885, #45467, #21777, #2625 ) ) ;
#21652 = VECTOR ( 'NONE', #27673, 1000.000000000000000 ) ;
#21653 = ORIENTED_EDGE ( 'NONE', *, *, #59283, .F. ) ;
#21654 = DIRECTION ( 'NONE',  ( -1.000000000000000000, 0.000000000000000000, 0.000000000000000000 ) ) ;
#21655 = ADVANCED_FACE ( 'NONE', ( #62096 ), #30438, .F. ) ;
#21656 = AXIS2_PLACEMENT_3D ( 'NONE', #67329, #3631, #13842 ) ;
#21657 = CARTESIAN_POINT ( 'NONE',  ( 8.000000000000007105, 249.8719672152120381, -95.00000000000133582 ) ) ;
#21658 = CARTESIAN_POINT ( 'NONE',  ( 39.88971011078924533, 8.472992116645412963, -50.61981746542778637 ) ) ;
#21659 = CARTESIAN_POINT ( 'NONE',  ( -165.9121868482145885, 80.88751546905562861, -71.14685045223694715 ) ) ;
#21661 = ORIENTED_EDGE ( 'NONE', *, *, #728, .F. ) ;
#21660 = CARTESIAN_POINT ( 'NONE',  ( -144.2029146819478171, 59.80706661873674079, -36.98889646392695596 ) ) ;
#21662 = CARTESIAN_POINT ( 'NONE',  ( 55.52751777340359496, 12.08567914268658683, 10.95808945309540405 ) ) ;
#21663 = EDGE_CURVE ( 'NONE', #9677, #22538, #57861, .T. ) ;
#21664 = VECTOR ( 'NONE', #57595, 1000.000000000000000 ) ;
#21665 = ORIENTED_EDGE ( 'NONE', *, *, #61914, .T. ) ;
#21666 = CARTESIAN_POINT ( 'NONE',  ( -131.2803255164624829, 50.14412978403780841, 43.34457761225254302 ) ) ;
#21667 = FACE_OUTER_BOUND ( 'NONE', #2172, .T. ) ;
#21668 = CARTESIAN_POINT ( 'NONE',  ( 81.76092782665034520, 17.81692437267513895, -10.76658827783151118 ) ) ;
#21669 = CARTESIAN_POINT ( 'NONE',  ( 87.10668362745094839, 19.58396519288861981, -77.66611478937539914 ) ) ;
#21670 = DIRECTION ( 'NONE',  ( -1.000000000000000000, 0.000000000000000000, 0.000000000000000000 ) ) ;
#21671 = CARTESIAN_POINT ( 'NONE',  ( -96.45845418068302024, 29.92035703021963755, 6.419777494690062980 ) ) ;
#21672 = CARTESIAN_POINT ( 'NONE',  ( -155.3953402213948038, 69.33856625680883212, -91.33370433575318259 ) ) ;
#21673 = EDGE_LOOP ( 'NONE', ( #12965, #26989, #61676 ) ) ;
#21674 = ADVANCED_FACE ( 'NONE', ( #3363 ), #36065, .F. ) ;
#21675 = ORIENTED_EDGE ( 'NONE', *, *, #62911, .F. ) ;
#21676 = CARTESIAN_POINT ( 'NONE',  ( 187.2465631085773339, 85.06582225041682932, -66.26497931038906586 ) ) ;
#21677 = CARTESIAN_POINT ( 'NONE',  ( 15.78827728214693416, 7.507518794609576496, -35.51894409868578606 ) ) ;
#21678 = DIRECTION ( 'NONE',  ( 7.727811381450903769E-14, 0.000000000000000000, 1.000000000000000000 ) ) ;
#21679 = LINE ( 'NONE', #26621, #3683 ) ;
#21680 = CARTESIAN_POINT ( 'NONE',  ( 107.0447263249841399, 28.53200276018955606, -63.47887945344969296 ) ) ;
#21681 = CARTESIAN_POINT ( 'NONE',  ( 83.37786665291103816, 18.33670623396829313, 43.98793584344309693 ) ) ;
#21682 = CARTESIAN_POINT ( 'NONE',  ( 4.606779575613957789, 24.69646479044443765, 0.000000000000000000 ) ) ;
#21683 = CARTESIAN_POINT ( 'NONE',  ( 45.35146934743632841, 10.27620685439441850, -38.52673262789923569 ) ) ;
#21684 = CARTESIAN_POINT ( 'NONE',  ( 212.0850679406002826, 117.0583048437721629, 64.89170834392957943 ) ) ;
#21685 = EDGE_LOOP ( 'NONE', ( #42353, #32502, #15540, #29956 ) ) ;
#21686 = CARTESIAN_POINT ( 'NONE',  ( -109.7793173546317291, 36.75648380851388453, -15.38638933786221763 ) ) ;
#21687 = ORIENTED_EDGE ( 'NONE', *, *, #67594, .T. ) ;
#21688 = CARTESIAN_POINT ( 'NONE',  ( -15.13254930056756820, 7.477527548005404867, -41.21022013649527338 ) ) ;
#21689 = PRESENTATION_LAYER_ASSIGNMENT (  '', '', ( #39786 ) ) ;
#21690 = CARTESIAN_POINT ( 'NONE',  ( -85.86555129592289859, 25.19562892552701783, 93.80983709230186207 ) ) ;
#21691 = CARTESIAN_POINT ( 'NONE',  ( 87.59078297315399197, 20.81577753000345865, 56.60314402004118506 ) ) ;
#21692 = CARTESIAN_POINT ( 'NONE',  ( 154.0401952541423611, 55.03227529428313147, -10.10604738963787419 ) ) ;
#21693 = FACE_OUTER_BOUND ( 'NONE', #66089, .T. ) ;
#21694 = CARTESIAN_POINT ( 'NONE',  ( -95.04371414958065145, 30.36527049547257562, -71.39807560214309490 ) ) ;
#21695 = VECTOR ( 'NONE', #60708, 1000.000000000000000 ) ;
#21696 = LINE ( 'NONE', #58981, #25908 ) ;
#21697 = VERTEX_POINT ( 'NONE', #25175 ) ;
#21698 = AXIS2_PLACEMENT_3D ( 'NONE', #3021, #41346, #8993 ) ;
#21699 = CARTESIAN_POINT ( 'NONE',  ( 211.5481110227417503, 116.2365999939639920, 93.47554241977024958 ) ) ;
#21700 = CARTESIAN_POINT ( 'NONE',  ( 110.0000000000000284, -22.00000000000000000, 0.000000000000000000 ) ) ;
#21701 = ORIENTED_EDGE ( 'NONE', *, *, #14050, .T. ) ;
#21702 = FACE_OUTER_BOUND ( 'NONE', #36586, .T. ) ;
#21703 = CARTESIAN_POINT ( 'NONE',  ( 18.89356949897823768, 62.19351277735707839, 133.5802547743875550 ) ) ;
#21704 = CIRCLE ( 'NONE', #30713, 245.3095347406802489 ) ;
#21705 = CARTESIAN_POINT ( 'NONE',  ( 39.40195752203891999, 9.424259417798142024, -62.46436805589144114 ) ) ;
#21706 = CARTESIAN_POINT ( 'NONE',  ( -6.126800896373027605, 6.786243985899686137, 30.30631899384127692 ) ) ;
#21707 = DIRECTION ( 'NONE',  ( 1.000000000000000000, 0.000000000000000000, -0.000000000000000000 ) ) ;
#21708 = AXIS2_PLACEMENT_3D ( 'NONE', #55111, #18188, #38595 ) ;
#21709 = CARTESIAN_POINT ( 'NONE',  ( -102.2801239173131052, 33.91021738430207222, -50.01457726497594081 ) ) ;
#21710 = VECTOR ( 'NONE', #12467, 1000.000000000000000 ) ;
#21711 = ORIENTED_EDGE ( 'NONE', *, *, #56949, .T. ) ;
#21713 = CIRCLE ( 'NONE', #365, 75.31295361348102801 ) ;
#21712 = DIRECTION ( 'NONE',  ( 9.368415800747543581E-15, -4.202629908585441676E-15, 0.9999999999999997780 ) ) ;
#21714 = CARTESIAN_POINT ( 'NONE',  ( -189.7334103489410495, 107.7745063523401114, -17.96279510330434448 ) ) ;
#21715 = DIRECTION ( 'NONE',  ( -1.000000000000000000, -1.001918046209079887E-14, 9.729495617646301779E-15 ) ) ;
#21716 = CARTESIAN_POINT ( 'NONE',  ( -166.3205068063721512, 81.30869308872871670, -45.38659965827987008 ) ) ;
#21717 = CARTESIAN_POINT ( 'NONE',  ( -180.6286109613758981, 95.89331854612689199, 92.18987725550799439 ) ) ;
#21718 = ORIENTED_EDGE ( 'NONE', *, *, #55175, .T. ) ;
#21719 = DIRECTION ( 'NONE',  ( 0.7071067811865475727, 2.220446049250312341E-16, -0.7071067811865474617 ) ) ;
#21720 = LINE ( 'NONE', #64644, #21750 ) ;
#21721 = CARTESIAN_POINT ( 'NONE',  ( 201.5876148766342908, 103.8397408698164952, -10.14323620147940908 ) ) ;
#21722 = CARTESIAN_POINT ( 'NONE',  ( -146.1757827157406666, 61.40416249728257725, 85.18476316236196055 ) ) ;
#21723 = CARTESIAN_POINT ( 'NONE',  ( 139.1353280997809634, 44.70436000187871173, 42.34369417666323443 ) ) ;
#21724 = ORIENTED_EDGE ( 'NONE', *, *, #69466, .F. ) ;
#21725 = CARTESIAN_POINT ( 'NONE',  ( 2.087089182034596824E-15, -6.732211846623400220, 4.339467034331201845 ) ) ;
#21726 = PLANE ( 'NONE',  #47401 ) ;
#21727 = CARTESIAN_POINT ( 'NONE',  ( 164.6598737201887559, 64.78038692612517480, 7.858682584642552094 ) ) ;
#21728 = DIRECTION ( 'NONE',  ( -1.000000000000000000, -1.509903313490212895E-14, 2.135044278125301096E-16 ) ) ;
#21729 = EDGE_LOOP ( 'NONE', ( #30399, #15741, #9242, #9197, #68879, #61829, #55271, #28270, #38481 ) ) ;
#21730 = CARTESIAN_POINT ( 'NONE',  ( 176.6156959113758660, 75.60152827082542615, 69.69554617303106170 ) ) ;
#21731 = EDGE_CURVE ( 'NONE', #33757, #61707, #68877, .T. ) ;
#21732 = ORIENTED_EDGE ( 'NONE', *, *, #1181, .T. ) ;
#21733 = CARTESIAN_POINT ( 'NONE',  ( -71.67841390531691559, 19.78168466957075822, -18.50581070427913843 ) ) ;
#21734 = CIRCLE ( 'NONE', #2627, 65.00000000000000000 ) ;
#21735 = CARTESIAN_POINT ( 'NONE',  ( 9.319975126229035567, 6.379801983805998944, 94.99999999999866418 ) ) ;
#21736 =( GEOMETRIC_REPRESENTATION_CONTEXT ( 3 ) GLOBAL_UNCERTAINTY_ASSIGNED_CONTEXT ( ( #24061 ) ) GLOBAL_UNIT_ASSIGNED_CONTEXT ( ( #31232, #27310, #55087 ) ) REPRESENTATION_CONTEXT ( 'NONE', 'WORKASPACE' ) );
#21738 = ORIENTED_EDGE ( 'NONE', *, *, #46200, .T. ) ;
#21737 = CARTESIAN_POINT ( 'NONE',  ( -61.34830047412111043, 62.92641549729705019, 133.5802547743875550 ) ) ;
#21739 = LINE ( 'NONE', #23149, #19591 ) ;
#21740 = EDGE_CURVE ( 'NONE', #31531, #40675, #37871, .T. ) ;
#21741 = CARTESIAN_POINT ( 'NONE',  ( 150.3360255159550150, 53.55172128635252449, -95.00000000000133582 ) ) ;
#21742 = CARTESIAN_POINT ( 'NONE',  ( 4.250000000000000000, 0.000000000000000000, -9.500000000000000000 ) ) ;
#21743 = VECTOR ( 'NONE', #61260, 1000.000000000000000 ) ;
#21744 = ORIENTED_EDGE ( 'NONE', *, *, #17716, .T. ) ;
#21745 = PLANE ( 'NONE',  #12027 ) ;
#21746 = VECTOR ( 'NONE', #61753, 1000.000000000000000 ) ;
#21747 = VECTOR ( 'NONE', #26834, 1000.000000000000000 ) ;
#21748 = DIRECTION ( 'NONE',  ( -0.000000000000000000, -0.000000000000000000, -1.000000000000000000 ) ) ;
#21749 = CARTESIAN_POINT ( 'NONE',  ( -180.2188652555596775, 96.98354576637426305, 35.88108729135068842 ) ) ;
#21750 = VECTOR ( 'NONE', #1662, 1000.000000000000000 ) ;
#21751 = CARTESIAN_POINT ( 'NONE',  ( -38.16002576456688899, 10.79155573432543669, -72.99943442513966829 ) ) ;
#21752 = EDGE_CURVE ( 'NONE', #27576, #564, #31170, .T. ) ;
#21753 = ORIENTED_EDGE ( 'NONE', *, *, #28085, .F. ) ;
#21754 = ORIENTED_EDGE ( 'NONE', *, *, #30028, .T. ) ;
#21755 = VERTEX_POINT ( 'NONE', #38476 ) ;
#21756 = VECTOR ( 'NONE', #38755, 1000.000000000000114 ) ;
#21757 = CARTESIAN_POINT ( 'NONE',  ( -1.333402737265964699, 0.000000000000000000, -9.910703160737465822 ) ) ;
#21758 = CARTESIAN_POINT ( 'NONE',  ( 24.96873044429757726, 1.250000000000021982, 0.000000000000000000 ) ) ;
#21759 =( NAMED_UNIT ( * ) SI_UNIT ( $, .STERADIAN. ) SOLID_ANGLE_UNIT ( ) );
#21760 = DIRECTION ( 'NONE',  ( -0.000000000000000000, 1.000000000000000000, 0.000000000000000000 ) ) ;
#21761 = CARTESIAN_POINT ( 'NONE',  ( -107.0206060416819014, 35.25485366694522327, 85.88817087773396963 ) ) ;
#21762 = DIRECTION ( 'NONE',  ( 2.168404344971009361E-16, 0.000000000000000000, -1.000000000000000000 ) ) ;
#21763 = DIRECTION ( 'NONE',  ( 0.3090169943749447312, 0.9510565162951544194, 0.000000000000000000 ) ) ;
#21764 = CARTESIAN_POINT ( 'NONE',  ( 8.000000000000007105, 249.8719672152120381, -95.00000000000133582 ) ) ;
#21766 = VERTEX_POINT ( 'NONE', #1908 ) ;
#21765 =( BOUNDED_CURVE ( )  B_SPLINE_CURVE ( 3, ( #69134, #54334, #20606, #42415 ),
 .UNSPECIFIED., .F., .F. ) 
 B_SPLINE_CURVE_WITH_KNOTS ( ( 4, 4 ),
 ( -2.664535259100375697E-15, 1.570796326794774433 ),
 .UNSPECIFIED. ) 
 CURVE ( )  GEOMETRIC_REPRESENTATION_ITEM ( )  RATIONAL_B_SPLINE_CURVE ( ( 1.000000000000000000, 0.8047378541243930261, 0.8047378541243930261, 1.000000000000000000 ) ) 
 REPRESENTATION_ITEM ( '' )  );
#21767 = DIRECTION ( 'NONE',  ( -0.000000000000000000, -0.000000000000000000, 1.000000000000000000 ) ) ;
#21768 = ORIENTED_EDGE ( 'NONE', *, *, #64022, .F. ) ;
#21769 = CARTESIAN_POINT ( 'NONE',  ( -29.87147652227455552, -74.98256102853682137, 133.5802547743875550 ) ) ;
#21770 = CARTESIAN_POINT ( 'NONE',  ( 187.2354698746856627, 85.05376776489249835, 32.48870243768265453 ) ) ;
#21771 = DIRECTION ( 'NONE',  ( -0.000000000000000000, -0.000000000000000000, -1.000000000000000000 ) ) ;
#21772 = CARTESIAN_POINT ( 'NONE',  ( -7.825402957745085430, -170.0000000000000000, 30.11558103944718923 ) ) ;
#21773 = CARTESIAN_POINT ( 'NONE',  ( -37.61622737004960015, 10.68719896441377237, -92.24730381973596138 ) ) ;
#21774 = CARTESIAN_POINT ( 'NONE',  ( -190.6985136298601731, 109.1272424661242582, 94.99999999999866418 ) ) ;
#21775 = CARTESIAN_POINT ( 'NONE',  ( 197.2089704088280087, 96.60702177658571088, 89.92753103993992170 ) ) ;
#21776 = DIRECTION ( 'NONE',  ( -0.000000000000000000, 1.000000000000000000, -0.000000000000000000 ) ) ;
#21777 = ORIENTED_EDGE ( 'NONE', *, *, #41837, .T. ) ;
#21778 = FACE_OUTER_BOUND ( 'NONE', #36393, .T. ) ;
#21779 = CARTESIAN_POINT ( 'NONE',  ( 25.00000000000000000, 65.13282190615278466, -5.000000000000000000 ) ) ;
#21780 = ORIENTED_EDGE ( 'NONE', *, *, #13762, .T. ) ;
#21781 = ORIENTED_EDGE ( 'NONE', *, *, #42084, .T. ) ;
#21782 = CYLINDRICAL_SURFACE ( 'NONE', #14518, 5.000000000000115463 ) ;
#21783 = PLANE ( 'NONE',  #18600 ) ;
#21784 = CARTESIAN_POINT ( 'NONE',  ( 40.38495044702527537, 9.554194848483444247, 29.96251898938304592 ) ) ;
#21785 =( NAMED_UNIT ( * ) PLANE_ANGLE_UNIT ( ) SI_UNIT ( $, .RADIAN. ) );
#21786 = AXIS2_PLACEMENT_3D ( 'NONE', #55283, #39812, #66910 ) ;
#21787 = CARTESIAN_POINT ( 'NONE',  ( -142.1381007084227122, 58.17237452544245002, 9.955516383538055791 ) ) ;
#21788 = VERTEX_POINT ( 'NONE', #60631 ) ;
#21789 = AXIS2_PLACEMENT_3D ( 'NONE', #25794, #31408, #13838 ) ;
#21790 = VERTEX_POINT ( 'NONE', #6109 ) ;
#21791 = CARTESIAN_POINT ( 'NONE',  ( -132.4776673493542773, 52.21763813822160216, 34.51875723904359461 ) ) ;
#21792 = ORIENTED_EDGE ( 'NONE', *, *, #6424, .T. ) ;
#21793 = CARTESIAN_POINT ( 'NONE',  ( -27.00000000000000355, 29.99999999999999645, 0.000000000000000000 ) ) ;
#21794 = CARTESIAN_POINT ( 'NONE',  ( 0.1317522424410015880, 1.959574484677831130, -8.000000000000001776 ) ) ;
#21795 = LINE ( 'NONE', #10551, #9403 ) ;
#21796 = EDGE_CURVE ( 'NONE', #19003, #30189, #18077, .T. ) ;
#21797 = DIRECTION ( 'NONE',  ( 1.000000000000000000, 0.000000000000000000, 0.000000000000000000 ) ) ;
#21798 = AXIS2_PLACEMENT_3D ( 'NONE', #64701, #48155, #10883 ) ;
#21799 = PRESENTATION_STYLE_ASSIGNMENT (( #53454 ) ) ;
#21800 = VECTOR ( 'NONE', #65079, 1000.000000000000000 ) ;
#21801 = EDGE_CURVE ( 'NONE', #38858, #27926, #54287, .T. ) ;
#21802 = AXIS2_PLACEMENT_3D ( 'NONE', #3160, #35153, #24961 ) ;
#21803 = CARTESIAN_POINT ( 'NONE',  ( -2.999999999999992450, 2.632990618166809235E-15, 21.50000000000000000 ) ) ;
#21804 = ORIENTED_EDGE ( 'NONE', *, *, #45424, .F. ) ;
#21805 = VERTEX_POINT ( 'NONE', #59917 ) ;
#21806 = CARTESIAN_POINT ( 'NONE',  ( -4.000000000000013323, 6.928203230275504332, 0.000000000000000000 ) ) ;
#21807 = DIRECTION ( 'NONE',  ( 0.000000000000000000, 0.000000000000000000, 1.000000000000000000 ) ) ;
#21808 = DIRECTION ( 'NONE',  ( -0.000000000000000000, -0.000000000000000000, -1.000000000000000000 ) ) ;
#21809 = DIRECTION ( 'NONE',  ( 0.000000000000000000, -0.000000000000000000, -1.000000000000000000 ) ) ;
#21810 = CARTESIAN_POINT ( 'NONE',  ( 65.40032188136233060, 13.23841673691966569, 30.19802725762940554 ) ) ;
#21811 = ORIENTED_EDGE ( 'NONE', *, *, #20253, .T. ) ;
#21812 = ADVANCED_FACE ( 'NONE', ( #17730 ), #46461, .T. ) ;
#21813 = CARTESIAN_POINT ( 'NONE',  ( 110.0000000000000284, 21.42428528562853174, 5.000000000000004441 ) ) ;
#21814 = ORIENTED_EDGE ( 'NONE', *, *, #63859, .T. ) ;
#21815 = EDGE_CURVE ( 'NONE', #47318, #8652, #11828, .T. ) ;
#21816 = CARTESIAN_POINT ( 'NONE',  ( -78.66644367742109978, 22.32174330031319442, 30.41820113967310490 ) ) ;
#21817 = ORIENTED_EDGE ( 'NONE', *, *, #42935, .F. ) ;
#21818 = EDGE_LOOP ( 'NONE', ( #24784, #22468, #5976, #57845 ) ) ;
#21819 = CARTESIAN_POINT ( 'NONE',  ( -142.1381007084227122, 58.17237452544243581, -70.57813538785298135 ) ) ;
#21820 = EDGE_CURVE ( 'NONE', #31511, #61512, #33212, .T. ) ;
#21821 = LINE ( 'NONE', #11612, #9078 ) ;
#21822 = CARTESIAN_POINT ( 'NONE',  ( -149.5074843970971301, -170.0000000000000000, 11.37627064943538890 ) ) ;
#21823 = VERTEX_POINT ( 'NONE', #39526 ) ;
#21824 = CARTESIAN_POINT ( 'NONE',  ( 188.9999999999999432, 190.0000000000000000, 72.99999999999998579 ) ) ;
#21825 = FILL_AREA_STYLE ('',( #6353 ) ) ;
#21826 = CARTESIAN_POINT ( 'NONE',  ( 153.2282895792479849, 54.42637815496162546, 30.71980616472758996 ) ) ;
#21827 = AXIS2_PLACEMENT_3D ( 'NONE', #56813, #66688, #49776 ) ;
#21828 = CARTESIAN_POINT ( 'NONE',  ( 23.81581464765709200, 7.603089679099848119, 0.000000000000000000 ) ) ;
#21829 = DIRECTION ( 'NONE',  ( -0.000000000000000000, -0.000000000000000000, -1.000000000000000000 ) ) ;
#21830 = CARTESIAN_POINT ( 'NONE',  ( -84.49322488516129681, 0.000000000000000000, 43.58025477438756212 ) ) ;
#21831 = DIRECTION ( 'NONE',  ( -1.000000000000000000, 0.000000000000000000, 0.000000000000000000 ) ) ;
#21832 = EDGE_CURVE ( 'NONE', #43301, #31528, #51348, .T. ) ;
#21833 = CARTESIAN_POINT ( 'NONE',  ( -24.70911172866235361, 8.583078995053023519, 34.36983212919319897 ) ) ;
#21834 = DIRECTION ( 'NONE',  ( 0.9115451497320358198, -0.4112000000000002875, 0.000000000000000000 ) ) ;
#21835 = EDGE_LOOP ( 'NONE', ( #2570, #25230, #58477, #9664 ) ) ;
#21836 = EDGE_CURVE ( 'NONE', #6688, #42114, #45842, .T. ) ;
#21837 = ADVANCED_FACE ( 'NONE', ( #24401 ), #47815, .F. ) ;
#21838 = FACE_BOUND ( 'NONE', #46301, .T. ) ;
#21839 = ADVANCED_FACE ( 'NONE', ( #39870 ), #47462, .F. ) ;
#21840 = CARTESIAN_POINT ( 'NONE',  ( -0.5158933718595631879, 6.525180340836110204, -68.06532982274359256 ) ) ;
#21841 = CIRCLE ( 'NONE', #62283, 5.000000000000000888 ) ;
#21842 = CARTESIAN_POINT ( 'NONE',  ( -177.1514380519393512, 93.28180884530867445, 71.50650821116707334 ) ) ;
#21843 = LINE ( 'NONE', #33106, #58516 ) ;
#21844 = DIRECTION ( 'NONE',  ( 1.000000000000000000, 0.000000000000000000, 0.000000000000000000 ) ) ;
#21845 = CARTESIAN_POINT ( 'NONE',  ( -85.36298448216592760, 26.07611629625833416, 14.48877058237737181 ) ) ;
#21846 = CYLINDRICAL_SURFACE ( 'NONE', #31458, 89.99999999999998579 ) ;
#21847 = AXIS2_PLACEMENT_3D ( 'NONE', #22051, #949, #28020 ) ;
#21848 = CARTESIAN_POINT ( 'NONE',  ( -152.9119739516381458, 67.12135129037712034, 4.678041278420704607 ) ) ;
#21849 = CARTESIAN_POINT ( 'NONE',  ( -72.69566972648141245, 20.13629716597854369, -91.74463633560024789 ) ) ;
#21850 = VECTOR ( 'NONE', #65405, 1000.000000000000000 ) ;
#21851 = CARTESIAN_POINT ( 'NONE',  ( 69.49862690228273721, 14.27023134440513630, 6.665126176731966723 ) ) ;
#21852 = CARTESIAN_POINT ( 'NONE',  ( -79.14638003838379632, 23.58242782405879012, 72.26275173013684139 ) ) ;
#21853 = CARTESIAN_POINT ( 'NONE',  ( 44.63883881567345213, 10.16630920665935278, -91.43600144160676280 ) ) ;
#21854 = ORIENTED_EDGE ( 'NONE', *, *, #13502, .F. ) ;
#21856 = CIRCLE ( 'NONE', #28601, 24.99999999999985434 ) ;
#21855 = CARTESIAN_POINT ( 'NONE',  ( -34.52542994698666945, 11.14027065218092183, 17.71174954528721202 ) ) ;
#21857 = EDGE_LOOP ( 'NONE', ( #11340, #20887, #43946, #16847 ) ) ;
#21858 = CARTESIAN_POINT ( 'NONE',  ( 109.3079614081140676, 28.45126415661779973, -62.81087680795587147 ) ) ;
#21859 = ORIENTED_EDGE ( 'NONE', *, *, #34694, .F. ) ;
#21860 = CARTESIAN_POINT ( 'NONE',  ( 86.14890207173840508, 20.31981596387580069, -62.66611478937539204 ) ) ;
#21861 = CARTESIAN_POINT ( 'NONE',  ( 103.3565118956568938, 26.91828102196332750, 93.79128338615151961 ) ) ;
#21862 = CARTESIAN_POINT ( 'NONE',  ( -142.3260422482980516, 59.60034523324940636, 67.30005160776828177 ) ) ;
#21863 = CARTESIAN_POINT ( 'NONE',  ( 66.94779593213118574, 13.61918177102165828, -9.984881045247117726 ) ) ;
#21864 = CARTESIAN_POINT ( 'NONE',  ( -24.71645982722742119, 9.599558729461495687, -39.48295160479800359 ) ) ;
#21865 = CARTESIAN_POINT ( 'NONE',  ( -47.61402178322637724, 13.84598486314982146, -70.54967370588845199 ) ) ;
#21866 = DIRECTION ( 'NONE',  ( 1.000000000000000000, 0.000000000000000000, 0.000000000000000000 ) ) ;
#21867 = CARTESIAN_POINT ( 'NONE',  ( -119.5404913382139824, 43.63271406506957106, -19.56318599381059897 ) ) ;
#21868 = EDGE_LOOP ( 'NONE', ( #34452, #7247, #37847, #29975 ) ) ;
#21869 = ORIENTED_EDGE ( 'NONE', *, *, #13358, .F. ) ;
#21870 = CARTESIAN_POINT ( 'NONE',  ( 32.15613847490628530, 8.588587416860169910, 62.30661714676169538 ) ) ;
#21871 = CARTESIAN_POINT ( 'NONE',  ( -167.1619226259398943, 82.18315278115414912, 60.60531548443081817 ) ) ;
#21872 = CARTESIAN_POINT ( 'NONE',  ( 128.9266876467504233, 39.68626248249439215, -91.54607739640439945 ) ) ;
#21873 = PRODUCT_DEFINITION_CONTEXT ( 'detailed design', #29618, 'design' ) ;
#21874 = CARTESIAN_POINT ( 'NONE',  ( 69.47389377197907834, 15.30385359588022709, -93.07428216817731936 ) ) ;
#21875 = VERTEX_POINT ( 'NONE', #31314 ) ;
#21876 = CARTESIAN_POINT ( 'NONE',  ( 98.48662049252141060, -156.6058287036421177, 10.00000000000000000 ) ) ;
#21877 = CARTESIAN_POINT ( 'NONE',  ( 186.6075385349484179, 85.85749512876286360, -21.97869164680669840 ) ) ;
#21878 = CARTESIAN_POINT ( 'NONE',  ( 211.7318474105134669, 118.3631723164074856, 7.243756357567826321 ) ) ;
#21879 = CARTESIAN_POINT ( 'NONE',  ( -58.33959211650994092, -29.48226216511403308, 43.58025477438756212 ) ) ;
#21880 = DIRECTION ( 'NONE',  ( -0.000000000000000000, 1.000000000000000000, -0.000000000000000000 ) ) ;
#21881 = CARTESIAN_POINT ( 'NONE',  ( 0.000000000000000000, 0.000000000000000000, 0.000000000000000000 ) ) ;
#21882 = DIRECTION ( 'NONE',  ( -0.000000000000000000, 1.000000000000000000, -0.000000000000000000 ) ) ;
#21883 = CARTESIAN_POINT ( 'NONE',  ( 164.1338586910085837, 64.33646242148853389, 67.20636812611378730 ) ) ;
#21884 = EDGE_CURVE ( 'NONE', #55546, #52541, #7744, .T. ) ;
#21885 = VECTOR ( 'NONE', #5574, 1000.000000000000000 ) ;
#21886 = ORIENTED_EDGE ( 'NONE', *, *, #15426, .F. ) ;
#21887 = DIRECTION ( 'NONE',  ( -1.000000000000000000, 0.000000000000000000, 0.000000000000000000 ) ) ;
#21888 = CARTESIAN_POINT ( 'NONE',  ( 92.20490818459943227, 22.47175429302964034, -38.28145556619914913 ) ) ;
#21889 = VECTOR ( 'NONE', #22460, 1000.000000000000000 ) ;
#21890 = CARTESIAN_POINT ( 'NONE',  ( -48.34500911884042296, 14.01939034823941910, 68.02609795225436073 ) ) ;
#21891 = CARTESIAN_POINT ( 'NONE',  ( 45.82394788922800899, 46.11928342727495078, 43.58025477438756923 ) ) ;
#21892 = DIRECTION ( 'NONE',  ( 1.000000000000000000, 0.000000000000000000, 0.000000000000000000 ) ) ;
#21893 = DIRECTION ( 'NONE',  ( 0.000000000000000000, 0.000000000000000000, 1.000000000000000000 ) ) ;
#21894 = VECTOR ( 'NONE', #66003, 1000.000000000000000 ) ;
#21895 = AXIS2_PLACEMENT_3D ( 'NONE', #24423, #30378, #25464 ) ;
#21896 = ORIENTED_EDGE ( 'NONE', *, *, #7722, .T. ) ;
#21898 = EDGE_CURVE ( 'NONE', #7404, #47113, #18767, .T. ) ;
#21897 = DIRECTION ( 'NONE',  ( -2.998955517602105048E-18, 4.127708154724731195E-18, -1.000000000000000000 ) ) ;
#21899 = EDGE_CURVE ( 'NONE', #57172, #54901, #36590, .T. ) ;
#21900 = AXIS2_PLACEMENT_3D ( 'NONE', #64135, #57834, #37063 ) ;
#21901 = CARTESIAN_POINT ( 'NONE',  ( 46.66904755831210139, -9.150666335777657423E-14, 2.000000000000001776 ) ) ;
#21902 = EDGE_LOOP ( 'NONE', ( #26574, #45100, #58690, #42968, #31610, #13468, #38650, #35437 ) ) ;
#21903 = EDGE_CURVE ( 'NONE', #12486, #21176, #62173, .T. ) ;
#21904 = ORIENTED_EDGE ( 'NONE', *, *, #16359, .T. ) ;
#21905 = DIRECTION ( 'NONE',  ( -0.3513748240813435175, 0.9362348706397369824, 2.500042656554809354E-16 ) ) ;
#21906 = CARTESIAN_POINT ( 'NONE',  ( 447.3372781065083927, 395.0000000000043769, 91.05029585798388325 ) ) ;
#21907 = CARTESIAN_POINT ( 'NONE',  ( 93.08174259058945665, 22.79847752828721141, -66.31129219526786756 ) ) ;
#21908 = VERTEX_POINT ( 'NONE', #62010 ) ;
#21909 = EDGE_CURVE ( 'NONE', #4017, #30296, #9350, .T. ) ;
#21910 = CARTESIAN_POINT ( 'NONE',  ( -55.53469534616547065, 14.81076603075805664, -77.06087458892359621 ) ) ;
#21911 = CARTESIAN_POINT ( 'NONE',  ( 36.76746179515744473, 8.081433644308896547, -9.248917121289487397 ) ) ;
#21912 = CARTESIAN_POINT ( 'NONE',  ( 177.0027897064244371, 75.97676392242546228, -37.41656822527980353 ) ) ;
#21913 = CARTESIAN_POINT ( 'NONE',  ( 164.9657042191946061, 63.72163127919190373, 90.13840011216286996 ) ) ;
#21914 = FACE_OUTER_BOUND ( 'NONE', #35253, .T. ) ;
#21915 = ORIENTED_EDGE ( 'NONE', *, *, #1922, .T. ) ;
#21916 = CARTESIAN_POINT ( 'NONE',  ( -49.13048465129993048, 14.20828170588045758, -38.08805284523984369 ) ) ;
#21917 = DIRECTION ( 'NONE',  ( -0.5508969814520946473, -0.8345732537213079727, 0.000000000000000000 ) ) ;
#21918 = CARTESIAN_POINT ( 'NONE',  ( 11.82929895397812992, 7.412564870773605818, 31.13995448514249631 ) ) ;
#21919 = CARTESIAN_POINT ( 'NONE',  ( -44.99999999999998579, 25.00000000000000000, 2.000000000000015543 ) ) ;
#21920 = CARTESIAN_POINT ( 'NONE',  ( -31.11269837220804035, 20.55634918610408945, 0.000000000000000000 ) ) ;
#21922 = EDGE_LOOP ( 'NONE', ( #9145, #1230, #54736, #6772 ) ) ;
#21921 = DIRECTION ( 'NONE',  ( 1.000000000000000000, 0.000000000000000000, 0.000000000000000000 ) ) ;
#21923 = ORIENTED_EDGE ( 'NONE', *, *, #1936, .T. ) ;
#21924 = EDGE_CURVE ( 'NONE', #7404, #23453, #48808, .T. ) ;
#21925 = EDGE_CURVE ( 'NONE', #53544, #6513, #11078, .T. ) ;
#21926 = EDGE_LOOP ( 'NONE', ( #63329, #51842, #8160, #65619 ) ) ;
#21927 = CARTESIAN_POINT ( 'NONE',  ( -11.57808265946729875, 7.164483090579918390, -22.57181510547873771 ) ) ;
#21928 = CARTESIAN_POINT ( 'NONE',  ( -54.56693200831792723, 14.55131601960338905, 45.31732777293116499 ) ) ;
#21929 = DIRECTION ( 'NONE',  ( -1.000000000000000000, 3.344045254895050726E-17, -1.337618101958020291E-16 ) ) ;
#21930 = CARTESIAN_POINT ( 'NONE',  ( -84.49322488516129681, 0.000000000000000000, 43.58025477438756212 ) ) ;
#21931 = ADVANCED_FACE ( 'NONE', ( #39702 ), #56570, .F. ) ;
#21932 = CARTESIAN_POINT ( 'NONE',  ( -38.17232309348613484, 11.81874355808867350, 67.90144012224213554 ) ) ;
#21933 = CARTESIAN_POINT ( 'NONE',  ( -11.78188048797445475, 8.190559674012728664, -22.44981765585516698 ) ) ;
#21934 = CARTESIAN_POINT ( 'NONE',  ( 153.2384531768736053, 54.43344429203624202, -64.25936496073454407 ) ) ;
#21935 = PLANE ( 'NONE',  #43210 ) ;
#21936 = ORIENTED_EDGE ( 'NONE', *, *, #29449, .F. ) ;
#21937 = AXIS2_PLACEMENT_3D ( 'NONE', #57326, #67541, #41149 ) ;
#21938 = DIRECTION ( 'NONE',  ( -0.000000000000000000, 0.7071067811865474617, -0.7071067811865474617 ) ) ;
#21939 = ORIENTED_EDGE ( 'NONE', *, *, #24011, .T. ) ;
#21940 = EDGE_LOOP ( 'NONE', ( #16661, #20308, #15713, #38662 ) ) ;
#21941 = DIRECTION ( 'NONE',  ( 0.000000000000000000, 0.000000000000000000, 1.000000000000000000 ) ) ;
#21942 = AXIS2_PLACEMENT_3D ( 'NONE', #32846, #6106, #55340 ) ;
#21943 = CARTESIAN_POINT ( 'NONE',  ( -61.26061298622803974, 17.48391647823794059, -92.17393543469286499 ) ) ;
#21944 = CARTESIAN_POINT ( 'NONE',  ( 117.7395339318602652, 32.50726632670704674, 90.38096001386408318 ) ) ;
#21945 = CARTESIAN_POINT ( 'NONE',  ( -151.2511071212632032, 67.00426547928871912, 18.68401857637098473 ) ) ;
#21946 = VECTOR ( 'NONE', #53346, 1000.000000000000000 ) ;
#21947 = AXIS2_PLACEMENT_3D ( 'NONE', #69120, #20948, #19923 ) ;
#21948 = DIRECTION ( 'NONE',  ( -1.000000000000000000, 0.000000000000000000, 0.000000000000000000 ) ) ;
#21949 = CARTESIAN_POINT ( 'NONE',  ( 47.74291447196797833, 2.000000000000001776, -75.60236247897087480 ) ) ;
#21950 = AXIS2_PLACEMENT_3D ( 'NONE', #9793, #30553, #20682 ) ;
#21951 = CARTESIAN_POINT ( 'NONE',  ( 110.0000000000000284, -22.00000000000000000, -5.000000000000004441 ) ) ;
#21952 = ORIENTED_EDGE ( 'NONE', *, *, #19041, .T. ) ;
#21953 = VERTEX_POINT ( 'NONE', #12273 ) ;
#21954 = VECTOR ( 'NONE', #13624, 1000.000000000000000 ) ;
#21955 = VERTEX_POINT ( 'NONE', #18592 ) ;
#21956 = VECTOR ( 'NONE', #22623, 1000.000000000000000 ) ;
#21957 = CARTESIAN_POINT ( 'NONE',  ( -156.9262190792699698, 72.10659547035872663, -14.32972382511977116 ) ) ;
#21958 = CARTESIAN_POINT ( 'NONE',  ( 32.30062460741315533, 8.603096374765343057, -45.54517555199483070 ) ) ;
#21959 = LINE ( 'NONE', #69103, #29269 ) ;
#21960 = DIRECTION ( 'NONE',  ( 3.306261395983863330E-15, 1.000000000000000000, -5.551115123125782702E-17 ) ) ;
#21961 = VERTEX_POINT ( 'NONE', #29488 ) ;
#21962 = CARTESIAN_POINT ( 'NONE',  ( 86.62931800182293784, 20.48449268398422873, -50.82156419891174437 ) ) ;
#21963 = CARTESIAN_POINT ( 'NONE',  ( -156.0171627975467743, 69.90368824761766575, 68.79920456856257260 ) ) ;
#21964 = CARTESIAN_POINT ( 'NONE',  ( -1.328627985309864590, 7.561890325089884790, -46.67342399825810162 ) ) ;
#21965 = CARTESIAN_POINT ( 'NONE',  ( 105.2506154496929582, 26.63995206619728506, 15.86906671377738576 ) ) ;
#21966 = PLANE ( 'NONE',  #58946 ) ;
#21967 = CARTESIAN_POINT ( 'NONE',  ( -83.52505811737955810, 24.23179517241434411, -48.35018627393339585 ) ) ;
#21968 = CARTESIAN_POINT ( 'NONE',  ( 0.000000000000000000, 0.000000000000000000, 40.00000000000003553 ) ) ;
#21969 = CARTESIAN_POINT ( 'NONE',  ( 427.4999999999999432, 207.5000000000000284, 0.000000000000000000 ) ) ;
#21970 = CARTESIAN_POINT ( 'NONE',  ( 8.951900209438534262, 6.378066731449594684, -72.95773463900229672 ) ) ;
#21971 = EDGE_CURVE ( 'NONE', #47318, #38945, #45677, .T. ) ;
#21972 = ORIENTED_EDGE ( 'NONE', *, *, #16110, .T. ) ;
#21973 = LINE ( 'NONE', #65961, #12522 ) ;
#21974 = APPLICATION_PROTOCOL_DEFINITION ( 'draft international standard', 'automotive_design', 1998, #23376 ) ;
#21975 = CARTESIAN_POINT ( 'NONE',  ( 179.0096185093687779, 76.53352131383243773, 29.58811944080985512 ) ) ;
#21976 = CYLINDRICAL_SURFACE ( 'NONE', #39934, 65.00000000000000000 ) ;
#21977 = CARTESIAN_POINT ( 'NONE',  ( -3.816391647148975608E-14, -9.237604307034022355, -8.785468820183664818 ) ) ;
#21978 = CARTESIAN_POINT ( 'NONE',  ( -59.42430146430388049, -27.22983999535795618, 43.58025477438756212 ) ) ;
#21979 = VERTEX_POINT ( 'NONE', #40389 ) ;
#21980 = PRODUCT_DEFINITION_SHAPE ( 'NONE', 'NONE',  #69634 ) ;
#21981 = B_SPLINE_CURVE_WITH_KNOTS ( 'NONE', 3,
 ( #23247, #6354, #60858, #12681, #34147, #7416, #49247, #43971, #49954, #55945, #22884, #54527, #28868, #1080, #7760, #50319, #54880, #22532, #6702, #39760, #16898, #2137, #23589, #65453, #65099, #17247, #66510, #38716, #65813, #60162, #13043, #33453, #29209, #11982, #28148, #17608, #49595, #1427, #44327, #39074, #33790, #7051, #28510, #41494, #8449 ),
 .UNSPECIFIED., .F., .F.,
 ( 4, 2, 2, 2, 2, 2, 2, 2, 2, 2, 2, 2, 2, 1, 2, 2, 2, 2, 2, 2, 2, 2, 4 ),
 ( 0.02356759485890610670, 0.02503765354686417546, 0.02577268289084322372, 0.02650771223482226852, 0.02797777092278037545, 0.02944782961073848238, 0.03018285895471753758, 0.03091788829869659277, 0.03238794698665466848, 0.03312297633063371327, 0.03385800567461275806, 0.03532806436257082683, 0.03606309370654985080, 0.03679812305052886784, 0.03753315239450789181, 0.03826818173848690885, 0.03973824042644495680, 0.04120829911440300475, 0.04267835780236105270, 0.04341338714634006279, 0.04414841649031907983, 0.04561847517827709309, 0.04708853386623509940 ),
 .UNSPECIFIED. ) ;
#21982 = VERTEX_POINT ( 'NONE', #61157 ) ;
#21984 = EDGE_CURVE ( 'NONE', #18463, #20826, #12979, .T. ) ;
#21983 = CARTESIAN_POINT ( 'NONE',  ( -126.3071720906782076, 46.76607039798766863, -88.60280507916129977 ) ) ;
#21985 = CARTESIAN_POINT ( 'NONE',  ( 184.0196598574194411, 81.62390236021667533, 83.58993435411535700 ) ) ;
#21986 = ORIENTED_EDGE ( 'NONE', *, *, #50807, .T. ) ;
#21987 = AXIS2_PLACEMENT_3D ( 'NONE', #23431, #45912, #34330 ) ;
#21988 = ORIENTED_EDGE ( 'NONE', *, *, #48720, .F. ) ;
#21989 = FACE_OUTER_BOUND ( 'NONE', #14026, .T. ) ;
#21990 = EDGE_CURVE ( 'NONE', #63860, #33355, #23184, .T. ) ;
#21991 = CARTESIAN_POINT ( 'NONE',  ( -74.58602291351357394, -7.967916035252095242, 170.0000000000000000 ) ) ;
#21992 = ORIENTED_EDGE ( 'NONE', *, *, #16803, .F. ) ;
#21993 = PLANE ( 'NONE',  #23363 ) ;
#21994 = CARTESIAN_POINT ( 'NONE',  ( 105.2147050270618820, 27.72205961956172260, -91.53208825577468133 ) ) ;
#21995 = EDGE_CURVE ( 'NONE', #863, #56212, #3737, .T. ) ;
#21996 = VECTOR ( 'NONE', #17183, 1000.000000000000114 ) ;
#21997 = CARTESIAN_POINT ( 'NONE',  ( 141.2361973397653117, 47.26569015399784490, 65.21956349169761324 ) ) ;
#21998 = CARTESIAN_POINT ( 'NONE',  ( -75.43044859198177221, 21.11535168543637297, -35.84517485573555007 ) ) ;
#21999 = EDGE_CURVE ( 'NONE', #50676, #46832, #34127, .T. ) ;
#22000 = CARTESIAN_POINT ( 'NONE',  ( -96.00016893459647349, 29.70347032303887502, 42.12695562128465099 ) ) ;
#22001 = VECTOR ( 'NONE', #59253, 1000.000000000000000 ) ;
#22002 = DIRECTION ( 'NONE',  ( -0.000000000000000000, -0.000000000000000000, 1.000000000000000000 ) ) ;
#22003 = CARTESIAN_POINT ( 'NONE',  ( -189.2352924136013996, 107.0839554967701304, 37.97586783404467070 ) ) ;
#22004 = AXIS2_PLACEMENT_3D ( 'NONE', #965, #5873, #22412 ) ;
#22005 = AXIS2_PLACEMENT_3D ( 'NONE', #32747, #34156, #27111 ) ;
#22006 = ORIENTED_EDGE ( 'NONE', *, *, #29771, .F. ) ;
#22007 = ORIENTED_EDGE ( 'NONE', *, *, #29255, .F. ) ;
#22008 = FACE_OUTER_BOUND ( 'NONE', #49315, .T. ) ;
#22009 = CIRCLE ( 'NONE', #63601, 242.4895526022646379 ) ;
#22010 = FACE_BOUND ( 'NONE', #49744, .T. ) ;
#22011 = CARTESIAN_POINT ( 'NONE',  ( 42.70988075781784943, 8.862408058333471672, -49.86848500202146539 ) ) ;
#22012 = CARTESIAN_POINT ( 'NONE',  ( 15.55634918610397399, -26.11269837220809364, 0.000000000000000000 ) ) ;
#22014 = VERTEX_POINT ( 'NONE', #61506 ) ;
#22013 = CARTESIAN_POINT ( 'NONE',  ( -142.9730935922300148, 58.82921737386682537, -38.62225429887013917 ) ) ;
#22015 = CARTESIAN_POINT ( 'NONE',  ( -173.1211646369891355, -170.0000000000000000, 72.66624519710475738 ) ) ;
#22016 = EDGE_LOOP ( 'NONE', ( #61763, #57213 ) ) ;
#22017 = CARTESIAN_POINT ( 'NONE',  ( -31.43908319763710679, -170.0000000000000000, -42.81719736520184938 ) ) ;
#22018 = CARTESIAN_POINT ( 'NONE',  ( 26.99999999999999645, -27.00000000000000355, 15.00000000000000000 ) ) ;
#22019 = DIRECTION ( 'NONE',  ( -1.000000000000000000, 0.000000000000000000, 0.000000000000000000 ) ) ;
#22020 = ADVANCED_FACE ( 'NONE', ( #34086 ), #11598, .F. ) ;
#22021 = DIRECTION ( 'NONE',  ( 0.000000000000000000, -1.000000000000000000, 0.000000000000000000 ) ) ;
#22022 = CARTESIAN_POINT ( 'NONE',  ( 89.88695630745282017, 20.55793566325393584, -63.39359200686787688 ) ) ;
#22023 = CARTESIAN_POINT ( 'NONE',  ( 10.55634918610396511, -41.66904755831214402, 0.000000000000000000 ) ) ;
#22024 = CARTESIAN_POINT ( 'NONE',  ( -97.49219489034497599, 30.41416107059307805, 5.381099477080671711 ) ) ;
#22025 = DIRECTION ( 'NONE',  ( -1.000000000000000000, 0.000000000000000000, 0.000000000000000000 ) ) ;
#22026 = EDGE_LOOP ( 'NONE', ( #8794, #36712 ) ) ;
#22027 = ORIENTED_EDGE ( 'NONE', *, *, #44042, .T. ) ;
#22028 = CARTESIAN_POINT ( 'NONE',  ( 45.02738683369922512, 9.207938468499239804, 32.44741314349040806 ) ) ;
#22029 = CARTESIAN_POINT ( 'NONE',  ( 12.46704290855393360, 6.417105965824392300, 30.78567100710504789 ) ) ;
#22030 = CARTESIAN_POINT ( 'NONE',  ( 63.01563776193091826, -170.0000000000000000, -70.06524142263343435 ) ) ;
#22031 = CARTESIAN_POINT ( 'NONE',  ( 49.99999999999998579, 19.99999999999996447, 1.999999999999984457 ) ) ;
#22032 = CARTESIAN_POINT ( 'NONE',  ( 210.9608386442062624, 117.1762372255316365, -39.69180030939477888 ) ) ;
#22033 = CARTESIAN_POINT ( 'NONE',  ( -84.49322488516129681, 0.000000000000000000, 43.58025477438756212 ) ) ;
#22034 = CARTESIAN_POINT ( 'NONE',  ( -190.6985136298602015, 109.1272424661243434, 16.02916387300914280 ) ) ;
#22035 = CARTESIAN_POINT ( 'NONE',  ( 44.34689728705970424, 10.12166135033765357, -37.45970703709721050 ) ) ;
#22036 = DIRECTION ( 'NONE',  ( -1.387778780781445676E-15, -2.095411779493312608E-31, -1.000000000000000000 ) ) ;
#22037 = ORIENTED_EDGE ( 'NONE', *, *, #38249, .F. ) ;
#22038 = CARTESIAN_POINT ( 'NONE',  ( -27.70115495247213033, 10.02455692117573882, 17.39240037915121206 ) ) ;
#22039 = ORIENTED_EDGE ( 'NONE', *, *, #41921, .F. ) ;
#22040 = VECTOR ( 'NONE', #51795, 1000.000000000000000 ) ;
#22041 = CARTESIAN_POINT ( 'NONE',  ( -11.57808265946730586, 7.164483090579920166, -49.41636569594241024 ) ) ;
#22042 = LINE ( 'NONE', #32600, #24025 ) ;
#22043 = CARTESIAN_POINT ( 'NONE',  ( 36.64089410029661309, -65.45232906116366678, 170.0000000000000000 ) ) ;
#22044 = CARTESIAN_POINT ( 'NONE',  ( -35.00000000000002842, -35.00000000000000000, 380.0000000000000000 ) ) ;
#22045 = CARTESIAN_POINT ( 'NONE',  ( 31.91383250562745388, 8.564461488296998937, 11.05764693793517139 ) ) ;
#22046 = VECTOR ( 'NONE', #12902, 1000.000000000000000 ) ;
#22047 = CARTESIAN_POINT ( 'NONE',  ( -96.77705718164442317, 31.18700926299569787, -64.23949498694426552 ) ) ;
#22048 = CARTESIAN_POINT ( 'NONE',  ( 116.7923802250937371, 33.15684512294094333, -93.43283724407298507 ) ) ;
#22049 = AXIS2_PLACEMENT_3D ( 'NONE', #36182, #58313, #47406 ) ;
#22050 = DIRECTION ( 'NONE',  ( -0.000000000000000000, 0.000000000000000000, -1.000000000000000000 ) ) ;
#22051 = CARTESIAN_POINT ( 'NONE',  ( 46.66904755831210139, 4.999999999999909406, 85.00100000000000477 ) ) ;
#22052 = ORIENTED_EDGE ( 'NONE', *, *, #13376, .F. ) ;
#22053 = DIRECTION ( 'NONE',  ( 0.7660444431189771253, 0.6427876096865404731, -1.328875279120069661E-16 ) ) ;
#22054 = DIRECTION ( 'NONE',  ( 1.000000000000000000, 0.000000000000000000, 0.000000000000000000 ) ) ;
#22055 = LINE ( 'NONE', #2012, #38515 ) ;
#22056 = CARTESIAN_POINT ( 'NONE',  ( -8.800520192024523070, 7.964629484975262130, 3.318412053709786758 ) ) ;
#22057 = EDGE_CURVE ( 'NONE', #24735, #18937, #28447, .T. ) ;
#22058 = CARTESIAN_POINT ( 'NONE',  ( 41.33434189587761409, 9.684413566891873160, -62.71343792220747559 ) ) ;
#22060 = ADVANCED_FACE ( 'NONE', ( #55522 ), #50256, .F. ) ;
#22059 = CARTESIAN_POINT ( 'NONE',  ( -5.401648928593166588, 6.744888135494082171, 44.72991648308484258 ) ) ;
#22061 = CARTESIAN_POINT ( 'NONE',  ( -31.11269837220806878, 5.000000000000056843, 2.000000000000001776 ) ) ;
#22062 = CARTESIAN_POINT ( 'NONE',  ( 93.28147497731882254, 22.87326625539070335, 94.43110130039434580 ) ) ;
#22063 = AXIS2_PLACEMENT_3D ( 'NONE', #48394, #57611, #53340 ) ;
#22064 = EDGE_CURVE ( 'NONE', #48865, #47682, #49816, .T. ) ;
#22065 = ORIENTED_EDGE ( 'NONE', *, *, #55850, .T. ) ;
#22066 = DIRECTION ( 'NONE',  ( 0.000000000000000000, 0.000000000000000000, 1.000000000000000000 ) ) ;
#22067 = CARTESIAN_POINT ( 'NONE',  ( 7.999999999999998224, -1.555946510856144993, -9.432911297836643172 ) ) ;
#22068 = DIRECTION ( 'NONE',  ( 1.110223024625158749E-14, 0.000000000000000000, 1.000000000000000000 ) ) ;
#22069 = CARTESIAN_POINT ( 'NONE',  ( -168.1839487819771364, 83.25723186408067988, -36.56132926469148003 ) ) ;
#22070 = ITEM_DEFINED_TRANSFORMATION ( 'NONE', 'NONE', #27623,  #66832 ) ;
#22071 = CARTESIAN_POINT ( 'NONE',  ( -173.1211646369891355, 87.12891641440857882, -61.55650775521367279 ) ) ;
#22072 = ORIENTED_EDGE ( 'NONE', *, *, #14830, .T. ) ;
#22073 = CARTESIAN_POINT ( 'NONE',  ( 112.3013380801407095, 388.0000000000077307, 91.05029585798746439 ) ) ;
#22074 = B_SPLINE_CURVE_WITH_KNOTS ( 'NONE', 3,
 ( #31380, #30688, #8548, #26098, #41582, #24729, #8891, #52138, #62352, #40891, #14165, #47197, #35964, #30344, #9580, #58108, #35627, #30000, #25423, #46863, #46506, #9925, #61993, #19786, #14844, #63391, #36311, #40542, #41249, #57766, #13809, #31039, #52813, #35273, #52483, #4306, #25768, #68654, #20464, #41927, #15198, #37329, #54545, #43291, #26448, #49264 ),
 .UNSPECIFIED., .F., .F.,
 ( 4, 2, 2, 2, 2, 2, 2, 2, 2, 2, 2, 2, 2, 2, 2, 2, 2, 2, 2, 2, 2, 2, 4 ),
 ( 3.122502256758252770E-17, 0.001572224531395700550, 0.003144449062791369875, 0.004716673594187039201, 0.006288898125582708526, 0.007861122656978377851, 0.009433347188374047176, 0.01021945945407186709, 0.01100557171976968875, 0.01179168398546750866, 0.01257779625116533032, 0.01415002078256097189, 0.01493613304825880048, 0.01572224531395662733, 0.01650835757965446113, 0.01729446984535228798, 0.01886669437674788966, 0.01965280664244568876, 0.02043891890814348439, 0.02201114343953908259, 0.02358336797093467732, 0.02436948023663247295, 0.02515559250233026511 ),
 .UNSPECIFIED. ) ;
#22075 = CARTESIAN_POINT ( 'NONE',  ( -4.725257700476006129, 6.708862164351558910, -9.239876348931433725 ) ) ;
#22076 = CARTESIAN_POINT ( 'NONE',  ( 197.2199569260504006, 98.22436319491366419, -16.31760007026884551 ) ) ;
#22077 = CARTESIAN_POINT ( 'NONE',  ( -145.4293260530172631, 60.79600197597825684, 85.60900646559132099 ) ) ;
#22078 = EDGE_CURVE ( 'NONE', #21823, #23678, #54264, .T. ) ;
#22079 = DIRECTION ( 'NONE',  ( -0.000000000000000000, -0.000000000000000000, -1.000000000000000000 ) ) ;
#22080 = ORIENTED_EDGE ( 'NONE', *, *, #44321, .F. ) ;
#22081 = CARTESIAN_POINT ( 'NONE',  ( -190.6985136298601731, 109.1272424661242582, 94.99999999999866418 ) ) ;
#22082 = CARTESIAN_POINT ( 'NONE',  ( 84.26390409839197559, 19.68678207880320841, 17.50091665772310989 ) ) ;
#22083 = EDGE_CURVE ( 'NONE', #58443, #64743, #9772, .T. ) ;
#22084 = CARTESIAN_POINT ( 'NONE',  ( -97.88021438939451002, 31.71889184683103480, 44.11149307090948213 ) ) ;
#22085 = CARTESIAN_POINT ( 'NONE',  ( -0.4996266546846072631, -170.0000000000000000, -95.00000000000133582 ) ) ;
#22086 = ORIENTED_EDGE ( 'NONE', *, *, #38328, .T. ) ;
#22087 = DIRECTION ( 'NONE',  ( 2.086468734322990096E-16, 1.377265952997550087E-16, 1.000000000000000000 ) ) ;
#22088 = VERTEX_POINT ( 'NONE', #47049 ) ;
#22089 = VERTEX_POINT ( 'NONE', #67480 ) ;
#22090 = VECTOR ( 'NONE', #31305, 1000.000000000000000 ) ;
#22091 = CARTESIAN_POINT ( 'NONE',  ( -121.9166680696882850, 43.93013778640997202, -89.72953050740939318 ) ) ;
#22092 = CARTESIAN_POINT ( 'NONE',  ( 15.55634918610397399, -31.11269837220809364, 0.000000000000000000 ) ) ;
#22093 = AXIS2_PLACEMENT_3D ( 'NONE', #35129, #45691, #61173 ) ;
#22095 = VERTEX_POINT ( 'NONE', #4151 ) ;
#22094 = CARTESIAN_POINT ( 'NONE',  ( 150.0980941434704619, 53.37942190380064034, 8.659987245234894715 ) ) ;
#22096 = CARTESIAN_POINT ( 'NONE',  ( 164.8942204024298235, 63.66138186734713855, 38.01188527962676034 ) ) ;
#22097 = DIRECTION ( 'NONE',  ( -0.8160245890732938934, -0.5780171883497599028, 0.000000000000000000 ) ) ;
#22098 = DIRECTION ( 'NONE',  ( 0.4887922226926451064, 0.000000000000000000, -0.8724002309921654597 ) ) ;
#22099 = AXIS2_PLACEMENT_3D ( 'NONE', #13100, #65165, #38427 ) ;
#22100 = VERTEX_POINT ( 'NONE', #57951 ) ;
#22101 = AXIS2_PLACEMENT_3D ( 'NONE', #52827, #41596, #3971 ) ;
#22102 = CARTESIAN_POINT ( 'NONE',  ( -23.85457283326427813, -7.880174245944393974, 3.061616997868437868E-16 ) ) ;
#22103 = CARTESIAN_POINT ( 'NONE',  ( 50.97490815085634352, 0.000000000000000000, -4.435653166495503896 ) ) ;
#22104 = CARTESIAN_POINT ( 'NONE',  ( 153.6158476725599371, 54.71469178023152580, -90.86794399618655405 ) ) ;
#22105 = CARTESIAN_POINT ( 'NONE',  ( 129.5225439633634608, 40.02995148249141266, 57.71575578625421343 ) ) ;
#22106 = ORIENTED_EDGE ( 'NONE', *, *, #43705, .T. ) ;
#22107 = ORIENTED_EDGE ( 'NONE', *, *, #65920, .F. ) ;
#22108 = VERTEX_POINT ( 'NONE', #52664 ) ;
#22109 = CARTESIAN_POINT ( 'NONE',  ( 188.9999999999999432, 192.0000000000000000, 0.000000000000000000 ) ) ;
#22110 = CARTESIAN_POINT ( 'NONE',  ( -47.81209834363054512, 12.85890427894798727, 93.48825161138802287 ) ) ;
#22111 = DIRECTION ( 'NONE',  ( 0.000000000000000000, -0.000000000000000000, -1.000000000000000000 ) ) ;
#22112 = LINE ( 'NONE', #1709, #19843 ) ;
#22113 = CARTESIAN_POINT ( 'NONE',  ( 70.10607374715122830, 14.42976827319814426, 88.53455713664466487 ) ) ;
#22114 = CYLINDRICAL_SURFACE ( 'NONE', #51668, 91.99999999999997158 ) ;
#22115 = CARTESIAN_POINT ( 'NONE',  ( 0.000000000000000000, 0.000000000000000000, 0.000000000000000000 ) ) ;
#22116 = CARTESIAN_POINT ( 'NONE',  ( -13.24252603915608617, 63.63674649211943546, 40.00000000000003553 ) ) ;
#22117 = CARTESIAN_POINT ( 'NONE',  ( -61.29635759142584561, -21.66977272663583776, 170.0000000000000000 ) ) ;
#22118 = ORIENTED_EDGE ( 'NONE', *, *, #59385, .T. ) ;
#22119 = CARTESIAN_POINT ( 'NONE',  ( -101.4485769343308021, 33.48710798375949338, -88.73808582770939779 ) ) ;
#22120 = EDGE_LOOP ( 'NONE', ( #11083, #24345, #50636, #33255 ) ) ;
#22121 = FACE_OUTER_BOUND ( 'NONE', #51642, .T. ) ;
#22122 = CARTESIAN_POINT ( 'NONE',  ( 212.0047492081761504, 116.9348962082588770, -72.39146962302672250 ) ) ;
#22123 = B_SPLINE_CURVE_WITH_KNOTS ( 'NONE', 3,
 ( #61119, #23842, #34748, #67793, #3082, #56184, #62152, #8000, #45639, #67116, #18909, #40355, #35081, #56531, #67448, #8358, #51271, #24545, #45981, #19239, #13969, #35431, #51609, #56894, #8709, #30162, #14660, #41740, #10756, #32223, #25231, #5136, #52965, #63201, #42426, #47016, #19950, #36121, #42759, #62859, #42080, #46668, #57582, #68475, #9388, #25916 ),
 .UNSPECIFIED., .F., .F.,
 ( 4, 2, 2, 2, 2, 2, 2, 2, 2, 2, 2, 2, 2, 2, 2, 2, 2, 2, 2, 2, 2, 2, 4 ),
 ( 0.000000000000000000, 0.003635178948345819169, 0.005452768422518699913, 0.007270357896691580224, 0.008179152633778006068, 0.009087947370864431912, 0.01090553684503732870, 0.01181433158212378404, 0.01272312631921023764, 0.01363192105629669297, 0.01454071579338314830, 0.01544951053046960364, 0.01635830526755605724, 0.01726710000464251257, 0.01817589474172896791, 0.01908468947881542324, 0.01999348421590187511, 0.02090227895298833391, 0.02181107369007478577, 0.02362866316424774155, 0.02544625263842069732, 0.02726384211259364962, 0.02908143158676660539 ),
 .UNSPECIFIED. ) ;
#22124 = CARTESIAN_POINT ( 'NONE',  ( 0.000000000000000000, 0.000000000000000000, -5.000000000000000000 ) ) ;
#22125 = DIRECTION ( 'NONE',  ( 0.4738686624730094610, -0.8805955318567321166, 0.000000000000000000 ) ) ;
#22126 = CARTESIAN_POINT ( 'NONE',  ( -35.29220329090401975, 10.25561257217314726, -90.06824336686142374 ) ) ;
#22127 = CARTESIAN_POINT ( 'NONE',  ( 18.88468164817598449, 7.626722602998420975, 30.67930430767540173 ) ) ;
#22128 = FACE_OUTER_BOUND ( 'NONE', #16664, .T. ) ;
#22129 = LINE ( 'NONE', #43917, #62954 ) ;
#22130 = DIRECTION ( 'NONE',  ( 0.000000000000000000, 0.000000000000000000, 1.000000000000000000 ) ) ;
#22131 = VERTEX_POINT ( 'NONE', #68836 ) ;
#22132 = VECTOR ( 'NONE', #21042, 1000.000000000000000 ) ;
#22133 = DIRECTION ( 'NONE',  ( 0.000000000000000000, 0.000000000000000000, 1.000000000000000000 ) ) ;
#22134 = CARTESIAN_POINT ( 'NONE',  ( 209.9518228411288874, 172.0000000000000284, 31.43423095485942298 ) ) ;
#22135 = ORIENTED_EDGE ( 'NONE', *, *, #45668, .F. ) ;
#22136 = EDGE_LOOP ( 'NONE', ( #66291, #30867, #17691, #8251 ) ) ;
#22137 = CARTESIAN_POINT ( 'NONE',  ( -86.06489347855098515, 25.27905598459107495, 36.66192029063178381 ) ) ;
#22139 = EDGE_CURVE ( 'NONE', #55869, #25791, #4489, .T. ) ;
#22138 = CARTESIAN_POINT ( 'NONE',  ( -24.03640295269301319, 9.507963273819777683, -70.89105126548017211 ) ) ;
#22140 = DIRECTION ( 'NONE',  ( -0.7660444431189771253, 0.6427876096865404731, 0.000000000000000000 ) ) ;
#22141 = CIRCLE ( 'NONE', #34524, 65.00000000000000000 ) ;
#22142 = DIRECTION ( 'NONE',  ( -1.000000000000000000, 0.000000000000000000, 0.000000000000000000 ) ) ;
#22143 = LINE ( 'NONE', #56495, #25238 ) ;
#22144 = EDGE_CURVE ( 'NONE', #17861, #66051, #63291, .T. ) ;
#22145 = AXIS2_PLACEMENT_3D ( 'NONE', #15915, #31746, #20846 ) ;
#22146 = VERTEX_POINT ( 'NONE', #41088 ) ;
#22147 = EDGE_CURVE ( 'NONE', #33627, #36947, #31233, .T. ) ;
#22148 = VERTEX_POINT ( 'NONE', #14693 ) ;
#22149 = PLANE ( 'NONE',  #19953 ) ;
#22150 = VECTOR ( 'NONE', #49756, 1000.000000000000000 ) ;
#22151 = VERTEX_POINT ( 'NONE', #24579 ) ;
#22152 = CARTESIAN_POINT ( 'NONE',  ( 266.9165763529819628, -52.00000000000000711, 128.9999999999999716 ) ) ;
#22153 = CARTESIAN_POINT ( 'NONE',  ( 181.7858281697336054, 80.75685888198293583, -89.93877274835493552 ) ) ;
#22154 = ADVANCED_FACE ( 'NONE', ( #57615 ), #68508, .T. ) ;
#22155 = CARTESIAN_POINT ( 'NONE',  ( 55.76298701799387914, 11.10663440745151753, 66.13237673744916378 ) ) ;
#22156 = CARTESIAN_POINT ( 'NONE',  ( 141.2794969024892850, 47.29417766120044320, 89.56677758534438283 ) ) ;
#22157 = VECTOR ( 'NONE', #1203, 1000.000000000000000 ) ;
#22158 = CARTESIAN_POINT ( 'NONE',  ( -30.58934775954355345, 10.47225103507684452, -89.04256022645139979 ) ) ;
#22159 = CARTESIAN_POINT ( 'NONE',  ( -49.42000000000000171, -36.09918303830819752, 20.41169613715280207 ) ) ;
#22160 = VECTOR ( 'NONE', #11804, 1000.000000000000000 ) ;
#22161 = ORIENTED_EDGE ( 'NONE', *, *, #10618, .T. ) ;
#22162 = EDGE_CURVE ( 'NONE', #24494, #1859, #36156, .T. ) ;
#22163 = DIRECTION ( 'NONE',  ( 0.000000000000000000, 0.000000000000000000, 1.000000000000000000 ) ) ;
#22164 = ORIENTED_EDGE ( 'NONE', *, *, #32388, .T. ) ;
#22165 = ORIENTED_EDGE ( 'NONE', *, *, #9627, .T. ) ;
#22166 = DIRECTION ( 'NONE',  ( -1.000000000000000000, 0.000000000000000000, 0.000000000000000000 ) ) ;
#22167 = CARTESIAN_POINT ( 'NONE',  ( 18.07314801315378006, 17.44990292519104003, 3.061616997868437868E-16 ) ) ;
#22168 = CARTESIAN_POINT ( 'NONE',  ( -35.00000000000000000, -35.00000000000000000, 0.000000000000000000 ) ) ;
#22169 = PLANE ( 'NONE',  #56871 ) ;
#22170 = FACE_OUTER_BOUND ( 'NONE', #63972, .T. ) ;
#22171 = VERTEX_POINT ( 'NONE', #58287 ) ;
#22172 = CARTESIAN_POINT ( 'NONE',  ( 82.34195123877069022, 18.00239921638038965, 16.52602691977476113 ) ) ;
#22173 = ORIENTED_EDGE ( 'NONE', *, *, #29173, .F. ) ;
#22174 = CARTESIAN_POINT ( 'NONE',  ( -77.72491324796695267, 21.96482567905607652, 30.46232876248773636 ) ) ;
#22175 = ORIENTED_EDGE ( 'NONE', *, *, #60985, .T. ) ;
#22176 = LINE ( 'NONE', #16889, #49928 ) ;
#22177 = ORIENTED_EDGE ( 'NONE', *, *, #29514, .F. ) ;
#22178 = CARTESIAN_POINT ( 'NONE',  ( -124.9970785861868166, 47.10847819093960709, 3.825783188233985666 ) ) ;
#22179 = CARTESIAN_POINT ( 'NONE',  ( 88.30010642107259855, 19.99780058782974734, 17.68303557786764912 ) ) ;
#22180 = LINE ( 'NONE', #6698, #14822 ) ;
#22181 = ORIENTED_EDGE ( 'NONE', *, *, #55920, .F. ) ;
#22182 = VECTOR ( 'NONE', #36965, 1000.000000000000000 ) ;
#22183 = LINE ( 'NONE', #43969, #28953 ) ;
#22184 = SHAPE_REPRESENTATION ( 'Bush', ( #66832 ), #24189 ) ;
#22185 = VECTOR ( 'NONE', #51902, 1000.000000000000114 ) ;
#22186 = CARTESIAN_POINT ( 'NONE',  ( -173.1211646369891355, -170.0000000000000000, -95.90105834567735599 ) ) ;
#22187 = CARTESIAN_POINT ( 'NONE',  ( -179.5186635612084558, 96.12511541314940189, -38.25937866299342716 ) ) ;
#22188 = CARTESIAN_POINT ( 'NONE',  ( 0.000000000000000000, 0.000000000000000000, 40.00000000000003553 ) ) ;
#22189 = CARTESIAN_POINT ( 'NONE',  ( -31.11269837220806878, 5.594483210025202879E-14, 2.000000000000001776 ) ) ;
#22190 = FACE_OUTER_BOUND ( 'NONE', #52027, .T. ) ;
#22191 = ORIENTED_EDGE ( 'NONE', *, *, #21024, .F. ) ;
#22192 = CARTESIAN_POINT ( 'NONE',  ( 139.6326990672751265, 46.22017155708128655, -75.15836175618863990 ) ) ;
#22193 = AXIS2_PLACEMENT_3D ( 'NONE', #13526, #18452, #13183 ) ;
#22194 = LINE ( 'NONE', #16564, #20906 ) ;
#22195 = ORIENTED_EDGE ( 'NONE', *, *, #28849, .F. ) ;
#22196 = FACE_BOUND ( 'NONE', #59707, .T. ) ;
#22197 = VECTOR ( 'NONE', #18734, 1000.000000000000000 ) ;
#22198 = DIRECTION ( 'NONE',  ( 1.000000000000000000, 0.000000000000000000, 0.000000000000000000 ) ) ;
#22199 = CARTESIAN_POINT ( 'NONE',  ( -178.2328124332055665, 94.56955476227568624, 59.65814836521386155 ) ) ;
#22200 = CARTESIAN_POINT ( 'NONE',  ( -145.3233446620410518, 62.00659513626053609, -9.226959667183525227 ) ) ;
#22201 = CARTESIAN_POINT ( 'NONE',  ( -118.6727642982647239, 43.09863379477474155, -44.51070304596819227 ) ) ;
#22202 = ADVANCED_FACE ( 'NONE', ( #25950 ), #36500, .F. ) ;
#22203 = CARTESIAN_POINT ( 'NONE',  ( 0.000000000000000000, 0.000000000000000000, 30.00000000000000000 ) ) ;
#22204 = DIRECTION ( 'NONE',  ( 0.000000000000000000, 0.000000000000000000, -1.000000000000000000 ) ) ;
#22205 = LINE ( 'NONE', #43292, #64007 ) ;
#22206 = CARTESIAN_POINT ( 'NONE',  ( -122.3759299995709853, 45.41285412136511468, -75.89897174332118368 ) ) ;
#22207 = CARTESIAN_POINT ( 'NONE',  ( 64.94794467308302899, 13.12874966082105033, 17.73165300221493723 ) ) ;
#22208 = CARTESIAN_POINT ( 'NONE',  ( 164.6499013411308852, 63.45576988183551492, 12.25078358121806232 ) ) ;
#22209 = CARTESIAN_POINT ( 'NONE',  ( 94.02861641584118502, 23.15570573563316259, -17.72789564107222304 ) ) ;
#22210 = ORIENTED_EDGE ( 'NONE', *, *, #41691, .T. ) ;
#22211 = AXIS2_PLACEMENT_3D ( 'NONE', #58274, #63904, #26276 ) ;
#22212 = CARTESIAN_POINT ( 'NONE',  ( -36.00304714721388422, 11.40794940913598943, 16.84363149277759675 ) ) ;
#22213 = ORIENTED_EDGE ( 'NONE', *, *, #63914, .T. ) ;
#22214 = DIRECTION ( 'NONE',  ( -0.000000000000000000, -0.000000000000000000, -1.000000000000000000 ) ) ;
#22215 = CARTESIAN_POINT ( 'NONE',  ( 86.15454111412297777, 20.32174891186170029, -77.66611478937542756 ) ) ;
#22216 = CARTESIAN_POINT ( 'NONE',  ( 117.4733638683028545, 33.50010943445380462, 92.82365936243014914 ) ) ;
#22217 = CARTESIAN_POINT ( 'NONE',  ( -143.3980294393558950, 60.45217072626397226, 60.70765849063186437 ) ) ;
#22218 = CARTESIAN_POINT ( 'NONE',  ( 66.08620257826613908, 13.40585338179127461, -9.529234331028934690 ) ) ;
#22219 = FACE_OUTER_BOUND ( 'NONE', #1068, .T. ) ;
#22220 = CARTESIAN_POINT ( 'NONE',  ( -53.38065169970957413, 15.27943072477081365, -62.24569998015859085 ) ) ;
#22221 = CARTESIAN_POINT ( 'NONE',  ( -74.09606306030876510, 21.70217968620899285, -90.35397259367368861 ) ) ;
#22222 = LINE ( 'NONE', #28185, #62196 ) ;
#22223 = ORIENTED_EDGE ( 'NONE', *, *, #7394, .F. ) ;
#22224 = ORIENTED_EDGE ( 'NONE', *, *, #6174, .T. ) ;
#22226 = ADVANCED_FACE ( 'NONE', ( #14007 ), #19985, .F. ) ;
#22225 = CARTESIAN_POINT ( 'NONE',  ( 34.45158752686798209, 8.829194381141995507, 69.91381216925195474 ) ) ;
#22227 = CARTESIAN_POINT ( 'NONE',  ( 174.6127059037623042, 72.30368563770916523, 59.82278449068079595 ) ) ;
#22228 = CARTESIAN_POINT ( 'NONE',  ( -167.4844853368928455, 82.52074065752736942, 60.21220728262811406 ) ) ;
#22229 = CARTESIAN_POINT ( 'NONE',  ( 0.000000000000000000, 0.000000000000000000, 41.38025477438755928 ) ) ;
#22230 = EDGE_CURVE ( 'NONE', #4257, #6514, #41435, .T. ) ;
#22231 = DIRECTION ( 'NONE',  ( 0.000000000000000000, 0.000000000000000000, -1.000000000000000000 ) ) ;
#22232 = ORIENTED_EDGE ( 'NONE', *, *, #21884, .T. ) ;
#22233 = CARTESIAN_POINT ( 'NONE',  ( 102.7983318509014765, 26.68040613344514611, -44.46865102779961632 ) ) ;
#22234 = CARTESIAN_POINT ( 'NONE',  ( -14.19447842053094533, 7.389800932646229725, 68.42821250095973085 ) ) ;
#22235 = CARTESIAN_POINT ( 'NONE',  ( 211.5034924207028268, 118.0100795718635283, 13.02898940588344345 ) ) ;
#22236 = CIRCLE ( 'NONE', #59278, 5.000000000000004441 ) ;
#22237 = CARTESIAN_POINT ( 'NONE',  ( -84.05936786797155946, 25.53661143797981126, -91.07400105329199391 ) ) ;
#22238 = CARTESIAN_POINT ( 'NONE',  ( 43.97326221476410524, 9.047815246749987494, -10.30912291823035787 ) ) ;
#22239 = DIRECTION ( 'NONE',  ( -0.000000000000000000, -0.000000000000000000, -1.000000000000000000 ) ) ;
#22240 = FACE_BOUND ( 'NONE', #13769, .T. ) ;
#22241 = CARTESIAN_POINT ( 'NONE',  ( -58.76005811686685831, 15.70653557534867240, -36.17866631179933279 ) ) ;
#22242 = AXIS2_PLACEMENT_3D ( 'NONE', #33060, #53105, #5282 ) ;
#22243 = EDGE_CURVE ( 'NONE', #21908, #18538, #40368, .T. ) ;
#22244 = ORIENTED_EDGE ( 'NONE', *, *, #60527, .T. ) ;
#22245 = AXIS2_PLACEMENT_3D ( 'NONE', #67094, #29778, #13264 ) ;
#22246 = CARTESIAN_POINT ( 'NONE',  ( 128.3889472838589256, 39.37765603157608041, 15.32265653812712891 ) ) ;
#22247 = CARTESIAN_POINT ( 'NONE',  ( -47.57182537987932847, 17.67134260003773605, -14.82801705809906068 ) ) ;
#22248 = CARTESIAN_POINT ( 'NONE',  ( -48.70883077256303295, 14.10659259062419224, 60.65374130472434899 ) ) ;
#22249 = FACE_OUTER_BOUND ( 'NONE', #61024, .T. ) ;
#22250 = CARTESIAN_POINT ( 'NONE',  ( 153.8366942494330942, 54.87992279068317458, 16.62999931596239378 ) ) ;
#22251 = EDGE_CURVE ( 'NONE', #7019, #15127, #5975, .T. ) ;
#22252 = EDGE_CURVE ( 'NONE', #51410, #63684, #4371, .T. ) ;
#22253 = CARTESIAN_POINT ( 'NONE',  ( -14.13685348404360731, 8.394908291011505597, 87.24003644221730269 ) ) ;
#22254 = CONICAL_SURFACE ( 'NONE', #61578, 74.95140232871122521, 0.8777644062502172329 ) ;
#22255 = EDGE_LOOP ( 'NONE', ( #67700, #24767 ) ) ;
#22256 = LINE ( 'NONE', #48960, #40432 ) ;
#22257 = CARTESIAN_POINT ( 'NONE',  ( -59.95707852844800101, 16.05120821151901822, 58.96607362597248425 ) ) ;
#22258 = ORIENTED_EDGE ( 'NONE', *, *, #35357, .F. ) ;
#22259 = AXIS2_PLACEMENT_3D ( 'NONE', #18497, #19180, #44882 ) ;
#22260 = ORIENTED_EDGE ( 'NONE', *, *, #23821, .F. ) ;
#22261 = DIRECTION ( 'NONE',  ( -0.000000000000000000, -0.000000000000000000, -1.000000000000000000 ) ) ;
#22262 = CARTESIAN_POINT ( 'NONE',  ( 447.3372781065086201, 0.000000000000000000, -146.4497041420118251 ) ) ;
#22263 = CARTESIAN_POINT ( 'NONE',  ( 105.8203563788590458, 26.88901185006198347, 43.17332345044523123 ) ) ;
#22264 = ORIENTED_EDGE ( 'NONE', *, *, #39272, .F. ) ;
#22265 = ORIENTED_EDGE ( 'NONE', *, *, #52180, .T. ) ;
#22266 = FACE_OUTER_BOUND ( 'NONE', #26736, .T. ) ;
#22267 = CARTESIAN_POINT ( 'NONE',  ( 161.7006237583814539, 62.31514460450500792, 30.69927748893351449 ) ) ;
#22268 = CARTESIAN_POINT ( 'NONE',  ( 107.0555969502564579, 28.53646637607230474, 3.461266515144562295 ) ) ;
#22269 = CARTESIAN_POINT ( 'NONE',  ( 67.55199883153193241, 14.80832170058782005, 4.476120955455310302 ) ) ;
#22270 = CARTESIAN_POINT ( 'NONE',  ( -35.00000000000000000, 225.0000000000000000, 0.000000000000000000 ) ) ;
#22271 = CARTESIAN_POINT ( 'NONE',  ( 103.8055367708241334, 27.11070767929350822, -12.69745074032687882 ) ) ;
#22272 = DIRECTION ( 'NONE',  ( -1.000000000000000000, -1.387778780781448141E-16, 5.551115123125781716E-16 ) ) ;
#22273 = CARTESIAN_POINT ( 'NONE',  ( 8.537735592981553268, 7.383000420390736451, 39.44863563677944995 ) ) ;
#22274 = FACE_OUTER_BOUND ( 'NONE', #62000, .T. ) ;
#22275 = CARTESIAN_POINT ( 'NONE',  ( 79.97490006123518924, 17.25652566631320539, 94.42763666094869279 ) ) ;
#22277 = ORIENTED_EDGE ( 'NONE', *, *, #42588, .F. ) ;
#22276 = DIRECTION ( 'NONE',  ( 0.000000000000000000, -0.000000000000000000, -1.000000000000000000 ) ) ;
#22278 = ORIENTED_EDGE ( 'NONE', *, *, #47699, .F. ) ;
#22279 = ORIENTED_EDGE ( 'NONE', *, *, #17286, .F. ) ;
#22280 = CARTESIAN_POINT ( 'NONE',  ( 86.62931800182293784, 20.48449268398423229, 56.55663816294300261 ) ) ;
#22281 = CARTESIAN_POINT ( 'NONE',  ( -165.7966693951447610, 80.76873405560772312, 93.63453536631139684 ) ) ;
#22282 = DIRECTION ( 'NONE',  ( 0.000000000000000000, 0.000000000000000000, 1.000000000000000000 ) ) ;
#22283 = EDGE_CURVE ( 'NONE', #11106, #61270, #37525, .T. ) ;
#22284 = CARTESIAN_POINT ( 'NONE',  ( -125.8938041572051389, 46.49392987655491538, 18.77539728269342945 ) ) ;
#22285 = CARTESIAN_POINT ( 'NONE',  ( -56.72676045871359207, 16.18052435693491375, -50.03113401488633372 ) ) ;
#22286 = CARTESIAN_POINT ( 'NONE',  ( -14.93280618462406828, 8.469244267267910686, -13.66615899223535280 ) ) ;
#22287 = AXIS2_PLACEMENT_3D ( 'NONE', #22073, #48098, #27340 ) ;
#22288 = CARTESIAN_POINT ( 'NONE',  ( 0.000000000000000000, 0.000000000000000000, 40.00000000000003553 ) ) ;
#22289 = CARTESIAN_POINT ( 'NONE',  ( 22.89634831467701304, 6.832298124325687283, -13.76902466704347638 ) ) ;
#22291 = EDGE_LOOP ( 'NONE', ( #17970, #27405, #69147, #22307 ) ) ;
#22290 = EDGE_CURVE ( 'NONE', #55679, #49668, #59324, .T. ) ;
#22292 = CARTESIAN_POINT ( 'NONE',  ( -31.43908319763710679, -170.0000000000000000, -35.31719736520183517 ) ) ;
#22293 = ORIENTED_EDGE ( 'NONE', *, *, #11568, .F. ) ;
#22294 = EDGE_LOOP ( 'NONE', ( #22774, #33524, #57961, #19936, #51433, #26105, #62640, #48526, #65525 ) ) ;
#22295 = AXIS2_PLACEMENT_3D ( 'NONE', #16791, #66409, #59693 ) ;
#22296 = CARTESIAN_POINT ( 'NONE',  ( 412.3372781065086201, 399.9999999999998863, 78.55029585798826020 ) ) ;
#22297 = CARTESIAN_POINT ( 'NONE',  ( 2.105723906874191037E-15, -7.321656987762880320, 3.318518101603019854 ) ) ;
#22298 = CARTESIAN_POINT ( 'NONE',  ( -28.03757796776831057, 10.07506086180835503, 84.71353597014326908 ) ) ;
#22299 = CARTESIAN_POINT ( 'NONE',  ( -95.88718821240196633, 29.65015105908825888, -46.44459427566074083 ) ) ;
#22300 = AXIS2_PLACEMENT_3D ( 'NONE', #67300, #40204, #50411 ) ;
#22301 = CARTESIAN_POINT ( 'NONE',  ( -109.7793173546317007, 36.75648380851387742, 11.45816125260146556 ) ) ;
#22302 = CARTESIAN_POINT ( 'NONE',  ( 23.09784929786603414, 6.844738137842330872, 39.21172352895144542 ) ) ;
#22303 = CARTESIAN_POINT ( 'NONE',  ( 134.7720294983483313, 43.15885542353188953, -9.221000502456890402 ) ) ;
#22304 = VERTEX_POINT ( 'NONE', #48755 ) ;
#22305 = EDGE_CURVE ( 'NONE', #60309, #44366, #591, .T. ) ;
#22306 = ORIENTED_EDGE ( 'NONE', *, *, #52096, .F. ) ;
#22307 = ORIENTED_EDGE ( 'NONE', *, *, #65368, .T. ) ;
#22308 = EDGE_CURVE ( 'NONE', #28214, #14673, #50172, .T. ) ;
#22309 = DIRECTION ( 'NONE',  ( 0.8090169943749506709, -0.5877852522924686962, 0.000000000000000000 ) ) ;
#22310 = CARTESIAN_POINT ( 'NONE',  ( 110.2429982417149432, 28.88204397445228722, -62.76698815611734972 ) ) ;
#22311 = CARTESIAN_POINT ( 'NONE',  ( 46.39999999999999858, 5.109226446042757607E-16, -4.171999999999999709 ) ) ;
#22312 = EDGE_CURVE ( 'NONE', #31650, #44375, #50520, .T. ) ;
#22313 = EDGE_CURVE ( 'NONE', #30419, #22638, #12900, .T. ) ;
#22314 = CARTESIAN_POINT ( 'NONE',  ( -38.69577193929645631, 10.89562623693159793, 62.60268121862340251 ) ) ;
#22315 = CARTESIAN_POINT ( 'NONE',  ( 201.5876148766343476, 103.8397408698165520, 70.39041556991163873 ) ) ;
#22316 = EDGE_LOOP ( 'NONE', ( #44411, #16452, #18556, #44029 ) ) ;
#22317 = CARTESIAN_POINT ( 'NONE',  ( 182.7686108735401262, 81.77235358504609053, 56.33239625640001691 ) ) ;
#22318 = CARTESIAN_POINT ( 'NONE',  ( 133.8566784816069344, -170.0000000000000000, -36.02331093239566684 ) ) ;
#22319 = CARTESIAN_POINT ( 'NONE',  ( -2.869721780807576561, 7.625909776230885839, -37.26733688883847151 ) ) ;
#22320 = FACE_OUTER_BOUND ( 'NONE', #47205, .T. ) ;
#22321 = DIRECTION ( 'NONE',  ( 0.000000000000000000, 0.000000000000000000, 1.000000000000000000 ) ) ;
#22322 = CARTESIAN_POINT ( 'NONE',  ( 22.81270948571148338, 6.827178363529886163, 66.99894383605555959 ) ) ;
#22323 = DIRECTION ( 'NONE',  ( 1.000000000000000000, 0.000000000000000000, 0.000000000000000000 ) ) ;
#22324 = CARTESIAN_POINT ( 'NONE',  ( 12.68603346975294066, 7.427591953486039067, 17.50285206886463030 ) ) ;
#22325 = ORIENTED_EDGE ( 'NONE', *, *, #28250, .T. ) ;
#22326 = LINE ( 'NONE', #64897, #49555 ) ;
#22327 = APPLICATION_PROTOCOL_DEFINITION ( 'draft international standard', 'automotive_design', 1998, #63726 ) ;
#22328 = DIRECTION ( 'NONE',  ( 0.000000000000000000, 0.000000000000000000, -1.000000000000000000 ) ) ;
#22329 = CARTESIAN_POINT ( 'NONE',  ( -133.3392045760936924, 51.59583146030207246, -43.46796065370383388 ) ) ;
#22330 = EDGE_CURVE ( 'NONE', #26863, #8775, #17226, .T. ) ;
#22331 = DIRECTION ( 'NONE',  ( 0.000000000000000000, -1.000000000000000000, 0.000000000000000000 ) ) ;
#22332 = EDGE_CURVE ( 'NONE', #30991, #28403, #34359, .T. ) ;
#22333 = CARTESIAN_POINT ( 'NONE',  ( 123.4242852856285566, 10.00000000000000000, -30.00000000000000000 ) ) ;
#22334 = ORIENTED_EDGE ( 'NONE', *, *, #62334, .F. ) ;
#22335 = B_SPLINE_CURVE_WITH_KNOTS ( 'NONE', 3,
 ( #45627, #3746, #55835, #8694, #13955, #50552, #2370, #24863, #19577, #51931, #57219, #35769, #30481, #40341, #25219, #67780, #18892, #39997, #46652, #29790, #13275, #67101, #30149, #51258, #7987, #34733, #62500, #68130, #29439, #56516, #41390, #19935, #3068, #45967, #29104, #41035, #9034, #14310, #19223, #61788, #62844, #7655, #23827, #66751, #13610, #50898, #61454, #62138, #56881, #56171, #8345, #51597, #2715, #35066, #24177, #67431, #3405, #26244, #32212, #14646, #52278, #41728 ),
 .UNSPECIFIED., .F., .F.,
 ( 4, 2, 2, 2, 2, 2, 2, 2, 2, 2, 2, 2, 2, 2, 2, 2, 2, 2, 2, 2, 2, 2, 2, 2, 2, 2, 2, 2, 2, 2, 4 ),
 ( 0.000000000000000000, 0.002279643572853625681, 0.003419465359280425294, 0.004559287145707224473, 0.005699108932134024086, 0.006269019825347425627, 0.006838930718560828036, 0.007978752504987699640, 0.009118574291414570376, 0.01025839607784144285, 0.01139821786426831358, 0.01367786143712207934, 0.01481768322354893794, 0.01595750500997579827, 0.01823714858282953280, 0.02051679215568326387, 0.02165661394211009644, 0.02279643572853692554, 0.02393625751496376158, 0.02507607930139059416, 0.02621590108781742673, 0.02735572287424425930, 0.02849554466067109534, 0.02963536644709792445, 0.03077518823352475702, 0.03191501001995159653, 0.03305483180637842217, 0.03362474269959182110, 0.03419465359280521310, 0.03533447537923198323, 0.03647429716565874641 ),
 .UNSPECIFIED. ) ;
#22336 = ORIENTED_EDGE ( 'NONE', *, *, #7662, .T. ) ;
#22337 = EDGE_CURVE ( 'NONE', #16958, #19609, #13244, .T. ) ;
#22338 = CARTESIAN_POINT ( 'NONE',  ( -133.2386639184428248, 51.52423002108237426, -94.50477388902842790 ) ) ;
#22339 = DIRECTION ( 'NONE',  ( 0.000000000000000000, 0.000000000000000000, 1.000000000000000000 ) ) ;
#22340 = ORIENTED_EDGE ( 'NONE', *, *, #46795, .T. ) ;
#22341 = VERTEX_POINT ( 'NONE', #39279 ) ;
#22342 = CARTESIAN_POINT ( 'NONE',  ( 41.49663191311417165, -50.03028622612021792, 170.0000000000000000 ) ) ;
#22343 = DIRECTION ( 'NONE',  ( 0.000000000000000000, -1.000000000000000000, 0.000000000000000000 ) ) ;
#22344 = EDGE_LOOP ( 'NONE', ( #13144, #42346, #23081, #26329 ) ) ;
#22345 = LINE ( 'NONE', #54694, #68294 ) ;
#22346 = VECTOR ( 'NONE', #49753, 1000.000000000000114 ) ;
#22347 = CARTESIAN_POINT ( 'NONE',  ( 139.2794027252094224, 45.99190465195506761, 69.05840653717436339 ) ) ;
#22348 = LINE ( 'NONE', #38171, #40951 ) ;
#22349 = B_SPLINE_CURVE_WITH_KNOTS ( 'NONE', 3,
 ( #65757, #60466, #27749, #11927, #33398, #7001 ),
 .UNSPECIFIED., .F., .F.,
 ( 4, 2, 4 ),
 ( 2.380731630024181461E-07, 0.002336973833157594133, 0.004673709593152186939 ),
 .UNSPECIFIED. ) ;
#22350 = CARTESIAN_POINT ( 'NONE',  ( -44.00727179482577611, 47.83680621839560132, 40.00000000000003553 ) ) ;
#22351 = PRESENTATION_LAYER_ASSIGNMENT (  '', '', ( #51589 ) ) ;
#22352 = DIRECTION ( 'NONE',  ( -0.000000000000000000, 1.000000000000000000, -0.000000000000000000 ) ) ;
#22353 = CARTESIAN_POINT ( 'NONE',  ( -49.44484229820457699, 14.28460989390479519, -10.86759184043735260 ) ) ;
#22354 = ORIENTED_EDGE ( 'NONE', *, *, #61698, .T. ) ;
#22355 = CARTESIAN_POINT ( 'NONE',  ( 112.5554747942046276, 29.96654954475020460, -50.56094890218214033 ) ) ;
#22356 = LINE ( 'NONE', #37840, #49389 ) ;
#22357 = CARTESIAN_POINT ( 'NONE',  ( -143.7133518487517279, 60.70463114991424902, -37.54395651202641204 ) ) ;
#22358 = CARTESIAN_POINT ( 'NONE',  ( 26.11269837220812562, 31.11269837220800483, 2.000000000000001776 ) ) ;
#22360 = VERTEX_POINT ( 'NONE', #49810 ) ;
#22359 = CARTESIAN_POINT ( 'NONE',  ( -133.1138189109049392, 51.43538799925376992, 89.75153789939945170 ) ) ;
#22361 = CARTESIAN_POINT ( 'NONE',  ( 55.56634333706182360, 12.09342294753929181, 9.466922162906941551 ) ) ;
#22362 = VERTEX_POINT ( 'NONE', #17456 ) ;
#22363 = CARTESIAN_POINT ( 'NONE',  ( -146.5341851369306028, 61.69744206542950593, 58.16577801895916622 ) ) ;
#22364 = CARTESIAN_POINT ( 'NONE',  ( -1.333402737265964699, 70.00000000000000000, -9.910703160737465822 ) ) ;
#22365 = DIRECTION ( 'NONE',  ( 0.000000000000000000, 0.7660444431189770143, 0.6427876096865403621 ) ) ;
#22366 = CARTESIAN_POINT ( 'NONE',  ( 182.5617509987553433, 80.11195108039726165, -24.23659823810514169 ) ) ;
#22367 = CARTESIAN_POINT ( 'NONE',  ( 79.52861599156696570, 17.11914630560288941, -18.94279912049138304 ) ) ;
#22368 = FACE_OUTER_BOUND ( 'NONE', #34893, .T. ) ;
#22369 = DIRECTION ( 'NONE',  ( -0.000000000000000000, 0.000000000000000000, -1.000000000000000000 ) ) ;
#22370 = EDGE_CURVE ( 'NONE', #20839, #9808, #56140, .T. ) ;
#22371 = CARTESIAN_POINT ( 'NONE',  ( -102.2801239173131194, 32.78103895658057354, 18.67452391595144334 ) ) ;
#22372 = CARTESIAN_POINT ( 'NONE',  ( -156.0525065694671696, 69.93592087802322510, -92.33156131024371405 ) ) ;
#22373 = ORIENTED_EDGE ( 'NONE', *, *, #29287, .T. ) ;
#22374 = VERTEX_POINT ( 'NONE', #66716 ) ;
#22375 = DIRECTION ( 'NONE',  ( 0.000000000000000000, 0.000000000000000000, 1.000000000000000000 ) ) ;
#22376 = CARTESIAN_POINT ( 'NONE',  ( 157.4703587214989398, -170.0000000000000000, 10.06491688178970456 ) ) ;
#22377 = CARTESIAN_POINT ( 'NONE',  ( 10.06749493632391967, 74.32123213259514216, 0.000000000000000000 ) ) ;
#22378 = CARTESIAN_POINT ( 'NONE',  ( -15.24379664668640899, 38.84509419542018094, 13.79046340968178441 ) ) ;
#22379 = CARTESIAN_POINT ( 'NONE',  ( -49.77357484059128012, -41.82599373102878104, 170.0000000000000000 ) ) ;
#22380 = DIRECTION ( 'NONE',  ( 1.000000000000000000, 0.000000000000000000, 0.000000000000000000 ) ) ;
#22381 = FACE_OUTER_BOUND ( 'NONE', #49056, .T. ) ;
#22382 = CARTESIAN_POINT ( 'NONE',  ( 46.90208227351340042, 10.52324439420451263, -43.36172691416860658 ) ) ;
#22383 = CARTESIAN_POINT ( 'NONE',  ( 161.7048274740120632, 61.01946783654761930, -76.67637307521195567 ) ) ;
#22384 = EDGE_CURVE ( 'NONE', #52636, #20984, #18514, .T. ) ;
#22385 = ORIENTED_EDGE ( 'NONE', *, *, #55416, .T. ) ;
#22386 = CARTESIAN_POINT ( 'NONE',  ( -27.49195330402088899, 9.993776132065301354, 4.489922646395196004 ) ) ;
#22387 = ORIENTED_EDGE ( 'NONE', *, *, #40258, .T. ) ;
#22388 = CARTESIAN_POINT ( 'NONE',  ( -37.38781680082739456, 10.64362327909143069, 6.278129842404852390 ) ) ;
#22389 = CARTESIAN_POINT ( 'NONE',  ( -86.17326876353082810, 25.32448302420862163, 91.54163727806503914 ) ) ;
#22390 = EDGE_CURVE ( 'NONE', #64497, #37048, #1290, .T. ) ;
#22391 = DIRECTION ( 'NONE',  ( 1.000000000000000000, 0.000000000000000000, 0.000000000000000000 ) ) ;
#22393 = CARTESIAN_POINT ( 'NONE',  ( 126.6464677212869532, 38.39096133771043640, 34.87906214376891967 ) ) ;
#22392 = B_SPLINE_CURVE_WITH_KNOTS ( 'NONE', 3,
 ( #21209, #9967, #26827, #53190, #4672, #16609, #42655, #27161, #36702, #5019, #68692, #31419, #26138, #48595, #47572, #15923, #21883, #47921, #37039, #10634, #64113, #43334, #37366, #64809, #58824, #53543, #48254, #85, #42983, #64456, #37719, #59167, #27508, #50011, #6050, #19301, #33845, #32795, #12387, #55286, #789, #49652, #1137, #7107 ),
 .UNSPECIFIED., .F., .F.,
 ( 4, 2, 2, 2, 2, 2, 2, 2, 2, 2, 2, 2, 2, 2, 2, 2, 2, 2, 2, 2, 2, 4 ),
 ( 1.387778780781445676E-17, 0.003360573201437459107, 0.004200716501796845567, 0.005040859802156232028, 0.006721146402874958112, 0.007561289703234315950, 0.008401433003593675522, 0.009241576303953032492, 0.01008171960431239120, 0.01176200620503115718, 0.01260214950539055231, 0.01344229280574994398, 0.01428243610610933738, 0.01512257940646873078, 0.01680286600718748982, 0.01764300930754687108, 0.01848315260790624887, 0.02016343920862502526, 0.02184372580934380165, 0.02352401241006257804, 0.02520429901078135443, 0.02688458561150013082 ),
 .UNSPECIFIED. ) ;
#22394 = CARTESIAN_POINT ( 'NONE',  ( 31.90170717962884694, 8.563261373066634263, 10.80943639421792746 ) ) ;
#22395 = VECTOR ( 'NONE', #29536, 1000.000000000000227 ) ;
#22396 = EDGE_CURVE ( 'NONE', #21805, #69223, #38757, .T. ) ;
#22397 = CARTESIAN_POINT ( 'NONE',  ( 86.62931800182292363, 19.42108912189597092, -35.82156419891171595 ) ) ;
#22398 = CARTESIAN_POINT ( 'NONE',  ( 74.99999999999998579, 9.184850993605147156E-15, 85.00000000000000000 ) ) ;
#22399 = CIRCLE ( 'NONE', #13424, 65.00000000000000000 ) ;
#22400 = DIRECTION ( 'NONE',  ( -0.000000000000000000, -0.000000000000000000, -1.000000000000000000 ) ) ;
#22401 = CARTESIAN_POINT ( 'NONE',  ( 46.66904755831210139, 4.999999999999909406, 0.000000000000000000 ) ) ;
#22402 = DIRECTION ( 'NONE',  ( 0.000000000000000000, 0.000000000000000000, 1.000000000000000000 ) ) ;
#22403 = VERTEX_POINT ( 'NONE', #24145 ) ;
#22404 = CARTESIAN_POINT ( 'NONE',  ( 0.000000000000000000, 0.000000000000000000, -10.00000000000000000 ) ) ;
#22405 = DIRECTION ( 'NONE',  ( -0.000000000000000000, 1.000000000000000000, -0.000000000000000000 ) ) ;
#22406 = CARTESIAN_POINT ( 'NONE',  ( -12.77550690612892126, 8.273784096785060882, 5.115475724758070442 ) ) ;
#22407 = CARTESIAN_POINT ( 'NONE',  ( -24.39249304643438521, 60.24953346690454481, 40.00000000000003553 ) ) ;
#22408 = CARTESIAN_POINT ( 'NONE',  ( -1.083610669212419220, 6.545642299653495755, 40.93835893625630717 ) ) ;
#22409 = CARTESIAN_POINT ( 'NONE',  ( -108.6634958860518338, 36.14357436892402831, -65.41376181801383893 ) ) ;
#22410 = CARTESIAN_POINT ( 'NONE',  ( 93.57136411925270636, 22.98262485654570142, 93.82112078936462751 ) ) ;
#22411 = ORIENTED_EDGE ( 'NONE', *, *, #45495, .T. ) ;
#22412 = DIRECTION ( 'NONE',  ( 0.9108602745606089179, 0.4127148655274876510, -7.830837685873009962E-15 ) ) ;
#22413 = CIRCLE ( 'NONE', #8921, 10.00000000000000178 ) ;
#22414 = DIRECTION ( 'NONE',  ( 0.000000000000000000, 0.000000000000000000, 1.000000000000000000 ) ) ;
#22415 = CARTESIAN_POINT ( 'NONE',  ( -130.1964689553233256, 49.39217932424207191, 17.43607221889983094 ) ) ;
#22416 = EDGE_CURVE ( 'NONE', #40691, #39142, #32756, .T. ) ;
#22417 = CARTESIAN_POINT ( 'NONE',  ( -171.5023337025455135, 86.83681590836891928, -49.54666913844562259 ) ) ;
#22418 = CARTESIAN_POINT ( 'NONE',  ( -133.3799602664182373, 52.86209125874979264, -41.88354727973125335 ) ) ;
#22419 = ORIENTED_EDGE ( 'NONE', *, *, #45581, .F. ) ;
#22420 = CARTESIAN_POINT ( 'NONE',  ( -118.8689810167775960, 42.03922634358562505, -45.05399606991056061 ) ) ;
#22421 = CARTESIAN_POINT ( 'NONE',  ( -4.504169684898449155, 6.697401007565304099, -9.344495963075038603 ) ) ;
#22422 = EDGE_CURVE ( 'NONE', #37971, #35286, #35268, .T. ) ;
#22423 = FACE_OUTER_BOUND ( 'NONE', #6429, .T. ) ;
#22424 = CARTESIAN_POINT ( 'NONE',  ( -1.327237339235002311, 7.561837009978236601, -66.00973041474892966 ) ) ;
#22425 =( REPRESENTATION_RELATIONSHIP ('NONE','NONE', #40274, #35767 ) REPRESENTATION_RELATIONSHIP_WITH_TRANSFORMATION ( #12924 )SHAPE_REPRESENTATION_RELATIONSHIP( ) );
#22426 = CARTESIAN_POINT ( 'NONE',  ( -63.73419499958981049, -12.83646726144931449, 170.0000000000000000 ) ) ;
#22427 = ORIENTED_EDGE ( 'NONE', *, *, #59840, .T. ) ;
#22428 = CARTESIAN_POINT ( 'NONE',  ( -15.15117926080556465, 8.490099586177995761, -95.00000000000133582 ) ) ;
#22429 = CARTESIAN_POINT ( 'NONE',  ( 197.6316695787931224, 97.13022718399025734, -41.29383634472684861 ) ) ;
#22430 = CARTESIAN_POINT ( 'NONE',  ( -151.2428028786328014, 66.99705074331122034, 30.91134539836198059 ) ) ;
#22431 = VECTOR ( 'NONE', #55876, 1000.000000000000000 ) ;
#22432 = LINE ( 'NONE', #36973, #16810 ) ;
#22434 = VERTEX_POINT ( 'NONE', #52588 ) ;
#22433 = LINE ( 'NONE', #66757, #12986 ) ;
#22435 = CARTESIAN_POINT ( 'NONE',  ( 178.1888264190354221, 77.13727704498026583, 70.58518440423399909 ) ) ;
#22436 = ORIENTED_EDGE ( 'NONE', *, *, #64725, .T. ) ;
#22437 = VERTEX_POINT ( 'NONE', #46620 ) ;
#22438 = CARTESIAN_POINT ( 'NONE',  ( -71.17819443284076897, 19.60909329639481413, -15.27992725511833427 ) ) ;
#22439 = CARTESIAN_POINT ( 'NONE',  ( -439.4229916354184979, 395.0000000000064801, -128.9497041420121093 ) ) ;
#22441 = ORIENTED_EDGE ( 'NONE', *, *, #26379, .F. ) ;
#22440 = CARTESIAN_POINT ( 'NONE',  ( 150.2060369882285045, 53.45752899907539302, 11.95053698778202467 ) ) ;
#22442 = CARTESIAN_POINT ( 'NONE',  ( 162.0835148203877054, 61.32844276806159201, 30.97683732797539946 ) ) ;
#22443 = FACE_OUTER_BOUND ( 'NONE', #66536, .T. ) ;
#22444 = VECTOR ( 'NONE', #9548, 1000.000000000000000 ) ;
#22445 = DIRECTION ( 'NONE',  ( -1.000000000000000000, -0.000000000000000000, -0.000000000000000000 ) ) ;
#22446 = PRODUCT_RELATED_PRODUCT_CATEGORY ( 'part', '', ( #43365 ) ) ;
#22447 = EDGE_LOOP ( 'NONE', ( #32856, #42222, #41834, #29931 ) ) ;
#22448 = CARTESIAN_POINT ( 'NONE',  ( -142.6105148419746911, 59.82538670924427038, -93.01220556088156854 ) ) ;
#22449 = EDGE_CURVE ( 'NONE', #34501, #48145, #4248, .T. ) ;
#22450 = LINE ( 'NONE', #12600, #62320 ) ;
#22451 = ADVANCED_FACE ( 'NONE', ( #56843 ), #19899, .F. ) ;
#22452 = CARTESIAN_POINT ( 'NONE',  ( 150.4747435624740604, 52.41018979694876379, -94.57218390293165555 ) ) ;
#22453 = CARTESIAN_POINT ( 'NONE',  ( -38.87848244732138170, 10.93141945332449616, -70.64516419336318620 ) ) ;
#22454 = CARTESIAN_POINT ( 'NONE',  ( 23.24047374271773236, 7.861801299833791390, 65.33839104122442620 ) ) ;
#22455 = VERTEX_POINT ( 'NONE', #14613 ) ;
#22456 = EDGE_LOOP ( 'NONE', ( #3155, #54342, #1046, #58446, #44332, #19503, #16705, #23206, #47895 ) ) ;
#22457 = VERTEX_POINT ( 'NONE', #57532 ) ;
#22458 = CIRCLE ( 'NONE', #20209, 24.99999999999985434 ) ;
#22459 = CARTESIAN_POINT ( 'NONE',  ( -2.645453300864630819E-14, -15.55634918610403616, 2.000000000000001776 ) ) ;
#22460 = DIRECTION ( 'NONE',  ( -0.000000000000000000, -1.000000000000000000, -0.000000000000000000 ) ) ;
#22461 = CARTESIAN_POINT ( 'NONE',  ( -38.92726670956012214, 10.94099576009806718, -43.30594718313987102 ) ) ;
#22462 = DIRECTION ( 'NONE',  ( -0.8118923937861950435, -0.5838071093367415143, 0.000000000000000000 ) ) ;
#22463 = CARTESIAN_POINT ( 'NONE',  ( 410.0000000000000000, 190.0000000000000000, -90.00000000000000000 ) ) ;
#22464 = CARTESIAN_POINT ( 'NONE',  ( -129.3963145237380843, 48.84337839101546308, 71.60049605309630749 ) ) ;
#22465 = CARTESIAN_POINT ( 'NONE',  ( -50.89515345785970624, 14.64311186056398384, 85.25617531740348909 ) ) ;
#22466 = ADVANCED_FACE ( 'NONE', ( #30799 ), #52247, .T. ) ;
#22467 = CARTESIAN_POINT ( 'NONE',  ( 83.38067517854670996, 18.33799117207140128, 57.29236275353452612 ) ) ;
#22468 = ORIENTED_EDGE ( 'NONE', *, *, #67454, .F. ) ;
#22469 = DIRECTION ( 'NONE',  ( -1.000000000000000000, 0.000000000000000000, 0.000000000000000000 ) ) ;
#22470 = FACE_OUTER_BOUND ( 'NONE', #6508, .T. ) ;
#22471 = EDGE_CURVE ( 'NONE', #30662, #68618, #37511, .T. ) ;
#22472 = ORIENTED_EDGE ( 'NONE', *, *, #36619, .F. ) ;
#22473 = CARTESIAN_POINT ( 'NONE',  ( 186.6054783416232112, 84.37128553200977876, 31.70807712453434846 ) ) ;
#22474 = LINE ( 'NONE', #43913, #9657 ) ;
#22475 = EDGE_CURVE ( 'NONE', #53864, #64948, #45350, .T. ) ;
#22476 = CARTESIAN_POINT ( 'NONE',  ( -29.70166638324963415, 57.83280658984260469, 3.061616997868437868E-16 ) ) ;
#22477 = DIRECTION ( 'NONE',  ( -1.000000000000000000, 0.000000000000000000, -0.000000000000000000 ) ) ;
#22478 = CARTESIAN_POINT ( 'NONE',  ( -55.05276343752909440, 14.68156374112637508, 18.47277718246750311 ) ) ;
#22479 = CIRCLE ( 'NONE', #35995, 24.69999999999999929 ) ;
#22480 = CARTESIAN_POINT ( 'NONE',  ( 152.8558173410470147, 54.14978343559395313, -37.69186017836011615 ) ) ;
#22481 = CARTESIAN_POINT ( 'NONE',  ( 164.1352994389932576, 64.33767534192696758, -73.91823402297541179 ) ) ;
#22482 = ORIENTED_EDGE ( 'NONE', *, *, #1432, .T. ) ;
#22483 = FACE_OUTER_BOUND ( 'NONE', #12240, .T. ) ;
#22484 = CARTESIAN_POINT ( 'NONE',  ( 2.905661822261151883E-14, 20.55634918610402906, 2.000000000000001776 ) ) ;
#22485 = ORIENTED_EDGE ( 'NONE', *, *, #41632, .F. ) ;
#22486 = CARTESIAN_POINT ( 'NONE',  ( 412.0000000000000000, 192.0000000000000000, 380.0000000000000000 ) ) ;
#22487 =( NAMED_UNIT ( * ) SI_UNIT ( $, .STERADIAN. ) SOLID_ANGLE_UNIT ( ) );
#22488 = VERTEX_POINT ( 'NONE', #42380 ) ;
#22489 = CARTESIAN_POINT ( 'NONE',  ( -85.90441187606242579, 25.21188850826091254, 39.94801297243609639 ) ) ;
#22490 = CARTESIAN_POINT ( 'NONE',  ( -26.50207385662996273, 9.849226639603653410, -75.32933197546118720 ) ) ;
#22491 = CARTESIAN_POINT ( 'NONE',  ( 46.12582897016704209, 10.39833982076225283, 40.74553764170175185 ) ) ;
#22492 = CARTESIAN_POINT ( 'NONE',  ( -24.19091603582231897, 8.513464105188679909, 66.50394091260255891 ) ) ;
#22493 = PLANE ( 'NONE',  #63386 ) ;
#22494 = VERTEX_POINT ( 'NONE', #32515 ) ;
#22495 = B_SPLINE_CURVE_WITH_KNOTS ( 'NONE', 3,
 ( #42543, #21426, #62969, #15128, #25698, #14774, #68259, #68919, #36929, #4566, #36589, #52069, #25355, #20393, #36240, #58035, #37253, #57697, #10522, #69274, #16149, #21099, #31994, #42868, #42205, #46787, #64338, #4910, #9507, #47126, #63666, #52415, #20063, #37602, #31313, #26716, #26029, #63997, #48146, #4232, #26374, #47814, #58705, #5256, #59056 ),
 .UNSPECIFIED., .F., .F.,
 ( 4, 2, 2, 2, 2, 2, 2, 2, 2, 2, 2, 1, 2, 2, 2, 2, 2, 2, 2, 2, 2, 2, 4 ),
 ( 0.000000000000000000, 0.001512548138464654733, 0.002268822207696980040, 0.003025096276929305564, 0.004537644415393922784, 0.005293918484626250476, 0.006050192553858578168, 0.007562740692323231817, 0.009075288830787885466, 0.01058783696925254258, 0.01134411103848488936, 0.01210038510771723613, 0.01285665917694958464, 0.01361293324618193142, 0.01512548138464657639, 0.01588175545387889021, 0.01663802952311120575, 0.01815057766157582991, 0.01966312580004045407, 0.02041939986927276962, 0.02117567393850508517, 0.02268822207696974402, 0.02420077021543440635 ),
 .UNSPECIFIED. ) ;
#22496 = VERTEX_POINT ( 'NONE', #5438 ) ;
#22497 = VECTOR ( 'NONE', #65261, 1000.000000000000114 ) ;
#22498 = CARTESIAN_POINT ( 'NONE',  ( -19.46539569203835640, 15.68752276659279943, 0.000000000000000000 ) ) ;
#22499 = EDGE_LOOP ( 'NONE', ( #10703, #1544, #14529, #51698 ) ) ;
#22500 = CARTESIAN_POINT ( 'NONE',  ( 33.75794032130628608, 8.754084575552406378, -11.31189195812216397 ) ) ;
#22501 = CARTESIAN_POINT ( 'NONE',  ( -49.77357484059128012, -41.82599373102878104, 170.0000000000000000 ) ) ;
#22502 = CARTESIAN_POINT ( 'NONE',  ( 55.76066037845576062, 11.10616952318089368, 62.19232937580554221 ) ) ;
#22503 = DIRECTION ( 'NONE',  ( -0.000000000000000000, -0.000000000000000000, -1.000000000000000000 ) ) ;
#22504 = CARTESIAN_POINT ( 'NONE',  ( 0.000000000000000000, 0.000000000000000000, 0.000000000000000000 ) ) ;
#22505 = CARTESIAN_POINT ( 'NONE',  ( 15.55634918610411610, 51.66904755831205875, 0.000000000000000000 ) ) ;
#22506 = ORIENTED_EDGE ( 'NONE', *, *, #51233, .T. ) ;
#22507 = DIRECTION ( 'NONE',  ( 0.000000000000000000, 0.000000000000000000, -1.000000000000000000 ) ) ;
#22508 = EDGE_LOOP ( 'NONE', ( #55303, #59306, #20598, #49939 ) ) ;
#22509 = ORIENTED_EDGE ( 'NONE', *, *, #9143, .F. ) ;
#22510 = CARTESIAN_POINT ( 'NONE',  ( -84.49322488516129681, 0.000000000000000000, 43.58025477438756212 ) ) ;
#22511 = CARTESIAN_POINT ( 'NONE',  ( -27.00000000000000355, -27.00000000000000355, 15.00000000000000000 ) ) ;
#22512 = DIRECTION ( 'NONE',  ( -1.000000000000000000, 0.000000000000000000, 0.000000000000000000 ) ) ;
#22513 = CARTESIAN_POINT ( 'NONE',  ( 138.6020257460770040, 44.36414356192210562, -64.53975052502872245 ) ) ;
#22514 = CARTESIAN_POINT ( 'NONE',  ( 447.3372781065085633, 400.0000000000000568, -146.4497041420118251 ) ) ;
#22515 = VECTOR ( 'NONE', #21948, 1000.000000000000000 ) ;
#22516 = ORIENTED_EDGE ( 'NONE', *, *, #8767, .F. ) ;
#22517 = CARTESIAN_POINT ( 'NONE',  ( 79.19132716134490124, 17.01584750883626995, 9.372603967536683456 ) ) ;
#22518 = ORIENTED_EDGE ( 'NONE', *, *, #41689, .F. ) ;
#22519 = CARTESIAN_POINT ( 'NONE',  ( -73.79615177260656367, 20.52570924097573624, 43.64279597580159731 ) ) ;
#22520 = ORIENTED_EDGE ( 'NONE', *, *, #60033, .T. ) ;
#22521 = CARTESIAN_POINT ( 'NONE',  ( -118.4753258120605466, 42.97785158603420541, -95.00000000000133582 ) ) ;
#22522 = EDGE_LOOP ( 'NONE', ( #63538, #43447, #13532, #14674 ) ) ;
#22523 = CARTESIAN_POINT ( 'NONE',  ( -146.5341851369306028, 61.69744206542950593, -76.05697493335925685 ) ) ;
#22524 = VECTOR ( 'NONE', #59238, 1000.000000000000000 ) ;
#22525 = CARTESIAN_POINT ( 'NONE',  ( 94.11746922806585758, 22.11341285603783291, 10.85955068103982057 ) ) ;
#22526 = EDGE_CURVE ( 'NONE', #62198, #9445, #25192, .T. ) ;
#22527 = CARTESIAN_POINT ( 'NONE',  ( 188.9999999999999432, -35.00000000000000000, 0.000000000000000000 ) ) ;
#22528 = EDGE_LOOP ( 'NONE', ( #415, #27881 ) ) ;
#22529 = DIRECTION ( 'NONE',  ( -0.000000000000000000, 1.000000000000000000, -0.000000000000000000 ) ) ;
#22530 = EDGE_CURVE ( 'NONE', #42281, #45595, #5771, .T. ) ;
#22531 = CARTESIAN_POINT ( 'NONE',  ( -17.50000000000002842, -18.06806526123148160, 0.000000000000000000 ) ) ;
#22532 = CARTESIAN_POINT ( 'NONE',  ( 32.38493285958205092, 8.611594965040675120, 34.75454220440185082 ) ) ;
#22533 = CARTESIAN_POINT ( 'NONE',  ( -177.5100621450480105, 93.70693725195826573, -48.31160080727584472 ) ) ;
#22534 = EDGE_CURVE ( 'NONE', #44530, #52688, #49565, .T. ) ;
#22535 = CARTESIAN_POINT ( 'NONE',  ( -128.9925397612932727, 48.56800623462827815, -22.40303128747859063 ) ) ;
#22536 = CARTESIAN_POINT ( 'NONE',  ( -45.00000000000000000, 22.99999999999998579, 0.000000000000000000 ) ) ;
#22537 = DIRECTION ( 'NONE',  ( 1.000000000000000000, 0.000000000000000000, 0.000000000000000000 ) ) ;
#22538 = VERTEX_POINT ( 'NONE', #18087 ) ;
#22539 = PLANE ( 'NONE',  #61287 ) ;
#22540 = CARTESIAN_POINT ( 'NONE',  ( -148.0058283997321098, 64.22864592525515093, -76.50871507917976544 ) ) ;
#22541 = ORIENTED_EDGE ( 'NONE', *, *, #15413, .T. ) ;
#22542 = EDGE_CURVE ( 'NONE', #50285, #45819, #21061, .T. ) ;
#22543 = FACE_BOUND ( 'NONE', #52066, .T. ) ;
#22544 = CARTESIAN_POINT ( 'NONE',  ( -4.955782747743210592, 6.720825863997140992, -76.70478924277563237 ) ) ;
#22545 = CARTESIAN_POINT ( 'NONE',  ( -31.43908319763709969, 10.61114334766716105, 30.21645440618916112 ) ) ;
#22546 = CARTESIAN_POINT ( 'NONE',  ( 0.08285530295198817452, 1.570896314769990587, 8.000000000000000000 ) ) ;
#22547 = CARTESIAN_POINT ( 'NONE',  ( 20.79325243092002751, 13.87950479462545772, 0.000000000000000000 ) ) ;
#22548 = CARTESIAN_POINT ( 'NONE',  ( -4.071369321747702053, 7.682719369516286534, 44.12691017724150555 ) ) ;
#22549 = CARTESIAN_POINT ( 'NONE',  ( 29.69502258243350923, 57.82046033912877903, 40.00000000000003553 ) ) ;
#22550 = CARTESIAN_POINT ( 'NONE',  ( 32.24915330809657377, -20.72408693595937734, 13.32819397642332326 ) ) ;
#22551 = CARTESIAN_POINT ( 'NONE',  ( -7.825402957745083654, 7.899365992529244984, -8.573520141480125645 ) ) ;
#22552 = CARTESIAN_POINT ( 'NONE',  ( -11.56945424397728139, 8.173256823723107800, 31.11234499143955645 ) ) ;
#22553 = CARTESIAN_POINT ( 'NONE',  ( 116.6457744947906860, 31.95847117670279403, 6.352866292760225519 ) ) ;
#22554 = CARTESIAN_POINT ( 'NONE',  ( 44.78501478287838466, 10.18870581198737391, -91.58250997119135661 ) ) ;
#22555 = ORIENTED_EDGE ( 'NONE', *, *, #39885, .T. ) ;
#22556 = CARTESIAN_POINT ( 'NONE',  ( -33.12994257348896099, 10.89587983539684402, 3.560888656335561731 ) ) ;
#22557 = VERTEX_POINT ( 'NONE', #28998 ) ;
#22558 = CARTESIAN_POINT ( 'NONE',  ( -443.1884682831975510, 394.9771332441898721, 92.74116978071172923 ) ) ;
#22559 = EDGE_CURVE ( 'NONE', #61856, #51247, #60641, .T. ) ;
#22560 = DIRECTION ( 'NONE',  ( -0.000000000000000000, 1.000000000000000000, -0.000000000000000000 ) ) ;
#22561 = CARTESIAN_POINT ( 'NONE',  ( 116.5839788410853544, 33.05236809212184568, 86.78057374190305495 ) ) ;
#22562 = CARTESIAN_POINT ( 'NONE',  ( 181.0840389613909736, -170.0000000000000000, -63.06960825634327961 ) ) ;
#22563 = CARTESIAN_POINT ( 'NONE',  ( 68.63487067129261732, 14.04635751989138903, -11.38481879685736153 ) ) ;
#22564 = AXIS2_PLACEMENT_3D ( 'NONE', #58143, #56766, #57797 ) ;
#22565 = CARTESIAN_POINT ( 'NONE',  ( -26.50207385662994852, 9.849226639603649858, -48.48478138499748979 ) ) ;
#22566 = CARTESIAN_POINT ( 'NONE',  ( -190.6985136298601731, 109.1272424661242582, -95.00000000000133582 ) ) ;
#22567 = VECTOR ( 'NONE', #19309, 1000.000000000000000 ) ;
#22568 = FACE_OUTER_BOUND ( 'NONE', #60609, .T. ) ;
#22569 = CARTESIAN_POINT ( 'NONE',  ( -125.8938041572051389, 47.69968343338778283, 3.775397282693376155 ) ) ;
#22570 = VERTEX_POINT ( 'NONE', #28637 ) ;
#22571 = ORIENTED_EDGE ( 'NONE', *, *, #27974, .F. ) ;
#22572 = DIRECTION ( 'NONE',  ( 0.000000000000000000, 1.000000000000000000, 0.000000000000000000 ) ) ;
#22573 = CARTESIAN_POINT ( 'NONE',  ( 174.2469308602414912, 71.96142024047682639, 60.55816399741460287 ) ) ;
#22574 = B_SPLINE_CURVE_WITH_KNOTS ( 'NONE', 3,
 ( #49545, #17192, #65760, #65051 ),
 .UNSPECIFIED., .F., .F.,
 ( 4, 4 ),
 ( 9.900409499083079903E-07, 0.05658314289920115397 ),
 .UNSPECIFIED. ) ;
#22576 = CARTESIAN_POINT ( 'NONE',  ( 42.02161712141799654, -26.09918303830819042, 30.00000000000000000 ) ) ;
#22575 = AXIS2_PLACEMENT_3D ( 'NONE', #47608, #30767, #69061 ) ;
#22577 = DIRECTION ( 'NONE',  ( -1.000000000000000000, 0.000000000000000000, 0.000000000000000000 ) ) ;
#22578 = CONICAL_SURFACE ( 'NONE', #23748, 8.000000000000000000, 1.047197551196600296 ) ;
#22579 = LINE ( 'NONE', #33498, #28556 ) ;
#22580 = ORIENTED_EDGE ( 'NONE', *, *, #15817, .F. ) ;
#22581 = CARTESIAN_POINT ( 'NONE',  ( 102.7414208686707866, 26.65627265923299660, -42.93303738452352292 ) ) ;
#22582 = CARTESIAN_POINT ( 'NONE',  ( 188.4918087359956758, 87.93403732562657638, -18.09163806308507461 ) ) ;
#22583 = CARTESIAN_POINT ( 'NONE',  ( -85.45399718454963534, 25.02415453493131281, -12.57056528233159298 ) ) ;
#22584 = DIRECTION ( 'NONE',  ( 1.387778780781445922E-16, -1.000000000000000000, -1.232595164407830946E-32 ) ) ;
#22585 = CARTESIAN_POINT ( 'NONE',  ( 45.36109889487609337, 9.259412558041139718, -11.69495450463035446 ) ) ;
#22586 = CARTESIAN_POINT ( 'NONE',  ( 206.3125232506203020, 108.5822159704961933, -9.646018633704194656 ) ) ;
#22587 = FACE_BOUND ( 'NONE', #66886, .T. ) ;
#22588 = CARTESIAN_POINT ( 'NONE',  ( -62.30463872474476261, 16.74658165105248386, -44.69399102852965200 ) ) ;
#22589 = VERTEX_POINT ( 'NONE', #12458 ) ;
#22590 = LINE ( 'NONE', #44030, #44749 ) ;
#22591 = CARTESIAN_POINT ( 'NONE',  ( 92.95016907945944240, 22.74936990452174967, -47.36605269353328396 ) ) ;
#22592 = LINE ( 'NONE', #12393, #54326 ) ;
#22593 = CARTESIAN_POINT ( 'NONE',  ( 34.76618902119740540, 54.93755186520760958, 41.38025477438755928 ) ) ;
#22594 = DIRECTION ( 'NONE',  ( -0.000000000000000000, -0.000000000000000000, -1.000000000000000000 ) ) ;
#22595 = CARTESIAN_POINT ( 'NONE',  ( 0.000000000000000000, 0.000000000000000000, 0.000000000000000000 ) ) ;
#22596 = EDGE_CURVE ( 'NONE', #63625, #65931, #56065, .T. ) ;
#22597 = ORIENTED_EDGE ( 'NONE', *, *, #36771, .T. ) ;
#22598 = DIRECTION ( 'NONE',  ( -0.000000000000000000, -0.000000000000000000, -1.000000000000000000 ) ) ;
#22599 = DIRECTION ( 'NONE',  ( 0.000000000000000000, 0.000000000000000000, 1.000000000000000000 ) ) ;
#22600 = ORIENTED_EDGE ( 'NONE', *, *, #29018, .F. ) ;
#22601 = ORIENTED_EDGE ( 'NONE', *, *, #56275, .T. ) ;
#22602 = LINE ( 'NONE', #28219, #22924 ) ;
#22603 = LINE ( 'NONE', #54604, #69196 ) ;
#22604 = CARTESIAN_POINT ( 'NONE',  ( 108.3906473026529511, 28.03385344351497110, 44.39384328560462478 ) ) ;
#22605 = ORIENTED_EDGE ( 'NONE', *, *, #25898, .F. ) ;
#22606 = VECTOR ( 'NONE', #31175, 1000.000000000000000 ) ;
#22607 = ORIENTED_EDGE ( 'NONE', *, *, #15404, .F. ) ;
#22608 = LINE ( 'NONE', #1156, #10540 ) ;
#22609 = CARTESIAN_POINT ( 'NONE',  ( 164.8444104055694481, 64.93678790243656351, 35.51303964267133750 ) ) ;
#22610 = CARTESIAN_POINT ( 'NONE',  ( -156.9900125991011066, 72.16580261738675972, -69.74404362362140830 ) ) ;
#22611 = FACE_OUTER_BOUND ( 'NONE', #12705, .T. ) ;
#22612 = DIRECTION ( 'NONE',  ( 0.000000000000000000, 0.000000000000000000, 1.000000000000000000 ) ) ;
#22613 = AXIS2_PLACEMENT_3D ( 'NONE', #3743, #19932, #40338 ) ;
#22614 = PRODUCT_DEFINITION_SHAPE ( 'NONE', 'NONE',  #63276 ) ;
#22615 = ADVANCED_FACE ( 'NONE', ( #11747 ), #1921, .F. ) ;
#22616 = CIRCLE ( 'NONE', #9176, 74.95140232871122521 ) ;
#22617 = PRESENTATION_LAYER_ASSIGNMENT (  '', '', ( #8013 ) ) ;
#22618 = CARTESIAN_POINT ( 'NONE',  ( 109.3047140914111850, 29.55674059952506738, -9.121791405023586208 ) ) ;
#22619 = FACE_OUTER_BOUND ( 'NONE', #30603, .T. ) ;
#22620 = CARTESIAN_POINT ( 'NONE',  ( -131.6253556217205016, 51.61436399519948282, -20.43251446978527852 ) ) ;
#22621 = CARTESIAN_POINT ( 'NONE',  ( -153.4120976477049965, 68.90960692040326308, -89.59491812855455350 ) ) ;
#22622 = DIRECTION ( 'NONE',  ( 0.000000000000000000, -0.000000000000000000, -1.000000000000000000 ) ) ;
#22623 = DIRECTION ( 'NONE',  ( 0.000000000000000000, 1.000000000000000000, 0.000000000000000000 ) ) ;
#22625 = VERTEX_POINT ( 'NONE', #54658 ) ;
#22624 = CARTESIAN_POINT ( 'NONE',  ( 0.7145311798163274108, 9.237604307034018802, -2.124379920709345337E-16 ) ) ;
#22626 = ORIENTED_EDGE ( 'NONE', *, *, #31980, .F. ) ;
#22627 = EDGE_CURVE ( 'NONE', #22403, #66816, #25104, .T. ) ;
#22628 = VECTOR ( 'NONE', #41595, 1000.000000000000000 ) ;
#22629 = ORIENTED_EDGE ( 'NONE', *, *, #26229, .T. ) ;
#22630 = CARTESIAN_POINT ( 'NONE',  ( -11.14445507968271265, 7.129894202659272651, -22.80362678214407168 ) ) ;
#22631 = CARTESIAN_POINT ( 'NONE',  ( -165.8387952943256778, 80.81203372455925660, 93.81362447417453154 ) ) ;
#22632 = DIRECTION ( 'NONE',  ( -0.000000000000000000, -0.000000000000000000, -1.000000000000000000 ) ) ;
#22633 = CARTESIAN_POINT ( 'NONE',  ( -46.66904755831210139, 6.635317295611287136E-14, 85.00100000000000477 ) ) ;
#22634 = CARTESIAN_POINT ( 'NONE',  ( -55.53456145826331181, 15.85318253404851419, -50.21632399845988459 ) ) ;
#22635 = CYLINDRICAL_SURFACE ( 'NONE', #32110, 5.000000000000000888 ) ;
#22636 = FACE_OUTER_BOUND ( 'NONE', #67647, .T. ) ;
#22637 = FACE_OUTER_BOUND ( 'NONE', #1503, .T. ) ;
#22638 = VERTEX_POINT ( 'NONE', #68013 ) ;
#22639 = FACE_OUTER_BOUND ( 'NONE', #4931, .T. ) ;
#22640 = EDGE_LOOP ( 'NONE', ( #23964, #29233, #64608, #64688 ) ) ;
#22641 = VERTEX_POINT ( 'NONE', #24411 ) ;
#22642 = EDGE_CURVE ( 'NONE', #4373, #10658, #1754, .T. ) ;
#22643 = CARTESIAN_POINT ( 'NONE',  ( -37.26544890750056283, -8.987879958075955855, 13.32819397642332682 ) ) ;
#22644 =( NAMED_UNIT ( * ) SI_UNIT ( $, .STERADIAN. ) SOLID_ANGLE_UNIT ( ) );
#22645 = DIRECTION ( 'NONE',  ( 0.5508969814521065267, -0.8345732537212999791, 0.000000000000000000 ) ) ;
#22647 = EDGE_CURVE ( 'NONE', #44455, #20799, #30719, .T. ) ;
#22646 = CARTESIAN_POINT ( 'NONE',  ( -21.27554331372999741, 61.43430442924864820, 170.0000000000000000 ) ) ;
#22648 = CARTESIAN_POINT ( 'NONE',  ( 442.3372781065085633, 369.9999999999999432, -141.4497041420118251 ) ) ;
#22649 = CARTESIAN_POINT ( 'NONE',  ( -125.0000000000000000, 1.530808498934191561E-14, 5.000000000000000000 ) ) ;
#22650 = CARTESIAN_POINT ( 'NONE',  ( 141.3400002717722828, 47.33399859146518907, -16.11108315197586194 ) ) ;
#22651 = ORIENTED_EDGE ( 'NONE', *, *, #45440, .T. ) ;
#22652 = ORIENTED_EDGE ( 'NONE', *, *, #21924, .T. ) ;
#22653 = ORIENTED_EDGE ( 'NONE', *, *, #69545, .T. ) ;
#22654 = CARTESIAN_POINT ( 'NONE',  ( -10.00000000000000000, 0.000000000000000000, 170.0010000000000048 ) ) ;
#22655 = CARTESIAN_POINT ( 'NONE',  ( -156.9919426121902575, 72.16759471857101005, -14.90541269196195451 ) ) ;
#22656 = CARTESIAN_POINT ( 'NONE',  ( 112.3013380801407521, 388.0000000000077307, 96.05029585798746439 ) ) ;
#22657 = CARTESIAN_POINT ( 'NONE',  ( 55.90910788310615231, 11.13585330978403576, -13.92866980567223756 ) ) ;
#22658 = UNCERTAINTY_MEASURE_WITH_UNIT (LENGTH_MEASURE( 1.000000000000000082E-05 ), #50619, 'distance_accuracy_value', 'NONE');
#22659 = AXIS2_PLACEMENT_3D ( 'NONE', #61621, #51068, #13096 ) ;
#22660 = CARTESIAN_POINT ( 'NONE',  ( -102.2801239173131194, 32.78103895658057354, 45.51907450641513009 ) ) ;
#22661 = PLANE ( 'NONE',  #60989 ) ;
#22662 = ORIENTED_EDGE ( 'NONE', *, *, #35754, .T. ) ;
#22663 = CARTESIAN_POINT ( 'NONE',  ( 181.0840389613909736, 80.03940679743416808, 56.15314469597509373 ) ) ;
#22664 = CARTESIAN_POINT ( 'NONE',  ( -156.7487895666416762, 70.57327586518566420, 63.09231583114617337 ) ) ;
#22665 = VECTOR ( 'NONE', #65262, 1000.000000000000000 ) ;
#22666 = DIRECTION ( 'NONE',  ( -9.860761315262647568E-31, 2.366582715663035416E-30, 1.000000000000000000 ) ) ;
#22667 = CARTESIAN_POINT ( 'NONE',  ( -0.7076388175553602888, 7.538734751903869657, -45.33243332686139127 ) ) ;
#22668 = CARTESIAN_POINT ( 'NONE',  ( 105.4375968828853729, 26.72149058755205786, 16.03008684478035661 ) ) ;
#22669 = CARTESIAN_POINT ( 'NONE',  ( -167.9399687280718751, 81.54040755612503233, -90.45838053675130652 ) ) ;
#22670 = DIRECTION ( 'NONE',  ( -0.000000000000000000, 0.02271222823333339177, -0.9997420440737084801 ) ) ;
#22671 = FACE_BOUND ( 'NONE', #30482, .T. ) ;
#22672 = CARTESIAN_POINT ( 'NONE',  ( 209.3223706822284100, 0.000000000000000000, 31.44247402469554942 ) ) ;
#22673 = CARTESIAN_POINT ( 'NONE',  ( 10.83046137699561484, 6.392429922561257527, -64.21464171610804783 ) ) ;
#22674 = EDGE_LOOP ( 'NONE', ( #64873, #65635, #17115, #38266 ) ) ;
#22675 = LINE ( 'NONE', #11069, #29346 ) ;
#22676 = CLOSED_SHELL ( 'NONE', ( #15436, #27058, #28984, #13852, #3753, #3151, #49477, #30584, #69129, #30111, #38824, #31453, #62504, #15634, #10233 ) ) ;
#22677 = DIRECTION ( 'NONE',  ( -0.000000000000000000, -0.000000000000000000, -1.000000000000000000 ) ) ;
#22678 = CARTESIAN_POINT ( 'NONE',  ( -132.4951995226844872, 50.99687809989499243, -45.98269415215550993 ) ) ;
#22679 = CARTESIAN_POINT ( 'NONE',  ( 46.65037935242578016, 9.463293687292242851, -68.02239084012497017 ) ) ;
#22680 = DIRECTION ( 'NONE',  ( 0.000000000000000000, 0.000000000000000000, -1.000000000000000000 ) ) ;
#22681 = VERTEX_POINT ( 'NONE', #35302 ) ;
#22682 = ADVANCED_FACE ( 'NONE', ( #56758 ), #8580, .F. ) ;
#22683 = VERTEX_POINT ( 'NONE', #30369 ) ;
#22684 = CARTESIAN_POINT ( 'NONE',  ( -447.6627218934914367, 399.9999999999998863, -116.4497041420118393 ) ) ;
#22685 = CARTESIAN_POINT ( 'NONE',  ( 180.9522142081943059, 78.47222086051785084, 82.99343427934738315 ) ) ;
#22686 = ORIENTED_EDGE ( 'NONE', *, *, #34348, .F. ) ;
#22687 = ADVANCED_FACE ( 'NONE', ( #51821 ), #3628, .T. ) ;
#22688 = EDGE_LOOP ( 'NONE', ( #46218, #57249, #4689, #56444 ) ) ;
#22689 = CARTESIAN_POINT ( 'NONE',  ( 180.2473887773227545, 77.76029175826236894, -36.22505766587961773 ) ) ;
#22690 = CARTESIAN_POINT ( 'NONE',  ( -78.66644367742111399, 22.32174330031318021, -23.27090004125422595 ) ) ;
#22691 = ORIENTED_EDGE ( 'NONE', *, *, #60489, .F. ) ;
#22692 = DIRECTION ( 'NONE',  ( 1.000000000000000000, 0.000000000000000000, 0.000000000000000000 ) ) ;
#22693 = LINE ( 'NONE', #544, #14282 ) ;
#22694 = CARTESIAN_POINT ( 'NONE',  ( -77.72491324796695267, 21.96482567905607297, -50.07132300890329901 ) ) ;
#22695 = CARTESIAN_POINT ( 'NONE',  ( 69.68177367721139603, 20.52767805628179687, 0.000000000000000000 ) ) ;
#22696 = CARTESIAN_POINT ( 'NONE',  ( 90.31682503704257670, 20.71196693118262289, -36.77252112897771497 ) ) ;
#22697 = CARTESIAN_POINT ( 'NONE',  ( -50.52615126106341847, 14.55080735582893148, -21.87146891271175875 ) ) ;
#22698 = ADVANCED_FACE ( 'NONE', ( #46892 ), #4334, .F. ) ;
#22699 = ORIENTED_EDGE ( 'NONE', *, *, #54445, .F. ) ;
#22700 = EDGE_CURVE ( 'NONE', #25068, #52964, #21526, .T. ) ;
#22701 = DIRECTION ( 'NONE',  ( -0.000000000000000000, -0.000000000000000000, -1.000000000000000000 ) ) ;
#22702 = FACE_BOUND ( 'NONE', #45968, .T. ) ;
#22703 = CARTESIAN_POINT ( 'NONE',  ( -142.5087559769085033, 59.74468185400780129, -39.56408865608762682 ) ) ;
#22704 = EDGE_CURVE ( 'NONE', #28859, #54708, #69375, .T. ) ;
#22705 = CARTESIAN_POINT ( 'NONE',  ( -171.5023337025454850, 86.83681590836890507, -76.39121972890930579 ) ) ;
#22707 = ORIENTED_EDGE ( 'NONE', *, *, #15906, .T. ) ;
#22706 = CARTESIAN_POINT ( 'NONE',  ( -132.6405077585060042, 51.09958558523505445, 88.51731180315442771 ) ) ;
#22708 = DIRECTION ( 'NONE',  ( 0.000000000000000000, 0.000000000000000000, 1.000000000000000000 ) ) ;
#22709 = CIRCLE ( 'NONE', #59744, 65.00000000000000000 ) ;
#22710 = EDGE_CURVE ( 'NONE', #24054, #10586, #29403, .T. ) ;
#22711 = EDGE_CURVE ( 'NONE', #58737, #49213, #69018, .T. ) ;
#22712 = VERTEX_POINT ( 'NONE', #36692 ) ;
#22713 = VECTOR ( 'NONE', #38009, 1000.000000000000000 ) ;
#22714 = CARTESIAN_POINT ( 'NONE',  ( -146.1260528621668016, 61.36307454672304829, 58.35490513784959887 ) ) ;
#22715 = DIRECTION ( 'NONE',  ( 0.000000000000000000, 0.000000000000000000, 1.000000000000000000 ) ) ;
#22716 = CARTESIAN_POINT ( 'NONE',  ( 24.96873044429757726, 1.250000000000021982, 0.000000000000000000 ) ) ;
#22717 = FACE_OUTER_BOUND ( 'NONE', #68381, .T. ) ;
#22718 = AXIS2_PLACEMENT_3D ( 'NONE', #47042, #30525, #57944 ) ;
#22719 = CARTESIAN_POINT ( 'NONE',  ( 82.94943325692328528, 18.19803534719806137, -23.01670398887183921 ) ) ;
#22720 = CARTESIAN_POINT ( 'NONE',  ( -27.00000000000000355, -27.00000000000000355, 12.00000000000000000 ) ) ;
#22721 = DIRECTION ( 'NONE',  ( -0.000000000000000000, 1.000000000000000000, -0.000000000000000000 ) ) ;
#22722 = CARTESIAN_POINT ( 'NONE',  ( -25.50819575705322606, 8.692660622847146357, -91.89581271472285096 ) ) ;
#22723 = CARTESIAN_POINT ( 'NONE',  ( -55.05276343752909440, 15.72344139423348430, 45.31732777293115788 ) ) ;
#22724 = ORIENTED_EDGE ( 'NONE', *, *, #61822, .F. ) ;
#22725 = VERTEX_POINT ( 'NONE', #58137 ) ;
#22726 = EDGE_CURVE ( 'NONE', #65848, #60623, #32092, .T. ) ;
#22727 = CARTESIAN_POINT ( 'NONE',  ( 46.50207827473962396, 9.439498081273459462, 34.98490145612715452 ) ) ;
#22728 = CARTESIAN_POINT ( 'NONE',  ( -173.1211646369891355, 88.63826465341152527, 72.66624519710475738 ) ) ;
#22729 = LINE ( 'NONE', #43127, #48048 ) ;
#22731 = EDGE_CURVE ( 'NONE', #8388, #25022, #64796, .T. ) ;
#22730 = CARTESIAN_POINT ( 'NONE',  ( 433.3728120124415568, 388.0000000000065938, 99.58582976392126795 ) ) ;
#22732 = EDGE_CURVE ( 'NONE', #28312, #33243, #64443, .T. ) ;
#22733 = ADVANCED_FACE ( 'NONE', ( #47223 ), #4936, .T. ) ;
#22734 = CARTESIAN_POINT ( 'NONE',  ( 210.0055645826033981, 115.7254585628714096, -49.14771549242088611 ) ) ;
#22735 = CARTESIAN_POINT ( 'NONE',  ( -71.15374617000811952, 20.66492714610676273, -69.44983854139488244 ) ) ;
#22736 = CARTESIAN_POINT ( 'NONE',  ( -109.7290872258107299, 36.72869630780160577, 63.84435436436351807 ) ) ;
#22737 = CARTESIAN_POINT ( 'NONE',  ( -29.49620345460273185, 9.280093073089044964, -35.55655680868790114 ) ) ;
#22738 = CARTESIAN_POINT ( 'NONE',  ( 162.7921669283191761, 61.91024532638674316, -75.75915507580972985 ) ) ;
#22739 = ORIENTED_EDGE ( 'NONE', *, *, #42584, .T. ) ;
#22740 = DIRECTION ( 'NONE',  ( -0.000000000000000000, -0.000000000000000000, 1.000000000000000000 ) ) ;
#22741 = ORIENTED_EDGE ( 'NONE', *, *, #22961, .F. ) ;
#22742 = LINE ( 'NONE', #28009, #25147 ) ;
#22743 = CARTESIAN_POINT ( 'NONE',  ( -86.07006026987795622, 25.28121476708071924, 92.84969470335587971 ) ) ;
#22744 = CARTESIAN_POINT ( 'NONE',  ( -82.93267503967652488, 23.99263498936122119, 70.93582899126512586 ) ) ;
#22745 = CARTESIAN_POINT ( 'NONE',  ( 130.3281282802763315, 40.49854652972196334, 30.37535463369031774 ) ) ;
#22746 = DIRECTION ( 'NONE',  ( 0.000000000000000000, 1.000000000000000000, -0.000000000000000000 ) ) ;
#22747 = CARTESIAN_POINT ( 'NONE',  ( 45.74764628539747235, 59.37057832282332726, 41.38025477438755928 ) ) ;
#22748 = CARTESIAN_POINT ( 'NONE',  ( 117.3187069485358620, 33.42192264892479869, -94.58789033624162812 ) ) ;
#22749 = DIRECTION ( 'NONE',  ( 0.000000000000000000, 0.000000000000000000, -1.000000000000000000 ) ) ;
#22750 = CARTESIAN_POINT ( 'NONE',  ( 212.1666685067961566, 117.1838024370489109, 89.67890646288726941 ) ) ;
#22751 = ORIENTED_EDGE ( 'NONE', *, *, #49528, .T. ) ;
#22752 = DIRECTION ( 'NONE',  ( 1.000000000000000000, 0.000000000000000000, 0.000000000000000000 ) ) ;
#22753 = FILL_AREA_STYLE ('',( #64976 ) ) ;
#22754 = CARTESIAN_POINT ( 'NONE',  ( -13.92109095214679648, 8.375243258322930373, 6.394640106076189490 ) ) ;
#22755 = CARTESIAN_POINT ( 'NONE',  ( 284.8387163486434588, -21.96381563589838493, -1.302408292197359208 ) ) ;
#22756 = DIRECTION ( 'NONE',  ( 0.000000000000000000, 0.000000000000000000, -1.000000000000000000 ) ) ;
#22757 = B_SPLINE_CURVE_WITH_KNOTS ( 'NONE', 3,
 ( #61434, #40319, #7633, #45596, #19911, #56150, #62113, #41366, #8321, #24840, #29085, #35393, #67756, #56853, #67081, #23804, #18871, #51910, #50532, #13590, #29765, #45942, #19200, #3717, #8671, #45245, #30125, #55814, #41015, #51576, #62470, #62819, #7967, #14286, #29422, #35746, #50872, #9015, #25196, #14623, #2352, #2690, #10037, #31165, #21278 ),
 .UNSPECIFIED., .F., .F.,
 ( 4, 2, 2, 1, 2, 2, 2, 2, 2, 2, 2, 2, 2, 2, 2, 2, 2, 2, 2, 2, 2, 2, 4 ),
 ( 0.02348395315094739880, 0.02495010856601295388, 0.02568318627354573142, 0.02641626398107850549, 0.02714934168861128302, 0.02788241939614406056, 0.02934857481120962605, 0.03008165251874241747, 0.03081473022627520542, 0.03228088564134076743, 0.03301396334887356232, 0.03374704105640635721, 0.03521319647147194004, 0.03667935188653752288, 0.03741242959407032470, 0.03814550730160312653, 0.03961166271666873018, 0.04107781813173433383, 0.04254397354679993748, 0.04327705125433273931, 0.04401012896186554113, 0.04547628437693114478, 0.04694243979199674843 ),
 .UNSPECIFIED. ) ;
#22758 = ORIENTED_EDGE ( 'NONE', *, *, #30250, .T. ) ;
#22759 = AXIS2_PLACEMENT_3D ( 'NONE', #50640, #7037, #61549 ) ;
#22760 = DIRECTION ( 'NONE',  ( 0.000000000000000000, 0.000000000000000000, 1.000000000000000000 ) ) ;
#22761 = CARTESIAN_POINT ( 'NONE',  ( -189.4223925288096666, 107.3427006758676470, -13.54568499105593382 ) ) ;
#22762 = CARTESIAN_POINT ( 'NONE',  ( -133.3926783185151521, 51.63401075114365568, 11.57669413790383572 ) ) ;
#22763 = CARTESIAN_POINT ( 'NONE',  ( -171.4943428135322847, 86.82484920477509149, -34.84193120942898503 ) ) ;
#22764 = CARTESIAN_POINT ( 'NONE',  ( -128.7724923851857000, 49.63576597317771189, -35.48433415201512275 ) ) ;
#22765 = ORIENTED_EDGE ( 'NONE', *, *, #24864, .T. ) ;
#22766 = CARTESIAN_POINT ( 'NONE',  ( 144.4165763529819344, 225.8585178651493663, 108.9999999999999858 ) ) ;
#22767 = AXIS2_PLACEMENT_3D ( 'NONE', #11198, #45660, #33381 ) ;
#22768 = CARTESIAN_POINT ( 'NONE',  ( -26.69131247781221106, -59.26697088777007849, 40.00000000000003553 ) ) ;
#22769 = LINE ( 'NONE', #18541, #69534 ) ;
#22770 = CARTESIAN_POINT ( 'NONE',  ( -0.5783162822156577842, 7.534184941292929594, -67.81582771104294238 ) ) ;
#22771 = ADVANCED_FACE ( 'NONE', ( #5360 ), #10974, .F. ) ;
#22772 = VECTOR ( 'NONE', #1471, 1000.000000000000000 ) ;
#22773 = FACE_OUTER_BOUND ( 'NONE', #26487, .T. ) ;
#22774 = ORIENTED_EDGE ( 'NONE', *, *, #12386, .F. ) ;
#22775 = CARTESIAN_POINT ( 'NONE',  ( 157.8370895073805684, 59.21456076921543143, -89.81328548006499091 ) ) ;
#22776 = CARTESIAN_POINT ( 'NONE',  ( 200.8298320869470217, 101.1869877914233342, -50.26595701390404969 ) ) ;
#22777 = CARTESIAN_POINT ( 'NONE',  ( -94.83794676023109105, 30.26879337035745365, 39.08187224689461203 ) ) ;
#22778 = CONICAL_SURFACE ( 'NONE', #28400, 4.171999999999999709, 0.7853981633974472798 ) ;
#22779 = CARTESIAN_POINT ( 'NONE',  ( 21.25987915030396636, 6.737472588634930482, -48.15424469599262380 ) ) ;
#22781 = VERTEX_POINT ( 'NONE', #68682 ) ;
#22780 = CARTESIAN_POINT ( 'NONE',  ( 0.000000000000000000, 0.000000000000000000, 170.0000000000000000 ) ) ;
#22782 = EDGE_CURVE ( 'NONE', #13713, #62027, #42305, .T. ) ;
#22783 = CARTESIAN_POINT ( 'NONE',  ( 177.7886308167536242, 76.74396398590876345, 70.40547167736322365 ) ) ;
#22784 = EDGE_CURVE ( 'NONE', #62313, #3776, #61297, .T. ) ;
#22785 = VERTEX_POINT ( 'NONE', #38402 ) ;
#22787 = EDGE_LOOP ( 'NONE', ( #28842, #20828, #57321, #33604 ) ) ;
#22786 = ADVANCED_FACE ( 'NONE', ( #33497 ), #60903, .F. ) ;
#22788 = CARTESIAN_POINT ( 'NONE',  ( 181.0840389613909736, 80.03940679743416808, 29.30859410551139277 ) ) ;
#22789 = LINE ( 'NONE', #44593, #36093 ) ;
#22790 = EDGE_CURVE ( 'NONE', #29635, #64884, #44373, .T. ) ;
#22792 = ORIENTED_EDGE ( 'NONE', *, *, #28772, .F. ) ;
#22791 = CARTESIAN_POINT ( 'NONE',  ( -14.93280618462407006, 8.469244267267917792, -67.35526017316270497 ) ) ;
#22793 = CARTESIAN_POINT ( 'NONE',  ( 160.9241720448059709, 60.38677655937337363, 43.58305608898694317 ) ) ;
#22794 = FACE_OUTER_BOUND ( 'NONE', #15678, .T. ) ;
#22795 = EDGE_CURVE ( 'NONE', #34219, #60980, #1126, .T. ) ;
#22796 = CARTESIAN_POINT ( 'NONE',  ( -452.6627218934914367, 399.9999999999998863, -111.4497041420118251 ) ) ;
#22797 = ORIENTED_EDGE ( 'NONE', *, *, #55831, .T. ) ;
#22798 = CARTESIAN_POINT ( 'NONE',  ( 10.06749493632391967, 74.32123213259514216, 0.000000000000000000 ) ) ;
#22799 = CARTESIAN_POINT ( 'NONE',  ( -29.87147652227456263, 68.79592317125366208, 73.58025477438755502 ) ) ;
#22801 = CARTESIAN_POINT ( 'NONE',  ( 111.1829448509513014, 30.43012797723691065, 44.56673546540911701 ) ) ;
#22800 = PRESENTATION_LAYER_ASSIGNMENT (  '', '', ( #46399 ) ) ;
#22802 = DIRECTION ( 'NONE',  ( -1.000000000000000000, 0.000000000000000000, 0.000000000000000000 ) ) ;
#22803 = CARTESIAN_POINT ( 'NONE',  ( 20.36233635256088093, 7.697399815318435756, 58.39548332934419506 ) ) ;
#22804 = VERTEX_POINT ( 'NONE', #33138 ) ;
#22805 = ORIENTED_EDGE ( 'NONE', *, *, #43805, .T. ) ;
#22806 = VERTEX_POINT ( 'NONE', #54211 ) ;
#22808 = EDGE_CURVE ( 'NONE', #32020, #6977, #60558, .T. ) ;
#22807 = CARTESIAN_POINT ( 'NONE',  ( 208.9381799476942660, 112.3426042533246658, -91.31812090025519524 ) ) ;
#22809 = LINE ( 'NONE', #27730, #52231 ) ;
#22810 = DIRECTION ( 'NONE',  ( -1.000000000000000000, 0.000000000000000000, 0.000000000000000000 ) ) ;
#22811 = AXIS2_PLACEMENT_3D ( 'NONE', #17444, #44535, #65293 ) ;
#22812 = CARTESIAN_POINT ( 'NONE',  ( -33.13098007862451055, 9.875138601866705557, -35.50648902819412456 ) ) ;
#22813 = CARTESIAN_POINT ( 'NONE',  ( -102.3225989298749141, 32.80186750033362841, 84.19102271607455634 ) ) ;
#22814 = EDGE_CURVE ( 'NONE', #1146, #68932, #40886, .T. ) ;
#22815 = DIRECTION ( 'NONE',  ( 0.000000000000000000, 0.000000000000000000, -1.000000000000000000 ) ) ;
#22816 = CARTESIAN_POINT ( 'NONE',  ( 24.33197424463712011, -22.91807472895442999, 6.893343212288945310 ) ) ;
#22817 = CARTESIAN_POINT ( 'NONE',  ( -61.97459043553174496, 17.69799435201358051, 94.41227228605326616 ) ) ;
#22819 = CARTESIAN_POINT ( 'NONE',  ( 81.76092782665033099, 17.81692437267514251, 69.76706349355957570 ) ) ;
#22818 = VECTOR ( 'NONE', #9794, 1000.000000000000000 ) ;
#22820 = ORIENTED_EDGE ( 'NONE', *, *, #67276, .F. ) ;
#22821 = CARTESIAN_POINT ( 'NONE',  ( 34.84173759613681653, 7.859847277726516701, 43.38827435105228147 ) ) ;
#22822 = VECTOR ( 'NONE', #22670, 1000.000000000000114 ) ;
#22823 = DIRECTION ( 'NONE',  ( -0.000000000000000000, 1.000000000000000000, -0.000000000000000000 ) ) ;
#22824 = ORIENTED_EDGE ( 'NONE', *, *, #59299, .T. ) ;
#22825 = CARTESIAN_POINT ( 'NONE',  ( 63.69186821587121017, 39.51023455020778385, 41.38025477438755928 ) ) ;
#22826 = CARTESIAN_POINT ( 'NONE',  ( 0.000000000000000000, 0.000000000000000000, 0.000000000000000000 ) ) ;
#22827 = CARTESIAN_POINT ( 'NONE',  ( -71.96390573417174608, 19.88067451234327265, 14.47695953071579922 ) ) ;
#22828 = CARTESIAN_POINT ( 'NONE',  ( -125.8938041572051389, 47.69968343338778993, 57.46449846362076386 ) ) ;
#22829 = CARTESIAN_POINT ( 'NONE',  ( -51.13073217147957905, 13.66490163179656925, 17.37025274476010495 ) ) ;
#22830 = VECTOR ( 'NONE', #6560, 1000.000000000000000 ) ;
#22831 = CARTESIAN_POINT ( 'NONE',  ( 151.3309484205704791, 53.03078371058069962, -39.30893049917887794 ) ) ;
#22832 = DIRECTION ( 'NONE',  ( -0.000000000000000000, -0.000000000000000000, -1.000000000000000000 ) ) ;
#22833 = ORIENTED_EDGE ( 'NONE', *, *, #28376, .T. ) ;
#22834 = CARTESIAN_POINT ( 'NONE',  ( 141.9165763529819344, 242.0000000000000000, 108.9999999999999858 ) ) ;
#22835 = ORIENTED_EDGE ( 'NONE', *, *, #35041, .F. ) ;
#22836 = CARTESIAN_POINT ( 'NONE',  ( -42.36049017605873956, -61.90437280228297112, 170.0000000000000000 ) ) ;
#22837 = LINE ( 'NONE', #7367, #62120 ) ;
#22838 = ORIENTED_EDGE ( 'NONE', *, *, #791, .T. ) ;
#22839 = CARTESIAN_POINT ( 'NONE',  ( 122.2516123306975402, 190.0000000000000000, -91.28179539054376335 ) ) ;
#22840 = CARTESIAN_POINT ( 'NONE',  ( 154.0515132159917471, 56.29926936869308918, -77.16036314277725694 ) ) ;
#22841 = FACE_OUTER_BOUND ( 'NONE', #38364, .T. ) ;
#22842 = CARTESIAN_POINT ( 'NONE',  ( -25.50312845906834269, 8.692070753302665764, 59.97022089822687008 ) ) ;
#22843 = ORIENTED_EDGE ( 'NONE', *, *, #52571, .T. ) ;
#22844 = ORIENTED_EDGE ( 'NONE', *, *, #21740, .T. ) ;
#22845 = CARTESIAN_POINT ( 'NONE',  ( -435.1627218934888788, 400.0000000000064801, -128.9497041420092387 ) ) ;
#22846 = ORIENTED_EDGE ( 'NONE', *, *, #54150, .T. ) ;
#22847 = CARTESIAN_POINT ( 'NONE',  ( 33.99754248246522792, 18.00000000000002842, 401.6295345748407613 ) ) ;
#22848 = CARTESIAN_POINT ( 'NONE',  ( 183.3913492984167704, 80.96922346472078402, 2.824542694585014502 ) ) ;
#22849 = CARTESIAN_POINT ( 'NONE',  ( -0.3252226420479318314, 7.525368746738508641, 63.97339285451934643 ) ) ;
#22850 = CARTESIAN_POINT ( 'NONE',  ( -25.13974312463025029, 9.657576844361820179, -92.43015382880602715 ) ) ;
#22851 = EDGE_LOOP ( 'NONE', ( #53701, #37494, #52398, #6694 ) ) ;
#22852 = EDGE_CURVE ( 'NONE', #2593, #15739, #39742, .T. ) ;
#22853 = AXIS2_PLACEMENT_3D ( 'NONE', #64535, #5446, #11062 ) ;
#22854 = CARTESIAN_POINT ( 'NONE',  ( -118.7011677090247304, 41.93687969120207981, -71.39957740465628433 ) ) ;
#22855 = ORIENTED_EDGE ( 'NONE', *, *, #7337, .T. ) ;
#22856 = VERTEX_POINT ( 'NONE', #17294 ) ;
#22857 = CARTESIAN_POINT ( 'NONE',  ( -84.49322488516129681, 0.000000000000000000, 43.58025477438756212 ) ) ;
#22858 = DIRECTION ( 'NONE',  ( 1.000000000000000000, 0.000000000000000000, 0.000000000000000000 ) ) ;
#22859 = AXIS2_PLACEMENT_3D ( 'NONE', #55169, #65038, #23183 ) ;
#22860 = CARTESIAN_POINT ( 'NONE',  ( -172.7116702014379257, 86.67317892691252723, -7.867406574286299303 ) ) ;
#22861 = CARTESIAN_POINT ( 'NONE',  ( -130.2340355668706309, 50.64168009053632602, -89.97067613245286566 ) ) ;
#22862 = DIRECTION ( 'NONE',  ( -0.7071067811865474617, 0.000000000000000000, 0.7071067811865474617 ) ) ;
#22863 = AXIS2_PLACEMENT_3D ( 'NONE', #60797, #7701, #55171 ) ;
#22864 = ORIENTED_EDGE ( 'NONE', *, *, #2884, .T. ) ;
#22865 = AXIS2_PLACEMENT_3D ( 'NONE', #54552, #757, #43649 ) ;
#22866 = ADVANCED_FACE ( 'NONE', ( #18003 ), #12375, .F. ) ;
#22867 = CARTESIAN_POINT ( 'NONE',  ( 79.52861599156696570, 17.11914630560288941, 7.901751469972297492 ) ) ;
#22868 = VERTEX_POINT ( 'NONE', #8493 ) ;
#22869 = VECTOR ( 'NONE', #41629, 999.9999999999998863 ) ;
#22870 = CARTESIAN_POINT ( 'NONE',  ( 109.9975424824652777, 296.0000000000000000, 418.0000000000000000 ) ) ;
#22871 = VERTEX_POINT ( 'NONE', #8843 ) ;
#22872 = CYLINDRICAL_SURFACE ( 'NONE', #58908, 10.00000000000000178 ) ;
#22873 = AXIS2_PLACEMENT_3D ( 'NONE', #33776, #55926, #34126 ) ;
#22874 = EDGE_CURVE ( 'NONE', #29587, #37010, #56322, .T. ) ;
#22875 = EDGE_CURVE ( 'NONE', #56265, #7572, #58852, .T. ) ;
#22876 = ORIENTED_EDGE ( 'NONE', *, *, #7740, .T. ) ;
#22877 = CARTESIAN_POINT ( 'NONE',  ( -143.8794621588508846, 59.54894433207191895, -74.12090710118032177 ) ) ;
#22878 = DIRECTION ( 'NONE',  ( -1.000000000000000000, 0.000000000000000000, 0.000000000000000000 ) ) ;
#22879 = EDGE_CURVE ( 'NONE', #65265, #24702, #25371, .T. ) ;
#22880 = LINE ( 'NONE', #43623, #2491 ) ;
#22881 = ORIENTED_EDGE ( 'NONE', *, *, #67167, .F. ) ;
#22882 = CARTESIAN_POINT ( 'NONE',  ( 0.4964154566687637438, -4.996589667937442414, -7.345652830558661250 ) ) ;
#22883 = CARTESIAN_POINT ( 'NONE',  ( 58.17717674717528809, 12.63051673829130550, 85.26196710955888136 ) ) ;
#22884 = CARTESIAN_POINT ( 'NONE',  ( 34.45972925205164472, 8.830088223935229408, 31.75137734477696938 ) ) ;
#22885 = CARTESIAN_POINT ( 'NONE',  ( -180.2243452982808378, 96.99029284948632323, -39.78723934564764875 ) ) ;
#22886 = CARTESIAN_POINT ( 'NONE',  ( -128.7650348665116837, 48.41336321950709731, -8.636724289455223413 ) ) ;
#22887 = CARTESIAN_POINT ( 'NONE',  ( 32.12337157895397866, 8.585320123189577046, -95.00000000000133582 ) ) ;
#22888 = CARTESIAN_POINT ( 'NONE',  ( 126.3737790127712515, 37.08609730334947585, -69.79690750847547065 ) ) ;
#22889 = ORIENTED_EDGE ( 'NONE', *, *, #25373, .T. ) ;
#22890 = DIRECTION ( 'NONE',  ( -0.000000000000000000, 1.000000000000000000, -0.000000000000000000 ) ) ;
#22891 = CARTESIAN_POINT ( 'NONE',  ( -144.9417090887490360, 61.69631066549397502, -75.11214843033646105 ) ) ;
#22892 = VERTEX_POINT ( 'NONE', #19730 ) ;
#22893 = CARTESIAN_POINT ( 'NONE',  ( -154.0833774771448930, 69.51012195447349029, -36.35145225699776006 ) ) ;
#22894 = CARTESIAN_POINT ( 'NONE',  ( -0.5751131641471395328, 6.527254166626919485, -67.82773600439074357 ) ) ;
#22895 = CARTESIAN_POINT ( 'NONE',  ( -173.5422248620771484, 89.11126078969411424, 72.66624519710472896 ) ) ;
#22896 = CARTESIAN_POINT ( 'NONE',  ( -142.9843132609582312, 60.12226089556225617, -11.75793129031485051 ) ) ;
#22897 = CYLINDRICAL_SURFACE ( 'NONE', #53627, 7.500000000000020428 ) ;
#22898 = CARTESIAN_POINT ( 'NONE',  ( -55.05276343752910151, -170.0000000000000000, -15.87177340799618364 ) ) ;
#22899 = CARTESIAN_POINT ( 'NONE',  ( -45.00000000000002132, -20.00000000000000355, 2.000000000000015543 ) ) ;
#22900 = EDGE_CURVE ( 'NONE', #14951, #61903, #35568, .T. ) ;
#22901 = CARTESIAN_POINT ( 'NONE',  ( 0.000000000000000000, 0.000000000000000000, 0.000000000000000000 ) ) ;
#22902 = DIRECTION ( 'NONE',  ( -1.000000000000000000, 0.000000000000000000, 0.000000000000000000 ) ) ;
#22903 = CARTESIAN_POINT ( 'NONE',  ( 33.40240440333036531, -1.250000000000021982, 6.893343212288935540 ) ) ;
#22904 = CARTESIAN_POINT ( 'NONE',  ( 117.3110050642447817, 32.29133253383015756, 7.707881950449412933 ) ) ;
#22905 = CARTESIAN_POINT ( 'NONE',  ( -48.72990440218273989, 14.11167693102101950, -92.36568283827145365 ) ) ;
#22906 = ORIENTED_EDGE ( 'NONE', *, *, #30192, .F. ) ;
#22907 = AXIS2_PLACEMENT_3D ( 'NONE', #33174, #60245, #45104 ) ;
#22908 = CARTESIAN_POINT ( 'NONE',  ( -33.36965723649377935, 10.93726715887723877, 3.620524580207087340 ) ) ;
#22909 = ORIENTED_EDGE ( 'NONE', *, *, #12539, .F. ) ;
#22910 = CARTESIAN_POINT ( 'NONE',  ( -443.6229740799759043, 394.9118408295729523, 93.31364146883153410 ) ) ;
#22911 = CARTESIAN_POINT ( 'NONE',  ( 79.33384730094455506, 18.11203072455035823, -71.92377449950194546 ) ) ;
#22912 = AXIS2_PLACEMENT_3D ( 'NONE', #45933, #19189, #17821 ) ;
#22913 = FACE_BOUND ( 'NONE', #55951, .T. ) ;
#22914 = LINE ( 'NONE', #33819, #40132 ) ;
#22915 = CARTESIAN_POINT ( 'NONE',  ( -24.95010104166214759, 9.631487977190600347, -39.04838185491376379 ) ) ;
#22916 = PLANE ( 'NONE',  #6344 ) ;
#22917 = VECTOR ( 'NONE', #37027, 1000.000000000000000 ) ;
#22918 = CARTESIAN_POINT ( 'NONE',  ( -173.1211646369891071, 87.12891641440857882, 57.66624519710472185 ) ) ;
#22919 = DIRECTION ( 'NONE',  ( -4.852411958229163333E-18, -1.576644219464802818E-18, -1.000000000000000000 ) ) ;
#22920 = ORIENTED_EDGE ( 'NONE', *, *, #34778, .F. ) ;
#22921 = VECTOR ( 'NONE', #58364, 1000.000000000000000 ) ;
#22922 = EDGE_LOOP ( 'NONE', ( #36265, #6678, #49644, #23341 ) ) ;
#22923 = B_SPLINE_CURVE_WITH_KNOTS ( 'NONE', 3,
 ( #63963, #53049, #37575, #20711, #26683, #48114, #26341, #15777, #21392, #59023, #47777, #58332, #42838, #52706, #21066, #10150, #10839, #42512, #32311, #53738, #37223, #58674, #5560, #58003, #9822, #31280, #20584, #4081, #3386, #31168, #68108, #46634, #24843, #25546, #42046, #40663, #62822, #30461, #30128, #46282, #67759, #52259, #46981 ),
 .UNSPECIFIED., .F., .F.,
 ( 4, 2, 2, 2, 2, 2, 2, 2, 2, 2, 2, 2, 1, 2, 2, 2, 2, 2, 2, 2, 2, 4 ),
 ( 0.02371951416048009159, 0.02520633211177537858, 0.02594974108742300126, 0.02669315006307062393, 0.02817996801436589011, 0.02966678596566115281, 0.03041019494130878589, 0.03115360391695641898, 0.03264042186825171638, 0.03412723981954701724, 0.03561405777084231117, 0.03635746674648995813, 0.03710087572213760509, 0.03784428469778525900, 0.03858769367343290596, 0.04007451162472822070, 0.04156132957602352851, 0.04304814752731883631, 0.04379155650296651103, 0.04453496547861417187, 0.04602178342990950743, 0.04750860138120484299 ),
 .UNSPECIFIED. ) ;
#22924 = VECTOR ( 'NONE', #38082, 1000.000000000000000 ) ;
#22925 = CYLINDRICAL_SURFACE ( 'NONE', #35422, 5.000000000000004441 ) ;
#22926 = CARTESIAN_POINT ( 'NONE',  ( 175.8963338753314360, 73.51705463274396379, 69.07525203059798002 ) ) ;
#22927 = DIRECTION ( 'NONE',  ( 0.000000000000000000, 0.000000000000000000, -1.000000000000000000 ) ) ;
#22928 = LINE ( 'NONE', #39121, #4639 ) ;
#22929 = AXIS2_PLACEMENT_3D ( 'NONE', #45631, #46304, #34397 ) ;
#22930 = CARTESIAN_POINT ( 'NONE',  ( -171.0950923142953854, 86.38958441093222973, -22.60122060940205202 ) ) ;
#22931 = VECTOR ( 'NONE', #2179, 1000.000000000000000 ) ;
#22932 = CARTESIAN_POINT ( 'NONE',  ( 8.000000000000007105, 249.8719672152120381, 94.99999999999866418 ) ) ;
#22933 = VERTEX_POINT ( 'NONE', #40489 ) ;
#22934 = CARTESIAN_POINT ( 'NONE',  ( 89.65730223173018487, 21.54473673261222899, 3.501741773472330621 ) ) ;
#22935 = DIRECTION ( 'NONE',  ( 0.3962817440048566620, 0.9137562205704280460, -0.08950055160341972849 ) ) ;
#22936 = FACE_OUTER_BOUND ( 'NONE', #60123, .T. ) ;
#22937 = CARTESIAN_POINT ( 'NONE',  ( -82.71271320792514814, 24.98855420139966199, -89.97510010486354304 ) ) ;
#22938 = DIRECTION ( 'NONE',  ( 1.000000000000000000, 1.387778780781445922E-16, 0.000000000000000000 ) ) ;
#22939 = CARTESIAN_POINT ( 'NONE',  ( 210.6741002223296846, 114.9147155784838503, -12.44257081975957746 ) ) ;
#22940 = FACE_BOUND ( 'NONE', #46141, .T. ) ;
#22941 = CARTESIAN_POINT ( 'NONE',  ( -59.56523643198717366, 15.93788386494078857, -36.72066679286387370 ) ) ;
#22942 = ADVANCED_FACE ( 'NONE', ( #2519 ), #46452, .F. ) ;
#22943 = EDGE_CURVE ( 'NONE', #59656, #46924, #3904, .T. ) ;
#22944 = ORIENTED_EDGE ( 'NONE', *, *, #35331, .F. ) ;
#22945 = LINE ( 'NONE', #54940, #15571 ) ;
#22946 = CARTESIAN_POINT ( 'NONE',  ( -55.05276343752909440, 14.68156374112637863, -62.06087458892354647 ) ) ;
#22947 = EDGE_CURVE ( 'NONE', #47361, #10179, #24675, .T. ) ;
#22948 = CARTESIAN_POINT ( 'NONE',  ( -7.825402957745087207, -170.0000000000000000, -89.10717191287116634 ) ) ;
#22949 = DIRECTION ( 'NONE',  ( -0.5508969814520944253, -0.8345732537213078617, 0.000000000000000000 ) ) ;
#22950 = CARTESIAN_POINT ( 'NONE',  ( 204.6977192012829789, 108.0580384837234931, 71.05227132923315025 ) ) ;
#22951 = DIRECTION ( 'NONE',  ( 1.000000000000000000, 0.000000000000000000, 0.000000000000000000 ) ) ;
#22952 = VERTEX_POINT ( 'NONE', #7798 ) ;
#22953 = CARTESIAN_POINT ( 'NONE',  ( 63.01563776193091826, 12.67277567978500308, 2.968410348757589023 ) ) ;
#22954 = DIRECTION ( 'NONE',  ( 0.000000000000000000, 0.000000000000000000, 1.000000000000000000 ) ) ;
#22955 = ORIENTED_EDGE ( 'NONE', *, *, #20549, .T. ) ;
#22956 = ORIENTED_EDGE ( 'NONE', *, *, #11464, .T. ) ;
#22957 = CIRCLE ( 'NONE', #51032, 5.000000000000000000 ) ;
#22958 = CARTESIAN_POINT ( 'NONE',  ( 0.06809871960542623892, -7.710219529346608702, 2.645508037661882916 ) ) ;
#22959 = CARTESIAN_POINT ( 'NONE',  ( -62.55320287144887459, 17.87319849854531384, -15.63420304729892152 ) ) ;
#22960 = CARTESIAN_POINT ( 'NONE',  ( 109.3047266816501377, 28.44977739115299187, 29.65533130390193151 ) ) ;
#22961 = EDGE_CURVE ( 'NONE', #20867, #26715, #30293, .T. ) ;
#22962 = ORIENTED_EDGE ( 'NONE', *, *, #40789, .T. ) ;
#22963 = EDGE_CURVE ( 'NONE', #25022, #49715, #45777, .T. ) ;
#22964 = AXIS2_PLACEMENT_3D ( 'NONE', #60027, #66039, #32956 ) ;
#22965 = ORIENTED_EDGE ( 'NONE', *, *, #7165, .T. ) ;
#22966 = CARTESIAN_POINT ( 'NONE',  ( -15.15117926080556465, 7.479311051197340632, -95.00000000000133582 ) ) ;
#22967 = CARTESIAN_POINT ( 'NONE',  ( 163.7403496014744633, 64.00600007368879574, 32.78579552523091678 ) ) ;
#22968 = CARTESIAN_POINT ( 'NONE',  ( 31.11269837220812562, 36.11269837220800838, 85.00100000000000477 ) ) ;
#22969 = CARTESIAN_POINT ( 'NONE',  ( 69.72564955710446100, 15.37006465677306721, 13.82808010939183596 ) ) ;
#22970 = CONICAL_SURFACE ( 'NONE', #31955, 74.95140232871122521, 0.8777644062502172329 ) ;
#22971 = CARTESIAN_POINT ( 'NONE',  ( 92.53566308513170213, 21.52138666710685300, 41.86074465914231979 ) ) ;
#22972 = VECTOR ( 'NONE', #21520, 1000.000000000000000 ) ;
#22973 = AXIS2_PLACEMENT_3D ( 'NONE', #55304, #21905, #43352 ) ;
#22974 = CARTESIAN_POINT ( 'NONE',  ( 108.3753929817421664, 29.13179266688724312, -9.298753174311741532 ) ) ;
#22975 = CARTESIAN_POINT ( 'NONE',  ( -49.12372073857198274, 14.20664392157176081, 6.353358384741189191 ) ) ;
#22976 = VECTOR ( 'NONE', #20609, 1000.000000000000000 ) ;
#22977 = CARTESIAN_POINT ( 'NONE',  ( -126.7944042662569046, 48.29830493043728978, -23.02871842506080213 ) ) ;
#22978 = DIRECTION ( 'NONE',  ( -0.000000000000000000, -0.000000000000000000, -1.000000000000000000 ) ) ;
#22979 = DIRECTION ( 'NONE',  ( -1.000000000000000000, 0.000000000000000000, -0.000000000000000000 ) ) ;
#22980 = CARTESIAN_POINT ( 'NONE',  ( 86.98834118549886796, 19.54364583620759532, 83.40280743883631942 ) ) ;
#22982 = ORIENTED_EDGE ( 'NONE', *, *, #59019, .F. ) ;
#22981 = DIRECTION ( 'NONE',  ( 0.000000000000000000, 1.000000000000000000, -0.000000000000000000 ) ) ;
#22983 = VERTEX_POINT ( 'NONE', #62652 ) ;
#22984 = ORIENTED_EDGE ( 'NONE', *, *, #43163, .T. ) ;
#22985 = CARTESIAN_POINT ( 'NONE',  ( 157.4703587214989398, -170.0000000000000000, 44.40946747225338953 ) ) ;
#22986 = CARTESIAN_POINT ( 'NONE',  ( -165.6851864275418507, 80.65423768630888901, 91.01486207682364693 ) ) ;
#22987 = CARTESIAN_POINT ( 'NONE',  ( -47.60396279792517760, 12.80997843568595052, -16.87800407465863373 ) ) ;
#22988 = CARTESIAN_POINT ( 'NONE',  ( 102.8066580714140628, 25.59117171227001819, -17.58622140034226788 ) ) ;
#22989 = CARTESIAN_POINT ( 'NONE',  ( -62.30163634902122993, 17.79682011226254446, -44.70441580692872208 ) ) ;
#22990 = LINE ( 'NONE', #44434, #10757 ) ;
#22991 = DIRECTION ( 'NONE',  ( -1.000000000000000000, -1.110223024625118675E-14, 1.110223024625118675E-14 ) ) ;
#22992 = CARTESIAN_POINT ( 'NONE',  ( -15.07200981767290848, 7.471751903425211339, 39.56416694737108486 ) ) ;
#22993 = ORIENTED_EDGE ( 'NONE', *, *, #35296, .F. ) ;
#22994 = CARTESIAN_POINT ( 'NONE',  ( -65.00200000000002376, 1.249999999999979350, 170.0000000000000000 ) ) ;
#22995 = VERTEX_POINT ( 'NONE', #62296 ) ;
#22996 = ORIENTED_EDGE ( 'NONE', *, *, #9693, .T. ) ;
#22997 = CARTESIAN_POINT ( 'NONE',  ( -142.6736406357357794, -170.0000000000000000, 94.99999999999866418 ) ) ;
#22998 = CARTESIAN_POINT ( 'NONE',  ( -58.35358059297030309, 16.63726411742650413, -89.66742083260719198 ) ) ;
#22999 = CARTESIAN_POINT ( 'NONE',  ( -165.7140086129056442, 80.68381997492572566, 37.10624841604320068 ) ) ;
#23000 = CARTESIAN_POINT ( 'NONE',  ( 112.5612011511790342, 31.08353758940340228, -23.72632233143615466 ) ) ;
#23001 = CARTESIAN_POINT ( 'NONE',  ( 437.3372781065085633, 395.0000000000001137, -123.9497041420121235 ) ) ;
#23002 = DIRECTION ( 'NONE',  ( -1.000000000000000000, 0.000000000000000000, 0.000000000000000000 ) ) ;
#23003 = CARTESIAN_POINT ( 'NONE',  ( 135.0005116824454205, 43.29964618809724897, -24.09459631371699118 ) ) ;
#23004 = ORIENTED_EDGE ( 'NONE', *, *, #32865, .T. ) ;
#23005 = ORIENTED_EDGE ( 'NONE', *, *, #17153, .F. ) ;
#23006 = VERTEX_POINT ( 'NONE', #51742 ) ;
#23007 = AXIS2_PLACEMENT_3D ( 'NONE', #68736, #63132, #8982 ) ;
#23008 = DIRECTION ( 'NONE',  ( 0.000000000000000000, -0.000000000000000000, 1.000000000000000000 ) ) ;
#23009 = CARTESIAN_POINT ( 'NONE',  ( -15.08468253268400083, 7.472949889606720575, 8.823174773458156039 ) ) ;
#23010 = FACE_OUTER_BOUND ( 'NONE', #60637, .T. ) ;
#23011 = CARTESIAN_POINT ( 'NONE',  ( 55.56474667084420815, 11.06706367715631778, -15.38353893648206849 ) ) ;
#23012 = VECTOR ( 'NONE', #43695, 1000.000000000000000 ) ;
#23013 = CARTESIAN_POINT ( 'NONE',  ( 70.34686579112810989, 18.11777090454213379, 41.38025477438755928 ) ) ;
#23014 = DIRECTION ( 'NONE',  ( 0.000000000000000000, -1.000000000000000000, 0.000000000000000000 ) ) ;
#23015 = VERTEX_POINT ( 'NONE', #50701 ) ;
#23016 = AXIS2_PLACEMENT_3D ( 'NONE', #38112, #68735, #59556 ) ;
#23017 = VECTOR ( 'NONE', #26982, 1000.000000000000000 ) ;
#23018 = CARTESIAN_POINT ( 'NONE',  ( -55.54036735998997898, 15.85474597822064702, -62.06087458892358200 ) ) ;
#23019 = CARTESIAN_POINT ( 'NONE',  ( 197.1979149960398274, 98.19687999751999996, -71.00583573180291808 ) ) ;
#23020 =( NAMED_UNIT ( * ) SI_UNIT ( $, .STERADIAN. ) SOLID_ANGLE_UNIT ( ) );
#23021 = CARTESIAN_POINT ( 'NONE',  ( -0.8863173716723027340, 7.545240407187534970, -40.04092009748728032 ) ) ;
#23022 = SURFACE_STYLE_FILL_AREA ( #867 ) ;
#23023 = CARTESIAN_POINT ( 'NONE',  ( -47.68562151781910785, -170.0000000000000000, -95.00000000000133582 ) ) ;
#23024 = LINE ( 'NONE', #23390, #45267 ) ;
#23025 = AXIS2_PLACEMENT_3D ( 'NONE', #33668, #55448, #6922 ) ;
#23026 = FACE_BOUND ( 'NONE', #67774, .T. ) ;
#23027 = PLANE ( 'NONE',  #64681 ) ;
#23028 = AXIS2_PLACEMENT_3D ( 'NONE', #52625, #25911, #47338 ) ;
#23029 = EDGE_CURVE ( 'NONE', #7667, #26503, #45423, .T. ) ;
#23030 = CIRCLE ( 'NONE', #28656, 0.4000000000000001887 ) ;
#23031 = EDGE_CURVE ( 'NONE', #55030, #6514, #28543, .T. ) ;
#23032 = VERTEX_POINT ( 'NONE', #9180 ) ;
#23033 = B_SPLINE_CURVE_WITH_KNOTS ( 'NONE', 3,
 ( #20547, #52222, #47619, #68412, #32155, #69071 ),
 .UNSPECIFIED., .F., .F.,
 ( 4, 2, 4 ),
 ( 0.03218943375184182137, 0.06469838935233371280, 0.09720734495282559728 ),
 .UNSPECIFIED. ) ;
#23034 = CARTESIAN_POINT ( 'NONE',  ( -31.11269837220812207, -26.11269837220801193, 2.000000000000001776 ) ) ;
#23035 = EDGE_CURVE ( 'NONE', #61402, #16881, #35914, .T. ) ;
#23036 = CARTESIAN_POINT ( 'NONE',  ( -31.11269837220809364, -15.55634918610397754, 85.00100000000000477 ) ) ;
#23037 = DIRECTION ( 'NONE',  ( 0.000000000000000000, 0.000000000000000000, -1.000000000000000000 ) ) ;
#23038 = CARTESIAN_POINT ( 'NONE',  ( 46.70715146412976537, 9.472433765547007667, -71.68030912521341236 ) ) ;
#23039 = DIRECTION ( 'NONE',  ( -0.000000000000000000, -0.000000000000000000, -1.000000000000000000 ) ) ;
#23040 = ORIENTED_EDGE ( 'NONE', *, *, #21133, .F. ) ;
#23041 = ORIENTED_EDGE ( 'NONE', *, *, #5920, .F. ) ;
#23042 = CARTESIAN_POINT ( 'NONE',  ( -130.2299182487217024, 49.41538973246969846, -89.96770515742747421 ) ) ;
#23043 = CARTESIAN_POINT ( 'NONE',  ( 188.5747655895476100, 86.52284255640786625, 89.95077014674320992 ) ) ;
#23044 = ORIENTED_EDGE ( 'NONE', *, *, #18986, .T. ) ;
#23045 = ORIENTED_EDGE ( 'NONE', *, *, #17864, .T. ) ;
#23046 = CARTESIAN_POINT ( 'NONE',  ( 174.2469308602415197, 71.96142024047681218, -46.82003836444015121 ) ) ;
#23047 = DIRECTION ( 'NONE',  ( 0.000000000000000000, -1.000000000000000000, 0.000000000000000000 ) ) ;
#23048 = CARTESIAN_POINT ( 'NONE',  ( 0.000000000000000000, 0.000000000000000000, 40.00000000000003553 ) ) ;
#23049 = EDGE_CURVE ( 'NONE', #17967, #40644, #30637, .T. ) ;
#23050 = VERTEX_POINT ( 'NONE', #52085 ) ;
#23051 = DIRECTION ( 'NONE',  ( 0.000000000000000000, 0.000000000000000000, 1.000000000000000000 ) ) ;
#23052 = CARTESIAN_POINT ( 'NONE',  ( -177.5259994307673708, 92.16784265327251546, 5.389069799081259049 ) ) ;
#23053 = CARTESIAN_POINT ( 'NONE',  ( -77.71448999903257970, 21.96089801565736721, -35.16068627303630478 ) ) ;
#23054 = CARTESIAN_POINT ( 'NONE',  ( 80.01789329971975917, 17.27008742253428153, -93.44501639533700654 ) ) ;
#23055 = CARTESIAN_POINT ( 'NONE',  ( -37.98601804829807094, 14.28438006995821219, -38.01398195170192906 ) ) ;
#23056 = CARTESIAN_POINT ( 'NONE',  ( -190.0468231512976161, 108.2116162189845170, 35.02347016645559563 ) ) ;
#23057 = ORIENTED_EDGE ( 'NONE', *, *, #67437, .F. ) ;
#23058 = CARTESIAN_POINT ( 'NONE',  ( 74.01791526339567895, -12.16185512414844716, 170.0000000000000000 ) ) ;
#23059 = VECTOR ( 'NONE', #31223, 1000.000000000000000 ) ;
#23060 = CARTESIAN_POINT ( 'NONE',  ( -73.10086105983761229, 21.34631349770504372, 16.12499931341085002 ) ) ;
#23061 = CARTESIAN_POINT ( 'NONE',  ( 41.33692564073608366, 8.668977654195479943, -50.37004257708993293 ) ) ;
#23062 = FACE_OUTER_BOUND ( 'NONE', #62793, .T. ) ;
#23063 = CIRCLE ( 'NONE', #55594, 24.99999999999985434 ) ;
#23065 = ORIENTED_EDGE ( 'NONE', *, *, #39970, .F. ) ;
#23064 = CARTESIAN_POINT ( 'NONE',  ( -118.5237170689549941, 41.82886034450997670, 90.37931702170654091 ) ) ;
#23066 = CARTESIAN_POINT ( 'NONE',  ( 86.62931800182293784, 19.42108912189597092, -50.82156419891174437 ) ) ;
#23067 = ORIENTED_EDGE ( 'NONE', *, *, #28907, .T. ) ;
#23068 = CARTESIAN_POINT ( 'NONE',  ( -143.8794621588507994, 59.54894433207190474, 60.10184585113807287 ) ) ;
#23069 = CARTESIAN_POINT ( 'NONE',  ( 83.59652366361571296, 19.46709838196857945, 44.07574043631387184 ) ) ;
#23070 = LINE ( 'NONE', #2317, #47788 ) ;
#23071 =( GEOMETRIC_REPRESENTATION_CONTEXT ( 3 ) GLOBAL_UNCERTAINTY_ASSIGNED_CONTEXT ( ( #68356 ) ) GLOBAL_UNIT_ASSIGNED_CONTEXT ( ( #36345, #41619, #46543 ) ) REPRESENTATION_CONTEXT ( 'NONE', 'WORKASPACE' ) );
#23072 = B_SPLINE_CURVE_WITH_KNOTS ( 'NONE', 3,
 ( #29610, #45092, #2201, #61628, #23998, #13781, #18719, #61283 ),
 .UNSPECIFIED., .F., .F.,
 ( 4, 2, 2, 4 ),
 ( 0.004673709593152186939, 0.005837709341827668555, 0.007001709090503151038, 0.009329708587854118607 ),
 .UNSPECIFIED. ) ;
#23074 = DIRECTION ( 'NONE',  ( 0.000000000000000000, -1.000000000000000000, -0.000000000000000000 ) ) ;
#23073 = VECTOR ( 'NONE', #58513, 1000.000000000000000 ) ;
#23075 = CARTESIAN_POINT ( 'NONE',  ( 140.1999945597799524, 45.38880890490935371, -20.68848176573018094 ) ) ;
#23076 = CARTESIAN_POINT ( 'NONE',  ( 39.88975917505624835, 9.487965272711651465, 3.069283715499572907 ) ) ;
#23077 = CARTESIAN_POINT ( 'NONE',  ( 87.59061758233886508, 19.75077892934019985, -62.71238299196379984 ) ) ;
#23078 = VECTOR ( 'NONE', #48999, 1000.000000000000000 ) ;
#23079 = CARTESIAN_POINT ( 'NONE',  ( 209.9518228411288874, 172.0000000000000284, 31.43423095485942298 ) ) ;
#23080 = DIRECTION ( 'NONE',  ( 0.000000000000000000, 1.000000000000000000, 0.000000000000000000 ) ) ;
#23081 = ORIENTED_EDGE ( 'NONE', *, *, #46393, .F. ) ;
#23082 = VERTEX_POINT ( 'NONE', #46807 ) ;
#23083 = CARTESIAN_POINT ( 'NONE',  ( 43.14356474118746831, 8.925336319666905993, 30.89513714664620281 ) ) ;
#23084 = CARTESIAN_POINT ( 'NONE',  ( 197.2197025888161761, 96.62026035493815357, -17.64164879660345164 ) ) ;
#23085 = CARTESIAN_POINT ( 'NONE',  ( -31.11269837220809364, -10.55634918610397932, 0.000000000000000000 ) ) ;
#23086 = FACE_OUTER_BOUND ( 'NONE', #64231, .T. ) ;
#23087 = CARTESIAN_POINT ( 'NONE',  ( 209.6698611676811197, 115.2210955123518517, -38.19286268395692474 ) ) ;
#23088 = B_SPLINE_CURVE_WITH_KNOTS ( 'NONE', 3,
 ( #1793, #6704, #28150, #23249, #44694, #66173, #7419, #50321, #68236, #3511, #51364, #30597, #29546, #8804, #24638, #46072, #2824, #36218, #52049, #9489, #51015, #62251, #8452, #67543 ),
 .UNSPECIFIED., .F., .F.,
 ( 4, 2, 2, 2, 2, 2, 2, 2, 2, 2, 2, 4 ),
 ( 0.000000000000000000, 0.001774223329494980465, 0.002661334994242444893, 0.003548446658989908888, 0.004435558323737373750, 0.005322669988484837744, 0.007096893317979765733, 0.007984004982727195901, 0.008871116647474627803, 0.01064533997696948987, 0.01241956330646435194, 0.01419378663595921401 ),
 .UNSPECIFIED. ) ;
#23089 = EDGE_CURVE ( 'NONE', #61986, #32859, #61938, .T. ) ;
#23090 = CARTESIAN_POINT ( 'NONE',  ( -78.66644367742109978, 23.39876645725288284, -76.96000122218160300 ) ) ;
#23091 = CARTESIAN_POINT ( 'NONE',  ( -149.5074843970971301, -170.0000000000000000, 18.87627064943540134 ) ) ;
#23092 = CARTESIAN_POINT ( 'NONE',  ( -24.07146890348362689, 8.497559956800399661, -41.35130633274434331 ) ) ;
#23093 = CARTESIAN_POINT ( 'NONE',  ( 163.2886151008987952, 62.32020850087171482, -75.20809123641221561 ) ) ;
#23094 = ORIENTED_EDGE ( 'NONE', *, *, #17731, .F. ) ;
#23095 = LINE ( 'NONE', #34950, #25453 ) ;
#23096 = VERTEX_POINT ( 'NONE', #67252 ) ;
#23097 = DIRECTION ( 'NONE',  ( -0.000000000000000000, -0.000000000000000000, 1.000000000000000000 ) ) ;
#23098 = DIRECTION ( 'NONE',  ( -1.000000000000000000, 0.000000000000000000, 0.000000000000000000 ) ) ;
#23099 = DIRECTION ( 'NONE',  ( -0.2225209339563184452, 0.9749279121818226201, 0.000000000000000000 ) ) ;
#23100 = CARTESIAN_POINT ( 'NONE',  ( -51.84164840787130402, -39.21024726209533640, 40.00000000000003553 ) ) ;
#23101 = DIRECTION ( 'NONE',  ( 0.000000000000000000, 0.000000000000000000, 1.000000000000000000 ) ) ;
#23102 = CYLINDRICAL_SURFACE ( 'NONE', #17682, 20.00000000000000355 ) ;
#23103 = DIRECTION ( 'NONE',  ( 0.7071067811865543451, 7.105427357601001070E-15, 0.7071067811865408004 ) ) ;
#23104 = CARTESIAN_POINT ( 'NONE',  ( -439.4229916354185548, 388.0000000000064801, -133.9497041420121377 ) ) ;
#23105 = LINE ( 'NONE', #22401, #2345 ) ;
#23106 = ORIENTED_EDGE ( 'NONE', *, *, #68060, .T. ) ;
#23107 = CARTESIAN_POINT ( 'NONE',  ( 57.07246224906427301, 12.39953617563784860, 68.75870423085009975 ) ) ;
#23108 = CARTESIAN_POINT ( 'NONE',  ( -13.47517652744367567, 8.334971000693556675, 15.72779575785819972 ) ) ;
#23109 = EDGE_CURVE ( 'NONE', #37153, #41430, #41533, .T. ) ;
#23110 = CARTESIAN_POINT ( 'NONE',  ( 15.55634918610400241, -10.55634918610406281, 0.000000000000000000 ) ) ;
#23111 = DIRECTION ( 'NONE',  ( 1.000000000000000000, -3.344045254895050726E-17, 0.000000000000000000 ) ) ;
#23112 = EDGE_CURVE ( 'NONE', #3968, #40134, #34882, .T. ) ;
#23113 = CARTESIAN_POINT ( 'NONE',  ( 127.2358066117906787, 38.72257733469225371, -20.23951017382307782 ) ) ;
#23114 = VECTOR ( 'NONE', #65998, 1000.000000000000000 ) ;
#23115 = EDGE_LOOP ( 'NONE', ( #33693, #33735, #17520, #25529 ) ) ;
#23116 = AXIS2_PLACEMENT_3D ( 'NONE', #45137, #13824, #8904 ) ;
#23117 = APPLICATION_PROTOCOL_DEFINITION ( 'draft international standard', 'automotive_design', 1998, #2208 ) ;
#23118 = EDGE_CURVE ( 'NONE', #41002, #63860, #47597, .T. ) ;
#23119 = DIRECTION ( 'NONE',  ( -1.000000000000000000, 0.000000000000000000, 0.000000000000000000 ) ) ;
#23120 = CARTESIAN_POINT ( 'NONE',  ( -31.92572261726339633, 10.69135962481465008, -50.31719736520186359 ) ) ;
#23121 = DIRECTION ( 'NONE',  ( -0.000000000000000000, 1.000000000000000000, -0.000000000000000000 ) ) ;
#23122 = CARTESIAN_POINT ( 'NONE',  ( 447.3372781065086201, 0.000000000000000000, 113.5502958579881749 ) ) ;
#23123 = ORIENTED_EDGE ( 'NONE', *, *, #17460, .F. ) ;
#23125 = CARTESIAN_POINT ( 'NONE',  ( -119.1795380581000074, 42.22910606512925114, -45.76561242440763522 ) ) ;
#23124 = VECTOR ( 'NONE', #51323, 1000.000000000000114 ) ;
#23126 = CARTESIAN_POINT ( 'NONE',  ( -71.90777365577140756, 21.14201501538314076, 41.38025477438755928 ) ) ;
#23127 = CARTESIAN_POINT ( 'NONE',  ( -147.3641864666714980, 62.38213854487954535, -22.66905609602007132 ) ) ;
#23128 = AXIS2_PLACEMENT_3D ( 'NONE', #27817, #28518, #5999 ) ;
#23129 = LINE ( 'NONE', #62842, #27176 ) ;
#23130 = DIRECTION ( 'NONE',  ( -0.000000000000000000, -0.000000000000000000, -1.000000000000000000 ) ) ;
#23131 = EDGE_CURVE ( 'NONE', #13211, #58078, #30986, .T. ) ;
#23132 = ORIENTED_EDGE ( 'NONE', *, *, #50272, .T. ) ;
#23133 = CARTESIAN_POINT ( 'NONE',  ( -62.15063206372444427, 17.75106610013994768, 8.499825761613776010 ) ) ;
#23134 = CARTESIAN_POINT ( 'NONE',  ( 197.8572563162090887, 97.41072138832262794, -40.73584554935744251 ) ) ;
#23135 = CARTESIAN_POINT ( 'NONE',  ( -95.21085197937820510, 30.44372064875428663, 40.57601684981261059 ) ) ;
#23136 = EDGE_CURVE ( 'NONE', #43935, #61832, #66774, .T. ) ;
#23137 = ADVANCED_FACE ( 'NONE', ( #13138 ), #9467, .T. ) ;
#23138 = ADVANCED_FACE ( 'NONE', ( #48499 ), #48163, .F. ) ;
#23139 = CARTESIAN_POINT ( 'NONE',  ( 18.21423326326596737, 6.590134686181412960, -35.90535394282123605 ) ) ;
#23141 = ORIENTED_EDGE ( 'NONE', *, *, #38439, .T. ) ;
#23140 = FACE_OUTER_BOUND ( 'NONE', #20154, .T. ) ;
#23142 = CYLINDRICAL_SURFACE ( 'NONE', #23896, 65.36598343705435354 ) ;
#23143 = ORIENTED_EDGE ( 'NONE', *, *, #67750, .T. ) ;
#23144 = VERTEX_POINT ( 'NONE', #15829 ) ;
#23145 = CARTESIAN_POINT ( 'NONE',  ( -122.6739428120618953, 44.40980909172365898, -89.31540991285331188 ) ) ;
#23146 = CARTESIAN_POINT ( 'NONE',  ( 447.3372781065085064, 400.0000000000001137, -146.4497041420118535 ) ) ;
#23148 = ORIENTED_EDGE ( 'NONE', *, *, #18337, .T. ) ;
#23147 = CARTESIAN_POINT ( 'NONE',  ( 10.78925482157233340, 22.68765681156020264, 3.061616997868437868E-16 ) ) ;
#23149 = CARTESIAN_POINT ( 'NONE',  ( 15.78827728214693416, -170.0000000000000000, -77.36349468914950478 ) ) ;
#23150 = DIRECTION ( 'NONE',  ( 0.000000000000000000, -0.000000000000000000, 1.000000000000000000 ) ) ;
#23151 = LINE ( 'NONE', #22796, #48488 ) ;
#23152 = PRODUCT_DEFINITION_SHAPE ( 'NONE', 'NONE',  #69630 ) ;
#23153 = VERTEX_POINT ( 'NONE', #69292 ) ;
#23154 = CARTESIAN_POINT ( 'NONE',  ( -144.0702036543480631, 60.99138314440749298, -90.83095804928598227 ) ) ;
#23155 = AXIS2_PLACEMENT_3D ( 'NONE', #10253, #31715, #53147 ) ;
#23156 = CARTESIAN_POINT ( 'NONE',  ( -35.38560449531983920, 10.27249159032101389, -22.35498971822604375 ) ) ;
#23157 = CARTESIAN_POINT ( 'NONE',  ( -180.3161328724958139, 97.10341277064809162, 40.46042418554912956 ) ) ;
#23158 = CARTESIAN_POINT ( 'NONE',  ( -132.0738857626834601, 51.93126104279141941, 7.018657644745633029 ) ) ;
#23159 = CARTESIAN_POINT ( 'NONE',  ( 16.77104078056616387, 7.540619757007627655, 71.81062785426281891 ) ) ;
#23160 = EDGE_LOOP ( 'NONE', ( #5459, #42688 ) ) ;
#23161 = EDGE_LOOP ( 'NONE', ( #61212, #65227, #61787, #23598 ) ) ;
#23162 = VECTOR ( 'NONE', #65313, 1000.000000000000000 ) ;
#23163 = ORIENTED_EDGE ( 'NONE', *, *, #29612, .T. ) ;
#23164 = DIRECTION ( 'NONE',  ( -1.000000000000000000, 0.000000000000000000, 0.000000000000000000 ) ) ;
#23165 = CARTESIAN_POINT ( 'NONE',  ( -4.613603609465520172, 74.86839895266042788, 170.0000000000000000 ) ) ;
#23166 = VECTOR ( 'NONE', #47668, 1000.000000000000000 ) ;
#23167 = AXIS2_PLACEMENT_3D ( 'NONE', #56792, #49752, #2985 ) ;
#23168 = CARTESIAN_POINT ( 'NONE',  ( 2.699999999999990408, 0.000000000000000000, 0.000000000000000000 ) ) ;
#23169 = CARTESIAN_POINT ( 'NONE',  ( -35.17686701826947626, 10.23452050416468317, -36.29668785629766603 ) ) ;
#23170 = ADVANCED_FACE ( 'NONE', ( #62985 ), #22970, .T. ) ;
#23171 = CARTESIAN_POINT ( 'NONE',  ( -94.81181312526928195, 29.14610013485190265, 92.47439075634365224 ) ) ;
#23172 = PRODUCT_DEFINITION_FORMATION_WITH_SPECIFIED_SOURCE ( 'ANY', '', #19738, .NOT_KNOWN. ) ;
#23173 = LINE ( 'NONE', #44618, #22431 ) ;
#23174 = CARTESIAN_POINT ( 'NONE',  ( -126.3458714439410784, 46.79154809309477514, 57.46449846362074965 ) ) ;
#23175 = CARTESIAN_POINT ( 'NONE',  ( 141.9165763529819344, -52.00000000000000711, 108.9999999999999858 ) ) ;
#23176 = VECTOR ( 'NONE', #7767, 1000.000000000000000 ) ;
#23177 = VERTEX_POINT ( 'NONE', #42890 ) ;
#23178 = CARTESIAN_POINT ( 'NONE',  ( 85.67452303415197434, 19.09699411916384548, 71.51082955247741779 ) ) ;
#23179 = ORIENTED_EDGE ( 'NONE', *, *, #64852, .T. ) ;
#23180 = EDGE_CURVE ( 'NONE', #13968, #25239, #52432, .T. ) ;
#23182 = CIRCLE ( 'NONE', #40046, 8.000000000000000000 ) ;
#23181 = CARTESIAN_POINT ( 'NONE',  ( 32.09567473596477782, 7.571373529017937365, 39.12545751119512261 ) ) ;
#23183 = DIRECTION ( 'NONE',  ( 0.000000000000000000, 0.000000000000000000, 1.000000000000000000 ) ) ;
#23184 = LINE ( 'NONE', #61833, #1521 ) ;
#23185 = FACE_OUTER_BOUND ( 'NONE', #1546, .T. ) ;
#23186 = CARTESIAN_POINT ( 'NONE',  ( 20.79325243092002751, 13.87950479462545772, 0.000000000000000000 ) ) ;
#23187 = CARTESIAN_POINT ( 'NONE',  ( 61.91366885787729046, 28.42865614898999738, 3.061616997868437868E-16 ) ) ;
#23188 = CARTESIAN_POINT ( 'NONE',  ( -51.78153763344962357, 13.82841714689605617, 4.206538418488238840 ) ) ;
#23189 = FACE_OUTER_BOUND ( 'NONE', #34610, .T. ) ;
#23190 = CARTESIAN_POINT ( 'NONE',  ( 164.0105905242218398, 64.23277447906893656, -74.14879248810279933 ) ) ;
#23191 = VERTEX_POINT ( 'NONE', #59073 ) ;
#23192 = LINE ( 'NONE', #28456, #1680 ) ;
#23193 = CARTESIAN_POINT ( 'NONE',  ( -188.7743570271016722, 108.2592512368506306, 92.51026036494342009 ) ) ;
#23194 = ORIENTED_EDGE ( 'NONE', *, *, #5572, .T. ) ;
#23195 = CARTESIAN_POINT ( 'NONE',  ( 2.309976723937610554, -7.903938623646890704, -9.369346954796176519 ) ) ;
#23196 = CARTESIAN_POINT ( 'NONE',  ( 31.11269837220803325, -15.55634918610409656, 85.00100000000000477 ) ) ;
#23197 = LINE ( 'NONE', #19288, #20702 ) ;
#23198 = VERTEX_POINT ( 'NONE', #21121 ) ;
#23199 = EDGE_CURVE ( 'NONE', #17554, #41847, #20413, .T. ) ;
#23200 = CARTESIAN_POINT ( 'NONE',  ( -80.31691774066412393, 22.95709084517032750, 45.23817464378598885 ) ) ;
#23201 = LINE ( 'NONE', #67170, #7359 ) ;
#23202 = CARTESIAN_POINT ( 'NONE',  ( 43.35536254672140188, 9.973606330917817786, 31.03574407154524195 ) ) ;
#23203 = EDGE_CURVE ( 'NONE', #64405, #23417, #32362, .T. ) ;
#23204 = CARTESIAN_POINT ( 'NONE',  ( 136.9798231265810387, 43.34196232604179500, -50.35791885916582089 ) ) ;
#23205 = EDGE_CURVE ( 'NONE', #28877, #59754, #42563, .T. ) ;
#23206 = ORIENTED_EDGE ( 'NONE', *, *, #17460, .T. ) ;
#23207 = CARTESIAN_POINT ( 'NONE',  ( 644.1895565744039232, 939.3221711212311220, 596.5068267248707343 ) ) ;
#23208 = ORIENTED_EDGE ( 'NONE', *, *, #3187, .T. ) ;
#23209 = FACE_OUTER_BOUND ( 'NONE', #4271, .T. ) ;
#23210 = ORIENTED_EDGE ( 'NONE', *, *, #50303, .F. ) ;
#23211 = CARTESIAN_POINT ( 'NONE',  ( 32.09610685027467980, 8.582590950734818591, -17.98836414960963737 ) ) ;
#23212 = CARTESIAN_POINT ( 'NONE',  ( -30.63688115438417725, -13.36654903315597309, 6.893343212288941757 ) ) ;
#23213 = CARTESIAN_POINT ( 'NONE',  ( -1.298947065946362001, 6.553849421084473548, 94.99999999999866418 ) ) ;
#23214 = CARTESIAN_POINT ( 'NONE',  ( -7.336630171688594437, 7.867399454768211342, 56.96013162991088308 ) ) ;
#23215 = PRODUCT_DEFINITION_SHAPE ( 'NONE', 'NONE',  #16408 ) ;
#23216 = FACE_OUTER_BOUND ( 'NONE', #39194, .T. ) ;
#23217 = DIRECTION ( 'NONE',  ( 0.000000000000000000, 0.000000000000000000, -1.000000000000000000 ) ) ;
#23218 = AXIS2_PLACEMENT_3D ( 'NONE', #42782, #69175, #37512 ) ;
#23219 = EDGE_LOOP ( 'NONE', ( #21435, #35487, #1864, #44697 ) ) ;
#23220 = CARTESIAN_POINT ( 'NONE',  ( 60.82895951008426749, -30.68107831874540636, 3.061616997868437868E-16 ) ) ;
#23221 = ORIENTED_EDGE ( 'NONE', *, *, #54121, .F. ) ;
#23222 = CARTESIAN_POINT ( 'NONE',  ( 164.8407099662994995, 63.61629583487393802, -18.19528167887739656 ) ) ;
#23223 = CARTESIAN_POINT ( 'NONE',  ( 32.99392442438140449, 7.662387294680161887, 94.99999999999866418 ) ) ;
#23224 = VECTOR ( 'NONE', #44369, 1000.000000000000000 ) ;
#23225 = DIRECTION ( 'NONE',  ( 0.9362348706397417564, -0.3513748240813305279, 0.000000000000000000 ) ) ;
#23226 = CARTESIAN_POINT ( 'NONE',  ( 141.3707934840545022, 46.15056991286792965, -70.39752903070149159 ) ) ;
#23227 = DIRECTION ( 'NONE',  ( -0.000000000000000000, -0.000000000000000000, -1.000000000000000000 ) ) ;
#23228 = EDGE_CURVE ( 'NONE', #27330, #19842, #10948, .T. ) ;
#23229 = EDGE_CURVE ( 'NONE', #23453, #51654, #3050, .T. ) ;
#23230 = AXIS2_PLACEMENT_3D ( 'NONE', #58157, #59518, #53201 ) ;
#23231 = ORIENTED_EDGE ( 'NONE', *, *, #6578, .F. ) ;
#23232 = DIRECTION ( 'NONE',  ( -0.000000000000000000, -0.000000000000000000, -1.000000000000000000 ) ) ;
#23233 = EDGE_CURVE ( 'NONE', #34620, #23417, #22143, .T. ) ;
#23234 = ORIENTED_EDGE ( 'NONE', *, *, #48567, .F. ) ;
#23235 = CARTESIAN_POINT ( 'NONE',  ( 8.683531412707429453, 6.377173148747125708, 39.92982772978346162 ) ) ;
#23236 = VERTEX_POINT ( 'NONE', #64710 ) ;
#23237 = CIRCLE ( 'NONE', #25497, 25.12245591505646303 ) ;
#23238 = CARTESIAN_POINT ( 'NONE',  ( -62.56514071794335052, 16.82532503654672240, -69.55340720332647209 ) ) ;
#23239 = CARTESIAN_POINT ( 'NONE',  ( 126.8191975983342132, 37.33444841723056840, -94.58288091666166508 ) ) ;
#23240 = VERTEX_POINT ( 'NONE', #29425 ) ;
#23241 = LINE ( 'NONE', #38005, #1613 ) ;
#23242 = CARTESIAN_POINT ( 'NONE',  ( 89.87518614971253328, 20.55373388674512114, 3.589420107556450912 ) ) ;
#23243 = CARTESIAN_POINT ( 'NONE',  ( 0.000000000000000000, 0.000000000000000000, -10.00000000000000000 ) ) ;
#23244 = ORIENTED_EDGE ( 'NONE', *, *, #7255, .F. ) ;
#23245 = CARTESIAN_POINT ( 'NONE',  ( 0.06809871960542558667, -6.146186931204439041, -5.354491962338080668 ) ) ;
#23246 = CARTESIAN_POINT ( 'NONE',  ( 57.23886567152862881, 12.43405960935903565, 86.20712845614353625 ) ) ;
#23247 = CARTESIAN_POINT ( 'NONE',  ( 39.40195752203892710, 9.424259417798134919, 29.91383430596324899 ) ) ;
#23248 = CARTESIAN_POINT ( 'NONE',  ( 79.40386128751609363, -170.0000000000000000, -95.00000000000133582 ) ) ;
#23249 = CARTESIAN_POINT ( 'NONE',  ( -180.0765937259068323, 96.80858110077558365, -93.08190667287861686 ) ) ;
#23250 = CARTESIAN_POINT ( 'NONE',  ( 155.7262569076171985, 56.30477153194511430, 71.10411761268670716 ) ) ;
#23251 = CYLINDRICAL_SURFACE ( 'NONE', #10257, 10.00000000000000178 ) ;
#23252 = VERTEX_POINT ( 'NONE', #59420 ) ;
#23253 = CARTESIAN_POINT ( 'NONE',  ( 135.0005116824453921, 43.29964618809727028, -77.78369749464437177 ) ) ;
#23254 = CARTESIAN_POINT ( 'NONE',  ( -143.8634661037141598, 60.82480701605705065, -74.12280952559889613 ) ) ;
#23255 = ORIENTED_EDGE ( 'NONE', *, *, #36557, .T. ) ;
#23256 = CARTESIAN_POINT ( 'NONE',  ( -153.1031717208031750, 68.63449618039562949, -48.89866867094185920 ) ) ;
#23257 = DIRECTION ( 'NONE',  ( 1.000000000000000000, 1.387778780781445922E-16, 0.000000000000000000 ) ) ;
#23258 = CARTESIAN_POINT ( 'NONE',  ( -38.80621516088652356, 11.94263260276895089, 39.18500952932296855 ) ) ;
#23259 = DIRECTION ( 'NONE',  ( -0.000000000000000000, -1.000000000000000000, -0.000000000000000000 ) ) ;
#23260 = CARTESIAN_POINT ( 'NONE',  ( -2.700000000000004619, 0.000000000000000000, -24.69999999999999929 ) ) ;
#23261 = CARTESIAN_POINT ( 'NONE',  ( -15.15117926080556465, 7.479311051197340632, -95.00000000000133582 ) ) ;
#23262 = DIRECTION ( 'NONE',  ( 0.000000000000000000, -1.000000000000000000, 0.000000000000000000 ) ) ;
#23263 = CARTESIAN_POINT ( 'NONE',  ( 74.62299871641495486, 5.461138973199016533, 3.061616997868437868E-16 ) ) ;
#23264 = CARTESIAN_POINT ( 'NONE',  ( -9.765753193741726790, 8.033970690975921869, 30.36677245833251959 ) ) ;
#23265 = CARTESIAN_POINT ( 'NONE',  ( 160.9241720448059141, 60.38677655937336652, 16.73850549852324576 ) ) ;
#23266 = DIRECTION ( 'NONE',  ( 0.000000000000000000, 0.000000000000000000, -1.000000000000000000 ) ) ;
#23267 = ORIENTED_EDGE ( 'NONE', *, *, #65101, .F. ) ;
#23268 = VECTOR ( 'NONE', #40825, 1000.000000000000000 ) ;
#23269 = EDGE_CURVE ( 'NONE', #22457, #58687, #50875, .T. ) ;
#23270 = CARTESIAN_POINT ( 'NONE',  ( -101.8187363387487494, 33.67461140603123226, -50.01457726497595502 ) ) ;
#23271 = ORIENTED_EDGE ( 'NONE', *, *, #68056, .T. ) ;
#23272 = LINE ( 'NONE', #48920, #45301 ) ;
#23273 = CARTESIAN_POINT ( 'NONE',  ( -21.27554331372999741, 61.43430442924864820, 43.58025477438756923 ) ) ;
#23274 = VECTOR ( 'NONE', #66468, 1000.000000000000000 ) ;
#23275 = CARTESIAN_POINT ( 'NONE',  ( 45.90128843543707404, 9.343910238294480308, 60.48342642519485679 ) ) ;
#23276 = CARTESIAN_POINT ( 'NONE',  ( 4.000000000000011546, -6.928203230275505220, -9.500000000000000000 ) ) ;
#23277 = CARTESIAN_POINT ( 'NONE',  ( -6.000000000000000000, 23.07878402833891229, 5.000000000000000000 ) ) ;
#23278 = VECTOR ( 'NONE', #30401, 1000.000000000000114 ) ;
#23279 = DIRECTION ( 'NONE',  ( -0.6910626489868580968, -0.7227948638273978821, 0.000000000000000000 ) ) ;
#23281 = AXIS2_PLACEMENT_3D ( 'NONE', #49898, #60100, #66457 ) ;
#23280 = DIRECTION ( 'NONE',  ( -0.000000000000000000, 1.000000000000000000, -0.000000000000000000 ) ) ;
#23282 = CARTESIAN_POINT ( 'NONE',  ( -119.2804658695887952, 43.47213805166349943, -19.11607275521528848 ) ) ;
#23283 = ORIENTED_EDGE ( 'NONE', *, *, #29208, .F. ) ;
#23284 = VERTEX_POINT ( 'NONE', #2694 ) ;
#23285 = ADVANCED_FACE ( 'NONE', ( #48850 ), #32698, .F. ) ;
#23286 = CARTESIAN_POINT ( 'NONE',  ( 0.000000000000000000, 500.0000000000000000, 0.000000000000000000 ) ) ;
#23287 = CARTESIAN_POINT ( 'NONE',  ( 180.2572128312847326, 77.77323980479698662, 56.18701387320973595 ) ) ;
#23288 = DIRECTION ( 'NONE',  ( -0.7818314824680221431, -0.6234898018587431423, 0.000000000000000000 ) ) ;
#23289 = CARTESIAN_POINT ( 'NONE',  ( -165.6208371326873987, 80.58821715390999429, 64.86840870663141345 ) ) ;
#23290 = VECTOR ( 'NONE', #40977, 1000.000000000000000 ) ;
#23291 = CARTESIAN_POINT ( 'NONE',  ( -171.5023337025455135, 86.83681590836889086, -22.70211854798193940 ) ) ;
#23292 = ADVANCED_FACE ( 'NONE', ( #54129 ), #27411, .T. ) ;
#23293 = ADVANCED_FACE ( 'NONE', ( #40322 ), #22493, .T. ) ;
#23294 = LINE ( 'NONE', #49643, #22772 ) ;
#23295 = ORIENTED_EDGE ( 'NONE', *, *, #11980, .T. ) ;
#23296 = DIRECTION ( 'NONE',  ( -0.000000000000000000, -0.000000000000000000, -1.000000000000000000 ) ) ;
#23297 = CARTESIAN_POINT ( 'NONE',  ( -14.19493007850031674, 7.389842975086043708, 60.49290409118579248 ) ) ;
#23298 = DIRECTION ( 'NONE',  ( -1.000000000000000000, 0.000000000000000000, 0.000000000000000000 ) ) ;
#23299 = FACE_OUTER_BOUND ( 'NONE', #57499, .T. ) ;
#23300 = PLANE ( 'NONE',  #36475 ) ;
#23301 = FACE_OUTER_BOUND ( 'NONE', #20281, .T. ) ;
#23302 = CARTESIAN_POINT ( 'NONE',  ( -62.56514138729678365, 16.82532522382519247, -42.70885660030685216 ) ) ;
#23303 = ORIENTED_EDGE ( 'NONE', *, *, #6348, .T. ) ;
#23304 = CARTESIAN_POINT ( 'NONE',  ( 0.000000000000000000, 0.000000000000000000, 40.00000000000003553 ) ) ;
#23305 = LINE ( 'NONE', #18017, #43983 ) ;
#23306 = CARTESIAN_POINT ( 'NONE',  ( -52.45048892661851170, 15.03803514841138345, 71.70015838030094812 ) ) ;
#23307 = CYLINDRICAL_SURFACE ( 'NONE', #48939, 7.500000000000020428 ) ;
#23308 = CARTESIAN_POINT ( 'NONE',  ( 211.3757499519976477, 117.8130818709823444, 66.97729077751435511 ) ) ;
#23309 = CARTESIAN_POINT ( 'NONE',  ( -4.000000000000013323, 6.928203230275504332, 0.000000000000000000 ) ) ;
#23310 = AXIS2_PLACEMENT_3D ( 'NONE', #348, #33072, #4 ) ;
#23311 = ORIENTED_EDGE ( 'NONE', *, *, #53666, .T. ) ;
#23312 = EDGE_CURVE ( 'NONE', #15400, #37405, #14206, .T. ) ;
#23313 = CARTESIAN_POINT ( 'NONE',  ( 55.90536342106780410, 11.13510150712953362, 8.031316846378679486 ) ) ;
#23314 = DIRECTION ( 'NONE',  ( 0.000000000000000000, 0.000000000000000000, 1.000000000000000000 ) ) ;
#23315 = ORIENTED_EDGE ( 'NONE', *, *, #8907, .T. ) ;
#23317 = CARTESIAN_POINT ( 'NONE',  ( 105.5230584365412909, 27.85718471813526165, -91.26905600704951382 ) ) ;
#23316 = VECTOR ( 'NONE', #34362, 1000.000000000000000 ) ;
#23318 = ORIENTED_EDGE ( 'NONE', *, *, #28923, .F. ) ;
#23319 = FACE_OUTER_BOUND ( 'NONE', #68966, .T. ) ;
#23320 = CARTESIAN_POINT ( 'NONE',  ( -61.77164219855453098, 17.63686644795249592, -12.50187732388345552 ) ) ;
#23321 = CARTESIAN_POINT ( 'NONE',  ( 157.4703587214989398, -170.0000000000000000, -97.31328548006501933 ) ) ;
#23322 = ORIENTED_EDGE ( 'NONE', *, *, #40841, .T. ) ;
#23323 = VECTOR ( 'NONE', #58060, 1000.000000000000114 ) ;
#23324 = ORIENTED_EDGE ( 'NONE', *, *, #28666, .F. ) ;
#23325 = CARTESIAN_POINT ( 'NONE',  ( -64.18058723658640474, -10.37664328995270857, 41.38025477438755928 ) ) ;
#23326 = CARTESIAN_POINT ( 'NONE',  ( 163.5944155533005926, 63.88379440759437955, 32.57248427008062208 ) ) ;
#23327 = CIRCLE ( 'NONE', #10940, 8.000000000000000000 ) ;
#23328 = CARTESIAN_POINT ( 'NONE',  ( -149.9475539515598541, 65.87716206616011050, -61.65738112195565890 ) ) ;
#23329 = CARTESIAN_POINT ( 'NONE',  ( 69.72789637502503979, 15.37065610545703898, 7.113218370438198157 ) ) ;
#23330 = CARTESIAN_POINT ( 'NONE',  ( 89.88695630745277754, 20.55793566325391097, 43.98461035498685590 ) ) ;
#23331 = VERTEX_POINT ( 'NONE', #52260 ) ;
#23332 = VECTOR ( 'NONE', #64750, 1000.000000000000000 ) ;
#23333 = AXIS2_PLACEMENT_3D ( 'NONE', #28881, #28161, #66185 ) ;
#23334 = CARTESIAN_POINT ( 'NONE',  ( 324.1677456657756125, 188.0000000000000000, -123.1183350412580779 ) ) ;
#23335 = CARTESIAN_POINT ( 'NONE',  ( -126.3453033442920344, 47.99870040347946798, -23.06915330777029283 ) ) ;
#23336 = CARTESIAN_POINT ( 'NONE',  ( -46.06722295615723795, -46.37372919877118704, 43.58025477438756212 ) ) ;
#23337 = CARTESIAN_POINT ( 'NONE',  ( 113.8568724296587646, 30.58972477291343495, -23.16725636275993239 ) ) ;
#23338 = CARTESIAN_POINT ( 'NONE',  ( 0.000000000000000000, 0.000000000000000000, 0.000000000000000000 ) ) ;
#23340 = ORIENTED_EDGE ( 'NONE', *, *, #29173, .T. ) ;
#23339 = DIRECTION ( 'NONE',  ( 0.000000000000000000, 0.000000000000000000, 1.000000000000000000 ) ) ;
#23341 = ORIENTED_EDGE ( 'NONE', *, *, #59241, .F. ) ;
#23343 = ORIENTED_EDGE ( 'NONE', *, *, #380, .F. ) ;
#23342 = PRODUCT_DEFINITION ( 'UNKNOWN', '', #34387, #58466 ) ;
#23344 = DIRECTION ( 'NONE',  ( 0.000000000000000000, 0.000000000000000000, -1.000000000000000000 ) ) ;
#23345 = CARTESIAN_POINT ( 'NONE',  ( 177.7964363391244831, 76.75162026635256041, 3.207951730180587546 ) ) ;
#23346 = CARTESIAN_POINT ( 'NONE',  ( -50.13771638889893723, 13.41835215703894235, -10.18558108554858421 ) ) ;
#23347 = CARTESIAN_POINT ( 'NONE',  ( 106.4107271020440209, 27.14892220304137993, -23.02936651802438206 ) ) ;
#23348 = CARTESIAN_POINT ( 'NONE',  ( 197.3059626281005876, 96.72682679064189415, 11.17401084065080674 ) ) ;
#23349 = CARTESIAN_POINT ( 'NONE',  ( 210.3652912788962510, 116.2694780445520450, 85.47466341958396185 ) ) ;
#23350 = EDGE_CURVE ( 'NONE', #49065, #35107, #25547, .T. ) ;
#23351 = CARTESIAN_POINT ( 'NONE',  ( 34.43940527065382895, 66.63700071734666608, 170.0000000000000000 ) ) ;
#23352 = FACE_OUTER_BOUND ( 'NONE', #13640, .T. ) ;
#23353 = CARTESIAN_POINT ( 'NONE',  ( -10.91976120871577649, 7.112268444252506150, 30.77925799739722379 ) ) ;
#23354 = ORIENTED_EDGE ( 'NONE', *, *, #6159, .F. ) ;
#23355 = EDGE_CURVE ( 'NONE', #63883, #11940, #24055, .T. ) ;
#23356 = CARTESIAN_POINT ( 'NONE',  ( -49.45633214486770868, -14.94581086528446789, 26.66469066592268788 ) ) ;
#23357 = VERTEX_POINT ( 'NONE', #4419 ) ;
#23358 = ORIENTED_EDGE ( 'NONE', *, *, #39722, .F. ) ;
#23359 = DIRECTION ( 'NONE',  ( -0.000000000000000000, 1.000000000000000000, -0.000000000000000000 ) ) ;
#23360 = CARTESIAN_POINT ( 'NONE',  ( -57.15783124718920760, 16.30010385357887159, -89.19421615593020647 ) ) ;
#23361 = CARTESIAN_POINT ( 'NONE',  ( -167.0073208999199323, 82.02183861952778443, 33.96945047750333657 ) ) ;
#23362 = CARTESIAN_POINT ( 'NONE',  ( 0.000000000000000000, 0.000000000000000000, 41.38025477438755928 ) ) ;
#23364 = CARTESIAN_POINT ( 'NONE',  ( -105.8768181937898731, 34.64545164169051361, 17.77285717464364367 ) ) ;
#23363 = AXIS2_PLACEMENT_3D ( 'NONE', #48699, #16021, #52954 ) ;
#23365 = B_SPLINE_CURVE_WITH_KNOTS ( 'NONE', 3,
 ( #21124, #52437, #42895, #36608, #336, #4932, #42568, #5613, #58389, #64715, #63685, #47834, #20417, #53103, #4256, #21791, #43239, #10199, #4586, #30990, #37277, #41881, #15501, #26055, #63338, #15150, #69296, #64025, #16172, #15833, #31668, #25716, #68940, #9880, #42223, #59077, #31333, #10894, #7518, #16526, #58727, #32366, #37981, #10546, #47147, #52760, #32021, #47482 ),
 .UNSPECIFIED., .F., .F.,
 ( 4, 2, 2, 2, 2, 2, 2, 2, 2, 2, 2, 2, 2, 2, 2, 2, 2, 2, 2, 2, 2, 2, 2, 4 ),
 ( 0.02554216173022672010, 0.02715505844859240209, 0.02796150680777521533, 0.02876795516695802857, 0.03038085188532359260, 0.03199374860368916357, 0.03360664532205472760, 0.03441309368123751655, 0.03521954204042029857, 0.03602599039960308752, 0.03683243875878587648, 0.03844533547715142663, 0.03925178383633420170, 0.04005823219551697678, 0.04086468055469975880, 0.04167112891388254081, 0.04247757727306530895, 0.04328402563224809096, 0.04489692235061371051, 0.04650981906897933005, 0.04731626742816215370, 0.04812271578734497735, 0.04973561250571069403, 0.05134850922407641072 ),
 .UNSPECIFIED. ) ;
#23366 = FACE_OUTER_BOUND ( 'NONE', #41420, .T. ) ;
#23367 = CARTESIAN_POINT ( 'NONE',  ( 140.2200249818744737, 46.60103563593123255, -20.65665471008218290 ) ) ;
#23368 = ORIENTED_EDGE ( 'NONE', *, *, #4434, .F. ) ;
#23369 = VERTEX_POINT ( 'NONE', #47310 ) ;
#23370 = ORIENTED_EDGE ( 'NONE', *, *, #8591, .F. ) ;
#23371 = AXIS2_PLACEMENT_3D ( 'NONE', #46192, #15231, #41276 ) ;
#23372 = CARTESIAN_POINT ( 'NONE',  ( 0.7145311798163228589, 4.618802153517005848, 8.000000000000000000 ) ) ;
#23373 = CARTESIAN_POINT ( 'NONE',  ( -4.180838820196604466, 65.23214221112780820, 3.125053320693570611E-16 ) ) ;
#23374 = CARTESIAN_POINT ( 'NONE',  ( 0.000000000000000000, -0.1068809833119260672, -91.05865558859387932 ) ) ;
#23375 = B_SPLINE_CURVE_WITH_KNOTS ( 'NONE', 3,
 ( #18324, #39781, #29232, #29568, #23952, #61241 ),
 .UNSPECIFIED., .F., .F.,
 ( 4, 2, 4 ),
 ( 1.095770181104900047E-06, 0.03239442681617710207, 0.06478775786217309818 ),
 .UNSPECIFIED. ) ;
#23377 = EDGE_CURVE ( 'NONE', #19781, #1198, #21841, .T. ) ;
#23376 = APPLICATION_CONTEXT ( 'automotive_design' ) ;
#23378 = AXIS2_PLACEMENT_3D ( 'NONE', #65414, #17206, #38679 ) ;
#23379 = EDGE_CURVE ( 'NONE', #25708, #42749, #68770, .T. ) ;
#23380 = UNCERTAINTY_MEASURE_WITH_UNIT (LENGTH_MEASURE( 1.000000000000000082E-05 ), #49026, 'distance_accuracy_value', 'NONE');
#23381 = CARTESIAN_POINT ( 'NONE',  ( -53.38256734720886243, 14.24001356352782643, 30.50165874791065335 ) ) ;
#23382 = CARTESIAN_POINT ( 'NONE',  ( 199.2049631873262570, 100.7347227143600321, 68.66534253790618436 ) ) ;
#23383 = ORIENTED_EDGE ( 'NONE', *, *, #38668, .F. ) ;
#23384 = VECTOR ( 'NONE', #15865, 1000.000000000000000 ) ;
#23385 = LINE ( 'NONE', #3298, #62677 ) ;
#23386 = CARTESIAN_POINT ( 'NONE',  ( 197.3119541548906568, 98.33923235143194574, -71.98455133656509020 ) ) ;
#23387 = SHAPE_REPRESENTATION_RELATIONSHIP ( 'NONE' , 'NONE' ,  #36174, #54154 ) ;
#23388 = CARTESIAN_POINT ( 'NONE',  ( -4.731197926646205865, 7.716745361328039898, -49.75446812449514766 ) ) ;
#23389 = CARTESIAN_POINT ( 'NONE',  ( -171.2055437419722352, 85.02094814279229240, -88.63902259587010235 ) ) ;
#23390 = CARTESIAN_POINT ( 'NONE',  ( 196.9999999999999716, 6.000000000000000000, 0.000000000000000000 ) ) ;
#23391 = DIRECTION ( 'NONE',  ( 0.000000000000000000, 0.000000000000000000, -1.000000000000000000 ) ) ;
#23392 = CARTESIAN_POINT ( 'NONE',  ( -31.43908319763710679, -170.0000000000000000, -62.16174795566551836 ) ) ;
#23393 = AXIS2_PLACEMENT_3D ( 'NONE', #12712, #6731, #50349 ) ;
#23394 = B_SPLINE_CURVE_WITH_KNOTS ( 'NONE', 3,
 ( #2093, #17558, #49906, #33042, #23195, #17912, #1036, #39027 ),
 .UNSPECIFIED., .F., .F.,
 ( 4, 2, 2, 4 ),
 ( 0.004673709593152140102, 0.005837709341827639932, 0.007001709090503139762, 0.009329708587854139423 ),
 .UNSPECIFIED. ) ;
#23395 = ORIENTED_EDGE ( 'NONE', *, *, #60222, .T. ) ;
#23396 = CARTESIAN_POINT ( 'NONE',  ( 275.5073993722361934, 21.88991381840460448, -2.219103374846307375 ) ) ;
#23397 = CARTESIAN_POINT ( 'NONE',  ( -133.1093894320205493, 51.43221067881453479, -71.37503833356859673 ) ) ;
#23398 = DIRECTION ( 'NONE',  ( 1.000000000000000000, 0.000000000000000000, 0.000000000000000000 ) ) ;
#23399 = DIRECTION ( 'NONE',  ( -0.000000000000000000, -1.000000000000000000, -0.000000000000000000 ) ) ;
#23400 = LINE ( 'NONE', #29350, #32205 ) ;
#23401 = ORIENTED_EDGE ( 'NONE', *, *, #49767, .T. ) ;
#23402 = DIRECTION ( 'NONE',  ( 1.000000000000000000, 0.000000000000000000, 0.000000000000000000 ) ) ;
#23403 = CARTESIAN_POINT ( 'NONE',  ( 188.2509234269329852, 86.16546166485385072, 92.74063656379689746 ) ) ;
#23404 = ORIENTED_EDGE ( 'NONE', *, *, #64103, .F. ) ;
#23405 = VERTEX_POINT ( 'NONE', #10041 ) ;
#23406 = CARTESIAN_POINT ( 'NONE',  ( 176.4367926094705297, 74.03315361639849357, -49.61664505837055827 ) ) ;
#23407 = CARTESIAN_POINT ( 'NONE',  ( -178.5790738944853615, 93.41591512785083751, -63.90684885259965853 ) ) ;
#23408 = B_SPLINE_CURVE_WITH_KNOTS ( 'NONE', 3,
 ( #2232, #51455, #67301, #61990, #66605, #56728, #23345, #66269, #23681, #7151, #28612, #44788, #45124, #18395, #20126, #41578, #46503, #10251, #15195, #41924, #14502, #57415, #26094, #31036, #63034, #62702, #30685, #4631, #20813, #19783, #36655, #21167, #47194, #47524, #35961, #57763, #25765, #4976, #52478, #52810, #25420, #31713, #9577, #9230 ),
 .UNSPECIFIED., .F., .F.,
 ( 4, 2, 2, 2, 2, 2, 2, 2, 2, 2, 2, 2, 2, 2, 2, 2, 2, 2, 2, 2, 2, 4 ),
 ( 0.02895403260893137515, 0.03071603688922227085, 0.03247804116951316655, 0.03424004544980405879, 0.03600204973009495796, 0.03776405401038585019, 0.03864505615053129284, 0.03952605829067672161, 0.04040706043082216425, 0.04128806257096759996, 0.04216906471111303567, 0.04305006685125847138, 0.04393106899140390709, 0.04481207113154934280, 0.04569307327169477850, 0.04657407541184021421, 0.04745507755198564992, 0.04833607969213108563, 0.05009808397242195011, 0.05186008825271282152, 0.05362209253300369294, 0.05714610109358540802 ),
 .UNSPECIFIED. ) ;
#23409 = CARTESIAN_POINT ( 'NONE',  ( 196.9999999999999716, 6.000000000000000000, 0.000000000000000000 ) ) ;
#23410 = EDGE_LOOP ( 'NONE', ( #13990, #43564, #28892, #17082 ) ) ;
#23411 = DIRECTION ( 'NONE',  ( 1.850371928290090422E-16, -1.000000000000000000, -1.110223024625156294E-16 ) ) ;
#23412 = LINE ( 'NONE', #29035, #32251 ) ;
#23413 = CARTESIAN_POINT ( 'NONE',  ( 447.3372781065085633, 399.9999999999998863, 113.5502958579881891 ) ) ;
#23414 = DIRECTION ( 'NONE',  ( 0.000000000000000000, 1.000000000000000000, 0.000000000000000000 ) ) ;
#23415 = CARTESIAN_POINT ( 'NONE',  ( 15.78827728214693416, 6.500811158483322139, -89.20804527961313113 ) ) ;
#23416 = CARTESIAN_POINT ( 'NONE',  ( -52.45048892661851880, 15.03803514841137989, -8.833493391090108560 ) ) ;
#23417 = VERTEX_POINT ( 'NONE', #52930 ) ;
#23418 = CIRCLE ( 'NONE', #68351, 5.000000000000000888 ) ;
#23419 = CARTESIAN_POINT ( 'NONE',  ( 111.1868021579656585, 29.32055685204858975, -35.96702300233707916 ) ) ;
#23420 = CARTESIAN_POINT ( 'NONE',  ( -77.02112161466367013, 22.77583432622784798, 18.39477498643213238 ) ) ;
#23421 = CARTESIAN_POINT ( 'NONE',  ( 45.04360969585142982, 9.210232288266707812, -38.15382515615639392 ) ) ;
#23422 = AXIS2_PLACEMENT_3D ( 'NONE', #18795, #29022, #2974 ) ;
#23424 = ORIENTED_EDGE ( 'NONE', *, *, #22083, .T. ) ;
#23423 = CARTESIAN_POINT ( 'NONE',  ( -133.1633009596832835, 51.47055553769570935, 93.77542264256487670 ) ) ;
#23425 = CARTESIAN_POINT ( 'NONE',  ( 84.97343609940689646, 18.86260005312943733, -36.00277291887266529 ) ) ;
#23426 = EDGE_CURVE ( 'NONE', #4244, #38832, #45946, .T. ) ;
#23427 = MECHANICAL_DESIGN_GEOMETRIC_PRESENTATION_REPRESENTATION (  '', ( #52623 ), #33570 ) ;
#23428 = EDGE_LOOP ( 'NONE', ( #68713, #25660 ) ) ;
#23429 = CARTESIAN_POINT ( 'NONE',  ( -142.5211356634642073, 58.47296527616907724, 62.32377730571725749 ) ) ;
#23430 = FACE_OUTER_BOUND ( 'NONE', #55710, .T. ) ;
#23431 = CARTESIAN_POINT ( 'NONE',  ( 0.000000000000000000, 0.000000000000000000, 41.38025477438755928 ) ) ;
#23432 = CARTESIAN_POINT ( 'NONE',  ( 93.32228019177715339, 22.88890999585040475, 33.81840254634702347 ) ) ;
#23433 = ADVANCED_FACE ( 'NONE', ( #35750 ), #17331, .T. ) ;
#23434 = CARTESIAN_POINT ( 'NONE',  ( 141.3707934840545022, 46.15056991286794386, -16.70842784977412521 ) ) ;
#23435 = DIRECTION ( 'NONE',  ( 0.3090169943749582759, -0.9510565162951499785, 0.000000000000000000 ) ) ;
#23436 = CARTESIAN_POINT ( 'NONE',  ( -178.5750994113944898, 94.98114813978523330, -20.53983915495086165 ) ) ;
#23437 = EDGE_CURVE ( 'NONE', #48053, #29969, #20056, .T. ) ;
#23438 = CARTESIAN_POINT ( 'NONE',  ( 26.12852347772543737, 70.00000000000000000, 129.5802547743875550 ) ) ;
#23439 = EDGE_LOOP ( 'NONE', ( #37397, #58569, #23424, #57408 ) ) ;
#23440 = ORIENTED_EDGE ( 'NONE', *, *, #54651, .T. ) ;
#23441 = ADVANCED_FACE ( 'NONE', ( #59252 ), #32528, .T. ) ;
#23442 = CARTESIAN_POINT ( 'NONE',  ( 46.65037935242577305, 9.463293687292226863, 39.35581152172980524 ) ) ;
#23443 = CARTESIAN_POINT ( 'NONE',  ( -20.55634918610403261, 2.818925648462311528E-14, 0.000000000000000000 ) ) ;
#23444 = DIRECTION ( 'NONE',  ( -1.000000000000000000, -0.000000000000000000, -0.000000000000000000 ) ) ;
#23445 = LINE ( 'NONE', #49795, #12676 ) ;
#23446 = DIRECTION ( 'NONE',  ( -0.000000000000000000, 1.000000000000000000, -0.000000000000000000 ) ) ;
#23447 = CARTESIAN_POINT ( 'NONE',  ( -75.43495400358861502, 22.18831810339352018, -76.23245966557912823 ) ) ;
#23448 = CARTESIAN_POINT ( 'NONE',  ( -104.1244073710069955, 33.72720758483610126, 72.14810588085583731 ) ) ;
#23449 = FACE_OUTER_BOUND ( 'NONE', #31547, .T. ) ;
#23450 = CARTESIAN_POINT ( 'NONE',  ( -4.164416015344990285, -64.86646004871191451, 170.0000000000000000 ) ) ;
#23451 = ORIENTED_EDGE ( 'NONE', *, *, #10728, .T. ) ;
#23452 = ORIENTED_EDGE ( 'NONE', *, *, #4527, .T. ) ;
#23453 = VERTEX_POINT ( 'NONE', #26903 ) ;
#23454 = FACE_OUTER_BOUND ( 'NONE', #18935, .T. ) ;
#23455 = CARTESIAN_POINT ( 'NONE',  ( -173.1211646369891355, -170.0000000000000000, 92.01079578756841215 ) ) ;
#23456 = CARTESIAN_POINT ( 'NONE',  ( -83.51052366780672287, 24.22613130369187573, 70.49372462622615387 ) ) ;
#23457 = EDGE_CURVE ( 'NONE', #6944, #38976, #40944, .T. ) ;
#23458 = DIRECTION ( 'NONE',  ( -0.000000000000000000, -1.000000000000000000, -0.000000000000000000 ) ) ;
#23459 = CARTESIAN_POINT ( 'NONE',  ( 106.9490892766209527, -21.63874093657134878, -3.974828052515719801 ) ) ;
#23460 = CARTESIAN_POINT ( 'NONE',  ( -102.2801239173131052, 33.91021738430207932, -76.85912785543962400 ) ) ;
#23461 = CARTESIAN_POINT ( 'NONE',  ( -35.00000000000002842, -35.00000000000000000, -2.000000000000000000 ) ) ;
#23462 = CARTESIAN_POINT ( 'NONE',  ( 57.09527843067914432, 12.40436368789086785, 32.70209107450780550 ) ) ;
#23463 = DIRECTION ( 'NONE',  ( 1.000000000000000000, 0.000000000000000000, 0.000000000000000000 ) ) ;
#23464 = CARTESIAN_POINT ( 'NONE',  ( 4.165045035620156710, 64.88046627338040651, 3.061616997868437868E-16 ) ) ;
#23465 = ORIENTED_EDGE ( 'NONE', *, *, #25816, .T. ) ;
#23466 = CARTESIAN_POINT ( 'NONE',  ( 442.3372781065085633, 400.0000000000000568, -116.4497041420118393 ) ) ;
#23467 = DIRECTION ( 'NONE',  ( -0.000000000000000000, -0.000000000000000000, -1.000000000000000000 ) ) ;
#23468 = CARTESIAN_POINT ( 'NONE',  ( -71.90777365577110913, -21.14201501538416395, 41.38025477438755928 ) ) ;
#23469 = LINE ( 'NONE', #39633, #20847 ) ;
#23470 = CARTESIAN_POINT ( 'NONE',  ( 200.4600337307565212, 100.7087439352120981, 69.75767833949197438 ) ) ;
#23471 = CARTESIAN_POINT ( 'NONE',  ( -97.21582058037952834, 30.28155166330514803, -90.65436857541234872 ) ) ;
#23472 = CIRCLE ( 'NONE', #61666, 24.99999999999985434 ) ;
#23473 = VERTEX_POINT ( 'NONE', #37805 ) ;
#23474 = CARTESIAN_POINT ( 'NONE',  ( 697.7645910007598786, 891.0064415308993375, 612.5068267248686880 ) ) ;
#23475 = LINE ( 'NONE', #44203, #56511 ) ;
#23476 = CARTESIAN_POINT ( 'NONE',  ( -37.37206033059242571, 11.66494618096613323, -47.41181603092942254 ) ) ;
#23477 = CARTESIAN_POINT ( 'NONE',  ( 50.97490815085634352, 6.000000000000000000, -9.435653166495500344 ) ) ;
#23478 = COLOUR_RGB ( '',0.7921568627450980005, 0.8196078431372548767, 0.9333333333333333481 ) ;
#23479 = CONTEXT_DEPENDENT_SHAPE_REPRESENTATION ( #16150, #54562 ) ;
#23480 = CARTESIAN_POINT ( 'NONE',  ( -165.7109829243804029, 79.24174252277771302, 90.83868518818385951 ) ) ;
#23481 = ORIENTED_EDGE ( 'NONE', *, *, #69148, .F. ) ;
#23482 = LINE ( 'NONE', #44920, #64981 ) ;
#23483 = CARTESIAN_POINT ( 'NONE',  ( -142.2626321327577159, 58.26997216742665131, -17.42748240704912988 ) ) ;
#23484 = CARTESIAN_POINT ( 'NONE',  ( -1.454841858088669948, 7.566772088227306625, -73.72818962830181988 ) ) ;
#23485 = CYLINDRICAL_SURFACE ( 'NONE', #45903, 4.999999999999997335 ) ;
#23486 = ORIENTED_EDGE ( 'NONE', *, *, #28494, .F. ) ;
#23487 = CARTESIAN_POINT ( 'NONE',  ( 164.6046919270428930, 64.73376589608267295, -95.00000000000133582 ) ) ;
#23488 = CARTESIAN_POINT ( 'NONE',  ( 198.4017331595409246, 98.09114638179335088, -47.91029365316073552 ) ) ;
#23489 = CARTESIAN_POINT ( 'NONE',  ( -97.48179118242300945, 31.52606332398819688, 32.23367912195875817 ) ) ;
#23490 = CARTESIAN_POINT ( 'NONE',  ( 23.03864809957654813, 6.841061756139156458, -41.08436505523182092 ) ) ;
#23492 = ORIENTED_EDGE ( 'NONE', *, *, #45920, .F. ) ;
#23491 = CARTESIAN_POINT ( 'NONE',  ( 116.0822834687217409, 32.80169113915574286, 14.99919757508403606 ) ) ;
#23493 = ADVANCED_FACE ( 'NONE', ( #31838 ), #26334, .T. ) ;
#23494 = CARTESIAN_POINT ( 'NONE',  ( -35.00000000000002842, -35.00000000000000000, -2.000000000000000000 ) ) ;
#23495 = VERTEX_POINT ( 'NONE', #4756 ) ;
#23496 = EDGE_LOOP ( 'NONE', ( #59110, #21123, #4063, #38337 ) ) ;
#23497 = CARTESIAN_POINT ( 'NONE',  ( -71.16584859396994034, 19.60484997908768179, -15.53593528491745879 ) ) ;
#23498 = DIRECTION ( 'NONE',  ( 1.000000000000000000, 0.000000000000000000, 0.000000000000000000 ) ) ;
#23500 = ORIENTED_EDGE ( 'NONE', *, *, #44691, .T. ) ;
#23499 = CARTESIAN_POINT ( 'NONE',  ( -11.13714165684778656, 8.138643170880696331, -76.49629683574410421 ) ) ;
#23501 = CARTESIAN_POINT ( 'NONE',  ( 15.55634918610397399, -26.11269837220809364, 85.00100000000000477 ) ) ;
#23503 = AXIS2_PLACEMENT_3D ( 'NONE', #41758, #63215, #19607 ) ;
#23502 = FACE_OUTER_BOUND ( 'NONE', #52077, .T. ) ;
#23504 = CARTESIAN_POINT ( 'NONE',  ( -72.21889834709583056, 21.03534256744171316, -38.75225259531774213 ) ) ;
#23505 = ORIENTED_EDGE ( 'NONE', *, *, #4432, .T. ) ;
#23506 = CARTESIAN_POINT ( 'NONE',  ( 179.3667785869576221, 78.30612312851273771, -90.10490419269625306 ) ) ;
#23507 = EDGE_CURVE ( 'NONE', #42064, #33355, #29697, .T. ) ;
#23508 = CARTESIAN_POINT ( 'NONE',  ( 135.6647932137617545, 43.70902528961477174, 44.30326689254214045 ) ) ;
#23509 = CARTESIAN_POINT ( 'NONE',  ( 154.6343438497236775, 55.47873774496031274, -90.35998153076583606 ) ) ;
#23510 = CARTESIAN_POINT ( 'NONE',  ( -22.06416059020191867, 12.01293505575286602, 0.000000000000000000 ) ) ;
#23511 = FACE_OUTER_BOUND ( 'NONE', #65732, .T. ) ;
#23512 = ORIENTED_EDGE ( 'NONE', *, *, #24071, .T. ) ;
#23513 = AXIS2_PLACEMENT_3D ( 'NONE', #11569, #44280, #43926 ) ;
#23514 = VERTEX_POINT ( 'NONE', #16692 ) ;
#23515 = ORIENTED_EDGE ( 'NONE', *, *, #8681, .F. ) ;
#23516 = ADVANCED_FACE ( 'NONE', ( #69463 ), #64892, .T. ) ;
#23517 = CARTESIAN_POINT ( 'NONE',  ( 6.933333333333328241, 8.000000000000000000, -11.86666666666666536 ) ) ;
#23518 = DIRECTION ( 'NONE',  ( 0.000000000000000000, 0.000000000000000000, -1.000000000000000000 ) ) ;
#23519 = DIRECTION ( 'NONE',  ( 1.000000000000000000, 0.000000000000000000, 0.000000000000000000 ) ) ;
#23520 = CARTESIAN_POINT ( 'NONE',  ( -173.1211646369891355, -170.0000000000000000, -76.55650775521370122 ) ) ;
#23521 = CARTESIAN_POINT ( 'NONE',  ( -142.1381007084227122, 58.17237452544241449, 36.80006697400171589 ) ) ;
#23522 = FACE_OUTER_BOUND ( 'NONE', #51607, .T. ) ;
#23523 = CARTESIAN_POINT ( 'NONE',  ( 109.9975424824652634, 172.0000000000000284, 256.8908838121927261 ) ) ;
#23524 = VERTEX_POINT ( 'NONE', #38498 ) ;
#23525 = CARTESIAN_POINT ( 'NONE',  ( 82.95057496836383848, 18.19812356106674045, 70.61033162475500546 ) ) ;
#23526 = ORIENTED_EDGE ( 'NONE', *, *, #29637, .T. ) ;
#23527 = CARTESIAN_POINT ( 'NONE',  ( -95.93275853296375999, 30.78481241411489577, -92.20198253166996949 ) ) ;
#23528 = SURFACE_STYLE_USAGE ( .BOTH. , #29147 ) ;
#23529 = EDGE_LOOP ( 'NONE', ( #32810, #33867, #50728, #28320 ) ) ;
#23530 = DIRECTION ( 'NONE',  ( -0.000000000000000000, -1.000000000000000000, -0.000000000000000000 ) ) ;
#23531 = EDGE_CURVE ( 'NONE', #32688, #41760, #52189, .T. ) ;
#23532 = DIRECTION ( 'NONE',  ( 0.000000000000000000, 0.000000000000000000, 1.000000000000000000 ) ) ;
#23533 = FACE_OUTER_BOUND ( 'NONE', #67799, .T. ) ;
#23534 = CARTESIAN_POINT ( 'NONE',  ( -22.50000000000003197, -18.06806526123148160, 378.0000000000000000 ) ) ;
#23535 = CARTESIAN_POINT ( 'NONE',  ( -49.45858366215607305, 13.25262207532076175, 5.971190123746847433 ) ) ;
#23536 = VECTOR ( 'NONE', #40025, 1000.000000000000000 ) ;
#23537 = EDGE_CURVE ( 'NONE', #21697, #34571, #7553, .T. ) ;
#23538 = DIRECTION ( 'NONE',  ( 0.9839295885986322210, -0.1785568947986229393, 0.000000000000000000 ) ) ;
#23539 = ADVANCED_FACE ( 'NONE', ( #44110, #65956, #23722, #18441, #2275, #34640, #33933, #49734, #23026, #22671, #50103, #1218, #6838, #66644, #45165, #50455, #27943, #12468, #1933, #39896, #39550, #44829, #28293, #49386, #54669, #6497, #1563, #61004, #65593, #12828, #7894, #61353, #66311, #60655, #38865, #60305, #12127, #17754, #34282, #29012, #33590, #39210, #55371, #13174, #55731, #7192, #28652, #56077, #11280, #17256, #16566, #49257, #16909, #5655, #15875, #64760, #54889, #38025, #59470, #54539, #33466, #59119, #32060, #21838, #32411, #27115, #48549, #69342, #21490, #32750, #6366, #6712, #65112, #53836, #54180, #22543, #6001, #37322, #16218, #53496, #27460, #65464, #22196, #59814, #384, #35, #43285, #48904, #743, #43635, #38369, #11629, #33102, #27819, #47879, #1091, #38727, #43984, #60172, #11993, #21164, #42609, #64064 ), #58774, .F. ) ;
#23540 = CARTESIAN_POINT ( 'NONE',  ( 0.000000000000000000, 190.0000000000000000, 380.0000000000000000 ) ) ;
#23541 = ORIENTED_EDGE ( 'NONE', *, *, #20870, .F. ) ;
#23542 = DIRECTION ( 'NONE',  ( 1.000000000000000000, -0.000000000000000000, 0.000000000000000000 ) ) ;
#23543 = CARTESIAN_POINT ( 'NONE',  ( -152.5046761101291963, 66.76407727525179325, -8.589501201676744913 ) ) ;
#23544 = ORIENTED_EDGE ( 'NONE', *, *, #17779, .F. ) ;
#23545 = CARTESIAN_POINT ( 'NONE',  ( 8.828807734114020533, 74.48902371486721563, 170.0000000000000000 ) ) ;
#23546 = CARTESIAN_POINT ( 'NONE',  ( -55.53456145826332602, 15.85318253404849642, 57.16187836339481976 ) ) ;
#23547 = LINE ( 'NONE', #55896, #65653 ) ;
#23548 = ORIENTED_EDGE ( 'NONE', *, *, #63250, .T. ) ;
#23549 = FACE_OUTER_BOUND ( 'NONE', #31909, .T. ) ;
#23550 = CARTESIAN_POINT ( 'NONE',  ( 152.6804161981488335, 55.27286404993341762, -76.24495480003128023 ) ) ;
#23551 = CARTESIAN_POINT ( 'NONE',  ( -98.69283175933883001, 30.99524616306737812, -22.27381787311723116 ) ) ;
#23552 = CARTESIAN_POINT ( 'NONE',  ( 140.9169160367233360, 45.85398962664670108, -40.93936509524743173 ) ) ;
#23553 = ORIENTED_EDGE ( 'NONE', *, *, #9143, .T. ) ;
#23554 = AXIS2_PLACEMENT_3D ( 'NONE', #40127, #56293, #52734 ) ;
#23555 = FACE_OUTER_BOUND ( 'NONE', #4314, .T. ) ;
#23556 = VERTEX_POINT ( 'NONE', #48210 ) ;
#23557 = DIRECTION ( 'NONE',  ( -0.000000000000000000, -0.000000000000000000, 1.000000000000000000 ) ) ;
#23558 = CARTESIAN_POINT ( 'NONE',  ( -452.6627218934914367, 399.9999999999998863, -146.4497041420118251 ) ) ;
#23559 = CARTESIAN_POINT ( 'NONE',  ( -3.255961059272218350, 7.643453059677440820, 16.73847348745228913 ) ) ;
#23560 = CARTESIAN_POINT ( 'NONE',  ( 140.3960818782622368, 46.71517501795715788, 94.43580953081790597 ) ) ;
#23561 = CARTESIAN_POINT ( 'NONE',  ( 181.0840389613909736, -170.0000000000000000, -70.56960825634330092 ) ) ;
#23562 = DIRECTION ( 'NONE',  ( 0.000000000000000000, 0.000000000000000000, -1.000000000000000000 ) ) ;
#23563 = CARTESIAN_POINT ( 'NONE',  ( -53.31111153860250340, -37.18770477615797176, 170.0000000000000000 ) ) ;
#23564 = ORIENTED_EDGE ( 'NONE', *, *, #36051, .T. ) ;
#23565 = DIRECTION ( 'NONE',  ( 0.000000000000000000, 0.000000000000000000, 1.000000000000000000 ) ) ;
#23566 = FACE_OUTER_BOUND ( 'NONE', #65822, .T. ) ;
#23567 = DIRECTION ( 'NONE',  ( 0.9009688679024155933, 0.4338837391175656699, 0.000000000000000000 ) ) ;
#23568 = CARTESIAN_POINT ( 'NONE',  ( -130.9162414595584494, 51.11675657752020641, -90.51570049338198487 ) ) ;
#23569 = DIRECTION ( 'NONE',  ( 0.000000000000000000, 3.469446951953616038E-17, -1.000000000000000000 ) ) ;
#23570 = VECTOR ( 'NONE', #65970, 1000.000000000000000 ) ;
#23571 = ORIENTED_EDGE ( 'NONE', *, *, #57132, .F. ) ;
#23572 = EDGE_CURVE ( 'NONE', #61065, #31799, #42939, .T. ) ;
#23573 = CARTESIAN_POINT ( 'NONE',  ( 157.4703587214989113, 58.92748579479258808, -24.27963370867398396 ) ) ;
#23574 = CARTESIAN_POINT ( 'NONE',  ( 8.951900209438530709, 6.378066731449591131, 34.42046772285240763 ) ) ;
#23575 = ORIENTED_EDGE ( 'NONE', *, *, #27011, .F. ) ;
#23576 = EDGE_CURVE ( 'NONE', #31797, #67247, #6074, .T. ) ;
#23577 = CARTESIAN_POINT ( 'NONE',  ( 66.30636076182547356, 14.49616748423541424, 70.91462538568637797 ) ) ;
#23578 = CARTESIAN_POINT ( 'NONE',  ( 12.93264331410934354, -21.39501663729232916, 0.000000000000000000 ) ) ;
#23579 = ORIENTED_EDGE ( 'NONE', *, *, #20397, .T. ) ;
#23580 = CARTESIAN_POINT ( 'NONE',  ( 162.7963212667073378, 63.21900188423068556, -38.33791397036713988 ) ) ;
#23581 = AXIS2_PLACEMENT_3D ( 'NONE', #26949, #48376, #56039 ) ;
#23582 = CARTESIAN_POINT ( 'NONE',  ( 66.50000000000000000, 0.000000000000000000, 85.00000000000000000 ) ) ;
#23583 = CARTESIAN_POINT ( 'NONE',  ( 159.2389084450350083, 59.03884018680376755, -36.32203399312435721 ) ) ;
#23584 = EDGE_LOOP ( 'NONE', ( #34728, #57310, #52120, #58584 ) ) ;
#23585 = CARTESIAN_POINT ( 'NONE',  ( -95.60805465865864505, 30.63099276904602419, 7.711323492103204558 ) ) ;
#23586 = ADVANCED_FACE ( 'NONE', ( #50270 ), #8049, .F. ) ;
#23587 = EDGE_CURVE ( 'NONE', #52584, #31501, #3132, .T. ) ;
#23588 = CARTESIAN_POINT ( 'NONE',  ( -15.55634918610400597, 20.55634918610405748, 0.000000000000000000 ) ) ;
#23589 = CARTESIAN_POINT ( 'NONE',  ( 31.90247004928963648, 8.563336936370818719, 36.91044412156482224 ) ) ;
#23590 = CARTESIAN_POINT ( 'NONE',  ( 66.73431804020511038, 14.60294556126670784, 30.79520888878160179 ) ) ;
#23591 = CARTESIAN_POINT ( 'NONE',  ( -128.1219934350341703, 47.97781708504714970, -8.393129055976467967 ) ) ;
#23592 = DIRECTION ( 'NONE',  ( 1.000000000000000000, 0.000000000000000000, 0.000000000000000000 ) ) ;
#23593 = CARTESIAN_POINT ( 'NONE',  ( 126.3580543567275072, 37.07735301062817257, -70.06395634770694869 ) ) ;
#23595 = ORIENTED_EDGE ( 'NONE', *, *, #22330, .F. ) ;
#23594 = ADVANCED_FACE ( 'NONE', ( #66466 ), #34794, .F. ) ;
#23596 = LINE ( 'NONE', #18309, #13004 ) ;
#23597 = CARTESIAN_POINT ( 'NONE',  ( -12.39770133248888939, 8.241491894828994802, 58.49459516380375845 ) ) ;
#23598 = ORIENTED_EDGE ( 'NONE', *, *, #33376, .F. ) ;
#23599 = EDGE_CURVE ( 'NONE', #2210, #14720, #2430, .T. ) ;
#23600 = VECTOR ( 'NONE', #60978, 1000.000000000000000 ) ;
#23601 = CARTESIAN_POINT ( 'NONE',  ( -154.8006992380339000, 70.15733562427992354, -36.97816043303905786 ) ) ;
#23602 = FACE_OUTER_BOUND ( 'NONE', #50503, .T. ) ;
#23603 = CARTESIAN_POINT ( 'NONE',  ( -35.38962320578852427, 11.29584325137385292, 44.09638843715468681 ) ) ;
#23604 = CARTESIAN_POINT ( 'NONE',  ( -167.6413528428655866, 81.22881971256911982, -47.35830433886697932 ) ) ;
#23605 = DIRECTION ( 'NONE',  ( -0.000000000000000000, 1.000000000000000000, -0.000000000000000000 ) ) ;
#23606 = CARTESIAN_POINT ( 'NONE',  ( 0.000000000000000000, 0.000000000000000000, 40.00000000000003553 ) ) ;
#23607 = CARTESIAN_POINT ( 'NONE',  ( -54.09522495088364735, 14.42642983673692392, -77.01522855835996495 ) ) ;
#23608 = CARTESIAN_POINT ( 'NONE',  ( 208.9507214515059843, 112.3605999017434982, -50.01955735436095551 ) ) ;
#23609 = CARTESIAN_POINT ( 'NONE',  ( -10.23531775138760658, 8.068923942586302189, 30.50907025205252410 ) ) ;
#23610 = CARTESIAN_POINT ( 'NONE',  ( 164.4728833318993111, 63.30716077995680990, 12.76463807767628644 ) ) ;
#23611 = EDGE_LOOP ( 'NONE', ( #66245, #24910, #42669, #40612 ) ) ;
#23612 = CARTESIAN_POINT ( 'NONE',  ( -99.10674985723794350, 32.31836975419496838, -49.32651561662824236 ) ) ;
#23613 = VERTEX_POINT ( 'NONE', #55185 ) ;
#23614 = LINE ( 'NONE', #34528, #4831 ) ;
#23615 = EDGE_CURVE ( 'NONE', #54414, #59656, #23547, .T. ) ;
#23616 = CARTESIAN_POINT ( 'NONE',  ( 110.0000000000000284, -21.42428528562853529, 5.000000000000004441 ) ) ;
#23617 = CARTESIAN_POINT ( 'NONE',  ( 45.02738683369923223, 9.207938468499236251, 59.29196373395410546 ) ) ;
#23618 = DIRECTION ( 'NONE',  ( 0.000000000000000000, -0.000000000000000000, 1.000000000000000000 ) ) ;
#23619 = DIRECTION ( 'NONE',  ( 1.000000000000000000, 0.000000000000000000, 0.000000000000000000 ) ) ;
#23620 = ADVANCED_FACE ( 'NONE', ( #23887 ), #2776, .F. ) ;
#23621 = EDGE_CURVE ( 'NONE', #42894, #35286, #24245, .T. ) ;
#23622 = AXIS2_PLACEMENT_3D ( 'NONE', #43869, #52778, #4272 ) ;
#23623 = CARTESIAN_POINT ( 'NONE',  ( -22.50000000000000355, -17.50000000000000000, 1.999999999999998224 ) ) ;
#23624 = CARTESIAN_POINT ( 'NONE',  ( -78.19460645047364267, 22.14203592077027238, 57.26275173013679876 ) ) ;
#23625 = LINE ( 'NONE', #19724, #37479 ) ;
#23626 = ORIENTED_EDGE ( 'NONE', *, *, #41161, .T. ) ;
#23627 = ORIENTED_EDGE ( 'NONE', *, *, #8274, .F. ) ;
#23628 = DIRECTION ( 'NONE',  ( -0.000000000000000000, 1.000000000000000000, -0.000000000000000000 ) ) ;
#23629 = CARTESIAN_POINT ( 'NONE',  ( 173.7227242028391174, 71.47307702680409136, 62.18859588645529612 ) ) ;
#23630 = CARTESIAN_POINT ( 'NONE',  ( -42.02161712141799654, -26.09918303830819042, 0.000000000000000000 ) ) ;
#23631 = DIRECTION ( 'NONE',  ( 1.110223024625155594E-14, 0.000000000000000000, 1.000000000000000000 ) ) ;
#23632 = CARTESIAN_POINT ( 'NONE',  ( -165.7149569557575433, 80.68479365246973600, -14.14659806419673416 ) ) ;
#23633 = VECTOR ( 'NONE', #49800, 1000.000000000000000 ) ;
#23634 = DIRECTION ( 'NONE',  ( 1.000000000000000000, 0.000000000000000000, 0.000000000000000000 ) ) ;
#23635 = ORIENTED_EDGE ( 'NONE', *, *, #43186, .T. ) ;
#23636 = CARTESIAN_POINT ( 'NONE',  ( 103.0004140566503139, 26.76634862952792560, -41.40820395346565164 ) ) ;
#23637 = DIRECTION ( 'NONE',  ( 0.000000000000000000, 0.000000000000000000, 1.000000000000000000 ) ) ;
#23638 = CARTESIAN_POINT ( 'NONE',  ( 123.4242852856285566, 0.000000000000000000, -30.00000000000000000 ) ) ;
#23639 = CARTESIAN_POINT ( 'NONE',  ( -61.29635759142615115, 21.66977272663494958, 170.0000000000000000 ) ) ;
#23640 = DIRECTION ( 'NONE',  ( -0.8160245890732938934, -0.5780171883497599028, 0.000000000000000000 ) ) ;
#23641 = FACE_BOUND ( 'NONE', #11196, .T. ) ;
#23642 = ORIENTED_EDGE ( 'NONE', *, *, #43707, .T. ) ;
#23643 = CARTESIAN_POINT ( 'NONE',  ( -65.36598343705435354, 0.000000000000000000, 41.38025477438755928 ) ) ;
#23644 = DIRECTION ( 'NONE',  ( -1.110223024625118675E-14, 0.000000000000000000, -1.000000000000000000 ) ) ;
#23645 = LINE ( 'NONE', #56689, #66735 ) ;
#23646 = CARTESIAN_POINT ( 'NONE',  ( -176.3763474213711220, 92.36993073950279154, 4.706365262177376607 ) ) ;
#23647 = CARTESIAN_POINT ( 'NONE',  ( 157.4703587214989113, 57.65129005721576760, 2.564916881789689018 ) ) ;
#23648 = VECTOR ( 'NONE', #28367, 1000.000000000000000 ) ;
#23649 = DIRECTION ( 'NONE',  ( 0.000000000000000000, 1.000000000000000000, 0.000000000000000000 ) ) ;
#23650 = ORIENTED_EDGE ( 'NONE', *, *, #25744, .T. ) ;
#23651 = LINE ( 'NONE', #65348, #3379 ) ;
#23652 = CARTESIAN_POINT ( 'NONE',  ( 197.8588046850312878, 99.02485934465610740, -40.73259020836108846 ) ) ;
#23653 = ORIENTED_EDGE ( 'NONE', *, *, #2005, .T. ) ;
#23654 = CARTESIAN_POINT ( 'NONE',  ( -32.53122303423116790, 7.681316636107238693, 6.893342932236740772 ) ) ;
#23655 = ORIENTED_EDGE ( 'NONE', *, *, #35496, .F. ) ;
#23656 = EDGE_CURVE ( 'NONE', #4597, #46092, #44985, .T. ) ;
#23657 = CARTESIAN_POINT ( 'NONE',  ( -86.15275984831842493, 25.31588180512566311, -68.94000942011957989 ) ) ;
#23658 = CARTESIAN_POINT ( 'NONE',  ( -57.42826130032240428, 16.37596353166459906, -22.98975030771917361 ) ) ;
#23659 = CARTESIAN_POINT ( 'NONE',  ( 89.87840278991590992, 21.62393877508912254, -76.93015269146556534 ) ) ;
#23660 = ORIENTED_EDGE ( 'NONE', *, *, #31234, .F. ) ;
#23661 = ORIENTED_EDGE ( 'NONE', *, *, #66589, .T. ) ;
#23662 = CARTESIAN_POINT ( 'NONE',  ( 45.89268866913130296, 10.36133864615983313, 68.02416549870430629 ) ) ;
#23663 = CARTESIAN_POINT ( 'NONE',  ( 437.3372781065085633, 399.9999999999998863, 108.5502958579881891 ) ) ;
#23664 = DIRECTION ( 'NONE',  ( -0.000000000000000000, -0.000000000000000000, -1.000000000000000000 ) ) ;
#23665 = CARTESIAN_POINT ( 'NONE',  ( 70.26639875985993910, 15.51307715494296602, 12.45038511837332074 ) ) ;
#23666 = ORIENTED_EDGE ( 'NONE', *, *, #43959, .T. ) ;
#23667 = EDGE_CURVE ( 'NONE', #50750, #55179, #18609, .T. ) ;
#23668 = CARTESIAN_POINT ( 'NONE',  ( -47.60266343315662141, 13.84328785304052900, 11.97199953281541340 ) ) ;
#23669 = CARTESIAN_POINT ( 'NONE',  ( -125.8938041572051389, 47.69968343338778283, -23.06915330777029638 ) ) ;
#23670 = DIRECTION ( 'NONE',  ( -0.000000000000000000, -0.000000000000000000, -1.000000000000000000 ) ) ;
#23671 = CARTESIAN_POINT ( 'NONE',  ( 115.2288739107204378, 31.25773204386717552, -22.18589349865573013 ) ) ;
#23672 = ADVANCED_FACE ( 'NONE', ( #61519 ), #55535, .F. ) ;
#23673 = CARTESIAN_POINT ( 'NONE',  ( 80.86807176260094820, 17.53499872637983259, 86.08745821396813369 ) ) ;
#23675 = ORIENTED_EDGE ( 'NONE', *, *, #64054, .F. ) ;
#23674 = CARTESIAN_POINT ( 'NONE',  ( -4.613603609464498767, -74.86839895266049894, 170.0000000000000000 ) ) ;
#23676 = ORIENTED_EDGE ( 'NONE', *, *, #52723, .T. ) ;
#23677 = VECTOR ( 'NONE', #65571, 1000.000000000000114 ) ;
#23678 = VERTEX_POINT ( 'NONE', #18257 ) ;
#23679 = CARTESIAN_POINT ( 'NONE',  ( 45.90128843543707404, 9.343910238294474979, 6.794325244267485964 ) ) ;
#23681 = CARTESIAN_POINT ( 'NONE',  ( 176.6238742729555042, 75.60943990211367804, 3.915602851659322869 ) ) ;
#23680 = VECTOR ( 'NONE', #7731, 1000.000000000000000 ) ;
#23682 = CARTESIAN_POINT ( 'NONE',  ( 0.7145311798161619876, -4.618802153517266085, -8.000000000000000000 ) ) ;
#23683 = CARTESIAN_POINT ( 'NONE',  ( 105.8022841538863901, 26.88074187880707910, -22.64102311982845706 ) ) ;
#23684 = CARTESIAN_POINT ( 'NONE',  ( 201.9869293910474823, 102.6997661182766990, 16.86785852109921180 ) ) ;
#23685 = CARTESIAN_POINT ( 'NONE',  ( 200.4927459033473554, 102.4002847909967358, 84.17857932545575750 ) ) ;
#23687 = CARTESIAN_POINT ( 'NONE',  ( 447.3372781065086201, 0.000000000000000000, 78.55029585798817493 ) ) ;
#23686 = VECTOR ( 'NONE', #61208, 1000.000000000000000 ) ;
#23688 = CARTESIAN_POINT ( 'NONE',  ( -65.00200000000002376, 1.250000000000011546, 41.38025477438755928 ) ) ;
#23689 = CARTESIAN_POINT ( 'NONE',  ( -11.14445507968271265, 7.129894202659277092, 30.88547439878327694 ) ) ;
#23690 = ORIENTED_EDGE ( 'NONE', *, *, #59197, .T. ) ;
#23691 = CARTESIAN_POINT ( 'NONE',  ( 15.78827728214693060, 7.507518794609574719, -8.674393508222097537 ) ) ;
#23692 = ORIENTED_EDGE ( 'NONE', *, *, #17292, .T. ) ;
#23693 = EDGE_LOOP ( 'NONE', ( #45373, #33222, #3210, #54673 ) ) ;
#23694 = CARTESIAN_POINT ( 'NONE',  ( -144.2155061717026001, 61.10843690942979833, 16.69664983447127682 ) ) ;
#23695 = CARTESIAN_POINT ( 'NONE',  ( 188.2950976467626560, 87.71503060978555766, -68.48684010819242474 ) ) ;
#23696 = CARTESIAN_POINT ( 'NONE',  ( -33.66581254962768810, 10.98864113404396825, 84.23646623808619438 ) ) ;
#23697 = VECTOR ( 'NONE', #12816, 1000.000000000000000 ) ;
#23698 = CARTESIAN_POINT ( 'NONE',  ( -101.3602137809054682, 32.31558061113913993, -49.97243961166241633 ) ) ;
#23699 = EDGE_CURVE ( 'NONE', #383, #66579, #40401, .T. ) ;
#23700 = PLANE ( 'NONE',  #27020 ) ;
#23701 = CARTESIAN_POINT ( 'NONE',  ( 0.000000000000000000, 0.000000000000000000, 40.00000000000003553 ) ) ;
#23702 = EDGE_CURVE ( 'NONE', #62233, #7559, #40746, .T. ) ;
#23703 = CARTESIAN_POINT ( 'NONE',  ( 141.1220430186941996, 47.19066702031172866, -14.79883838647629446 ) ) ;
#23704 = ORIENTED_EDGE ( 'NONE', *, *, #42413, .T. ) ;
#23705 = ORIENTED_EDGE ( 'NONE', *, *, #28738, .T. ) ;
#23706 = CARTESIAN_POINT ( 'NONE',  ( 187.2885369019321615, 86.60256649394396788, 94.72525040610283042 ) ) ;
#23707 = CARTESIAN_POINT ( 'NONE',  ( -102.2801239173131194, -170.0000000000000000, -15.67002667451224163 ) ) ;
#23708 = CARTESIAN_POINT ( 'NONE',  ( -27.33809850692101051, 60.78020202768021818, 34.48241823986843713 ) ) ;
#23709 = CARTESIAN_POINT ( 'NONE',  ( 56.19513604272051310, 11.19349063094194996, -13.24700682944630259 ) ) ;
#23710 = VECTOR ( 'NONE', #59741, 1000.000000000000000 ) ;
#23711 = CARTESIAN_POINT ( 'NONE',  ( -188.6739852773920347, 108.2139733222100517, 36.71694418889097022 ) ) ;
#23712 = CARTESIAN_POINT ( 'NONE',  ( 201.9721407532275066, 104.3507814346148308, 70.55148779649883295 ) ) ;
#23713 = ORIENTED_EDGE ( 'NONE', *, *, #15494, .F. ) ;
#23714 = CARTESIAN_POINT ( 'NONE',  ( -64.83840629396345889, -4.580509716060184644, 40.00000000000003553 ) ) ;
#23715 = CARTESIAN_POINT ( 'NONE',  ( -59.96408504033279030, 17.10126854471815605, -63.87159806579914800 ) ) ;
#23716 = CARTESIAN_POINT ( 'NONE',  ( 201.5876148766343476, 103.8397408698165378, -63.83233738240677724 ) ) ;
#23717 = CARTESIAN_POINT ( 'NONE',  ( -177.2385321673937142, 68.86478131554724769, 308.3077276702996414 ) ) ;
#23718 = CARTESIAN_POINT ( 'NONE',  ( 279.6727132707902115, -21.42428528562853174, 4.999999999999985789 ) ) ;
#23719 = FILL_AREA_STYLE ('',( #66996 ) ) ;
#23720 = CARTESIAN_POINT ( 'NONE',  ( -166.9982296371934467, 80.56207291422407479, 7.137779597826984457 ) ) ;
#23721 = CARTESIAN_POINT ( 'NONE',  ( -78.66644367742109978, 22.32174330031318732, -50.11545063171791270 ) ) ;
#23722 = FACE_BOUND ( 'NONE', #69418, .T. ) ;
#23723 = CARTESIAN_POINT ( 'NONE',  ( 0.000000000000000000, 0.000000000000000000, 170.0000000000000000 ) ) ;
#23724 = CARTESIAN_POINT ( 'NONE',  ( -0.5158933718595627438, 6.525180340836106652, 66.15742312957483762 ) ) ;
#23725 = ORIENTED_EDGE ( 'NONE', *, *, #58455, .T. ) ;
#23726 = DIRECTION ( 'NONE',  ( -0.000000000000000000, -0.000000000000000000, -1.000000000000000000 ) ) ;
#23727 = CIRCLE ( 'NONE', #61922, 19.99999999999997868 ) ;
#23728 = CARTESIAN_POINT ( 'NONE',  ( 150.2060369882285613, 53.45752899907545697, 65.63963816870943901 ) ) ;
#23729 = FACE_OUTER_BOUND ( 'NONE', #64704, .T. ) ;
#23730 = DIRECTION ( 'NONE',  ( -0.000000000000000000, -1.000000000000000000, -0.000000000000000000 ) ) ;
#23731 = DIRECTION ( 'NONE',  ( -0.000000000000000000, 1.000000000000000000, -0.000000000000000000 ) ) ;
#23732 = VECTOR ( 'NONE', #41300, 1000.000000000000000 ) ;
#23733 = ORIENTED_EDGE ( 'NONE', *, *, #20278, .T. ) ;
#23734 = FILL_AREA_STYLE_COLOUR ( '', #63970 ) ;
#23735 = EDGE_CURVE ( 'NONE', #48439, #4870, #23197, .T. ) ;
#23736 = CARTESIAN_POINT ( 'NONE',  ( -447.6627218934912662, 369.9999999999998295, 108.5502958579877060 ) ) ;
#23737 = ORIENTED_EDGE ( 'NONE', *, *, #9343, .T. ) ;
#23738 = VECTOR ( 'NONE', #31568, 1000.000000000000000 ) ;
#23739 = ORIENTED_EDGE ( 'NONE', *, *, #3644, .F. ) ;
#23740 = ADVANCED_FACE ( 'NONE', ( #56583 ), #17914, .T. ) ;
#23741 = DIRECTION ( 'NONE',  ( 0.000000000000000000, 1.000000000000000000, -0.000000000000000000 ) ) ;
#23742 = CARTESIAN_POINT ( 'NONE',  ( 150.0980941434705187, 53.37942190380064034, 35.50453783569854238 ) ) ;
#23743 = CARTESIAN_POINT ( 'NONE',  ( 29.99999999999999645, -27.00000000000000355, 0.000000000000000000 ) ) ;
#23744 = ORIENTED_EDGE ( 'NONE', *, *, #18650, .F. ) ;
#23745 = DIRECTION ( 'NONE',  ( -1.000000000000000000, 0.000000000000000000, 0.000000000000000000 ) ) ;
#23746 = CARTESIAN_POINT ( 'NONE',  ( -180.5231752320737542, 95.76423526868920533, 12.72482689812798640 ) ) ;
#23747 = CARTESIAN_POINT ( 'NONE',  ( -0.8055628312658252854, 6.535476276302840226, 8.119209976128034967 ) ) ;
#23748 = AXIS2_PLACEMENT_3D ( 'NONE', #28524, #19258, #65826 ) ;
#23749 = DIRECTION ( 'NONE',  ( 0.000000000000000000, 0.000000000000000000, -1.000000000000000000 ) ) ;
#23750 = CARTESIAN_POINT ( 'NONE',  ( -25.80443741485378695, 9.749985135376006085, -10.99864234085158010 ) ) ;
#23751 = CARTESIAN_POINT ( 'NONE',  ( 157.4703587214989113, 57.65129005721576050, 17.56491688178971700 ) ) ;
#23752 = EDGE_CURVE ( 'NONE', #54755, #69128, #12996, .T. ) ;
#23753 = ORIENTED_EDGE ( 'NONE', *, *, #1270, .T. ) ;
#23754 = DIRECTION ( 'NONE',  ( -0.000000000000000000, 0.7071067811865474617, 0.7071067811865474617 ) ) ;
#23755 = CYLINDRICAL_SURFACE ( 'NONE', #31438, 5.000000000000004441 ) ;
#23756 = ADVANCED_FACE ( 'NONE', ( #29853 ), #66127, .F. ) ;
#23757 = B_SPLINE_CURVE_WITH_KNOTS ( 'NONE', 3,
 ( #10926, #64053, #48538, #49246, #59803, #69333, #38715, #38358, #11270, #65098 ),
 .UNSPECIFIED., .F., .F.,
 ( 4, 2, 2, 2, 4 ),
 ( 0.004323147273503904695, 0.005401969756752490054, 0.006480792240001076281, 0.007559614723249662507, 0.008638437206498247867 ),
 .UNSPECIFIED. ) ;
#23758 = LINE ( 'NONE', #51186, #6857 ) ;
#23759 = EDGE_CURVE ( 'NONE', #47060, #17967, #14033, .T. ) ;
#23760 = CARTESIAN_POINT ( 'NONE',  ( 412.3372781065089612, 397.0710678118719557, -111.4497041420121803 ) ) ;
#23762 = VERTEX_POINT ( 'NONE', #57283 ) ;
#23761 = CARTESIAN_POINT ( 'NONE',  ( -118.7818591202210570, 41.98604392202508251, 89.40455488510173154 ) ) ;
#23763 = CARTESIAN_POINT ( 'NONE',  ( 82.95057496836383848, 18.19812356106674045, -36.76787073709972731 ) ) ;
#23764 = ORIENTED_EDGE ( 'NONE', *, *, #67591, .T. ) ;
#23765 = FACE_OUTER_BOUND ( 'NONE', #56839, .T. ) ;
#23766 = CARTESIAN_POINT ( 'NONE',  ( 85.67165909753200026, 20.15791549876377076, 44.66629182770078899 ) ) ;
#23767 = DIRECTION ( 'NONE',  ( -0.000000000000000000, -0.000000000000000000, -1.000000000000000000 ) ) ;
#23768 = CARTESIAN_POINT ( 'NONE',  ( 184.0013086981203116, 81.60415045669145684, -9.957762043733517032 ) ) ;
#23769 = DIRECTION ( 'NONE',  ( 0.000000000000000000, 1.000000000000000000, -0.000000000000000000 ) ) ;
#23770 = LINE ( 'NONE', #28341, #19653 ) ;
#23771 = CARTESIAN_POINT ( 'NONE',  ( -175.1968289912785224, 90.99944698359495021, -8.147980974625541606 ) ) ;
#23772 = LINE ( 'NONE', #33981, #47468 ) ;
#23773 = EDGE_LOOP ( 'NONE', ( #11955, #66661, #29373, #21904 ) ) ;
#23774 = VERTEX_POINT ( 'NONE', #20674 ) ;
#23775 = AXIS2_PLACEMENT_3D ( 'NONE', #20174, #25122, #8936 ) ;
#23776 = CARTESIAN_POINT ( 'NONE',  ( 31.11269837220803325, -15.55634918610409656, 2.000000000000001776 ) ) ;
#23777 = CARTESIAN_POINT ( 'NONE',  ( 158.3595886390532144, 58.34525996025799088, 56.29374580151184659 ) ) ;
#23778 = DIRECTION ( 'NONE',  ( 1.387778780781445429E-16, -1.000000000000000000, -3.081487911019577365E-33 ) ) ;
#23779 = DIRECTION ( 'NONE',  ( 9.899279560275165216E-15, -1.665334536937735057E-16, 1.000000000000000000 ) ) ;
#23780 = CIRCLE ( 'NONE', #1325, 65.00000000000000000 ) ;
#23781 = CARTESIAN_POINT ( 'NONE',  ( -185.0000000000000000, 2.357445088358655073E-14, 2.499999999999999556 ) ) ;
#23782 = CARTESIAN_POINT ( 'NONE',  ( -107.0584934212648420, 35.27493744466470105, 70.66521497598225210 ) ) ;
#23783 = CARTESIAN_POINT ( 'NONE',  ( 0.000000000000000000, 0.000000000000000000, 85.00100000000000477 ) ) ;
#23784 = EDGE_CURVE ( 'NONE', #27023, #14111, #38479, .T. ) ;
#23785 = CARTESIAN_POINT ( 'NONE',  ( 8.000000000000007105, 249.8719672152120381, 94.99999999999866418 ) ) ;
#23786 = EDGE_LOOP ( 'NONE', ( #2513, #20289 ) ) ;
#23787 = PRODUCT_DEFINITION_SHAPE ( 'NONE', 'NONE',  #69590 ) ;
#23788 = ORIENTED_EDGE ( 'NONE', *, *, #43792, .T. ) ;
#23789 = ORIENTED_EDGE ( 'NONE', *, *, #27091, .T. ) ;
#23790 = VECTOR ( 'NONE', #5606, 1000.000000000000000 ) ;
#23791 = CARTESIAN_POINT ( 'NONE',  ( -440.1146514826274938, 400.0000000000065370, -133.9016337311479958 ) ) ;
#23792 = CARTESIAN_POINT ( 'NONE',  ( -71.19538519667726462, 19.61500601486861584, 90.87246897265434598 ) ) ;
#23793 = DIRECTION ( 'NONE',  ( -0.000000000000000000, -0.000000000000000000, -1.000000000000000000 ) ) ;
#23794 = B_SPLINE_CURVE_WITH_KNOTS ( 'NONE', 3,
 ( #58039, #46439, #40823, #54465, #21105, #58709, #53773, #27746, #42873, #22126, #27049, #64341, #1027, #64696, #42547, #37607, #10877, #21773, #38302, #15814, #33033, #59742 ),
 .UNSPECIFIED., .F., .F.,
 ( 4, 2, 2, 2, 2, 2, 2, 2, 2, 2, 4 ),
 ( 0.01028001298432954305, 0.01156964999863937214, 0.01221446850579429276, 0.01285928701294921338, 0.01414892402725907369, 0.01479374253441401513, 0.01543856104156895483, 0.01672819805587879086, 0.01737301656303372882, 0.01801783507018866332, 0.02059710909880842558 ),
 .UNSPECIFIED. ) ;
#23795 = CARTESIAN_POINT ( 'NONE',  ( 129.1052153257903683, 39.78893484542955861, 42.83382366789680162 ) ) ;
#23796 = CARTESIAN_POINT ( 'NONE',  ( 24.96873044429758082, -1.250000000000021982, 0.000000000000000000 ) ) ;
#23797 = LINE ( 'NONE', #33663, #65958 ) ;
#23798 = VECTOR ( 'NONE', #52743, 1000.000000000000000 ) ;
#23799 = CARTESIAN_POINT ( 'NONE',  ( -96.76336539645315327, 31.18045094643428783, -20.77494314902249783 ) ) ;
#23800 = CARTESIAN_POINT ( 'NONE',  ( 56.28782924480458405, 12.23883190161851431, 40.66469570347511819 ) ) ;
#23801 = CARTESIAN_POINT ( 'NONE',  ( 44.50274518366926912, 9.127743804123598537, 85.59476506304760335 ) ) ;
#23802 = CARTESIAN_POINT ( 'NONE',  ( 35.00000000000000000, 4.286263797015736496E-15, 30.00000000000000000 ) ) ;
#23803 = VERTEX_POINT ( 'NONE', #41793 ) ;
#23804 = CARTESIAN_POINT ( 'NONE',  ( -1.728570918131775880, 6.570609986804655023, -47.29287092331269093 ) ) ;
#23805 = DIRECTION ( 'NONE',  ( -1.000000000000000000, 1.509903313490212895E-14, 2.135044278125301096E-16 ) ) ;
#23806 = CARTESIAN_POINT ( 'NONE',  ( -15.27733754929849930, 8.502213909106950851, 11.74977910805278292 ) ) ;
#23807 = CARTESIAN_POINT ( 'NONE',  ( -148.6409722988649946, 63.44808865916660778, 18.82920403144292720 ) ) ;
#23808 = CARTESIAN_POINT ( 'NONE',  ( -102.2801239173131194, -170.0000000000000000, -8.170026674512227416 ) ) ;
#23809 = CARTESIAN_POINT ( 'NONE',  ( 197.1980152960109933, 96.59350208824302797, 63.88959311545310271 ) ) ;
#23810 = B_SPLINE_CURVE_WITH_KNOTS ( 'NONE', 3,
 ( #36737, #22275, #43372, #64844, #32829, #43018, #54258, #48984, #31794, #63465, #15275, #26517, #7142, #28961, #39846, #65907, #6450, #23673, #59892, #1516, #54623, #60952, #7508, #54972, #2225, #61303, #50055, #22980, #50406, #11714, #33187, #34594, #18049, #17340, #44064, #56030, #66262, #44424, #39505, #7844, #27901, #60606, #45116, #49337, #65544, #38812, #12773, #34235, #13127, #55677, #12425, #43712, #33883, #1169 ),
 .UNSPECIFIED., .F., .F.,
 ( 4, 2, 2, 2, 2, 2, 2, 2, 2, 2, 2, 2, 2, 2, 2, 2, 2, 2, 2, 2, 2, 2, 2, 2, 2, 2, 4 ),
 ( 0.000000000000000000, 0.002050985862343569343, 0.003076478793515368109, 0.004101971724687166442, 0.005127464655858964340, 0.006152957587030763106, 0.007178450518202561005, 0.008203943449374360639, 0.009229436380546157670, 0.01025492931171795470, 0.01230591517406149152, 0.01435690103640502834, 0.01538239396757682190, 0.01640788689874861372, 0.01743337982992040555, 0.01845887276109219738, 0.01948436569226398921, 0.02050985862343578103, 0.02256084448577935081, 0.02358633741695114958, 0.02461183034812294834, 0.02563732327929474711, 0.02666281621046654587, 0.02768830914163834464, 0.02871380207281014341, 0.03076478793515374094, 0.03281577379749733153 ),
 .UNSPECIFIED. ) ;
#23811 = CARTESIAN_POINT ( 'NONE',  ( 126.8114659053431410, 38.48351437375811201, -19.30170971946317948 ) ) ;
#23812 = ORIENTED_EDGE ( 'NONE', *, *, #7801, .T. ) ;
#23813 = CARTESIAN_POINT ( 'NONE',  ( 583.3875284499980580, 850.3103760001782803, 739.5068267248710754 ) ) ;
#23814 = CARTESIAN_POINT ( 'NONE',  ( -190.3061188229048923, 108.5745819235681893, -11.38602486233425282 ) ) ;
#23815 = CARTESIAN_POINT ( 'NONE',  ( -35.99414836699284592, 11.40630460607620478, -48.79583236974338689 ) ) ;
#23816 = CYLINDRICAL_SURFACE ( 'NONE', #13280, 25.00000000000145306 ) ;
#23817 = ADVANCED_FACE ( 'NONE', ( #56940 ), #8759, .T. ) ;
#23818 = CARTESIAN_POINT ( 'NONE',  ( -177.1350677909553610, 91.70863480978455584, 85.65203958319301591 ) ) ;
#23819 = EDGE_LOOP ( 'NONE', ( #28770, #59880, #41561, #23465, #46500, #57788, #55468, #3716, #5513, #10648, #57007, #51608, #43189, #35925, #15070 ) ) ;
#23820 = DIRECTION ( 'NONE',  ( -0.000000000000000000, 1.000000000000000000, -0.000000000000000000 ) ) ;
#23821 = EDGE_CURVE ( 'NONE', #30571, #38092, #55297, .T. ) ;
#23822 = ADVANCED_FACE ( 'NONE', ( #58638 ), #60028, .F. ) ;
#23823 = FACE_OUTER_BOUND ( 'NONE', #62051, .T. ) ;
#23824 = ADVANCED_FACE ( 'NONE', ( #11484 ), #58988, .F. ) ;
#23825 = CARTESIAN_POINT ( 'NONE',  ( -0.3252226420479320534, 7.525368746738510417, -70.24936009779905532 ) ) ;
#23826 = EDGE_CURVE ( 'NONE', #52549, #1174, #953, .T. ) ;
#23827 = CARTESIAN_POINT ( 'NONE',  ( 151.3114175117524098, 54.26246727166002870, 86.30372711477225778 ) ) ;
#23828 = ORIENTED_EDGE ( 'NONE', *, *, #52622, .T. ) ;
#23829 = LINE ( 'NONE', #18546, #52561 ) ;
#23830 = DIRECTION ( 'NONE',  ( 0.000000000000000000, 0.000000000000000000, -1.000000000000000000 ) ) ;
#23831 = ADVANCED_FACE ( 'NONE', ( #28024 ), #32276, .T. ) ;
#23832 = CARTESIAN_POINT ( 'NONE',  ( -149.9475539515598257, 65.87716206616006787, 45.72082123989907387 ) ) ;
#23833 = VECTOR ( 'NONE', #51341, 1000.000000000000000 ) ;
#23834 = CARTESIAN_POINT ( 'NONE',  ( 21.73827885904430346, 6.764046335627705631, -47.59151161415723408 ) ) ;
#23835 = CIRCLE ( 'NONE', #58654, 25.12245591505646303 ) ;
#23837 = EDGE_LOOP ( 'NONE', ( #32925, #38279, #21548, #5281 ) ) ;
#23836 = CARTESIAN_POINT ( 'NONE',  ( 117.6853163455685234, 33.60747889659834442, 11.32768630793334452 ) ) ;
#23838 = CARTESIAN_POINT ( 'NONE',  ( 62.04664474957770892, 12.44961624115901699, 44.76574209983286323 ) ) ;
#23839 = ORIENTED_EDGE ( 'NONE', *, *, #6902, .T. ) ;
#23840 = CIRCLE ( 'NONE', #52977, 65.36598343705435354 ) ;
#23841 = VERTEX_POINT ( 'NONE', #10455 ) ;
#23842 = CARTESIAN_POINT ( 'NONE',  ( -172.3038663181179402, 87.72015621195185986, 18.97714401617737678 ) ) ;
#23843 = EDGE_CURVE ( 'NONE', #29654, #67731, #41854, .T. ) ;
#23845 = CARTESIAN_POINT ( 'NONE',  ( 23.28869764673362752, 6.856674305776599532, -69.37513493160868450 ) ) ;
#23844 = AXIS2_PLACEMENT_3D ( 'NONE', #50649, #66854, #61558 ) ;
#23846 = EDGE_CURVE ( 'NONE', #22892, #8745, #64623, .T. ) ;
#23848 = ORIENTED_EDGE ( 'NONE', *, *, #24705, .F. ) ;
#23847 = CARTESIAN_POINT ( 'NONE',  ( -13.79190010541704225, 8.363435739308565431, -65.19196453362162913 ) ) ;
#23849 = PLANE ( 'NONE',  #67912 ) ;
#23850 = CLOSED_SHELL ( 'NONE', ( #67763, #61553, #64908, #48239, #40342, #69561, #14145, #50110, #28282 ) ) ;
#23851 = CARTESIAN_POINT ( 'NONE',  ( -3.841371665203041630E-11, 0.000000000000000000, 10.00000000000000000 ) ) ;
#23852 = CARTESIAN_POINT ( 'NONE',  ( -74.20136529587823304, 21.74007521413448529, -36.58445878614914903 ) ) ;
#23853 = EDGE_LOOP ( 'NONE', ( #2043, #51818, #36277, #32118 ) ) ;
#23854 = CARTESIAN_POINT ( 'NONE',  ( 212.1913428512247322, 119.0779339498137972, -71.02503579638820952 ) ) ;
#23855 = CARTESIAN_POINT ( 'NONE',  ( 137.5911612413395630, 44.91497189902067078, 43.51869277555784521 ) ) ;
#23856 = LINE ( 'NONE', #18570, #23536 ) ;
#23857 = CYLINDRICAL_SURFACE ( 'NONE', #50462, 7.500000000000013323 ) ;
#23858 = CARTESIAN_POINT ( 'NONE',  ( -71.97767679134960872, -170.0000000000000000, 94.99999999999866418 ) ) ;
#23859 = ORIENTED_EDGE ( 'NONE', *, *, #55021, .T. ) ;
#23860 = EDGE_LOOP ( 'NONE', ( #49909, #10331, #44622, #49877 ) ) ;
#23861 = ORIENTED_EDGE ( 'NONE', *, *, #37219, .T. ) ;
#23862 = CARTESIAN_POINT ( 'NONE',  ( 0.000000000000000000, 0.000000000000000000, 41.38025477438755928 ) ) ;
#23863 = CARTESIAN_POINT ( 'NONE',  ( -31.92580063159128301, 9.671320706097198183, -50.31719736520185648 ) ) ;
#23864 = CARTESIAN_POINT ( 'NONE',  ( -99.41031881471059251, 31.34608289732367226, 84.75242236955884323 ) ) ;
#23865 = DIRECTION ( 'NONE',  ( 0.08963930890344089242, -0.9959742939952384022, 2.500042656554810340E-16 ) ) ;
#23866 = CARTESIAN_POINT ( 'NONE',  ( 3.678442866637813759E-12, -65.13282190615278466, -5.000000000000000000 ) ) ;
#23867 = DIRECTION ( 'NONE',  ( -0.000000000000000000, -1.000000000000000000, -0.000000000000000000 ) ) ;
#23868 = ORIENTED_EDGE ( 'NONE', *, *, #32572, .F. ) ;
#23869 = CARTESIAN_POINT ( 'NONE',  ( -106.7004823116342322, 36.22460663120047997, 44.09704765575368413 ) ) ;
#23870 = ORIENTED_EDGE ( 'NONE', *, *, #65109, .T. ) ;
#23871 = CARTESIAN_POINT ( 'NONE',  ( 38.91493890549798351, 8.346224043800607006, 29.91383430596325255 ) ) ;
#23872 = CARTESIAN_POINT ( 'NONE',  ( 0.000000000000000000, 0.000000000000000000, 0.000000000000000000 ) ) ;
#23873 = CARTESIAN_POINT ( 'NONE',  ( 28.03312937960905060, 18.20512990257157426, 6.893342934923163412 ) ) ;
#23874 = CARTESIAN_POINT ( 'NONE',  ( 410.0000000000000000, 0.000000000000000000, 2.000000000000000000 ) ) ;
#23875 = DIRECTION ( 'NONE',  ( -1.000000000000000000, 0.000000000000000000, 0.000000000000000000 ) ) ;
#23876 = CARTESIAN_POINT ( 'NONE',  ( -125.6703656163502245, 47.55170550253213690, 57.46449846362074254 ) ) ;
#23877 = CARTESIAN_POINT ( 'NONE',  ( -11.56945424397727962, 8.173256823723109576, -49.42130677995150023 ) ) ;
#23878 = AXIS2_PLACEMENT_3D ( 'NONE', #64598, #27996, #16405 ) ;
#23879 = CARTESIAN_POINT ( 'NONE',  ( 157.0336341255055856, 57.31169401067816693, -51.12418429913763873 ) ) ;
#23880 = VERTEX_POINT ( 'NONE', #21703 ) ;
#23881 = VECTOR ( 'NONE', #52301, 1000.000000000000000 ) ;
#23882 = CARTESIAN_POINT ( 'NONE',  ( -106.8349332276852977, 35.15552157736319572, -90.24117577083924857 ) ) ;
#23883 = CARTESIAN_POINT ( 'NONE',  ( -157.0077369422017739, 70.81157624963285002, -15.74938127126972098 ) ) ;
#23884 = ORIENTED_EDGE ( 'NONE', *, *, #28368, .F. ) ;
#23885 = DIRECTION ( 'NONE',  ( 1.000000000000000000, 0.000000000000000000, 0.000000000000000000 ) ) ;
#23886 = CARTESIAN_POINT ( 'NONE',  ( -55.54036735998996477, 15.85474597822063636, 72.16187836339486239 ) ) ;
#23887 = FACE_OUTER_BOUND ( 'NONE', #38020, .T. ) ;
#23888 = ORIENTED_EDGE ( 'NONE', *, *, #6157, .T. ) ;
#23889 = CARTESIAN_POINT ( 'NONE',  ( 0.000000000000000000, -1.426547569622074412E-15, 159.3522585083728131 ) ) ;
#23890 = CARTESIAN_POINT ( 'NONE',  ( 150.9128604434958163, 53.97103482421773180, -74.14689824430200815 ) ) ;
#23891 = CARTESIAN_POINT ( 'NONE',  ( -31.92580063159127590, 9.671320706097196407, 30.21645440618916467 ) ) ;
#23892 = VECTOR ( 'NONE', #9072, 1000.000000000000000 ) ;
#23893 = CARTESIAN_POINT ( 'NONE',  ( -24.33435124463267130, 8.532637995283112176, 66.97631264891070657 ) ) ;
#23894 = EDGE_LOOP ( 'NONE', ( #45647, #39948, #3182, #56900 ) ) ;
#23896 = AXIS2_PLACEMENT_3D ( 'NONE', #5557, #17859, #59020 ) ;
#23895 = SHAPE_REPRESENTATION_RELATIONSHIP ( 'NONE' , 'NONE' ,  #64096, #40723 ) ;
#23897 = DIRECTION ( 'NONE',  ( 0.000000000000000000, -0.000000000000000000, 1.000000000000000000 ) ) ;
#23898 = ORIENTED_EDGE ( 'NONE', *, *, #59527, .T. ) ;
#23899 = CARTESIAN_POINT ( 'NONE',  ( 33.31166872005965729, 8.707041209322236242, -20.65919876726036719 ) ) ;
#23900 = CARTESIAN_POINT ( 'NONE',  ( 181.9295719569814764, 79.46350097013164770, 2.499600187509602112 ) ) ;
#23901 = DIRECTION ( 'NONE',  ( 0.9749279121818227312, 0.2225209339563184729, 5.102127870520021228E-18 ) ) ;
#23902 = CARTESIAN_POINT ( 'NONE',  ( 127.0101228374496998, 38.59541841538369056, 87.63242888966352950 ) ) ;
#23903 = FACE_OUTER_BOUND ( 'NONE', #58031, .T. ) ;
#23904 = ADVANCED_FACE ( 'NONE', ( #53357 ), #48764, .F. ) ;
#23905 = CARTESIAN_POINT ( 'NONE',  ( -120.4586945679390482, 43.01762219615314109, -64.06711385159694316 ) ) ;
#23906 = VERTEX_POINT ( 'NONE', #69540 ) ;
#23907 = CARTESIAN_POINT ( 'NONE',  ( 164.8471526211110927, 63.62172173173269130, -15.39771934190674330 ) ) ;
#23908 = CYLINDRICAL_SURFACE ( 'NONE', #53022, 65.36598343705435354 ) ;
#23909 = CARTESIAN_POINT ( 'NONE',  ( 67.93926590385571274, 13.86859831467925197, 69.83615169925958810 ) ) ;
#23910 = CARTESIAN_POINT ( 'NONE',  ( 137.4117721579686986, 43.61242559081429704, -63.74683598648854854 ) ) ;
#23911 = EDGE_CURVE ( 'NONE', #2651, #27095, #53707, .T. ) ;
#23912 = DIRECTION ( 'NONE',  ( 0.000000000000000000, 0.000000000000000000, 1.000000000000000000 ) ) ;
#23913 = EDGE_LOOP ( 'NONE', ( #16135, #60322, #39724, #50168 ) ) ;
#23914 = LINE ( 'NONE', #13366, #50749 ) ;
#23915 = DIRECTION ( 'NONE',  ( 0.000000000000000000, 0.000000000000000000, 1.000000000000000000 ) ) ;
#23916 = ORIENTED_EDGE ( 'NONE', *, *, #17943, .F. ) ;
#23917 = CARTESIAN_POINT ( 'NONE',  ( -12.50000000000000000, 207.5000000000000284, 20.00000000000000000 ) ) ;
#23918 = CARTESIAN_POINT ( 'NONE',  ( -109.0191069781766657, -170.0000000000000000, 94.99999999999866418 ) ) ;
#23919 = EDGE_CURVE ( 'NONE', #8726, #36296, #10825, .T. ) ;
#23920 = AXIS2_PLACEMENT_3D ( 'NONE', #37508, #58613, #59645 ) ;
#23921 = ORIENTED_EDGE ( 'NONE', *, *, #3257, .T. ) ;
#23922 = CARTESIAN_POINT ( 'NONE',  ( 160.4986104110022609, 61.33701824525267199, -36.75893793876068827 ) ) ;
#23923 = LINE ( 'NONE', #18992, #65075 ) ;
#23924 = DIRECTION ( 'NONE',  ( -0.000000000000000000, -1.000000000000000000, -0.000000000000000000 ) ) ;
#23925 = CARTESIAN_POINT ( 'NONE',  ( 161.7048274740120917, 61.01946783654761219, -49.83182248474824405 ) ) ;
#23926 = AXIS2_PLACEMENT_3D ( 'NONE', #36408, #24130, #14943 ) ;
#23927 = VERTEX_POINT ( 'NONE', #50184 ) ;
#23928 = CARTESIAN_POINT ( 'NONE',  ( -98.67557579989343708, 32.10670856967968945, 4.580045852397571338 ) ) ;
#23929 = AXIS2_PLACEMENT_3D ( 'NONE', #26308, #64272, #37891 ) ;
#23930 = CARTESIAN_POINT ( 'NONE',  ( 64.66746655423649770, 14.09646650629620979, 83.67892219932799946 ) ) ;
#23931 = CARTESIAN_POINT ( 'NONE',  ( 429.8372781065084496, 400.0000000000042633, 96.05029585798401115 ) ) ;
#23932 = CARTESIAN_POINT ( 'NONE',  ( 82.94816950786172072, 19.25538918181906567, -9.938066344431240040 ) ) ;
#23933 = CARTESIAN_POINT ( 'NONE',  ( -131.3154845336012215, 50.16828105866952114, -20.77399769732809531 ) ) ;
#23934 = VECTOR ( 'NONE', #10288, 1000.000000000000000 ) ;
#23935 = CARTESIAN_POINT ( 'NONE',  ( 152.1327777395850376, 53.61712543276776444, 69.02866056097568048 ) ) ;
#23936 = CARTESIAN_POINT ( 'NONE',  ( 132.9485794245231602, 40.87843215479637138, -62.90929565402166190 ) ) ;
#23937 = VERTEX_POINT ( 'NONE', #23468 ) ;
#23938 = CARTESIAN_POINT ( 'NONE',  ( 5.799999999999999822, 8.000000000000000000, 0.000000000000000000 ) ) ;
#23939 = CARTESIAN_POINT ( 'NONE',  ( -119.1064753703575718, 43.36500113374746945, 94.99999999999866418 ) ) ;
#23940 = ORIENTED_EDGE ( 'NONE', *, *, #55920, .T. ) ;
#23941 = AXIS2_PLACEMENT_3D ( 'NONE', #38199, #34339, #44529 ) ;
#23942 = CARTESIAN_POINT ( 'NONE',  ( -151.2428028786328014, 66.99705074331122034, -49.62230637302906899 ) ) ;
#23943 = CARTESIAN_POINT ( 'NONE',  ( 2.644994884459113571, -7.710515798486386352, -0.08224679563972556173 ) ) ;
#23944 = CARTESIAN_POINT ( 'NONE',  ( 15.78827728214693771, 7.507518794609574719, 71.85925826316895382 ) ) ;
#23945 = CARTESIAN_POINT ( 'NONE',  ( -1.095583923122880332, 7.553030873957007785, 40.93520185086673280 ) ) ;
#23946 = CARTESIAN_POINT ( 'NONE',  ( -7.825402957745085430, 6.891034867348153625, -89.10717191287116634 ) ) ;
#23947 = CARTESIAN_POINT ( 'NONE',  ( -47.55235941796723864, 12.79790236059690400, -69.32320573674819286 ) ) ;
#23948 = CARTESIAN_POINT ( 'NONE',  ( -0.5658006089934850547, 7.533733779014708531, -18.02006150488200831 ) ) ;
#23949 = CARTESIAN_POINT ( 'NONE',  ( -422.6627218934906978, 394.9999999999998295, 83.55029585798750702 ) ) ;
#23950 = CARTESIAN_POINT ( 'NONE',  ( -60.97727891098335817, 16.35024395194894709, 6.347587653709224398 ) ) ;
#23951 = ORIENTED_EDGE ( 'NONE', *, *, #46140, .F. ) ;
#23952 = CARTESIAN_POINT ( 'NONE',  ( -17.35806719188560265, 28.56537455181723928, 6.893343212288936428 ) ) ;
#23953 = VERTEX_POINT ( 'NONE', #44907 ) ;
#23954 = CARTESIAN_POINT ( 'NONE',  ( 103.1567541746301657, 25.73937982110324540, -72.77541118461569170 ) ) ;
#23955 = CARTESIAN_POINT ( 'NONE',  ( 45.04506994399702080, 10.22854084020123722, -21.24017278588418378 ) ) ;
#23956 = CARTESIAN_POINT ( 'NONE',  ( 42.71504753277075395, 8.863481902720391048, 70.99139177545366408 ) ) ;
#23957 = FACE_OUTER_BOUND ( 'NONE', #36609, .T. ) ;
#23958 = CARTESIAN_POINT ( 'NONE',  ( -447.6627218934914367, 399.9999999999998863, -136.4497041420118251 ) ) ;
#23959 = CARTESIAN_POINT ( 'NONE',  ( 0.3173508448886513400, 5.375634714784618851, -6.689127551062007626 ) ) ;
#23960 = ADVANCED_FACE ( 'NONE', ( #1648 ), #40996, .T. ) ;
#23961 = CYLINDRICAL_SURFACE ( 'NONE', #54375, 7.500000000000013323 ) ;
#23962 = DIRECTION ( 'NONE',  ( -0.000000000000000000, 1.000000000000000000, -0.000000000000000000 ) ) ;
#23963 = ORIENTED_EDGE ( 'NONE', *, *, #27948, .T. ) ;
#23964 = ORIENTED_EDGE ( 'NONE', *, *, #50890, .F. ) ;
#23965 = DIRECTION ( 'NONE',  ( 1.000000000000000000, 0.000000000000000000, 0.000000000000000000 ) ) ;
#23966 = PLANE ( 'NONE',  #59139 ) ;
#23967 = CARTESIAN_POINT ( 'NONE',  ( -31.11269837220801193, 36.11269837220812207, 0.000000000000000000 ) ) ;
#23968 = EDGE_CURVE ( 'NONE', #46238, #35076, #55452, .T. ) ;
#23969 = CARTESIAN_POINT ( 'NONE',  ( 108.3942953861066485, 29.14039925067522674, 56.67208651439320732 ) ) ;
#23970 = AXIS2_PLACEMENT_3D ( 'NONE', #66308, #56412, #45512 ) ;
#23971 = CARTESIAN_POINT ( 'NONE',  ( 2.699999999999990408, 0.000000000000000000, 0.000000000000000000 ) ) ;
#23972 = CIRCLE ( 'NONE', #7096, 185.0000000000000000 ) ;
#23973 = CARTESIAN_POINT ( 'NONE',  ( 59.29474530993688575, 12.86968658439548996, -9.859655179614705389 ) ) ;
#23974 = VERTEX_POINT ( 'NONE', #29767 ) ;
#23975 = CARTESIAN_POINT ( 'NONE',  ( 442.3372781065085633, 370.0000000000038085, 108.5502958579885870 ) ) ;
#23976 = CARTESIAN_POINT ( 'NONE',  ( 22.89270809252618832, 7.840160460323050806, -40.60289454668881604 ) ) ;
#23977 = CARTESIAN_POINT ( 'NONE',  ( -86.15275984831841072, 25.31588180512570574, -15.25090823919218153 ) ) ;
#23978 = AXIS2_PLACEMENT_3D ( 'NONE', #46257, #61744, #25523 ) ;
#23979 = DIRECTION ( 'NONE',  ( 0.000000000000000000, 0.000000000000000000, -1.000000000000000000 ) ) ;
#23980 = CARTESIAN_POINT ( 'NONE',  ( 209.6877167158270652, 113.4449353909247407, -11.37733726706599491 ) ) ;
#23981 = FACE_BOUND ( 'NONE', #5624, .T. ) ;
#23983 = EDGE_CURVE ( 'NONE', #52549, #10264, #26773, .T. ) ;
#23982 = VECTOR ( 'NONE', #26515, 1000.000000000000000 ) ;
#23984 = AXIS2_PLACEMENT_3D ( 'NONE', #65868, #27857, #49300 ) ;
#23985 = EDGE_CURVE ( 'NONE', #18138, #57137, #33672, .T. ) ;
#23986 = VECTOR ( 'NONE', #66920, 1000.000000000000227 ) ;
#23987 = ORIENTED_EDGE ( 'NONE', *, *, #48862, .F. ) ;
#23988 = PLANE ( 'NONE',  #59227 ) ;
#23989 = DIRECTION ( 'NONE',  ( -1.001915251000354105E-14, 1.000000000000000000, -5.551115123125782702E-17 ) ) ;
#23990 = AXIS2_PLACEMENT_3D ( 'NONE', #66614, #40215, #8205 ) ;
#23991 = DIRECTION ( 'NONE',  ( -0.000000000000000000, -0.000000000000000000, -1.000000000000000000 ) ) ;
#23992 = CARTESIAN_POINT ( 'NONE',  ( -180.4614954900548298, 97.28277348252829881, 9.908402751631699701 ) ) ;
#23993 = EDGE_CURVE ( 'NONE', #11589, #46342, #30460, .T. ) ;
#23994 = CARTESIAN_POINT ( 'NONE',  ( 210.6592759200687794, 116.7161312026394029, 68.11051040608630558 ) ) ;
#23995 = CARTESIAN_POINT ( 'NONE',  ( -173.1211646369891355, 87.12891641440857882, 30.82169460664101734 ) ) ;
#23996 = EDGE_LOOP ( 'NONE', ( #59455, #7177, #51561, #11394 ) ) ;
#23997 = CARTESIAN_POINT ( 'NONE',  ( 188.9999999999999432, -35.00000000000000000, -2.000000000000000888 ) ) ;
#23998 = CARTESIAN_POINT ( 'NONE',  ( -5.690023276062404101, -5.952467836904166809, -9.369346954796180071 ) ) ;
#23999 = ORIENTED_EDGE ( 'NONE', *, *, #61245, .T. ) ;
#24000 = LINE ( 'NONE', #60933, #30651 ) ;
#24001 = ORIENTED_EDGE ( 'NONE', *, *, #21033, .T. ) ;
#24002 = CARTESIAN_POINT ( 'NONE',  ( 6.400000000000000355, 9.237604307034018802, 0.000000000000000000 ) ) ;
#24003 = CARTESIAN_POINT ( 'NONE',  ( -56.01329802674225533, 15.98369420723829570, -23.32578036508402519 ) ) ;
#24004 = CARTESIAN_POINT ( 'NONE',  ( 94.14197848494937659, 23.19876128416616368, -70.15589403930768242 ) ) ;
#24006 = ORIENTED_EDGE ( 'NONE', *, *, #40841, .F. ) ;
#24005 = EDGE_CURVE ( 'NONE', #39183, #29751, #51075, .T. ) ;
#24007 = ORIENTED_EDGE ( 'NONE', *, *, #37141, .F. ) ;
#24008 = CARTESIAN_POINT ( 'NONE',  ( 46.23304607317101045, 10.41544405387738692, 61.15242819165885635 ) ) ;
#24009 = ADVANCED_FACE ( 'NONE', ( #31496 ), #63505, .F. ) ;
#24011 = EDGE_CURVE ( 'NONE', #38551, #52273, #40662, .T. ) ;
#24010 = CARTESIAN_POINT ( 'NONE',  ( 447.3372781065086770, 400.0000000000000568, -146.4497041420117966 ) ) ;
#24012 = EDGE_CURVE ( 'NONE', #32175, #44993, #18442, .T. ) ;
#24013 = CARTESIAN_POINT ( 'NONE',  ( 16.76400266940279238, 6.533513613209218640, 3.217594506424259482 ) ) ;
#24014 = ORIENTED_EDGE ( 'NONE', *, *, #38207, .T. ) ;
#24015 = B_SPLINE_CURVE_WITH_KNOTS ( 'NONE', 3,
 ( #42462, #33313, #1291, #34705, #29077, #44180, #55089, #34360, #22745, #6913, #28724, #50522, #56141, #28364, #39621, #50173, #22393, #943, #60722, #60017, #65669, #49811, #34002, #2002, #38936, #54742, #7626, #11837, #39965, #60383, #12197, #23795, #43832, #17457, #12542, #28013, #18170, #44549 ),
 .UNSPECIFIED., .F., .F.,
 ( 4, 2, 2, 2, 2, 2, 2, 2, 2, 2, 2, 2, 2, 2, 2, 2, 2, 2, 4 ),
 ( 0.02546424207107602852, 0.02703543426729208138, 0.02782103036540014424, 0.02860662646350820362, 0.03017781865972439526, 0.03174901085594058342, 0.03332020305215677852, 0.03489139524837296669, 0.03646258744458916179, 0.03724818354269725240, 0.03803377964080534995, 0.03881937573891344750, 0.03960497183702154506, 0.04117616403323773322, 0.04274735622945392832, 0.04431854842567012343, 0.04588974062188631853, 0.04746093281810250669, 0.05060331721053488996 ),
 .UNSPECIFIED. ) ;
#24016 = DIRECTION ( 'NONE',  ( -0.000000000000000000, 0.000000000000000000, 1.000000000000000000 ) ) ;
#24017 = CARTESIAN_POINT ( 'NONE',  ( 58.46823952472683317, 12.69204591816733263, -37.23638717655476427 ) ) ;
#24018 = CONICAL_SURFACE ( 'NONE', #9458, 73.43826238111391547, 0.6747409422235518539 ) ;
#24019 = CARTESIAN_POINT ( 'NONE',  ( -13.18921082026369618, 8.309042481534840263, -91.29599530343861602 ) ) ;
#24020 = DIRECTION ( 'NONE',  ( -1.000000000000000000, 0.000000000000000000, 0.000000000000000000 ) ) ;
#24021 = LINE ( 'NONE', #3947, #51154 ) ;
#24023 = VERTEX_POINT ( 'NONE', #21619 ) ;
#24022 = DIRECTION ( 'NONE',  ( 1.000000000000000000, 0.000000000000000000, 0.000000000000000000 ) ) ;
#24024 = EDGE_LOOP ( 'NONE', ( #68728, #56549, #46570, #8401 ) ) ;
#24025 = VECTOR ( 'NONE', #17097, 1000.000000000000000 ) ;
#24026 = ORIENTED_EDGE ( 'NONE', *, *, #12395, .F. ) ;
#24027 = VECTOR ( 'NONE', #7957, 1000.000000000000000 ) ;
#24028 = CARTESIAN_POINT ( 'NONE',  ( 46.64694836521740484, 9.462741877720631578, 8.614408483111491321 ) ) ;
#24029 = DIRECTION ( 'NONE',  ( -1.850371928290090422E-16, 1.000000000000000000, 1.110223024625156171E-16 ) ) ;
#24030 = CARTESIAN_POINT ( 'NONE',  ( -51.34325167237332010, 13.71819364263221530, -9.348823597919418305 ) ) ;
#24031 = CARTESIAN_POINT ( 'NONE',  ( 103.8093541423578614, 26.01745837747064272, -20.46464144355324422 ) ) ;
#24032 = CARTESIAN_POINT ( 'NONE',  ( 42.02161712141799654, -26.09918303830819042, 0.000000000000000000 ) ) ;
#24033 = VECTOR ( 'NONE', #21767, 1000.000000000000000 ) ;
#24034 = CARTESIAN_POINT ( 'NONE',  ( 209.2537571925653026, 114.6008442271929226, 84.43188915064283151 ) ) ;
#24035 = AXIS2_PLACEMENT_3D ( 'NONE', #20947, #37812, #5109 ) ;
#24036 = PLANE ( 'NONE',  #56828 ) ;
#24037 = DIRECTION ( 'NONE',  ( 0.000000000000000000, 0.000000000000000000, -1.000000000000000000 ) ) ;
#24038 = CARTESIAN_POINT ( 'NONE',  ( -8.320652113663530969, 6.923290556636832349, 45.11558103944723541 ) ) ;
#24039 = ORIENTED_EDGE ( 'NONE', *, *, #53887, .F. ) ;
#24040 = AXIS2_PLACEMENT_3D ( 'NONE', #3489, #62931, #45714 ) ;
#24041 = CARTESIAN_POINT ( 'NONE',  ( 9.050324533885206080, 7.384616180193987134, -19.50471979745130469 ) ) ;
#24042 = ORIENTED_EDGE ( 'NONE', *, *, #8595, .F. ) ;
#24043 = VERTEX_POINT ( 'NONE', #48673 ) ;
#24044 = DIRECTION ( 'NONE',  ( -0.000000000000000000, -0.000000000000000000, 1.000000000000000000 ) ) ;
#24045 = DIRECTION ( 'NONE',  ( -1.000000000000000000, 0.000000000000000000, 0.000000000000000000 ) ) ;
#24046 = VECTOR ( 'NONE', #18604, 1000.000000000000000 ) ;
#24047 = CARTESIAN_POINT ( 'NONE',  ( -38.46365568132284807, 11.87544203234370066, 88.69750035019276879 ) ) ;
#24048 = CARTESIAN_POINT ( 'NONE',  ( -8.470329472542999693E-17, -0.7818963812180738104, 8.000000000000000000 ) ) ;
#24049 = LINE ( 'NONE', #25445, #3490 ) ;
#24050 = EDGE_CURVE ( 'NONE', #16525, #8487, #43065, .T. ) ;
#24051 = CARTESIAN_POINT ( 'NONE',  ( 169.9999999999999716, 3.680555555555560243, 4.000000000000000000 ) ) ;
#24052 = CARTESIAN_POINT ( 'NONE',  ( 126.5880720616306121, 37.20544379858409911, -41.65621509857714955 ) ) ;
#24053 = ORIENTED_EDGE ( 'NONE', *, *, #59603, .F. ) ;
#24054 = VERTEX_POINT ( 'NONE', #43413 ) ;
#24055 =( BOUNDED_CURVE ( )  B_SPLINE_CURVE ( 3, ( #46283, #15320, #52598, #51914 ),
 .UNSPECIFIED., .F., .F. ) 
 B_SPLINE_CURVE_WITH_KNOTS ( ( 4, 4 ),
 ( 0.000000000000000000, 1.570796326794796638 ),
 .UNSPECIFIED. ) 
 CURVE ( )  GEOMETRIC_REPRESENTATION_ITEM ( )  RATIONAL_B_SPLINE_CURVE ( ( 1.000000000000000000, 0.8047378541243885852, 0.8047378541243885852, 1.000000000000000000 ) ) 
 REPRESENTATION_ITEM ( '' )  );
#24056 = ADVANCED_FACE ( 'NONE', ( #64536 ), #4754, .F. ) ;
#24057 = PLANE ( 'NONE',  #10259 ) ;
#24058 = CARTESIAN_POINT ( 'NONE',  ( -14.55425570676091773, 7.423011834016144839, 14.09261391691513765 ) ) ;
#24059 = DIRECTION ( 'NONE',  ( -1.020422603260505347E-14, 1.000000000000000000, 5.551115123125782702E-17 ) ) ;
#24060 = CARTESIAN_POINT ( 'NONE',  ( -23.99924996210628692, 8.487987924059021694, -68.68209970087039551 ) ) ;
#24061 = UNCERTAINTY_MEASURE_WITH_UNIT (LENGTH_MEASURE( 1.000000000000000082E-05 ), #31232, 'distance_accuracy_value', 'NONE');
#24062 = CARTESIAN_POINT ( 'NONE',  ( 12.46704290855393360, 6.417105965824391411, 3.941120416641372692 ) ) ;
#24063 = EDGE_LOOP ( 'NONE', ( #7606, #18381, #46614, #20220, #27705, #44645 ) ) ;
#24064 = DIRECTION ( 'NONE',  ( -3.989004196750080799E-18, -3.181124695048499213E-18, -1.000000000000000000 ) ) ;
#24065 = CARTESIAN_POINT ( 'NONE',  ( -62.50103539982529099, 17.85731685071835528, -70.57177136977581711 ) ) ;
#24066 = CARTESIAN_POINT ( 'NONE',  ( 201.5987353083854998, 103.8544727311226836, -77.51376041726710753 ) ) ;
#24067 = CARTESIAN_POINT ( 'NONE',  ( 275.5080822241899909, -21.88977794987917491, -2.220096651196673765 ) ) ;
#24068 = DIRECTION ( 'NONE',  ( -0.000000000000000000, 1.000000000000000000, -0.000000000000000000 ) ) ;
#24069 = CARTESIAN_POINT ( 'NONE',  ( -167.1540252468942072, 80.72321878831102993, 6.926423838769506958 ) ) ;
#24070 = CARTESIAN_POINT ( 'NONE',  ( 46.39999999999999858, 0.000000000000000000, 4.171999999999999709 ) ) ;
#24071 = EDGE_CURVE ( 'NONE', #31978, #67838, #27590, .T. ) ;
#24072 = CARTESIAN_POINT ( 'NONE',  ( -47.55360235114366674, 12.79819361309568571, 64.14926665824262386 ) ) ;
#24073 = ADVANCED_FACE ( 'NONE', ( #64185 ), #16690, .T. ) ;
#24074 = ADVANCED_FACE ( 'NONE', ( #31836, #38144 ), #21966, .T. ) ;
#24075 = CIRCLE ( 'NONE', #18492, 2.999999999999999112 ) ;
#24076 = FACE_OUTER_BOUND ( 'NONE', #39827, .T. ) ;
#24077 = ADVANCED_FACE ( 'NONE', ( #10370 ), #59250, .T. ) ;
#24078 = ORIENTED_EDGE ( 'NONE', *, *, #613, .F. ) ;
#24080 = CARTESIAN_POINT ( 'NONE',  ( 277.4922189950061693, 21.56887920590509111, 4.337924292484275135 ) ) ;
#24079 = AXIS2_PLACEMENT_3D ( 'NONE', #67744, #57873, #52587 ) ;
#24081 = CARTESIAN_POINT ( 'NONE',  ( 150.4542242713869484, 53.63744268572192198, 66.41804297856887729 ) ) ;
#24082 = CARTESIAN_POINT ( 'NONE',  ( 204.6977192012829505, 108.0580384837234931, 29.20772073876942088 ) ) ;
#24083 = B_SPLINE_CURVE_WITH_KNOTS ( 'NONE', 3,
 ( #51581, #41020, #9704, #29770, #31171, #3051, #63171, #51234, #61768, #67414, #3388, #14965, #68771, #19916, #9020, #46284, #41371, #30463, #14291, #67761, #3722, #24513, #57202, #51915, #20586, #35054, #35752, #25202, #62825, #52599, #14628, #36091, #57547, #30815, #9351, #8326, #45947, #19205, #13937, #47312, #41708, #13594, #52261 ),
 .UNSPECIFIED., .F., .F.,
 ( 4, 2, 2, 2, 2, 2, 2, 2, 1, 2, 2, 2, 2, 2, 2, 2, 2, 2, 2, 2, 2, 4 ),
 ( 3.469446951953614189E-18, 0.001466285743483493852, 0.002199428615225239910, 0.002932571486966985535, 0.004398857230450466810, 0.005865142973933949386, 0.007331428717417431094, 0.008064571589159175852, 0.008797714460900918007, 0.009530857332642663632, 0.01026400020438440752, 0.01173028594786789183, 0.01319657169135137788, 0.01466285743483486219, 0.01539600030657660261, 0.01612914317831834130, 0.01759542892180181173, 0.01906171466528528563, 0.01979485753702702258, 0.02052800040876875606, 0.02199428615225222650, 0.02346057189573569693 ),
 .UNSPECIFIED. ) ;
#24084 = LINE ( 'NONE', #61360, #63781 ) ;
#24085 = CARTESIAN_POINT ( 'NONE',  ( 64.98797965777978902, 1.249999999999979350, 170.0000000000000000 ) ) ;
#24086 = AXIS2_PLACEMENT_3D ( 'NONE', #58386, #47831, #10196 ) ;
#24087 = ORIENTED_EDGE ( 'NONE', *, *, #64141, .T. ) ;
#24088 = CIRCLE ( 'NONE', #6076, 5.000000000000000888 ) ;
#24089 = CARTESIAN_POINT ( 'NONE',  ( 8.828807734114011652, 74.48902371486721563, 133.5802547743875550 ) ) ;
#24090 = DIRECTION ( 'NONE',  ( -1.000000000000000000, 0.000000000000000000, 0.000000000000000000 ) ) ;
#24091 = ORIENTED_EDGE ( 'NONE', *, *, #35809, .T. ) ;
#24092 = ORIENTED_EDGE ( 'NONE', *, *, #38853, .T. ) ;
#24093 = VECTOR ( 'NONE', #18291, 1000.000000000000000 ) ;
#24094 = DIRECTION ( 'NONE',  ( -0.000000000000000000, -1.000000000000000000, -0.000000000000000000 ) ) ;
#24095 = CARTESIAN_POINT ( 'NONE',  ( 152.1381498073140790, 54.87048121475574192, 31.61318467975951663 ) ) ;
#24096 = DIRECTION ( 'NONE',  ( -1.000000000000000000, 0.000000000000000000, 0.000000000000000000 ) ) ;
#24097 = ORIENTED_EDGE ( 'NONE', *, *, #63202, .T. ) ;
#24098 = CARTESIAN_POINT ( 'NONE',  ( 31.11269837220800127, -31.11269837220812562, 2.000000000000001776 ) ) ;
#24099 = CARTESIAN_POINT ( 'NONE',  ( -178.7483298110139458, 93.61800926271536127, 6.512559139046779855 ) ) ;
#24100 = CARTESIAN_POINT ( 'NONE',  ( -2.190131154568199179, 6.589492063460817839, 5.815768188893855495 ) ) ;
#24101 = CARTESIAN_POINT ( 'NONE',  ( 55.56634333706183781, 12.09342294753929892, -44.22217901802044082 ) ) ;
#24102 = ADVANCED_FACE ( 'NONE', ( #22320 ), #20936, .T. ) ;
#24104 = ADVANCED_FACE ( 'NONE', ( #37446 ), #47656, .F. ) ;
#24103 = CARTESIAN_POINT ( 'NONE',  ( -83.13046924527392889, 25.15778674529016357, 31.88650284985251915 ) ) ;
#24105 = CARTESIAN_POINT ( 'NONE',  ( -3.816391647148975608E-14, -9.237604307034022355, -0.7145311798163346273 ) ) ;
#24106 = LINE ( 'NONE', #57489, #14038 ) ;
#24107 = ADVANCED_FACE ( 'NONE', ( #64890 ), #11759, .F. ) ;
#24108 = VERTEX_POINT ( 'NONE', #11400 ) ;
#24109 = CARTESIAN_POINT ( 'NONE',  ( 117.3110050642448101, 32.29133253383016466, -45.98121923047796145 ) ) ;
#24110 = CARTESIAN_POINT ( 'NONE',  ( -77.71490760329790248, 23.03637365463981723, 3.619075319522604417 ) ) ;
#24111 = CARTESIAN_POINT ( 'NONE',  ( 41.81982603358023454, 8.735900550613184379, -36.00357662167354533 ) ) ;
#24112 = DIRECTION ( 'NONE',  ( -1.000000000000000000, -4.565061778886334783E-18, 0.000000000000000000 ) ) ;
#24114 = ORIENTED_EDGE ( 'NONE', *, *, #48199, .F. ) ;
#24113 = CARTESIAN_POINT ( 'NONE',  ( 442.3372781065085633, 370.0000000000001137, -141.4497041420118251 ) ) ;
#24115 = DIRECTION ( 'NONE',  ( 0.000000000000000000, 0.000000000000000000, 1.000000000000000000 ) ) ;
#24116 = EDGE_LOOP ( 'NONE', ( #62046, #4550, #840, #65819 ) ) ;
#24117 = DIRECTION ( 'NONE',  ( 1.000000000000000000, 0.000000000000000000, 0.000000000000000000 ) ) ;
#24118 = CARTESIAN_POINT ( 'NONE',  ( 109.9975424824652634, 179.2896996249788799, 369.5505932007772003 ) ) ;
#24119 = FACE_OUTER_BOUND ( 'NONE', #1720, .T. ) ;
#24120 = CARTESIAN_POINT ( 'NONE',  ( 185.1802655733641529, 82.84606286178492951, -10.58188840605224534 ) ) ;
#24121 = CARTESIAN_POINT ( 'NONE',  ( -124.1094910780272329, 45.33021696310841975, 57.67627168393939741 ) ) ;
#24122 = DIRECTION ( 'NONE',  ( -0.000000000000000000, 1.000000000000000000, -0.000000000000000000 ) ) ;
#24123 = CARTESIAN_POINT ( 'NONE',  ( -177.1381400275772080, 93.26609858452818003, -21.71591573839441125 ) ) ;
#24124 = VECTOR ( 'NONE', #54003, 1000.000000000000000 ) ;
#24125 = CARTESIAN_POINT ( 'NONE',  ( -47.79955240516189008, 13.88975739862082648, 35.84505809694404377 ) ) ;
#24126 = ORIENTED_EDGE ( 'NONE', *, *, #28085, .T. ) ;
#24127 = VERTEX_POINT ( 'NONE', #5783 ) ;
#24128 = CARTESIAN_POINT ( 'NONE',  ( 104.7034219878852070, 26.40210929103716353, 58.87558030574008683 ) ) ;
#24129 = DIRECTION ( 'NONE',  ( 0.000000000000000000, 1.000000000000000000, 0.000000000000000000 ) ) ;
#24130 = DIRECTION ( 'NONE',  ( -0.000000000000000000, 1.000000000000000000, -0.000000000000000000 ) ) ;
#24131 = AXIS2_PLACEMENT_3D ( 'NONE', #67493, #28821, #62203 ) ;
#24132 = CARTESIAN_POINT ( 'NONE',  ( 185.5415406465189676, 83.23025870924411151, -49.77515318378037534 ) ) ;
#24133 = CARTESIAN_POINT ( 'NONE',  ( -109.0297561673456386, 36.34391931706014134, 68.14367124605330162 ) ) ;
#24134 = AXIS2_PLACEMENT_3D ( 'NONE', #18603, #28816, #66810 ) ;
#24135 = CARTESIAN_POINT ( 'NONE',  ( -25.35398647985413945, 8.671412257862215256, -47.20835425011359376 ) ) ;
#24136 = CARTESIAN_POINT ( 'NONE',  ( 164.7250737226290482, 63.51898362052163804, -68.54626621448289825 ) ) ;
#24137 = VERTEX_POINT ( 'NONE', #53622 ) ;
#24138 = ORIENTED_EDGE ( 'NONE', *, *, #20958, .F. ) ;
#24139 = AXIS2_PLACEMENT_3D ( 'NONE', #62508, #30157, #52287 ) ;
#24140 = ORIENTED_EDGE ( 'NONE', *, *, #24190, .T. ) ;
#24141 = DIRECTION ( 'NONE',  ( -0.000000000000000000, -0.000000000000000000, -1.000000000000000000 ) ) ;
#24142 = EDGE_CURVE ( 'NONE', #35701, #57672, #33236, .T. ) ;
#24143 = AXIS2_PLACEMENT_3D ( 'NONE', #41018, #29768, #68440 ) ;
#24144 = CARTESIAN_POINT ( 'NONE',  ( -73.15403579853486349, 20.29791129869458643, 86.51172062028520315 ) ) ;
#24145 = CARTESIAN_POINT ( 'NONE',  ( 66.50000000000000000, 0.000000000000000000, 17.57656211871651308 ) ) ;
#24146 = FACE_OUTER_BOUND ( 'NONE', #52858, .T. ) ;
#24147 = DIRECTION ( 'NONE',  ( -1.393823445737823288E-16, 0.7660444431189770143, 0.6427876096865403621 ) ) ;
#24148 = CARTESIAN_POINT ( 'NONE',  ( -60.66101049381763488, 17.30588917955501316, 42.82097766060025634 ) ) ;
#24149 = CARTESIAN_POINT ( 'NONE',  ( -96.02159028238561689, 30.82695531378848841, -11.52968351012710180 ) ) ;
#24150 = DIRECTION ( 'NONE',  ( 0.6427876096865403621, -0.7660444431189770143, 1.393823445737823288E-16 ) ) ;
#24151 = CARTESIAN_POINT ( 'NONE',  ( 31.91416675805597336, 7.553393781468399126, 90.55988232731206722 ) ) ;
#24152 = DIRECTION ( 'NONE',  ( 0.000000000000000000, 1.000000000000000000, -0.000000000000000000 ) ) ;
#24153 = ORIENTED_EDGE ( 'NONE', *, *, #68245, .T. ) ;
#24154 = DIRECTION ( 'NONE',  ( 0.9510565162951544194, -0.3090169943749446757, 0.000000000000000000 ) ) ;
#24155 = DIRECTION ( 'NONE',  ( -0.000000000000000000, -0.000000000000000000, -1.000000000000000000 ) ) ;
#24156 = CARTESIAN_POINT ( 'NONE',  ( -189.2826425734428994, 107.1493800926106275, -41.23753037017266365 ) ) ;
#24157 = CARTESIAN_POINT ( 'NONE',  ( 181.0840389613909736, -170.0000000000000000, 44.30859410551141764 ) ) ;
#24158 = ADVANCED_FACE ( 'NONE', ( #32874 ), #49029, .F. ) ;
#24159 = CARTESIAN_POINT ( 'NONE',  ( 282.2220340837702679, -21.53708152545855725, -4.491189304432787743 ) ) ;
#24160 = CARTESIAN_POINT ( 'NONE',  ( -106.6940984894958007, 35.07986071359378855, -75.44142825345944914 ) ) ;
#24161 = CARTESIAN_POINT ( 'NONE',  ( 126.3681350380370958, 38.23508791628618297, -16.18615085686329991 ) ) ;
#24162 = EDGE_CURVE ( 'NONE', #48193, #8543, #33104, .T. ) ;
#24163 = EDGE_CURVE ( 'NONE', #34668, #45811, #39836, .T. ) ;
#24164 = ORIENTED_EDGE ( 'NONE', *, *, #53812, .F. ) ;
#24165 = DIRECTION ( 'NONE',  ( -9.664909915183042863E-15, 4.028099159653623277E-15, -0.9999999999999997780 ) ) ;
#24166 = DIRECTION ( 'NONE',  ( 0.000000000000000000, -0.8660254037844382635, -0.5000000000000008882 ) ) ;
#24167 = CARTESIAN_POINT ( 'NONE',  ( -38.93847286785603501, 11.96870349976818027, -43.32391969549294686 ) ) ;
#24168 = LINE ( 'NONE', #40672, #46956 ) ;
#24169 = ITEM_DEFINED_TRANSFORMATION ( 'NONE', 'NONE', #27519,  #66832 ) ;
#24170 = CARTESIAN_POINT ( 'NONE',  ( -178.4330126279765523, 93.24097428920383379, 86.68317579884340773 ) ) ;
#24171 = ORIENTED_EDGE ( 'NONE', *, *, #40114, .F. ) ;
#24172 = CARTESIAN_POINT ( 'NONE',  ( -125.8938041572051105, 46.49392987655494380, -34.91370389823391918 ) ) ;
#24173 = CARTESIAN_POINT ( 'NONE',  ( -148.4259959918497600, 63.26767374754767559, -8.043489788822235198 ) ) ;
#24174 = CARTESIAN_POINT ( 'NONE',  ( 198.8752826725511227, 100.3130050945023299, 5.128836562248959119 ) ) ;
#24175 = ORIENTED_EDGE ( 'NONE', *, *, #54937, .T. ) ;
#24176 = VECTOR ( 'NONE', #15203, 1000.000000000000000 ) ;
#24177 = CARTESIAN_POINT ( 'NONE',  ( 150.1779365646289932, 53.43719151385364086, 92.36095605438667633 ) ) ;
#24178 = ORIENTED_EDGE ( 'NONE', *, *, #314, .F. ) ;
#24179 = CARTESIAN_POINT ( 'NONE',  ( -58.32502757340554211, 16.62877055630753631, 4.207105285353801349 ) ) ;
#24180 = CARTESIAN_POINT ( 'NONE',  ( 126.3580543567275640, 37.07735301062818678, 37.31424601414773434 ) ) ;
#24181 = AXIS2_PLACEMENT_3D ( 'NONE', #30663, #24704, #31020 ) ;
#24182 = FACE_OUTER_BOUND ( 'NONE', #57636, .T. ) ;
#24183 = DIRECTION ( 'NONE',  ( -0.000000000000000000, 1.000000000000000000, -0.000000000000000000 ) ) ;
#24184 = VECTOR ( 'NONE', #55334, 1000.000000000000000 ) ;
#24186 = LINE ( 'NONE', #35073, #50734 ) ;
#24185 = CIRCLE ( 'NONE', #12988, 243.4957430088094839 ) ;
#24188 = ORIENTED_EDGE ( 'NONE', *, *, #3422, .T. ) ;
#24187 = DIRECTION ( 'NONE',  ( -0.2225209339563042066, -0.9749279121818259508, 0.000000000000000000 ) ) ;
#24189 =( GEOMETRIC_REPRESENTATION_CONTEXT ( 3 ) GLOBAL_UNCERTAINTY_ASSIGNED_CONTEXT ( ( #63421 ) ) GLOBAL_UNIT_ASSIGNED_CONTEXT ( ( #46277, #52925, #69458 ) ) REPRESENTATION_CONTEXT ( 'NONE', 'WORKASPACE' ) );
#24190 = EDGE_CURVE ( 'NONE', #62155, #8631, #2273, .T. ) ;
#24191 = CARTESIAN_POINT ( 'NONE',  ( 55.52750043885184539, 11.05966813607792787, 36.82308146611499211 ) ) ;
#24192 = CIRCLE ( 'NONE', #19658, 5.000000000000087930 ) ;
#24193 = VERTEX_POINT ( 'NONE', #28649 ) ;
#24194 = VERTEX_POINT ( 'NONE', #60653 ) ;
#24195 = PLANE ( 'NONE',  #55860 ) ;
#24196 = AXIS2_PLACEMENT_3D ( 'NONE', #14626, #41369, #67412 ) ;
#24197 = CARTESIAN_POINT ( 'NONE',  ( 18.66025561752210038, 6.609375019058819412, -76.80469486127859113 ) ) ;
#24199 = ORIENTED_EDGE ( 'NONE', *, *, #13768, .T. ) ;
#24198 = CARTESIAN_POINT ( 'NONE',  ( -133.3799602664182657, 52.86209125874979975, 65.49465508212347231 ) ) ;
#24200 = DIRECTION ( 'NONE',  ( -2.921639538487254261E-16, -1.134144525784205431E-35, -1.000000000000000000 ) ) ;
#24201 = DIRECTION ( 'NONE',  ( 0.000000000000000000, 0.000000000000000000, 1.000000000000000000 ) ) ;
#24202 = FACE_BOUND ( 'NONE', #28138, .T. ) ;
#24203 = EDGE_LOOP ( 'NONE', ( #51317, #3738 ) ) ;
#24204 = CARTESIAN_POINT ( 'NONE',  ( 211.5034924207028268, 118.0100795718634998, -67.50466236550761323 ) ) ;
#24205 = B_SPLINE_CURVE_WITH_KNOTS ( 'NONE', 3,
 ( #39247, #49070, #23423, #909, #39930, #7232, #6171, #33966, #28689, #22359, #59979, #44862, #22706, #44516, #65990, #49774, #45204, #50487, #65272, #1600, #60690, #17063, #33278, #65632, #54707, #6875, #7591, #18135, #6534, #12866, #66347, #61040, #34321, #28327, #49423, #1253, #33626, #55769, #17420, #38899, #61388, #55056, #2310, #23761, #13210, #23064, #25155, #14246, #7926, #56110, #46237, #45551, #8278, #3340, #51188, #51534 ),
 .UNSPECIFIED., .F., .F.,
 ( 4, 2, 2, 2, 2, 2, 2, 2, 2, 2, 2, 2, 2, 2, 2, 2, 2, 2, 2, 2, 2, 2, 2, 2, 2, 2, 2, 4 ),
 ( 0.000000000000000000, 0.002031929280119430282, 0.003047893920179118102, 0.004063858560238805921, 0.005079823200298493741, 0.006095787840358182427, 0.007111752480417870247, 0.008127717120477558066, 0.009143681760537246753, 0.01015964640059693370, 0.01117561104065662239, 0.01219157568071631108, 0.01320754032077599803, 0.01422350496083568498, 0.01625543424095507103, 0.01828736352107445534, 0.02031929280119383271, 0.02133525744125350579, 0.02235122208131317192, 0.02336718672137284153, 0.02438315136143250766, 0.02641508064155189198, 0.02743104528161158240, 0.02844700992167126935, 0.02946297456173096324, 0.03047893920179065019, 0.03149490384185034408, 0.03251086848191003104 ),
 .UNSPECIFIED. ) ;
#24206 = CARTESIAN_POINT ( 'NONE',  ( 140.7888851157410102, 46.97220912571250295, 39.88480869005077523 ) ) ;
#24207 = DIRECTION ( 'NONE',  ( -0.000000000000000000, 1.000000000000000000, -0.000000000000000000 ) ) ;
#24208 = CARTESIAN_POINT ( 'NONE',  ( -132.8150886319751862, 52.45790550853842404, 8.374808787430902512 ) ) ;
#24209 = CARTESIAN_POINT ( 'NONE',  ( 66.30230369578305272, 14.49551544185123220, -76.81116625487784688 ) ) ;
#24210 = ORIENTED_EDGE ( 'NONE', *, *, #2326, .T. ) ;
#24211 = ORIENTED_EDGE ( 'NONE', *, *, #66970, .F. ) ;
#24212 = FACE_OUTER_BOUND ( 'NONE', #63064, .T. ) ;
#24213 = CARTESIAN_POINT ( 'NONE',  ( 210.9044300540503514, 115.2613339746486076, -93.29905180977844736 ) ) ;
#24214 = PLANE ( 'NONE',  #55798 ) ;
#24215 = DIRECTION ( 'NONE',  ( 0.000000000000000000, 0.000000000000000000, -1.000000000000000000 ) ) ;
#24216 = CARTESIAN_POINT ( 'NONE',  ( -20.63749999999999929, 0.000000000000000000, -19.99999999999999289 ) ) ;
#24217 = EDGE_CURVE ( 'NONE', #6748, #56804, #52795, .T. ) ;
#24218 = LINE ( 'NONE', #29828, #66580 ) ;
#24219 = CARTESIAN_POINT ( 'NONE',  ( -72.21947956767112942, 21.03570528348185320, -19.61146733724643099 ) ) ;
#24221 = EDGE_LOOP ( 'NONE', ( #45018, #4686, #65598, #21780 ) ) ;
#24220 = EDGE_CURVE ( 'NONE', #11797, #11917, #24306, .T. ) ;
#24222 = CARTESIAN_POINT ( 'NONE',  ( -104.1393288135077313, 34.86912007524089319, 45.30014082762043159 ) ) ;
#24223 = ORIENTED_EDGE ( 'NONE', *, *, #57908, .T. ) ;
#24224 = VECTOR ( 'NONE', #27639, 1000.000000000000000 ) ;
#24225 = CARTESIAN_POINT ( 'NONE',  ( 33.03621582719334526, 7.666716336587123592, 33.44051306690047909 ) ) ;
#24226 = EDGE_CURVE ( 'NONE', #8357, #11118, #2963, .T. ) ;
#24227 = CARTESIAN_POINT ( 'NONE',  ( 86.15454111412294935, 20.32174891186170029, 56.55663816294301682 ) ) ;
#24228 = ORIENTED_EDGE ( 'NONE', *, *, #29845, .F. ) ;
#24229 = DIRECTION ( 'NONE',  ( 0.000000000000000000, 0.000000000000000000, 1.000000000000000000 ) ) ;
#24230 = PLANE ( 'NONE',  #26518 ) ;
#24232 = CARTESIAN_POINT ( 'NONE',  ( 141.9165763529819344, -52.00000000000000711, 129.0000000000000000 ) ) ;
#24231 = VECTOR ( 'NONE', #43732, 1000.000000000000114 ) ;
#24233 = CARTESIAN_POINT ( 'NONE',  ( 11.30618213853385967, 74.15344055032308290, 170.0000000000000000 ) ) ;
#24234 = CYLINDRICAL_SURFACE ( 'NONE', #68207, 7.500000000000020428 ) ;
#24235 = CARTESIAN_POINT ( 'NONE',  ( 152.6560521232695748, 54.00248515670892147, -49.38016601471965572 ) ) ;
#24236 = VECTOR ( 'NONE', #28550, 1000.000000000000000 ) ;
#24237 = AXIS2_PLACEMENT_3D ( 'NONE', #68373, #30385, #51837 ) ;
#24238 = ORIENTED_EDGE ( 'NONE', *, *, #56787, .T. ) ;
#24239 = CARTESIAN_POINT ( 'NONE',  ( 169.9999999999999716, 3.680555555555560243, 0.000000000000000000 ) ) ;
#24240 = FACE_OUTER_BOUND ( 'NONE', #61730, .T. ) ;
#24241 = VERTEX_POINT ( 'NONE', #29684 ) ;
#24242 = AXIS2_PLACEMENT_3D ( 'NONE', #10126, #47069, #52353 ) ;
#24243 = CARTESIAN_POINT ( 'NONE',  ( -452.6627218934859798, 400.0000000000064801, -146.4497041420121377 ) ) ;
#24244 = LINE ( 'NONE', #34793, #29691 ) ;
#24245 = LINE ( 'NONE', #67166, #460 ) ;
#24246 = ORIENTED_EDGE ( 'NONE', *, *, #53019, .F. ) ;
#24247 = DIRECTION ( 'NONE',  ( -0.000000000000000000, -0.000000000000000000, 1.000000000000000000 ) ) ;
#24248 = AXIS2_PLACEMENT_3D ( 'NONE', #13890, #8967, #3677 ) ;
#24249 = CARTESIAN_POINT ( 'NONE',  ( 149.9683128897950155, 53.28564708287393614, -69.93847851234227164 ) ) ;
#24250 = CARTESIAN_POINT ( 'NONE',  ( -37.38781680082738745, 10.64362327909142714, 33.12268043286852759 ) ) ;
#24251 = CARTESIAN_POINT ( 'NONE',  ( -26.49516976694650339, 8.831756547364859600, 70.22208721445005608 ) ) ;
#24252 = EDGE_CURVE ( 'NONE', #12094, #50931, #41622, .T. ) ;
#24253 = EDGE_CURVE ( 'NONE', #62112, #168, #35374, .T. ) ;
#24254 = EDGE_LOOP ( 'NONE', ( #19158, #58420, #25715, #22881, #17747, #12193 ) ) ;
#24255 = CARTESIAN_POINT ( 'NONE',  ( 830.5071894358213740, 1001.591584617517810, 776.5068267248775555 ) ) ;
#24256 = CARTESIAN_POINT ( 'NONE',  ( -151.2428028786327729, 66.99705074331122034, 57.75589598882568509 ) ) ;
#24257 = CARTESIAN_POINT ( 'NONE',  ( -119.5267374018686724, 42.44190186039717361, 42.11622477189887803 ) ) ;
#24258 = ORIENTED_EDGE ( 'NONE', *, *, #38422, .F. ) ;
#24259 = CARTESIAN_POINT ( 'NONE',  ( -737.6000277536880958, -694.2189502691659300, 10.00000000000000000 ) ) ;
#24260 = CARTESIAN_POINT ( 'NONE',  ( 93.32502112557678231, 21.81526022999040038, 60.64118160440343530 ) ) ;
#24261 = DIRECTION ( 'NONE',  ( 0.000000000000000000, 0.000000000000000000, -1.000000000000000000 ) ) ;
#24262 = CARTESIAN_POINT ( 'NONE',  ( -118.3960663196801022, 41.75130200162921312, -69.82620201183787856 ) ) ;
#24263 = ORIENTED_EDGE ( 'NONE', *, *, #22647, .T. ) ;
#24264 = CARTESIAN_POINT ( 'NONE',  ( 163.1265310614426483, 62.18610413911354584, -21.71095227450152620 ) ) ;
#24265 = DIRECTION ( 'NONE',  ( 0.000000000000000000, 0.000000000000000000, 1.000000000000000000 ) ) ;
#24266 = CARTESIAN_POINT ( 'NONE',  ( 64.69649025047540647, 13.06878919510321957, 56.84423949185725178 ) ) ;
#24267 = CARTESIAN_POINT ( 'NONE',  ( 140.2200249818743885, 46.60103563593123255, 6.187895880381468317 ) ) ;
#24268 = LINE ( 'NONE', #46742, #2701 ) ;
#24269 = VERTEX_POINT ( 'NONE', #51147 ) ;
#24270 = CARTESIAN_POINT ( 'NONE',  ( 163.7379901688712778, 64.00402364591245430, -12.65244977937952875 ) ) ;
#24271 = CARTESIAN_POINT ( 'NONE',  ( 73.51344971438123821, 14.61114034329559352, 41.38025477438755928 ) ) ;
#24272 = EDGE_LOOP ( 'NONE', ( #42846, #22520, #44832, #67309 ) ) ;
#24273 = VECTOR ( 'NONE', #10678, 1000.000000000000000 ) ;
#24274 = CARTESIAN_POINT ( 'NONE',  ( 66.30230369578303851, 14.49551544185124818, 57.41158669744056908 ) ) ;
#24275 = CARTESIAN_POINT ( 'NONE',  ( 126.6419157458061022, 37.23544530986323053, 92.77959788058313961 ) ) ;
#24276 = B_SPLINE_CURVE_WITH_KNOTS ( 'NONE', 3,
 ( #16681, #5775, #38135, #11392, #37104, #153, #58545, #43406, #32867, #26554, #37794, #59932, #54299, #58893, #27582, #32516, #48666, #33229, #54659, #507, #49021, #861, #65225, #42720, #38489, #22314, #26892, #53613, #17017, #10363, #53263, #69453, #11750, #20928, #6487, #47988, #64177, #48320, #21611, #15990, #27934, #11056, #37438, #63847 ),
 .UNSPECIFIED., .F., .F.,
 ( 4, 2, 2, 2, 2, 2, 2, 2, 2, 2, 2, 2, 2, 2, 2, 2, 2, 2, 2, 2, 2, 4 ),
 ( 7.152448122690996019E-18, 0.001476829494128784797, 0.002215244241193187278, 0.002953658988257589543, 0.004430488482386393638, 0.005907317976515197300, 0.007384147470644000961, 0.008122562217708420573, 0.008860976964772839318, 0.01033780645890166987, 0.01181463595303050042, 0.01255305070009489314, 0.01329146544715928933, 0.01476829494128811815, 0.01550670968835254557, 0.01624512443541697645, 0.01772195392954585905, 0.01919878342367474511, 0.01993719817073917946, 0.02067561291780361729, 0.02215244241193247560, 0.02362927190606133043 ),
 .UNSPECIFIED. ) ;
#24277 = ORIENTED_EDGE ( 'NONE', *, *, #15775, .F. ) ;
#24278 = CARTESIAN_POINT ( 'NONE',  ( 162.0812592823604916, 62.62783216273700049, -37.68953501586388910 ) ) ;
#24279 = DIRECTION ( 'NONE',  ( 0.000000000000000000, 0.000000000000000000, -1.000000000000000000 ) ) ;
#24280 = LINE ( 'NONE', #61890, #23686 ) ;
#24281 = LINE ( 'NONE', #51008, #57522 ) ;
#24282 = VECTOR ( 'NONE', #19999, 1000.000000000000000 ) ;
#24283 = CIRCLE ( 'NONE', #17527, 27.00000000000000000 ) ;
#24284 = ORIENTED_EDGE ( 'NONE', *, *, #5851, .F. ) ;
#24285 = PRODUCT_DEFINITION_FORMATION_WITH_SPECIFIED_SOURCE ( 'ANY', '', #67620, .NOT_KNOWN. ) ;
#24286 = CARTESIAN_POINT ( 'NONE',  ( 0.000000000000000000, 2.755455298081544778E-15, -22.50000000000000000 ) ) ;
#24287 = VECTOR ( 'NONE', #35264, 1000.000000000000000 ) ;
#24288 = CARTESIAN_POINT ( 'NONE',  ( 230.9999999999999432, 192.0000000000000000, 380.0000000000000000 ) ) ;
#24289 = B_SPLINE_CURVE_WITH_KNOTS ( 'NONE', 3,
 ( #45238, #50174, #7272, #3036, #1638, #28725, #2003, #23459, #34361, #7627, #18516, #56845, #42037, #31486, #36769, #41694, #19901, #68759, #67748, #46972, #20572, #36075, #30450, #8661, #63154, #57875, #41009, #30801, #46623, #14615, #68098, #14278, #69101, #20235, #3376, #68430 ),
 .UNSPECIFIED., .F., .F.,
 ( 4, 2, 2, 2, 2, 2, 2, 2, 2, 2, 2, 2, 2, 2, 2, 2, 2, 4 ),
 ( 0.02352539391595309323, 0.02450549414544716739, 0.02548559437494124155, 0.02646569460443531571, 0.02744579483392938987, 0.02842589506342346750, 0.02940599529291754166, 0.03038609552241161235, 0.03136619575190568998, 0.03234629598139976414, 0.03332639621089383830, 0.03430649644038791246, 0.03528659666988198662, 0.03626669689937606078, 0.03724679712887013494, 0.03773684724361715120, 0.03822689735836416747, 0.03920699758785820693 ),
 .UNSPECIFIED. ) ;
#24290 = CARTESIAN_POINT ( 'NONE',  ( -450.6627218934913230, 217.8591479523843475, -111.4497041420117966 ) ) ;
#24291 = AXIS2_PLACEMENT_3D ( 'NONE', #58030, #53765, #42864 ) ;
#24292 = DIRECTION ( 'NONE',  ( 0.000000000000000000, -0.7071067811865474617, 0.7071067811865474617 ) ) ;
#24293 = CARTESIAN_POINT ( 'NONE',  ( -149.5074843970971017, 64.17983161892348676, -61.65738112195564469 ) ) ;
#24294 = CARTESIAN_POINT ( 'NONE',  ( -144.5499722824449691, 60.08555854030711174, -90.35693536357965172 ) ) ;
#24295 = CARTESIAN_POINT ( 'NONE',  ( 127.4750938923429402, 37.70245908594341699, -74.31642906583816455 ) ) ;
#24296 = ORIENTED_EDGE ( 'NONE', *, *, #3724, .F. ) ;
#24297 = CARTESIAN_POINT ( 'NONE',  ( -95.04371414958066566, 30.36527049547257562, 62.82467735017532817 ) ) ;
#24298 = CARTESIAN_POINT ( 'NONE',  ( -7.825402957745081878, 7.899365992529270741, 56.96013162991089018 ) ) ;
#24299 = ORIENTED_EDGE ( 'NONE', *, *, #133, .T. ) ;
#24300 = CARTESIAN_POINT ( 'NONE',  ( -156.6862310659955142, 71.88416263379565407, -40.06925897084124699 ) ) ;
#24301 = EDGE_CURVE ( 'NONE', #42183, #30648, #41967, .T. ) ;
#24302 = PLANE ( 'NONE',  #33156 ) ;
#24303 = CARTESIAN_POINT ( 'NONE',  ( -430.1627218934915504, 394.9999999999998295, -123.9497041420119530 ) ) ;
#24304 = CARTESIAN_POINT ( 'NONE',  ( -154.6171773099879658, 68.63761944777706958, -63.66210952773269582 ) ) ;
#24305 = CARTESIAN_POINT ( 'NONE',  ( 55.50964472539083516, 11.05611641653240440, 90.85181882182600077 ) ) ;
#24306 = B_SPLINE_CURVE_WITH_KNOTS ( 'NONE', 3,
 ( #40245, #49732, #29010, #12826, #12466, #34280, #61351, #55729, #33931, #66642, #45163, #24069, #23720, #18439, #54667, #44827, #45513, #60303, #18786, #27941, #39893, #66309, #13172, #29339, #6836, #49384, #34638, #7190, #39208, #56075, #44108, #55015, #28291, #7892, #1561, #50791, #65954, #17752, #62390, #14204, #19125, #35662, #40930, #68023, #52519, #31082 ),
 .UNSPECIFIED., .F., .F.,
 ( 4, 2, 2, 2, 2, 2, 2, 2, 2, 2, 2, 2, 2, 2, 2, 2, 2, 2, 2, 2, 2, 2, 4 ),
 ( 0.02989107162308296539, 0.03170280136394040132, 0.03351453110479783726, 0.03532626084565526625, 0.03713799058651270218, 0.03894972032737013812, 0.03985558519779883180, 0.04076145006822753242, 0.04166731493865623304, 0.04257317980908492672, 0.04347904467951362040, 0.04438490954994231408, 0.04529077442037101470, 0.04619663929079970838, 0.04710250416122840206, 0.04800836903165709574, 0.04891423390208579636, 0.04982009877251449004, 0.05163182851337182189, 0.05344355825422915374, 0.05525528799508648559, 0.05706701773594381744, 0.05887874747680114235 ),
 .UNSPECIFIED. ) ;
#24307 = CARTESIAN_POINT ( 'NONE',  ( -53.38256734720888375, 14.24001356352780334, -76.87654361394403679 ) ) ;
#24308 = CARTESIAN_POINT ( 'NONE',  ( -4.502148936856955608, 7.704491846230413721, -9.332046380200495150 ) ) ;
#24309 = EDGE_CURVE ( 'NONE', #29362, #44986, #57802, .T. ) ;
#24310 = CARTESIAN_POINT ( 'NONE',  ( 173.5843421840238250, 71.34465141434343138, 10.26728517241832250 ) ) ;
#24311 = CARTESIAN_POINT ( 'NONE',  ( -62.56514071794336473, 16.82532503654673306, 10.98024456806455618 ) ) ;
#24312 = ORIENTED_EDGE ( 'NONE', *, *, #35735, .F. ) ;
#24313 = CARTESIAN_POINT ( 'NONE',  ( 198.7765072002625288, 100.1872738704526427, 94.99999999999866418 ) ) ;
#24315 = ORIENTED_EDGE ( 'NONE', *, *, #43666, .T. ) ;
#24314 = ADVANCED_FACE ( 'NONE', ( #58147 ), #44339, .T. ) ;
#24316 = CARTESIAN_POINT ( 'NONE',  ( 105.4193882736796297, 26.71329717705292239, -76.03135858187803819 ) ) ;
#24317 = CARTESIAN_POINT ( 'NONE',  ( 46.12582897016703498, 10.39833982076227414, -12.94356353922558611 ) ) ;
#24318 = CARTESIAN_POINT ( 'NONE',  ( 43.96465529479667111, 9.046527005589350523, 58.28554417598712689 ) ) ;
#24319 = LINE ( 'NONE', #55973, #32361 ) ;
#24320 = EDGE_CURVE ( 'NONE', #49272, #44530, #83, .T. ) ;
#24321 = DIRECTION ( 'NONE',  ( -1.000000000000000000, 0.000000000000000000, 0.000000000000000000 ) ) ;
#24322 = DIRECTION ( 'NONE',  ( 0.000000000000000000, 0.000000000000000000, -1.000000000000000000 ) ) ;
#24323 = CARTESIAN_POINT ( 'NONE',  ( 7.533997733929801655, -64.93035244659006366, 6.377659838150150565E-18 ) ) ;
#24324 = PLANE ( 'NONE',  #57730 ) ;
#24325 = EDGE_LOOP ( 'NONE', ( #9113, #54378 ) ) ;
#24326 = ORIENTED_EDGE ( 'NONE', *, *, #54042, .T. ) ;
#24327 = FACE_OUTER_BOUND ( 'NONE', #63524, .T. ) ;
#24328 = CARTESIAN_POINT ( 'NONE',  ( 0.000000000000000000, 0.000000000000000000, 170.0000000000000000 ) ) ;
#24329 = CARTESIAN_POINT ( 'NONE',  ( 180.6710448012268273, 78.18844465372406205, -24.38050707541595230 ) ) ;
#24330 = CONICAL_SURFACE ( 'NONE', #45706, 74.95140232871122521, 0.8777644062502172329 ) ;
#24331 = CARTESIAN_POINT ( 'NONE',  ( 103.5589117581614715, 27.00490790413961761, 67.39597877340914067 ) ) ;
#24332 = DIRECTION ( 'NONE',  ( -0.000000000000000000, 1.000000000000000000, -0.000000000000000000 ) ) ;
#24333 = EDGE_CURVE ( 'NONE', #5466, #56882, #3239, .T. ) ;
#24334 = AXIS2_PLACEMENT_3D ( 'NONE', #25188, #25534, #15652 ) ;
#24335 = CARTESIAN_POINT ( 'NONE',  ( -84.49322488516129681, 0.000000000000000000, 43.58025477438756212 ) ) ;
#24336 = VERTEX_POINT ( 'NONE', #42981 ) ;
#24337 = CARTESIAN_POINT ( 'NONE',  ( -2.374459999240197572, -25.00999262126968148, 0.000000000000000000 ) ) ;
#24338 = CARTESIAN_POINT ( 'NONE',  ( 280.0000000000000000, -22.00000000000000000, 0.000000000000000000 ) ) ;
#24339 = CARTESIAN_POINT ( 'NONE',  ( -63.33140416796853600, 16.18162651919395500, 41.38025477438755928 ) ) ;
#24340 = CARTESIAN_POINT ( 'NONE',  ( 0.000000000000000000, 0.000000000000000000, 0.000000000000000000 ) ) ;
#24341 = FACE_BOUND ( 'NONE', #39931, .T. ) ;
#24342 = ORIENTED_EDGE ( 'NONE', *, *, #64407, .T. ) ;
#24343 = VECTOR ( 'NONE', #52421, 1000.000000000000000 ) ;
#24344 = ORIENTED_EDGE ( 'NONE', *, *, #48961, .F. ) ;
#24345 = ORIENTED_EDGE ( 'NONE', *, *, #2568, .F. ) ;
#24346 = CARTESIAN_POINT ( 'NONE',  ( 442.3372781065086201, 395.0000000000043201, 108.5502958579839117 ) ) ;
#24347 = DIRECTION ( 'NONE',  ( 1.000000000000000000, 0.000000000000000000, 0.000000000000000000 ) ) ;
#24348 = DIRECTION ( 'NONE',  ( 0.000000000000000000, 1.000000000000000000, -0.000000000000000000 ) ) ;
#24349 = DIRECTION ( 'NONE',  ( 0.000000000000000000, 0.000000000000000000, 1.000000000000000000 ) ) ;
#24350 = CARTESIAN_POINT ( 'NONE',  ( 8.306098662352679796, 6.376413070772140479, 90.59040921272263347 ) ) ;
#24351 = CARTESIAN_POINT ( 'NONE',  ( 22.93737758745371735, 9.943676855699235873, 0.000000000000000000 ) ) ;
#24352 = VERTEX_POINT ( 'NONE', #432 ) ;
#24353 = LINE ( 'NONE', #3240, #33711 ) ;
#24354 = CARTESIAN_POINT ( 'NONE',  ( -125.8938041572051389, 47.69968343338778283, -49.91370389823397602 ) ) ;
#24355 = ORIENTED_EDGE ( 'NONE', *, *, #43049, .F. ) ;
#24356 = LINE ( 'NONE', #34908, #13773 ) ;
#24357 = ORIENTED_EDGE ( 'NONE', *, *, #8082, .F. ) ;
#24358 = CARTESIAN_POINT ( 'NONE',  ( -86.15441609607630369, 25.31657638323078530, -69.95505817415272531 ) ) ;
#24359 = CARTESIAN_POINT ( 'NONE',  ( -18.24318075359455804, -17.27206262134411574, 0.000000000000000000 ) ) ;
#24360 = CARTESIAN_POINT ( 'NONE',  ( 86.62931800182293784, 20.48449268398423939, -77.66611478937542756 ) ) ;
#24361 = VERTEX_POINT ( 'NONE', #52847 ) ;
#24362 = ORIENTED_EDGE ( 'NONE', *, *, #59441, .T. ) ;
#24363 = CARTESIAN_POINT ( 'NONE',  ( 46.12611922993085045, 10.39838587005582227, 60.92721693493930246 ) ) ;
#24364 = FACE_OUTER_BOUND ( 'NONE', #48427, .T. ) ;
#24365 = CARTESIAN_POINT ( 'NONE',  ( 23.28869764673362397, 6.856674305776598644, 11.15851683978236686 ) ) ;
#24366 = EDGE_LOOP ( 'NONE', ( #52374, #22691, #49672, #40852, #8031, #28977 ) ) ;
#24367 = EDGE_CURVE ( 'NONE', #29979, #58622, #42313, .T. ) ;
#24368 = PRODUCT_DEFINITION_SHAPE ( 'NONE', 'NONE',  #69583 ) ;
#24369 = AXIS2_PLACEMENT_3D ( 'NONE', #13233, #68003, #35981 ) ;
#24370 = LINE ( 'NONE', #45814, #47745 ) ;
#24371 = FACE_OUTER_BOUND ( 'NONE', #48789, .T. ) ;
#24372 = CARTESIAN_POINT ( 'NONE',  ( 114.6632852039171127, 30.98120524556723510, -22.64169526929315879 ) ) ;
#24373 = CARTESIAN_POINT ( 'NONE',  ( 80.71682498289317209, 18.54204664833076421, -38.68071917220413525 ) ) ;
#24374 = AXIS2_PLACEMENT_3D ( 'NONE', #37539, #48084, #9098 ) ;
#24376 = EDGE_LOOP ( 'NONE', ( #8826, #12180 ) ) ;
#24375 = CARTESIAN_POINT ( 'NONE',  ( -170.0946319916217533, 85.30045104993550353, -89.02616900977504599 ) ) ;
#24377 = ORIENTED_EDGE ( 'NONE', *, *, #28757, .T. ) ;
#24378 = ORIENTED_EDGE ( 'NONE', *, *, #24864, .F. ) ;
#24379 = CARTESIAN_POINT ( 'NONE',  ( 0.3173508448886507294, -5.375634714784613521, 6.689127551062007626 ) ) ;
#24380 = LINE ( 'NONE', #13806, #6866 ) ;
#24381 = CARTESIAN_POINT ( 'NONE',  ( -51.99406906667273631, 13.88268392809765572, -9.019565312798222934 ) ) ;
#24382 = DIRECTION ( 'NONE',  ( 0.000000000000000000, 0.000000000000000000, 1.000000000000000000 ) ) ;
#24383 = AXIS2_PLACEMENT_3D ( 'NONE', #16842, #11216, #32683 ) ;
#24384 = FACE_OUTER_BOUND ( 'NONE', #14453, .T. ) ;
#24385 = CARTESIAN_POINT ( 'NONE',  ( -27.04746142609647208, 8.911459164085380635, -90.41129225940227343 ) ) ;
#24386 = CARTESIAN_POINT ( 'NONE',  ( 212.1956890233897752, 119.0847181231351470, 90.11100298095867345 ) ) ;
#24387 = ADVANCED_FACE ( 'NONE', ( #9964 ), #43330, .F. ) ;
#24388 = DIRECTION ( 'NONE',  ( 0.3090169943749447312, 0.9510565162951544194, -0.000000000000000000 ) ) ;
#24389 = CARTESIAN_POINT ( 'NONE',  ( -75.43044859198181484, 21.11535168543635876, -62.68972544619923326 ) ) ;
#24390 = CARTESIAN_POINT ( 'NONE',  ( -11.57808265946729875, 7.164483090579920166, 31.11728607544860381 ) ) ;
#24391 = EDGE_LOOP ( 'NONE', ( #43584, #6336, #32989, #19554 ) ) ;
#24392 = AXIS2_PLACEMENT_3D ( 'NONE', #6619, #65371, #6263 ) ;
#24393 = CARTESIAN_POINT ( 'NONE',  ( -450.6627218934913230, 177.8591479523843475, 78.55029585798814651 ) ) ;
#24394 = VERTEX_POINT ( 'NONE', #11324 ) ;
#24395 = ORIENTED_EDGE ( 'NONE', *, *, #30475, .F. ) ;
#24396 = B_SPLINE_CURVE_WITH_KNOTS ( 'NONE', 3,
 ( #62125, #35057, #25210, #67419, #13262, #46988, #41024, #46641, #67768, #57206, #19922, #30824, #67092, #56865, #19214, #51920, #68117, #40670, #41378, #45608, #34723, #56502, #14298, #8684, #40329, #62481, #8333, #25555, #62833, #14634, #18533, #50882, #39985, #56161, #29430, #37121, #59259, #58563 ),
 .UNSPECIFIED., .F., .F.,
 ( 4, 2, 2, 2, 2, 2, 2, 2, 2, 2, 2, 2, 2, 2, 2, 2, 2, 2, 4 ),
 ( 0.02546424207107603199, 0.02703543426729210220, 0.02782103036540017199, 0.02860662646350824179, 0.03017781865972445424, 0.03174901085594066669, 0.03332020305215688261, 0.03489139524837309159, 0.03646258744458930751, 0.03724818354269739118, 0.03803377964080548179, 0.03881937573891357240, 0.03960497183702166302, 0.04117616403323783036, 0.04274735622945401159, 0.04431854842567018588, 0.04588974062188636016, 0.04746093281810253445, 0.05060331721053489690 ),
 .UNSPECIFIED. ) ;
#24397 = DIRECTION ( 'NONE',  ( -0.000000000000000000, -0.000000000000000000, -1.000000000000000000 ) ) ;
#24398 = CARTESIAN_POINT ( 'NONE',  ( 187.5165082312810227, 86.85340440641661530, -74.43517852492631448 ) ) ;
#24399 = CARTESIAN_POINT ( 'NONE',  ( -165.6215009671260816, 80.58889799860443759, 38.63580300477691765 ) ) ;
#24400 = EDGE_CURVE ( 'NONE', #26725, #67396, #25299, .T. ) ;
#24401 = FACE_OUTER_BOUND ( 'NONE', #39768, .T. ) ;
#24402 = CARTESIAN_POINT ( 'NONE',  ( -24.60892750534350171, 9.584951112520226246, 7.763877395040260865 ) ) ;
#24403 = LINE ( 'NONE', #19810, #12476 ) ;
#24404 = CARTESIAN_POINT ( 'NONE',  ( 11.82929895397813524, 7.412564870773604930, -49.39369728624853195 ) ) ;
#24405 = CARTESIAN_POINT ( 'NONE',  ( 126.3737790127712515, 37.08609730334947585, -42.95235691801180167 ) ) ;
#24406 = EDGE_LOOP ( 'NONE', ( #56399, #47709, #2848 ) ) ;
#24407 = ORIENTED_EDGE ( 'NONE', *, *, #61876, .T. ) ;
#24408 = CARTESIAN_POINT ( 'NONE',  ( 8.942470798084380945, -23.47701018505899739, 3.061616997868437868E-16 ) ) ;
#24409 = CARTESIAN_POINT ( 'NONE',  ( -8.314575874103551811, 6.922894809783095127, 3.271030448983516692 ) ) ;
#24410 = FACE_OUTER_BOUND ( 'NONE', #62347, .T. ) ;
#24411 = CARTESIAN_POINT ( 'NONE',  ( -13.32397999418070533, 63.99361958670518646, 41.38025477438755928 ) ) ;
#24412 = ADVANCED_FACE ( 'NONE', ( #15235 ), #47570, .F. ) ;
#24413 = ADVANCED_FACE ( 'NONE', ( #38066 ), #63775, .F. ) ;
#24414 = CARTESIAN_POINT ( 'NONE',  ( 9.290502160020464473, 6.379616279862540651, 6.916542375528051956 ) ) ;
#24415 = EDGE_CURVE ( 'NONE', #60658, #42281, #30856, .T. ) ;
#24416 = VERTEX_POINT ( 'NONE', #20854 ) ;
#24417 = CARTESIAN_POINT ( 'NONE',  ( -46.66904755831212981, -10.55634918610397222, 85.00100000000000477 ) ) ;
#24418 = CARTESIAN_POINT ( 'NONE',  ( -62.06231780744543869, 17.72446026058425517, -66.88159662817442097 ) ) ;
#24419 = DIRECTION ( 'NONE',  ( -0.000000000000000000, -0.000000000000000000, -1.000000000000000000 ) ) ;
#24420 = AXIS2_PLACEMENT_3D ( 'NONE', #22857, #18628, #7030 ) ;
#24421 = CARTESIAN_POINT ( 'NONE',  ( -178.2381786520593892, 93.01028335822118720, -36.72343023615520963 ) ) ;
#24422 = CARTESIAN_POINT ( 'NONE',  ( 9.962235950565768050, -64.23203137738408941, 40.00000000000003553 ) ) ;
#24423 = CARTESIAN_POINT ( 'NONE',  ( 8.000000000000007105, 249.8719672152120381, 94.99999999999866418 ) ) ;
#24424 = CARTESIAN_POINT ( 'NONE',  ( 110.0000000000000284, 21.42428528562853174, 5.000000000000004441 ) ) ;
#24425 = CARTESIAN_POINT ( 'NONE',  ( -48.32993240732259466, 12.98137013984324817, 68.02384498338118135 ) ) ;
#24426 = AXIS2_PLACEMENT_3D ( 'NONE', #28898, #60195, #2508 ) ;
#24427 = B_SPLINE_CURVE_WITH_KNOTS ( 'NONE', 3,
 ( #36671, #10609, #9592, #5347 ),
 .UNSPECIFIED., .F., .F.,
 ( 4, 4 ),
 ( 0.1259919275528360305, 0.1829744153748752156 ),
 .UNSPECIFIED. ) ;
#24428 = CARTESIAN_POINT ( 'NONE',  ( -0.5751131641471390887, 6.527254166626920373, 66.39501694792768660 ) ) ;
#24429 = ORIENTED_EDGE ( 'NONE', *, *, #38176, .F. ) ;
#24430 = CIRCLE ( 'NONE', #1982, 5.000000000000018652 ) ;
#24431 = CARTESIAN_POINT ( 'NONE',  ( 275.1608908971991809, 21.96390383200032304, -1.300086469598740635 ) ) ;
#24432 = DIRECTION ( 'NONE',  ( 1.000000000000000000, -0.000000000000000000, -0.000000000000000000 ) ) ;
#24433 = DIRECTION ( 'NONE',  ( 0.000000000000000000, 0.000000000000000000, -1.000000000000000000 ) ) ;
#24434 = CARTESIAN_POINT ( 'NONE',  ( -50.14771795543004629, 13.42081263859818030, -48.41097516278959034 ) ) ;
#24435 = DIRECTION ( 'NONE',  ( -0.000000000000000000, -0.000000000000000000, -1.000000000000000000 ) ) ;
#24436 = DIRECTION ( 'NONE',  ( 0.000000000000000000, -0.000000000000000000, 1.000000000000000000 ) ) ;
#24437 = VECTOR ( 'NONE', #17503, 1000.000000000000000 ) ;
#24438 = AXIS2_PLACEMENT_3D ( 'NONE', #1787, #60514, #7046 ) ;
#24439 = ORIENTED_EDGE ( 'NONE', *, *, #18267, .F. ) ;
#24440 =( NAMED_UNIT ( * ) SI_UNIT ( $, .STERADIAN. ) SOLID_ANGLE_UNIT ( ) );
#24441 = CARTESIAN_POINT ( 'NONE',  ( -4.339467034331206285, -6.732211846623409102, -6.390228312323252966E-15 ) ) ;
#24442 = ORIENTED_EDGE ( 'NONE', *, *, #52416, .F. ) ;
#24443 = EDGE_LOOP ( 'NONE', ( #30489, #33331, #68676, #36266, #18924, #26155, #42329, #40409, #63348 ) ) ;
#24444 = FACE_OUTER_BOUND ( 'NONE', #16527, .T. ) ;
#24445 = CARTESIAN_POINT ( 'NONE',  ( 149.9714610887121466, 53.28792066194168342, 36.60205868149071762 ) ) ;
#24446 = DIRECTION ( 'NONE',  ( 0.5128992774058949156, 0.8584487936018728726, 2.500042656554809354E-16 ) ) ;
#24447 = VERTEX_POINT ( 'NONE', #59508 ) ;
#24448 = PLANE ( 'NONE',  #63772 ) ;
#24449 = CARTESIAN_POINT ( 'NONE',  ( -180.6009936245623635, 95.85948119829090786, 12.10851691733632407 ) ) ;
#24450 = CARTESIAN_POINT ( 'NONE',  ( -4.504169684898447379, 6.697401007565304099, 17.50005462738863926 ) ) ;
#24451 = CARTESIAN_POINT ( 'NONE',  ( 55.99998955208978657, 12.18058389017405396, -40.55750410589438104 ) ) ;
#24452 = CARTESIAN_POINT ( 'NONE',  ( -85.73740570227381852, 26.23277384689409431, 35.40511533989044324 ) ) ;
#24453 = CARTESIAN_POINT ( 'NONE',  ( 156.0703099390621276, 56.57038975554689131, 83.22409554701557965 ) ) ;
#24454 = CARTESIAN_POINT ( 'NONE',  ( 138.2204650371259333, 44.12203217345473405, 16.28412638663770196 ) ) ;
#24455 = EDGE_CURVE ( 'NONE', #62594, #40284, #69385, .T. ) ;
#24456 = ORIENTED_EDGE ( 'NONE', *, *, #45675, .T. ) ;
#24458 = EDGE_CURVE ( 'NONE', #56740, #35856, #63659, .T. ) ;
#24457 = CARTESIAN_POINT ( 'NONE',  ( -3.566018963826330879, 51.54211443464424036, 26.66469066592269144 ) ) ;
#24459 = LINE ( 'NONE', #60339, #8953 ) ;
#24460 = CARTESIAN_POINT ( 'NONE',  ( 43.14712943604300932, 8.926114770663666320, -36.61723071961753817 ) ) ;
#24461 = DIRECTION ( 'NONE',  ( 1.000000000000000000, 0.000000000000000000, 0.000000000000000000 ) ) ;
#24463 = VERTEX_POINT ( 'NONE', #7467 ) ;
#24462 = DIRECTION ( 'NONE',  ( -0.000000000000000000, 1.000000000000000000, -0.000000000000000000 ) ) ;
#24464 = DIRECTION ( 'NONE',  ( 1.000000000000000000, 0.000000000000000000, 0.000000000000000000 ) ) ;
#24465 = EDGE_LOOP ( 'NONE', ( #15103, #38057 ) ) ;
#24466 = CARTESIAN_POINT ( 'NONE',  ( -143.3925773749112409, 59.16144459815140522, 69.41541250540224439 ) ) ;
#24467 = VECTOR ( 'NONE', #1239, 1000.000000000000114 ) ;
#24468 = CARTESIAN_POINT ( 'NONE',  ( 82.12277968641507186, 18.98848723477812683, 43.22702714516130840 ) ) ;
#24469 = CARTESIAN_POINT ( 'NONE',  ( -63.33140416796830152, -16.18162651919485384, 6.377659838150159810E-18 ) ) ;
#24470 = ADVANCED_FACE ( 'NONE', ( #17303 ), #23300, .T. ) ;
#24471 = CARTESIAN_POINT ( 'NONE',  ( 182.7789203043889188, 80.33475476315291530, -9.562155104270011918 ) ) ;
#24472 = EDGE_CURVE ( 'NONE', #52352, #58078, #28920, .T. ) ;
#24473 =( BOUNDED_CURVE ( )  B_SPLINE_CURVE ( 3, ( #20857, #26486, #52849, #63430 ),
 .UNSPECIFIED., .F., .F. ) 
 B_SPLINE_CURVE_WITH_KNOTS ( ( 4, 4 ),
 ( 1.570796326794897224, 3.141592653589780237 ),
 .UNSPECIFIED. ) 
 CURVE ( )  GEOMETRIC_REPRESENTATION_ITEM ( )  RATIONAL_B_SPLINE_CURVE ( ( 1.000000000000000000, 0.8047378541243681571, 0.8047378541243681571, 1.000000000000000000 ) ) 
 REPRESENTATION_ITEM ( '' )  );
#24474 = CARTESIAN_POINT ( 'NONE',  ( -120.4816138481825050, 43.03185659245511374, 59.74961932001716747 ) ) ;
#24475 = VECTOR ( 'NONE', #49462, 1000.000000000000000 ) ;
#24476 = CARTESIAN_POINT ( 'NONE',  ( -79.61235761536670452, 23.76245710489567742, -23.22627702482678913 ) ) ;
#24477 = CARTESIAN_POINT ( 'NONE',  ( -180.5234362879040191, 97.35934147644938719, -14.11989895273327456 ) ) ;
#24478 = CARTESIAN_POINT ( 'NONE',  ( -47.61402178322637724, 13.84598486314981791, 36.82852865596623104 ) ) ;
#24479 = ORIENTED_EDGE ( 'NONE', *, *, #3959, .T. ) ;
#24480 = ORIENTED_EDGE ( 'NONE', *, *, #48539, .F. ) ;
#24481 = EDGE_CURVE ( 'NONE', #37440, #26997, #55284, .T. ) ;
#24482 = VECTOR ( 'NONE', #7901, 1000.000000000000000 ) ;
#24483 = DIRECTION ( 'NONE',  ( 0.000000000000000000, 0.000000000000000000, 1.000000000000000000 ) ) ;
#24484 = CARTESIAN_POINT ( 'NONE',  ( 104.3931729003987243, 26.26823401847089912, 68.67546489303082069 ) ) ;
#24485 = DIRECTION ( 'NONE',  ( 0.000000000000000000, 0.000000000000000000, -1.000000000000000000 ) ) ;
#24486 = EDGE_CURVE ( 'NONE', #17220, #10774, #9513, .T. ) ;
#24487 = DIRECTION ( 'NONE',  ( 0.000000000000000000, 0.000000000000000000, 1.000000000000000000 ) ) ;
#24488 = VECTOR ( 'NONE', #5990, 999.9999999999998863 ) ;
#24489 = CARTESIAN_POINT ( 'NONE',  ( -452.6627218934913230, 399.9999999999997726, 113.5502958579881891 ) ) ;
#24490 = LINE ( 'NONE', #67394, #13506 ) ;
#24491 = CARTESIAN_POINT ( 'NONE',  ( -142.0273276822220794, 59.36478176800545725, 91.25952348669476066 ) ) ;
#24492 = ORIENTED_EDGE ( 'NONE', *, *, #12873, .F. ) ;
#24493 = VERTEX_POINT ( 'NONE', #59857 ) ;
#24494 = VERTEX_POINT ( 'NONE', #27859 ) ;
#24495 = AXIS2_PLACEMENT_3D ( 'NONE', #22377, #59999, #6894 ) ;
#24496 = CARTESIAN_POINT ( 'NONE',  ( 15.55634918610411610, 46.66904755831205875, 2.000000000000001776 ) ) ;
#24497 = CARTESIAN_POINT ( 'NONE',  ( 70.34686579112809568, 18.11777090454216577, 170.0000000000000000 ) ) ;
#24498 = CARTESIAN_POINT ( 'NONE',  ( 68.45098769362918745, 13.99935947269948500, -48.39431334976815435 ) ) ;
#24499 = DIRECTION ( 'NONE',  ( 0.5407162030609374836, -0.6444004775717707689, 0.5407162030609373726 ) ) ;
#24500 = CARTESIAN_POINT ( 'NONE',  ( -61.53550548562873246, 17.56596194025584978, 41.62090751969812885 ) ) ;
#24501 = CARTESIAN_POINT ( 'NONE',  ( -74.81012118577224612, 5.477980300262961677, 170.0000000000000000 ) ) ;
#24502 = EDGE_CURVE ( 'NONE', #46532, #39310, #55995, .T. ) ;
#24503 = EDGE_CURVE ( 'NONE', #18610, #4596, #18011, .T. ) ;
#24504 = CARTESIAN_POINT ( 'NONE',  ( 35.65685430025424552, 7.951642554322393863, 70.77480580695264223 ) ) ;
#24505 = DIRECTION ( 'NONE',  ( 0.9009688679024218105, -0.4338837391175525693, 0.000000000000000000 ) ) ;
#24506 = VERTEX_POINT ( 'NONE', #60219 ) ;
#24507 = CARTESIAN_POINT ( 'NONE',  ( 20.89850557012432830, 13.94239061780435662, 3.061616997868437868E-16 ) ) ;
#24508 = CARTESIAN_POINT ( 'NONE',  ( 0.000000000000000000, 0.000000000000000000, 10.00000000000000000 ) ) ;
#24510 = EDGE_CURVE ( 'NONE', #14354, #22557, #24185, .T. ) ;
#24509 = CARTESIAN_POINT ( 'NONE',  ( -20.00000000000002842, 3.680555555555560243, 4.000000000000000000 ) ) ;
#24511 = FACE_OUTER_BOUND ( 'NONE', #34400, .T. ) ;
#24512 = CARTESIAN_POINT ( 'NONE',  ( 126.3541873520043737, 37.07520218256170352, -17.17827544387097305 ) ) ;
#24513 = CARTESIAN_POINT ( 'NONE',  ( 23.28809538736928531, 7.864824219997530008, -15.68220158935621988 ) ) ;
#24514 = CARTESIAN_POINT ( 'NONE',  ( -109.3432140528234839, 36.51591785955879743, -66.78469379273217044 ) ) ;
#24515 = B_SPLINE_CURVE_WITH_KNOTS ( 'NONE', 3,
 ( #67426, #52274, #62133, #9368, #13952, #35409, #56874, #51927, #3740, #14643, #30830, #26238, #5800, #42743, #52611, #5462, #31183, #43431, #58919, #57898, #37464, #64909, #64202, #5115, #47671, #10736, #26578, #58571, #69126, #69477, #178, #48015, #10385, #16013, #47327, #25897, #20956, #68785, #31857, #32208, #16703, #15679, #26918 ),
 .UNSPECIFIED., .F., .F.,
 ( 4, 2, 2, 2, 2, 2, 2, 2, 2, 2, 2, 2, 1, 2, 2, 2, 2, 2, 2, 2, 2, 4 ),
 ( 0.02362927190606132349, 0.02510248541563191507, 0.02583909217041720913, 0.02657569892520249971, 0.02804891243477307741, 0.02952212594434365511, 0.03025873269912894223, 0.03099533945391422934, 0.03246855296348480358, 0.03394176647305537087, 0.03541497998262594510, 0.03615158673741123568, 0.03688819349219652627, 0.03762480024698181685, 0.03836140700176710744, 0.03983462051133769555, 0.04130783402090827672, 0.04278104753047885789, 0.04351765428526415541, 0.04425426104004945294, 0.04572747454962003411, 0.04720068805919061528 ),
 .UNSPECIFIED. ) ;
#24516 = ORIENTED_EDGE ( 'NONE', *, *, #18886, .T. ) ;
#24517 = SHAPE_DEFINITION_REPRESENTATION ( #25942, #40274 ) ;
#24518 = DIRECTION ( 'NONE',  ( 0.000000000000000000, 0.5000000000000007772, -0.8660254037844381525 ) ) ;
#24519 = DIRECTION ( 'NONE',  ( -0.000000000000000000, 1.000000000000000000, -0.000000000000000000 ) ) ;
#24520 = CARTESIAN_POINT ( 'NONE',  ( 65.13282190615461786, 1.839221433318906476E-12, -9.999999999999998224 ) ) ;
#24521 = CARTESIAN_POINT ( 'NONE',  ( 0.000000000000000000, 0.000000000000000000, 40.00000000000003553 ) ) ;
#24522 = EDGE_LOOP ( 'NONE', ( #11279, #7803, #48029, #35745 ) ) ;
#24523 = CARTESIAN_POINT ( 'NONE',  ( 126.3732561463888402, 38.23795180971325891, 9.601229107663494133 ) ) ;
#24524 = ORIENTED_EDGE ( 'NONE', *, *, #62082, .F. ) ;
#24525 = FACE_BOUND ( 'NONE', #68964, .T. ) ;
#24526 = FACE_OUTER_BOUND ( 'NONE', #53354, .T. ) ;
#24527 = VERTEX_POINT ( 'NONE', #66562 ) ;
#24528 = AXIS2_PLACEMENT_3D ( 'NONE', #22152, #64359, #37630 ) ;
#24529 = DIRECTION ( 'NONE',  ( 1.000000000000000000, 0.000000000000000000, 0.000000000000000000 ) ) ;
#24530 = ORIENTED_EDGE ( 'NONE', *, *, #49839, .T. ) ;
#24531 = CARTESIAN_POINT ( 'NONE',  ( 131.6115093721025175, 41.25402743071403933, -77.52764994514272701 ) ) ;
#24532 = CARTESIAN_POINT ( 'NONE',  ( 50.97490815085634352, 0.000000000000000000, -9.435653166495500344 ) ) ;
#24533 = AXIS2_PLACEMENT_3D ( 'NONE', #48863, #11246, #22163 ) ;
#24534 = B_SPLINE_CURVE_WITH_KNOTS ( 'NONE', 3,
 ( #12824, #35309, #66640, #2961, #18094, #34636, #30376, #18437, #24421, #51827, #45863, #56768, #34278, #67335, #40928, #19123, #40577, #55727, #62032, #62388, #13170, #35660, #3637, #25112, #66307, #64108, #52845, #14543, #68688, #46544, #10285, #36346, #4667, #57454, #37034, #20502, #57798, #20164, #5367, #41280, #63075, #9266, #31751, #15919, #31080, #62739 ),
 .UNSPECIFIED., .F., .F.,
 ( 4, 2, 2, 2, 2, 2, 2, 2, 2, 2, 2, 2, 2, 2, 2, 2, 2, 2, 2, 2, 2, 2, 4 ),
 ( 0.000000000000000000, 0.003736383952885418379, 0.005604575929328127135, 0.007472767905770836758, 0.008406863893992191569, 0.009340959882213546381, 0.01120915185865624039, 0.01214324784687757092, 0.01307734383509889971, 0.01401143982332023023, 0.01494553581154155902, 0.01587963179976289302, 0.01681372778798422354, 0.01774782377620555407, 0.01868191976442688459, 0.01961601575264821859, 0.02055011174086954912, 0.02148420772909087964, 0.02241830371731221017, 0.02428649569375488856, 0.02615468767019756696, 0.02802287964664024883, 0.02989107162308292723 ),
 .UNSPECIFIED. ) ;
#24535 = CARTESIAN_POINT ( 'NONE',  ( -154.0716379918897019, 69.49957566103795159, 32.25060227376270205 ) ) ;
#24536 = CARTESIAN_POINT ( 'NONE',  ( -15.55634918610405748, -15.55634918610400774, 0.000000000000000000 ) ) ;
#24537 = VECTOR ( 'NONE', #5412, 1000.000000000000000 ) ;
#24538 = CARTESIAN_POINT ( 'NONE',  ( -34.75846525699014933, 54.92585086258208804, 40.00000000000003553 ) ) ;
#24540 = VERTEX_POINT ( 'NONE', #18351 ) ;
#24539 = LINE ( 'NONE', #35778, #60058 ) ;
#24541 = CARTESIAN_POINT ( 'NONE',  ( 56.66438910147191166, 11.28870326331392882, 33.31645525201592051 ) ) ;
#24542 = EDGE_LOOP ( 'NONE', ( #10181, #25657, #68460, #884 ) ) ;
#24543 = ORIENTED_EDGE ( 'NONE', *, *, #22961, .T. ) ;
#24544 = AXIS2_PLACEMENT_3D ( 'NONE', #4319, #14860, #30358 ) ;
#24546 = EDGE_CURVE ( 'NONE', #38709, #43082, #15183, .T. ) ;
#24545 = CARTESIAN_POINT ( 'NONE',  ( -165.7713056973201731, 80.74264649718246289, 12.99982703628925407 ) ) ;
#24547 = FACE_OUTER_BOUND ( 'NONE', #36938, .T. ) ;
#24549 = VERTEX_POINT ( 'NONE', #41802 ) ;
#24548 = CARTESIAN_POINT ( 'NONE',  ( -22.50000000000003197, -18.06806526123148160, 380.0000000000000000 ) ) ;
#24550 = LINE ( 'NONE', #13976, #55542 ) ;
#24551 = CARTESIAN_POINT ( 'NONE',  ( -71.22896441287284119, 20.69091426169408621, -43.61454751274712294 ) ) ;
#24552 = VERTEX_POINT ( 'NONE', #4171 ) ;
#24553 = CARTESIAN_POINT ( 'NONE',  ( 174.7644348140981947, 73.82982812962299590, -93.36945622964188374 ) ) ;
#24554 = EDGE_CURVE ( 'NONE', #17392, #22806, #31251, .T. ) ;
#24555 = CARTESIAN_POINT ( 'NONE',  ( 140.2200249818744453, 46.60103563593123255, 33.03244647084515861 ) ) ;
#24556 = CARTESIAN_POINT ( 'NONE',  ( 116.6681538161788438, 33.09439081574000596, 33.21055421480799197 ) ) ;
#24557 = CARTESIAN_POINT ( 'NONE',  ( -127.6894679065405711, 48.89973668460851997, 18.57123567224974536 ) ) ;
#24558 = EDGE_CURVE ( 'NONE', #15127, #7019, #19699, .T. ) ;
#24559 = CARTESIAN_POINT ( 'NONE',  ( 66.07923263163412742, 14.44036440557998446, -76.91531762281159956 ) ) ;
#24560 = ORIENTED_EDGE ( 'NONE', *, *, #54151, .T. ) ;
#24561 = ADVANCED_FACE ( 'NONE', ( #37201 ), #18706, .T. ) ;
#24562 = ORIENTED_EDGE ( 'NONE', *, *, #65039, .F. ) ;
#24563 = CARTESIAN_POINT ( 'NONE',  ( -147.7925265216585444, 64.04960911618974251, -22.77289545559010264 ) ) ;
#24564 = FACE_OUTER_BOUND ( 'NONE', #39698, .T. ) ;
#24565 = EDGE_CURVE ( 'NONE', #62736, #34240, #68018, .T. ) ;
#24566 = CARTESIAN_POINT ( 'NONE',  ( 0.000000000000000000, 0.000000000000000000, -50.00000000000000000 ) ) ;
#24567 = CARTESIAN_POINT ( 'NONE',  ( 46.57905527587767125, 10.47094344121033060, -94.59163972955721533 ) ) ;
#24568 = CARTESIAN_POINT ( 'NONE',  ( -65.20298343242130557, -4.613322252418190494, 43.58025477438756212 ) ) ;
#24569 = CARTESIAN_POINT ( 'NONE',  ( -145.3279998500303236, 60.71393190715791377, 31.98882707624600030 ) ) ;
#24570 = CARTESIAN_POINT ( 'NONE',  ( -120.6739978760426055, 44.33795494230363943, 43.51089096318784044 ) ) ;
#24571 = CARTESIAN_POINT ( 'NONE',  ( -167.6413528428656150, 81.22881971256914824, -74.20285492933068383 ) ) ;
#24572 = ORIENTED_EDGE ( 'NONE', *, *, #12077, .F. ) ;
#24573 = CARTESIAN_POINT ( 'NONE',  ( -108.9145525555662459, 37.42858360505774584, 34.51211213987539850 ) ) ;
#24574 = ORIENTED_EDGE ( 'NONE', *, *, #34718, .F. ) ;
#24575 = AXIS2_PLACEMENT_3D ( 'NONE', #6759, #1139, #28208 ) ;
#24576 = CARTESIAN_POINT ( 'NONE',  ( -38.69577193929646342, 10.89562623693159615, 8.913580037696034353 ) ) ;
#24577 = LINE ( 'NONE', #13656, #31846 ) ;
#24578 = ORIENTED_EDGE ( 'NONE', *, *, #24455, .F. ) ;
#24579 = CARTESIAN_POINT ( 'NONE',  ( 111.9975424824652634, 296.0000000000000000, 529.9060149868646477 ) ) ;
#24580 = CARTESIAN_POINT ( 'NONE',  ( -189.5325095384513077, 107.4952257375067290, -66.82603086747147358 ) ) ;
#24581 = LINE ( 'NONE', #34783, #29890 ) ;
#24582 = DIRECTION ( 'NONE',  ( 0.000000000000000000, 0.000000000000000000, -1.000000000000000000 ) ) ;
#24583 = CARTESIAN_POINT ( 'NONE',  ( 32.15641333221390852, 7.577415570152256308, 12.52186555248743538 ) ) ;
#24584 = CARTESIAN_POINT ( 'NONE',  ( -14.92860730136983882, 8.468845235798745819, -45.33787050070434788 ) ) ;
#24585 = DIRECTION ( 'NONE',  ( 1.000000000000000000, 0.000000000000000000, -0.000000000000000000 ) ) ;
#24586 = EDGE_CURVE ( 'NONE', #5113, #34356, #53542, .T. ) ;
#24587 = ORIENTED_EDGE ( 'NONE', *, *, #46561, .T. ) ;
#24588 = B_SPLINE_CURVE_WITH_KNOTS ( 'NONE', 3,
 ( #28615, #50415, #18399, #39514, #34933, #51796, #68329, #57079, #4634, #63037, #46163, #68990, #62705, #67637, #51458, #14506 ),
 .UNSPECIFIED., .F., .F.,
 ( 4, 2, 2, 2, 2, 2, 2, 4 ),
 ( 0.000000000000000000, 0.001318014594730357791, 0.002636029189460715582, 0.003954043784191073156, 0.005272058378921431164, 0.006590072973651789172, 0.007908087568382146312, 0.01054411675784286233 ),
 .UNSPECIFIED. ) ;
#24589 = CARTESIAN_POINT ( 'NONE',  ( -107.3439416623322842, 35.42826784730606704, -90.65402495570906183 ) ) ;
#24590 = VERTEX_POINT ( 'NONE', #26993 ) ;
#24591 = LINE ( 'NONE', #3810, #65410 ) ;
#24592 = CARTESIAN_POINT ( 'NONE',  ( -20.55634918610405748, -15.55634918610400774, 2.000000000000000000 ) ) ;
#24594 = ADVANCED_FACE ( 'NONE', ( #43855 ), #48773, .T. ) ;
#24593 = CARTESIAN_POINT ( 'NONE',  ( 311.9975424824652350, 170.0000000000000284, 536.6193948016162949 ) ) ;
#24595 = ORIENTED_EDGE ( 'NONE', *, *, #67074, .F. ) ;
#24596 = CARTESIAN_POINT ( 'NONE',  ( -125.0000000000000000, 0.000000000000000000, -5.000000000000000000 ) ) ;
#24597 = CARTESIAN_POINT ( 'NONE',  ( -15.13254930056756287, 7.477527548005406643, -68.05477072695896368 ) ) ;
#24598 = CARTESIAN_POINT ( 'NONE',  ( -35.17686701826947626, 10.23452050416468317, 44.23696391509336934 ) ) ;
#24599 = CARTESIAN_POINT ( 'NONE',  ( -29.49620345460275317, 9.280093073089043187, 71.82164555316683163 ) ) ;
#24600 = ORIENTED_EDGE ( 'NONE', *, *, #29303, .F. ) ;
#24601 = DIRECTION ( 'NONE',  ( 1.000000000000000000, 0.000000000000000000, 0.000000000000000000 ) ) ;
#24602 = CARTESIAN_POINT ( 'NONE',  ( 21.27121078971612889, 61.42097029141972087, 73.58025477438755502 ) ) ;
#24603 = CARTESIAN_POINT ( 'NONE',  ( -119.1795380581000074, 42.22910606512925114, 34.76803934698340015 ) ) ;
#24604 = CARTESIAN_POINT ( 'NONE',  ( -58.32860549785898030, 15.58423118879329294, -49.46749250328178960 ) ) ;
#24605 = ORIENTED_EDGE ( 'NONE', *, *, #9536, .F. ) ;
#24606 = CARTESIAN_POINT ( 'NONE',  ( -177.5288247523079121, 93.72924674643513754, -62.97066215026593738 ) ) ;
#24607 = CARTESIAN_POINT ( 'NONE',  ( 92.19920907511534836, 21.39700525884449434, 59.01058764121106748 ) ) ;
#24608 = DIRECTION ( 'NONE',  ( -1.000000000000000000, 0.000000000000000000, 0.000000000000000000 ) ) ;
#24609 =( NAMED_UNIT ( * ) PLANE_ANGLE_UNIT ( ) SI_UNIT ( $, .RADIAN. ) );
#24610 = CYLINDRICAL_SURFACE ( 'NONE', #66111, 5.000000000000004441 ) ;
#24611 = VERTEX_POINT ( 'NONE', #43510 ) ;
#24612 = CARTESIAN_POINT ( 'NONE',  ( 197.9847015768255289, 97.56951352050452897, 40.06412533389060115 ) ) ;
#24613 = LINE ( 'NONE', #4524, #10348 ) ;
#24614 = CARTESIAN_POINT ( 'NONE',  ( 70.25990036603479894, 14.47042233282420298, 66.11517460769501042 ) ) ;
#24615 = CARTESIAN_POINT ( 'NONE',  ( 187.4018290418642039, 85.23542003817890134, -93.36671599347617700 ) ) ;
#24616 = CARTESIAN_POINT ( 'NONE',  ( 0.000000000000000000, 0.000000000000000000, 380.0000000000000000 ) ) ;
#24617 = EDGE_LOOP ( 'NONE', ( #13870, #22244, #7334 ) ) ;
#24618 = EDGE_CURVE ( 'NONE', #15622, #44112, #60107, .T. ) ;
#24619 = CARTESIAN_POINT ( 'NONE',  ( 160.9097745014958036, 61.67033591969550343, -10.11087558020973987 ) ) ;
#24620 = ORIENTED_EDGE ( 'NONE', *, *, #19312, .F. ) ;
#24622 = EDGE_CURVE ( 'NONE', #45386, #7953, #48422, .T. ) ;
#24621 = CARTESIAN_POINT ( 'NONE',  ( 70.12389542974192125, 15.47520081968151651, 61.71442529660797049 ) ) ;
#24623 = CARTESIAN_POINT ( 'NONE',  ( 128.4441453432628180, 38.25093000060704895, 85.49679608215056703 ) ) ;
#24624 = AXIS2_PLACEMENT_3D ( 'NONE', #24791, #30071, #3669 ) ;
#24625 = VECTOR ( 'NONE', #12407, 1000.000000000000000 ) ;
#24627 = ORIENTED_EDGE ( 'NONE', *, *, #8021, .F. ) ;
#24626 = LINE ( 'NONE', #7499, #44348 ) ;
#24628 = CARTESIAN_POINT ( 'NONE',  ( -143.8566410313463564, 59.53044870492033880, -64.19978731914612524 ) ) ;
#24629 = FACE_OUTER_BOUND ( 'NONE', #2559, .T. ) ;
#24630 = DIRECTION ( 'NONE',  ( -0.8465179929926601732, -0.5323601107705934199, 0.000000000000000000 ) ) ;
#24631 = ORIENTED_EDGE ( 'NONE', *, *, #43171, .F. ) ;
#24632 = B_SPLINE_CURVE_WITH_KNOTS ( 'NONE', 3,
 ( #53333, #21336, #36838, #9415, #64252, #4812, #25605, #36490, #58277, #41767, #30872, #16060, #52654, #26626, #9761, #42449, #48061, #47039, #52315, #10098, #31553, #63907, #69515, #14680, #63224, #47716, #42783, #52991, #37513, #15377, #36146, #4138, #20647, #63566, #20302, #15032, #10432, #42108, #57940, #4479, #15721, #25937, #68824, #21003, #37170 ),
 .UNSPECIFIED., .F., .F.,
 ( 4, 2, 2, 2, 2, 2, 2, 2, 2, 2, 2, 1, 2, 2, 2, 2, 2, 2, 2, 2, 2, 2, 4 ),
 ( 0.000000000000000000, 0.001512548138464682055, 0.002268822207697023408, 0.003025096276929364111, 0.004537644415394017326, 0.005293918484626359763, 0.006050192553858700466, 0.007562740692323367993, 0.009075288830788034652, 0.01058783696925270218, 0.01134411103848502640, 0.01210038510771735062, 0.01285665917694967485, 0.01361293324618199907, 0.01512548138464661802, 0.01588175545387892837, 0.01663802952311123351, 0.01815057766157585420, 0.01966312580004047489, 0.02041939986927278697, 0.02117567393850509905, 0.02268822207696975790, 0.02420077021543442022 ),
 .UNSPECIFIED. ) ;
#24633 = CARTESIAN_POINT ( 'NONE',  ( -97.88021438939455265, 31.71889184683105611, 17.26694248044579538 ) ) ;
#24634 = EDGE_CURVE ( 'NONE', #33798, #40228, #65331, .T. ) ;
#24635 = CARTESIAN_POINT ( 'NONE',  ( 36.85262215550067566, 53.56030941157737146, 170.0000000000000000 ) ) ;
#24636 = FACE_OUTER_BOUND ( 'NONE', #32210, .T. ) ;
#24637 = CARTESIAN_POINT ( 'NONE',  ( 83.38619203015947789, 19.39783821526630447, -23.25651540956177499 ) ) ;
#24638 = CARTESIAN_POINT ( 'NONE',  ( -177.2783414347497626, 93.43285667108899872, -89.65509825100188834 ) ) ;
#24639 = CARTESIAN_POINT ( 'NONE',  ( 150.5550643769628891, 52.46819381604269239, 60.83852809269659190 ) ) ;
#24640 = EDGE_CURVE ( 'NONE', #50057, #34560, #33683, .T. ) ;
#24641 = DIRECTION ( 'NONE',  ( -0.000000000000000000, -0.000000000000000000, -1.000000000000000000 ) ) ;
#24642 = ORIENTED_EDGE ( 'NONE', *, *, #59778, .T. ) ;
#24643 = CARTESIAN_POINT ( 'NONE',  ( -95.20053778133913625, 30.43887292928078026, 62.33583445852484317 ) ) ;
#24645 = ADVANCED_FACE ( 'NONE', ( #611 ), #64987, .T. ) ;
#24644 = DIRECTION ( 'NONE',  ( -0.000000000000000000, 1.000000000000000000, -0.000000000000000000 ) ) ;
#24646 = ORIENTED_EDGE ( 'NONE', *, *, #58575, .T. ) ;
#24647 = CARTESIAN_POINT ( 'NONE',  ( 155.2870855780214470, 57.23765125306420032, -9.590301590278679456 ) ) ;
#24648 = CARTESIAN_POINT ( 'NONE',  ( 210.6592759200688079, 116.7161312026394171, -12.42314136530470670 ) ) ;
#24649 = CARTESIAN_POINT ( 'NONE',  ( -4.072522659361689890, 7.683023425615342461, 31.11739723680042857 ) ) ;
#24650 = CARTESIAN_POINT ( 'NONE',  ( -4.613603609465529054, 74.86839895266042788, 133.5802547743875550 ) ) ;
#24651 = CARTESIAN_POINT ( 'NONE',  ( -54.57280099357648595, 14.55288945003961310, -77.06087458892361042 ) ) ;
#24652 = CARTESIAN_POINT ( 'NONE',  ( -1.096061481932294024, 7.553048580900440179, -19.39417165875558879 ) ) ;
#24653 = CARTESIAN_POINT ( 'NONE',  ( 180.2473887773227545, 77.76029175826238315, 17.46404351504774510 ) ) ;
#24654 = FACE_OUTER_BOUND ( 'NONE', #36832, .T. ) ;
#24655 = ORIENTED_EDGE ( 'NONE', *, *, #25346, .F. ) ;
#24656 = CARTESIAN_POINT ( 'NONE',  ( 447.3372781065086201, 0.000000000000000000, 78.55029585798817493 ) ) ;
#24657 = ORIENTED_EDGE ( 'NONE', *, *, #20414, .T. ) ;
#24658 = CARTESIAN_POINT ( 'NONE',  ( 110.2429982417149574, 29.99119854320846201, -50.92243756565370916 ) ) ;
#24659 = CARTESIAN_POINT ( 'NONE',  ( -21.78980970457817179, 0.000000000000000000, 33.04664611826583354 ) ) ;
#24660 = LINE ( 'NONE', #1818, #52939 ) ;
#24661 = DIRECTION ( 'NONE',  ( 1.000000000000000000, 0.000000000000000000, 0.000000000000000000 ) ) ;
#24662 = CARTESIAN_POINT ( 'NONE',  ( 18.43272992546528144, 7.606837839440253823, 44.53733308803361979 ) ) ;
#24663 = CIRCLE ( 'NONE', #63958, 299.9999999999999432 ) ;
#24664 = CARTESIAN_POINT ( 'NONE',  ( -109.6657532478350845, 37.84376708859253569, -17.00084428919926438 ) ) ;
#24665 = EDGE_LOOP ( 'NONE', ( #43122, #49749, #68545, #49224 ) ) ;
#24666 = CARTESIAN_POINT ( 'NONE',  ( 60.82895951008426749, -30.68107831874539926, 43.58025477438756923 ) ) ;
#24667 = LINE ( 'NONE', #67245, #2704 ) ;
#24668 = EDGE_LOOP ( 'NONE', ( #26070, #42904, #34354, #22571, #35706, #63780 ) ) ;
#24669 = EDGE_CURVE ( 'NONE', #44993, #32175, #5359, .T. ) ;
#24670 = ORIENTED_EDGE ( 'NONE', *, *, #37323, .F. ) ;
#24671 = DIRECTION ( 'NONE',  ( -0.5407162030609375947, -0.6444004775717706579, 0.5407162030609372616 ) ) ;
#24672 = CARTESIAN_POINT ( 'NONE',  ( 432.4999999999999432, 207.5000000000000284, 378.0000000000000000 ) ) ;
#24673 = DIRECTION ( 'NONE',  ( 0.000000000000000000, 0.000000000000000000, 1.000000000000000000 ) ) ;
#24674 = CARTESIAN_POINT ( 'NONE',  ( 104.7227067006896277, 27.50728936118536438, 58.85534883732941580 ) ) ;
#24675 = LINE ( 'NONE', #34546, #54322 ) ;
#24676 = VECTOR ( 'NONE', #15188, 1000.000000000000000 ) ;
#24677 = CARTESIAN_POINT ( 'NONE',  ( 56.29445224195348629, 12.24017809212662122, -19.74059151869303719 ) ) ;
#24678 = ORIENTED_EDGE ( 'NONE', *, *, #46371, .F. ) ;
#24679 = AXIS2_PLACEMENT_3D ( 'NONE', #4435, #53638, #21297 ) ;
#24680 = CARTESIAN_POINT ( 'NONE',  ( -2.747334540031024730, -33.31268936679798287, 6.893343212288937316 ) ) ;
#24681 = ORIENTED_EDGE ( 'NONE', *, *, #25906, .T. ) ;
#24682 = CARTESIAN_POINT ( 'NONE',  ( 206.6955592216989714, 109.1214665502617862, 2.622639889806200220 ) ) ;
#24683 = FACE_OUTER_BOUND ( 'NONE', #10543, .T. ) ;
#24684 = CARTESIAN_POINT ( 'NONE',  ( 212.0047492081759799, 116.9348962082588059, 34.98673273882808132 ) ) ;
#24685 = FACE_BOUND ( 'NONE', #14141, .T. ) ;
#24686 = EDGE_LOOP ( 'NONE', ( #64659, #46445, #40296, #10701 ) ) ;
#24687 = ORIENTED_EDGE ( 'NONE', *, *, #23507, .F. ) ;
#24688 = CARTESIAN_POINT ( 'NONE',  ( 111.3018128478065876, -21.46140473645479929, 4.838640910132746775 ) ) ;
#24689 = CARTESIAN_POINT ( 'NONE',  ( -118.4108695702138618, 42.93846248464117821, 92.41764988183072660 ) ) ;
#24690 = LINE ( 'NONE', #45437, #44196 ) ;
#24691 = CARTESIAN_POINT ( 'NONE',  ( 0.000000000000000000, 0.000000000000000000, 170.0000000000000000 ) ) ;
#24692 = CARTESIAN_POINT ( 'NONE',  ( -868.3301948030079984, -622.0000000000060254, 10.00000000000000000 ) ) ;
#24693 = AXIS2_PLACEMENT_3D ( 'NONE', #54882, #7054, #28512 ) ;
#24694 = CARTESIAN_POINT ( 'NONE',  ( 84.27368848767926579, 18.63026910897604083, -77.30289597407090696 ) ) ;
#24695 = ADVANCED_FACE ( 'NONE', ( #8334 ), #19215, .T. ) ;
#24696 = ORIENTED_EDGE ( 'NONE', *, *, #65600, .T. ) ;
#24697 = DIRECTION ( 'NONE',  ( 0.000000000000000000, -1.000000000000000000, 0.000000000000000000 ) ) ;
#24698 = PLANE ( 'NONE',  #61975 ) ;
#24699 = ADVANCED_FACE ( 'NONE', ( #29431 ), #3057, .F. ) ;
#24700 = EDGE_LOOP ( 'NONE', ( #30321, #1391, #38693, #37024 ) ) ;
#24701 = CARTESIAN_POINT ( 'NONE',  ( -440.1146514826278917, 394.9999999999955094, 101.0022254471289358 ) ) ;
#24702 = VERTEX_POINT ( 'NONE', #34380 ) ;
#24703 = CARTESIAN_POINT ( 'NONE',  ( -79.14127775978546708, 22.50259208414362533, -76.96000122218161721 ) ) ;
#24704 = DIRECTION ( 'NONE',  ( 0.5773502691896258421, 0.5773502691896258421, -0.5773502691896258421 ) ) ;
#24705 = EDGE_CURVE ( 'NONE', #59695, #54597, #12922, .T. ) ;
#24706 = APPLICATION_CONTEXT ( 'automotive_design' ) ;
#24707 = ORIENTED_EDGE ( 'NONE', *, *, #28336, .T. ) ;
#24708 = EDGE_CURVE ( 'NONE', #50424, #50563, #66744, .T. ) ;
#24709 = EDGE_LOOP ( 'NONE', ( #45756, #38260 ) ) ;
#24710 = CARTESIAN_POINT ( 'NONE',  ( 46.51377856795992471, 10.46037936279324221, 66.68987646718457540 ) ) ;
#24711 = CIRCLE ( 'NONE', #30324, 65.36598343705435354 ) ;
#24712 = FACE_OUTER_BOUND ( 'NONE', #52819, .T. ) ;
#24713 = CARTESIAN_POINT ( 'NONE',  ( 17.72992212664810907, 6.570588738776103277, 3.421689050534150844 ) ) ;
#24714 = EDGE_LOOP ( 'NONE', ( #23401, #8807, #51355, #13941 ) ) ;
#24715 = CARTESIAN_POINT ( 'NONE',  ( -20.55634918610411077, -41.66904755831209428, 0.000000000000000000 ) ) ;
#24716 = FACE_OUTER_BOUND ( 'NONE', #59779, .T. ) ;
#24717 = LINE ( 'NONE', #57403, #16805 ) ;
#24718 = EDGE_CURVE ( 'NONE', #59217, #889, #9609, .T. ) ;
#24719 = CARTESIAN_POINT ( 'NONE',  ( 116.1021807117071916, 31.68810634233424395, -11.86957610067093860 ) ) ;
#24720 = DIRECTION ( 'NONE',  ( 1.000000000000000000, 0.000000000000000000, 0.000000000000000000 ) ) ;
#24721 = CARTESIAN_POINT ( 'NONE',  ( -442.6627218934912662, 394.9999999999998295, 113.5502958579882034 ) ) ;
#24722 = EDGE_LOOP ( 'NONE', ( #66709, #20208, #56368, #67953 ) ) ;
#24723 = AXIS2_PLACEMENT_3D ( 'NONE', #802, #33857, #55298 ) ;
#24724 = ORIENTED_EDGE ( 'NONE', *, *, #43009, .F. ) ;
#24725 = CARTESIAN_POINT ( 'NONE',  ( -14.19745717986860534, 56.58567516677720022, 27.58472369372398347 ) ) ;
#24726 = CARTESIAN_POINT ( 'NONE',  ( -175.7347375270319105, 91.62140458887586192, 84.96244202411565993 ) ) ;
#24727 = CYLINDRICAL_SURFACE ( 'NONE', #5342, 65.36598343705435354 ) ;
#24728 = DIRECTION ( 'NONE',  ( -1.000000000000000000, 0.000000000000000000, 0.000000000000000000 ) ) ;
#24729 = CARTESIAN_POINT ( 'NONE',  ( 130.7531879853686405, 39.58149302537893988, 17.00924939245568623 ) ) ;
#24730 = DIRECTION ( 'NONE',  ( -0.000000000000000000, 1.000000000000000000, 0.000000000000000000 ) ) ;
#24731 = CARTESIAN_POINT ( 'NONE',  ( 199.2613222657365668, 100.8067368203101069, 85.21932682755294763 ) ) ;
#24732 = CARTESIAN_POINT ( 'NONE',  ( 212.0104729185451049, 118.7959000526602864, 38.40396052458186205 ) ) ;
#24733 = CARTESIAN_POINT ( 'NONE',  ( -75.00168449119588843, 20.95943092127967589, -62.91188405899502101 ) ) ;
#24734 = DIRECTION ( 'NONE',  ( 0.000000000000000000, -0.000000000000000000, 1.000000000000000000 ) ) ;
#24735 = VERTEX_POINT ( 'NONE', #52941 ) ;
#24736 = CARTESIAN_POINT ( 'NONE',  ( 9.045716588192245666, 7.384596431530732197, -12.85322072703573859 ) ) ;
#24737 = ORIENTED_EDGE ( 'NONE', *, *, #24367, .F. ) ;
#24738 = CARTESIAN_POINT ( 'NONE',  ( 201.9869293910475676, 102.6997661182766990, -9.976692069364466064 ) ) ;
#24739 = ORIENTED_EDGE ( 'NONE', *, *, #48620, .T. ) ;
#24740 = CARTESIAN_POINT ( 'NONE',  ( -143.3980294393559234, 60.45217072626395094, 7.018557309704483771 ) ) ;
#24741 = CARTESIAN_POINT ( 'NONE',  ( 187.5246323291926842, 86.86207184872515086, -66.68771993737131254 ) ) ;
#24742 = CARTESIAN_POINT ( 'NONE',  ( -146.5309471467636229, 62.99917515507672050, 71.95316401501160897 ) ) ;
#24743 = VECTOR ( 'NONE', #3605, 1000.000000000000000 ) ;
#24744 = DIRECTION ( 'NONE',  ( -1.000000000000000000, 0.000000000000000000, 0.000000000000000000 ) ) ;
#24745 = CARTESIAN_POINT ( 'NONE',  ( 35.44781468922821688, 7.928097401423690016, -49.49746209005169106 ) ) ;
#24746 = CARTESIAN_POINT ( 'NONE',  ( 563.4809901518626702, 190.0000000000000000, 57.79371821540657095 ) ) ;
#24747 = CARTESIAN_POINT ( 'NONE',  ( -417.6627218934913230, 219.4906275429376308, -144.4497041420118819 ) ) ;
#24748 = CARTESIAN_POINT ( 'NONE',  ( 127.4750938923429544, 37.70245908594341699, -47.47187847537448135 ) ) ;
#24749 = ORIENTED_EDGE ( 'NONE', *, *, #31067, .T. ) ;
#24750 = ORIENTED_EDGE ( 'NONE', *, *, #28646, .T. ) ;
#24751 = CARTESIAN_POINT ( 'NONE',  ( 187.7216195934903169, 87.07953284547519957, 86.98655473364385671 ) ) ;
#24752 = PLANE ( 'NONE',  #30802 ) ;
#24753 = CARTESIAN_POINT ( 'NONE',  ( 55.00000000000000000, 16.00000000000000000, -5.803681084894614095 ) ) ;
#24754 = UNCERTAINTY_MEASURE_WITH_UNIT (LENGTH_MEASURE( 1.000000000000000082E-05 ), #33734, 'distance_accuracy_value', 'NONE');
#24755 = AXIS2_PLACEMENT_3D ( 'NONE', #33572, #17734, #66622 ) ;
#24756 = CARTESIAN_POINT ( 'NONE',  ( 14.80582440982707482, 6.470883766728820596, 18.12156665253656840 ) ) ;
#24757 = DIRECTION ( 'NONE',  ( -0.000000000000000000, -6.405132834375902056E-16, 1.000000000000000000 ) ) ;
#24758 = CARTESIAN_POINT ( 'NONE',  ( -45.00000000000002132, 20.00000000000000355, 0.000000000000000000 ) ) ;
#24759 = CARTESIAN_POINT ( 'NONE',  ( 205.5130322755755401, 109.1888880665735684, 17.36317014830577676 ) ) ;
#24760 = EDGE_CURVE ( 'NONE', #28906, #26796, #35654, .T. ) ;
#24761 = CARTESIAN_POINT ( 'NONE',  ( 278.7020975237396669, -21.46299323290192262, 4.831387770023922279 ) ) ;
#24762 = PLANE ( 'NONE',  #43070 ) ;
#24763 = CARTESIAN_POINT ( 'NONE',  ( -24.32471770265757627, 9.546495606312140225, 62.13629395109772702 ) ) ;
#24764 = CARTESIAN_POINT ( 'NONE',  ( 0.000000000000000000, 0.000000000000000000, 0.000000000000000000 ) ) ;
#24765 = CARTESIAN_POINT ( 'NONE',  ( -48.56549579811110817, 13.03742088415615541, 68.45772509223345992 ) ) ;
#24766 = CARTESIAN_POINT ( 'NONE',  ( -7.825402957745083654, 6.891034867348165172, 56.96013162991089018 ) ) ;
#24767 = ORIENTED_EDGE ( 'NONE', *, *, #61159, .F. ) ;
#24768 = LINE ( 'NONE', #39559, #63084 ) ;
#24769 = DIRECTION ( 'NONE',  ( 1.000000000000000000, -0.000000000000000000, -0.000000000000000000 ) ) ;
#24770 = DIRECTION ( 'NONE',  ( 0.000000000000000000, 0.000000000000000000, -1.000000000000000000 ) ) ;
#24771 = CARTESIAN_POINT ( 'NONE',  ( -52.45215874217870322, 13.99961488531757503, -49.75515071437175862 ) ) ;
#24772 = LINE ( 'NONE', #35322, #67219 ) ;
#24773 = VECTOR ( 'NONE', #66335, 1000.000000000000000 ) ;
#24774 = CARTESIAN_POINT ( 'NONE',  ( 0.000000000000000000, 192.0000000000000000, 0.000000000000000000 ) ) ;
#24775 = ORIENTED_EDGE ( 'NONE', *, *, #8831, .T. ) ;
#24776 = CARTESIAN_POINT ( 'NONE',  ( -25.10237775011639982, -1.004202417053851937, 0.000000000000000000 ) ) ;
#24777 = FACE_BOUND ( 'NONE', #20183, .T. ) ;
#24778 = EDGE_CURVE ( 'NONE', #68402, #54490, #56866, .T. ) ;
#24779 = ORIENTED_EDGE ( 'NONE', *, *, #17928, .F. ) ;
#24780 = ORIENTED_EDGE ( 'NONE', *, *, #43666, .F. ) ;
#24781 = CARTESIAN_POINT ( 'NONE',  ( 311.9975424824652350, 170.0000000000000284, 254.5114349394235091 ) ) ;
#24782 = CYLINDRICAL_SURFACE ( 'NONE', #62488, 7.500000000000020428 ) ;
#24783 = CARTESIAN_POINT ( 'NONE',  ( 15.78827728214693060, 7.507518794609574719, -8.674393508222097537 ) ) ;
#24784 = ORIENTED_EDGE ( 'NONE', *, *, #10397, .T. ) ;
#24785 = CARTESIAN_POINT ( 'NONE',  ( 99.71998884745383407, 2.000000000000000000, 7.478223336038896996 ) ) ;
#24786 = CARTESIAN_POINT ( 'NONE',  ( -55.05276343752910151, -170.0000000000000000, 91.50642895385851716 ) ) ;
#24787 = LINE ( 'NONE', #19495, #62295 ) ;
#24788 = ADVANCED_FACE ( 'NONE', ( #4766 ), #35759, .F. ) ;
#24789 = VECTOR ( 'NONE', #2753, 1000.000000000000000 ) ;
#24790 = CARTESIAN_POINT ( 'NONE',  ( 62.05396267233469132, 13.48332220860126540, -50.67464569965138566 ) ) ;
#24791 = CARTESIAN_POINT ( 'NONE',  ( 0.000000000000000000, 0.000000000000000000, 30.00000000000000000 ) ) ;
#24792 = CARTESIAN_POINT ( 'NONE',  ( -2.645508037661902456, -7.710219529346618472, -0.06809871960543704972 ) ) ;
#24793 = CARTESIAN_POINT ( 'NONE',  ( 140.4586216751744985, 45.55624550472995793, 6.597895794798392721 ) ) ;
#24794 = ORIENTED_EDGE ( 'NONE', *, *, #42643, .T. ) ;
#24795 = CARTESIAN_POINT ( 'NONE',  ( 110.7164744784863757, 29.10110206241301611, -35.92243756565368784 ) ) ;
#24796 = CARTESIAN_POINT ( 'NONE',  ( 10.83418588031599583, 6.392467435475929882, 58.70663493700131852 ) ) ;
#24797 = ADVANCED_FACE ( 'NONE', ( #15673 ), #8685, .F. ) ;
#24798 = CARTESIAN_POINT ( 'NONE',  ( 46.41758729921144777, 9.425975226414236019, -45.78279639359242026 ) ) ;
#24799 = CARTESIAN_POINT ( 'NONE',  ( -77.48202330058325060, 22.94882077088976047, 84.19497686350740651 ) ) ;
#24801 = VERTEX_POINT ( 'NONE', #42404 ) ;
#24800 = CARTESIAN_POINT ( 'NONE',  ( -15.67984581961064450, 63.08044415722863363, 170.0000000000000000 ) ) ;
#24802 = LINE ( 'NONE', #30081, #36415 ) ;
#24803 = EDGE_LOOP ( 'NONE', ( #53971, #23828, #40146, #57589 ) ) ;
#24804 = VECTOR ( 'NONE', #1640, 1000.000000000000000 ) ;
#24805 = EDGE_CURVE ( 'NONE', #34775, #16199, #44397, .T. ) ;
#24806 = EDGE_LOOP ( 'NONE', ( #27339, #26415, #57735, #51065 ) ) ;
#24807 = CARTESIAN_POINT ( 'NONE',  ( -146.1142527948576060, 61.35394402951021675, 71.75774863290075700 ) ) ;
#24808 = CARTESIAN_POINT ( 'NONE',  ( 6.590627084543000613, -57.96611065023441967, 27.58472315868180402 ) ) ;
#24809 = CARTESIAN_POINT ( 'NONE',  ( 197.1980152960109649, 96.59350208824301376, -70.33315983686533457 ) ) ;
#24810 = CARTESIAN_POINT ( 'NONE',  ( 0.000000000000000000, 0.000000000000000000, -7.000000000000000000 ) ) ;
#24811 = CARTESIAN_POINT ( 'NONE',  ( 31.11269837220806522, -6.375108774214766072E-14, 85.00100000000000477 ) ) ;
#24812 = CARTESIAN_POINT ( 'NONE',  ( -78.66644367742111399, 23.39876645725285798, -8.270900041254197532 ) ) ;
#24813 = CARTESIAN_POINT ( 'NONE',  ( -176.3856149167965839, 92.38076834121986280, -8.600915367064782657 ) ) ;
#24814 = CARTESIAN_POINT ( 'NONE',  ( -153.1121305730337383, 67.29834700374527756, -35.73192746080628268 ) ) ;
#24815 = ORIENTED_EDGE ( 'NONE', *, *, #53762, .F. ) ;
#24816 = ORIENTED_EDGE ( 'NONE', *, *, #24162, .T. ) ;
#24817 = CYLINDRICAL_SURFACE ( 'NONE', #29795, 25.00000000000145306 ) ;
#24818 = CARTESIAN_POINT ( 'NONE',  ( 102.8458551240039895, 25.60773946375957166, 62.69125674198833309 ) ) ;
#24819 = CARTESIAN_POINT ( 'NONE',  ( 163.1265310614426767, 62.18610413911353874, 58.82269949688948429 ) ) ;
#24820 = DIRECTION ( 'NONE',  ( -0.000000000000000000, 1.000000000000000000, -0.000000000000000000 ) ) ;
#24821 = FACE_OUTER_BOUND ( 'NONE', #14937, .T. ) ;
#24822 = CARTESIAN_POINT ( 'NONE',  ( 412.3372781065083927, 397.0710678118695114, 78.55029585798419589 ) ) ;
#24823 = CARTESIAN_POINT ( 'NONE',  ( -31.43908319763710679, 9.591432048623762086, 72.06100499665289760 ) ) ;
#24824 = VERTEX_POINT ( 'NONE', #63864 ) ;
#24825 = EDGE_LOOP ( 'NONE', ( #4659, #54553, #25083, #1813, #17544 ) ) ;
#24826 = EDGE_LOOP ( 'NONE', ( #3163, #39248, #50039, #2913, #41058, #616, #11308, #6727, #93 ) ) ;
#24827 = CARTESIAN_POINT ( 'NONE',  ( -152.9008427825210958, 68.45483453645054794, -22.16050399148043226 ) ) ;
#24828 = CARTESIAN_POINT ( 'NONE',  ( 39.40195752203892710, 9.424259417798134919, -50.61981746542779348 ) ) ;
#24829 = CYLINDRICAL_SURFACE ( 'NONE', #69088, 7.500000000000013323 ) ;
#24830 = CARTESIAN_POINT ( 'NONE',  ( 109.4667359685670078, 28.52415501392344410, -89.64184605405843342 ) ) ;
#24831 = CARTESIAN_POINT ( 'NONE',  ( -57.89360549284270974, 16.50663738101750511, 44.77101158031961603 ) ) ;
#24832 = AXIS2_PLACEMENT_3D ( 'NONE', #11737, #5762, #49711 ) ;
#24833 = CARTESIAN_POINT ( 'NONE',  ( -38.80621507254812741, 11.94263265896524473, -68.19319284720511121 ) ) ;
#24834 = LINE ( 'NONE', #13585, #63778 ) ;
#24835 = CARTESIAN_POINT ( 'NONE',  ( 11.21653854975268771, 6.397128675385706842, -10.20870010705862363 ) ) ;
#24836 = CIRCLE ( 'NONE', #13630, 74.95140232871122521 ) ;
#24837 = B_SPLINE_CURVE_WITH_KNOTS ( 'NONE', 3,
 ( #63873, #10741, #5467, #36109, #20604, #10390, #10058, #57902, #63186, #42748, #48349, #9724, #36800, #21638, #182, #42066, #14988, #57563, #63526, #43092, #15342, #58242, #48019, #25564, #4774, #69480, #37472, #68462, #16019, #21300, #26922, #47002, #31518, #31186, #20267, #4102, #52952, #47674, #58923, #69132 ),
 .UNSPECIFIED., .F., .F.,
 ( 4, 2, 2, 2, 2, 2, 2, 2, 2, 2, 2, 2, 2, 2, 2, 2, 2, 2, 2, 4 ),
 ( 0.02454308262168998500, 0.02608670964102876785, 0.02685852315069817489, 0.02763033666036758540, 0.02917396367970639948, 0.02994577718937580652, 0.03071759069904521355, 0.03226121771838405539, 0.03303303122805349712, 0.03380484473772293885, 0.03534847175706178762, 0.03689209877640063640, 0.03843572579573948517, 0.03997935281507833394, 0.04152297983441718271, 0.04306660685375603148, 0.04461023387309488025, 0.04615386089243372902, 0.04769748791177257780, 0.04924111493111142657 ),
 .UNSPECIFIED. ) ;
#24839 = ORIENTED_EDGE ( 'NONE', *, *, #67334, .T. ) ;
#24838 = EDGE_CURVE ( 'NONE', #16988, #41527, #46989, .T. ) ;
#24840 = CARTESIAN_POINT ( 'NONE',  ( -3.868882431147343315, 6.665575841812209745, -49.29435056024676953 ) ) ;
#24841 = DIRECTION ( 'NONE',  ( 0.000000000000000000, 0.000000000000000000, -1.000000000000000000 ) ) ;
#24842 = CARTESIAN_POINT ( 'NONE',  ( -121.5677746760273408, 43.71038933438990881, 17.42027109748232050 ) ) ;
#24843 = CARTESIAN_POINT ( 'NONE',  ( 67.93926590385571274, 13.86859831467923954, -64.38660125305884208 ) ) ;
#24844 = CARTESIAN_POINT ( 'NONE',  ( -17.50000000000002842, 207.5000000000000284, 0.000000000000000000 ) ) ;
#24845 = FACE_OUTER_BOUND ( 'NONE', #3249, .T. ) ;
#24846 = CARTESIAN_POINT ( 'NONE',  ( 197.3707490726349647, 96.80690576410100334, 65.18469054512721073 ) ) ;
#24847 = VECTOR ( 'NONE', #49152, 1000.000000000000000 ) ;
#24848 = EDGE_CURVE ( 'NONE', #8872, #48097, #47757, .T. ) ;
#24849 = ORIENTED_EDGE ( 'NONE', *, *, #46345, .F. ) ;
#24850 = PRODUCT_CONTEXT ( 'NONE', #44409, 'mechanical' ) ;
#24851 = AXIS2_PLACEMENT_3D ( 'NONE', #15716, #31219, #43125 ) ;
#24852 = DIRECTION ( 'NONE',  ( -0.000000000000000000, -0.000000000000000000, 1.000000000000000000 ) ) ;
#24853 = DIRECTION ( 'NONE',  ( 1.000000000000000000, 0.000000000000000000, 0.000000000000000000 ) ) ;
#24854 = DIRECTION ( 'NONE',  ( 0.2225209339563184452, -0.9749279121818226201, 0.000000000000000000 ) ) ;
#24855 = CARTESIAN_POINT ( 'NONE',  ( 186.0827296088607170, 85.28826835108066007, -38.12883777694066367 ) ) ;
#24856 = EDGE_LOOP ( 'NONE', ( #65849, #56941, #54165, #28596, #55192 ) ) ;
#24857 = ORIENTED_EDGE ( 'NONE', *, *, #17966, .F. ) ;
#24858 = EDGE_CURVE ( 'NONE', #15369, #49352, #63177, .T. ) ;
#24859 = FACE_OUTER_BOUND ( 'NONE', #4274, .T. ) ;
#24860 = DIRECTION ( 'NONE',  ( -0.000000000000000000, 1.000000000000000000, -0.000000000000000000 ) ) ;
#24861 = EDGE_CURVE ( 'NONE', #69425, #54206, #57553, .T. ) ;
#24862 = ORIENTED_EDGE ( 'NONE', *, *, #30027, .F. ) ;
#24863 = CARTESIAN_POINT ( 'NONE',  ( 164.9799824490939670, 65.05186898783672689, 90.53880561405300398 ) ) ;
#24864 = EDGE_CURVE ( 'NONE', #11023, #40688, #28695, .T. ) ;
#24865 = ORIENTED_EDGE ( 'NONE', *, *, #39661, .F. ) ;
#24866 = CARTESIAN_POINT ( 'NONE',  ( -57.43883374585515611, 16.37892664338858495, 18.08720956373479893 ) ) ;
#24867 = CARTESIAN_POINT ( 'NONE',  ( 128.4224537826254107, 38.23837035195747092, 42.20221012506080172 ) ) ;
#24868 = CARTESIAN_POINT ( 'NONE',  ( -52.69240448066660321, 53.30312580971368419, 41.38025477438755928 ) ) ;
#24869 = ADVANCED_FACE ( 'NONE', ( #51921 ), #36440, .F. ) ;
#24870 = ADVANCED_FACE ( 'NONE', ( #36792 ), #14080, .T. ) ;
#24871 = CARTESIAN_POINT ( 'NONE',  ( -102.2801239173131052, 32.78103895658057354, 30.51907450641510522 ) ) ;
#24872 = CARTESIAN_POINT ( 'NONE',  ( 6.000000000000000000, 19.07878402833891229, 4.999999999999997335 ) ) ;
#24874 = ORIENTED_EDGE ( 'NONE', *, *, #37228, .T. ) ;
#24873 = CARTESIAN_POINT ( 'NONE',  ( -10.00000000000000000, 1.224646799147353256E-15, -4.999999999999997335 ) ) ;
#24875 = CARTESIAN_POINT ( 'NONE',  ( 60.63507185982728487, 12.13307030573223599, 44.42928727059375404 ) ) ;
#24876 = ORIENTED_EDGE ( 'NONE', *, *, #31851, .F. ) ;
#24877 = EDGE_LOOP ( 'NONE', ( #37818, #63812, #44840, #57526 ) ) ;
#24878 =( BOUNDED_CURVE ( )  B_SPLINE_CURVE ( 3, ( #60199, #12020, #60551, #1119 ),
 .UNSPECIFIED., .F., .F. ) 
 B_SPLINE_CURVE_WITH_KNOTS ( ( 4, 4 ),
 ( 2.506209174768083692, 3.776976132411494103 ),
 .UNSPECIFIED. ) 
 CURVE ( )  GEOMETRIC_REPRESENTATION_ITEM ( )  RATIONAL_B_SPLINE_CURVE ( ( 1.000000000000000000, 0.8698961108463045822, 0.8698961108463045822, 1.000000000000000000 ) ) 
 REPRESENTATION_ITEM ( '' )  );
#24879 = CARTESIAN_POINT ( 'NONE',  ( 174.1348882614952061, 73.23561817543357222, 39.64404733447431539 ) ) ;
#24880 = EDGE_CURVE ( 'NONE', #20962, #8527, #42147, .T. ) ;
#24881 = CARTESIAN_POINT ( 'NONE',  ( 21.25987915030396636, 6.737472588634913606, -74.99879528645634252 ) ) ;
#24883 = EDGE_LOOP ( 'NONE', ( #42467, #17899 ) ) ;
#24882 = DIRECTION ( 'NONE',  ( -0.000000000000000000, -1.000000000000000000, -0.000000000000000000 ) ) ;
#24884 = CARTESIAN_POINT ( 'NONE',  ( -99.98911906681071571, 32.75458865035245992, 84.54173588161988562 ) ) ;
#24885 = CIRCLE ( 'NONE', #27067, 0.3000000000000051514 ) ;
#24886 = EDGE_CURVE ( 'NONE', #14210, #55930, #60796, .T. ) ;
#24887 = EDGE_CURVE ( 'NONE', #49789, #69259, #65241, .T. ) ;
#24888 = CARTESIAN_POINT ( 'NONE',  ( -71.57025115638936086, 20.80908992785613165, -45.09462308011600129 ) ) ;
#24889 = ADVANCED_FACE ( 'NONE', ( #64197 ), #17037, .T. ) ;
#24890 = ORIENTED_EDGE ( 'NONE', *, *, #46085, .T. ) ;
#24891 = CARTESIAN_POINT ( 'NONE',  ( 212.1976655298228422, 119.0878071902807278, -70.84834327812836818 ) ) ;
#24892 = CIRCLE ( 'NONE', #63095, 5.000000000000004441 ) ;
#24893 = VECTOR ( 'NONE', #63237, 1000.000000000000000 ) ;
#24894 = CARTESIAN_POINT ( 'NONE',  ( 141.3400002717723396, 47.33399859146519617, 37.57801802895147603 ) ) ;
#24895 = DIRECTION ( 'NONE',  ( -1.000000000000000000, 0.000000000000000000, 0.000000000000000000 ) ) ;
#24896 = CARTESIAN_POINT ( 'NONE',  ( 15.78827728214693416, -170.0000000000000000, -50.51894409868581448 ) ) ;
#24897 = CARTESIAN_POINT ( 'NONE',  ( 69.49112875363886133, 15.30845942322119768, -73.85730488686293427 ) ) ;
#24898 = EDGE_LOOP ( 'NONE', ( #55350, #21264, #9061, #21243 ) ) ;
#24899 = ORIENTED_EDGE ( 'NONE', *, *, #45762, .F. ) ;
#24900 = CARTESIAN_POINT ( 'NONE',  ( -145.5195986658808351, 62.16746116576787529, -21.82433970153511282 ) ) ;
#24901 = VECTOR ( 'NONE', #42290, 1000.000000000000000 ) ;
#24902 = CARTESIAN_POINT ( 'NONE',  ( -171.0814041607219451, 84.88598211196838861, -49.44167807983354379 ) ) ;
#24903 = CARTESIAN_POINT ( 'NONE',  ( 412.3372781065085633, 219.4906275429376308, -144.4497041420117682 ) ) ;
#24904 = CARTESIAN_POINT ( 'NONE',  ( 133.8566784816069344, -170.0000000000000000, -70.36786152285935714 ) ) ;
#24905 = FACE_OUTER_BOUND ( 'NONE', #4800, .T. ) ;
#24906 = DIRECTION ( 'NONE',  ( -1.000000000000000000, 0.000000000000000000, 0.000000000000000000 ) ) ;
#24907 = DIRECTION ( 'NONE',  ( 0.8660254037844378194, 0.5000000000000013323, 0.000000000000000000 ) ) ;
#24908 = CARTESIAN_POINT ( 'NONE',  ( -120.0051930351106364, 43.92079660368833061, 42.77160068737919829 ) ) ;
#24909 = CARTESIAN_POINT ( 'NONE',  ( -168.7187482717114051, 82.35796501763488209, -75.14684098565754766 ) ) ;
#24910 = ORIENTED_EDGE ( 'NONE', *, *, #18743, .F. ) ;
#24911 = CARTESIAN_POINT ( 'NONE',  ( -105.4487797565984124, 35.55724615608637862, 31.20524870816166896 ) ) ;
#24912 = ORIENTED_EDGE ( 'NONE', *, *, #15247, .T. ) ;
#24913 = CARTESIAN_POINT ( 'NONE',  ( -178.9255766471344771, 93.82953196344688251, -91.12939640909104355 ) ) ;
#24914 = ORIENTED_EDGE ( 'NONE', *, *, #33696, .F. ) ;
#24915 = CARTESIAN_POINT ( 'NONE',  ( -81.96040367003716653, 23.60340032034881830, -89.55302406663774661 ) ) ;
#24916 = DIRECTION ( 'NONE',  ( -0.2660368455666826670, 0.9639628606958512425, 5.102127870520021228E-18 ) ) ;
#24917 = CARTESIAN_POINT ( 'NONE',  ( -447.6627218934919483, 370.0000000000056275, -141.4497041420121661 ) ) ;
#24918 = CARTESIAN_POINT ( 'NONE',  ( 15.68296563925591514, -63.09411298019745828, 170.0000000000000000 ) ) ;
#24919 = B_SPLINE_CURVE_WITH_KNOTS ( 'NONE', 3,
 ( #26409, #43607, #6329, #65077, #47844, #37640, #61195, #12660, #66489, #39389, #40085, #24264, #65788, #60839, #1763, #50629, #34817, #34121, #50295, #23222, #45709, #13018, #55560, #54856, #67187, #28128, #23907, #17585, #7388, #6681, #44672, #18975, #55211, #34478, #40426, #28843, #39051, #55922, #12311, #61869, #7735, #61541, #17936, #56254 ),
 .UNSPECIFIED., .F., .F.,
 ( 4, 2, 2, 2, 2, 2, 2, 2, 2, 2, 2, 2, 2, 2, 2, 2, 2, 2, 2, 2, 2, 4 ),
 ( 0.02638217555535137329, 0.02805347641364857800, 0.02972477727194578270, 0.03139607813024299088, 0.03306737898854019558, 0.03390302941768881528, 0.03473867984683744192, 0.03640998070513468826, 0.03724563113428332184, 0.03808128156343194848, 0.03891693199258058206, 0.03975258242172921563, 0.04058823285087784227, 0.04142388328002646891, 0.04225953370917509555, 0.04309518413832372219, 0.04476648499662096159, 0.04643778585491820099, 0.04810908671321544039, 0.04978038757151267979, 0.05145168842980991225, 0.05312298928810715165 ),
 .UNSPECIFIED. ) ;
#24920 = CARTESIAN_POINT ( 'NONE',  ( 32.28603806442400526, 7.590310383548726669, 8.149296409025412302 ) ) ;
#24921 = CARTESIAN_POINT ( 'NONE',  ( -13.77312480593389132, 8.361845410302544579, -47.49360053362800471 ) ) ;
#24922 = DIRECTION ( 'NONE',  ( 5.096990367256702165E-18, 2.289061013375335776E-19, -1.000000000000000000 ) ) ;
#24923 = ORIENTED_EDGE ( 'NONE', *, *, #62429, .F. ) ;
#24924 = LINE ( 'NONE', #51655, #8420 ) ;
#24925 = ORIENTED_EDGE ( 'NONE', *, *, #1009, .T. ) ;
#24926 = FACE_OUTER_BOUND ( 'NONE', #65253, .T. ) ;
#24927 = CARTESIAN_POINT ( 'NONE',  ( -56.73868929054667376, 16.18382781951277138, 71.97397694089359277 ) ) ;
#24928 = CARTESIAN_POINT ( 'NONE',  ( -24.94151142167917712, 8.614613465433007988, 7.093782003634580668 ) ) ;
#24929 = VERTEX_POINT ( 'NONE', #16006 ) ;
#24930 = CYLINDRICAL_SURFACE ( 'NONE', #26617, 35.00000000000000000 ) ;
#24931 = CARTESIAN_POINT ( 'NONE',  ( -59.09409272559887683, 15.80233242102493918, -90.08371057033618001 ) ) ;
#24932 = CARTESIAN_POINT ( 'NONE',  ( -38.15923928782687824, 10.79140400702259406, 41.05568229944667991 ) ) ;
#24933 = SURFACE_STYLE_USAGE ( .BOTH. , #3472 ) ;
#24934 = ADVANCED_FACE ( 'NONE', ( #1225 ), #27953, .F. ) ;
#24935 = ORIENTED_EDGE ( 'NONE', *, *, #58344, .T. ) ;
#24936 = DIRECTION ( 'NONE',  ( 1.005272254328559711E-14, -0.9999999999999998890, -3.996802888650563546E-15 ) ) ;
#24937 = PLANE ( 'NONE',  #32962 ) ;
#24938 = CARTESIAN_POINT ( 'NONE',  ( -121.2008155373973892, 43.48033530165985638, 32.24946013892020602 ) ) ;
#24939 = CARTESIAN_POINT ( 'NONE',  ( 0.3173508448886560029, 8.480771745766405800, 1.310872448937997259 ) ) ;
#24940 = EDGE_LOOP ( 'NONE', ( #24299, #11934, #39262, #60059 ) ) ;
#24941 = CYLINDRICAL_SURFACE ( 'NONE', #49233, 65.00000000000000000 ) ;
#24942 = AXIS2_PLACEMENT_3D ( 'NONE', #42262, #41566, #32398 ) ;
#24943 = CARTESIAN_POINT ( 'NONE',  ( 133.2949513180626298, 42.25961182073308464, 83.19458329861414825 ) ) ;
#24944 = EDGE_CURVE ( 'NONE', #5719, #30890, #38506, .T. ) ;
#24945 = PRODUCT_DEFINITION_SHAPE ( 'NONE', 'NONE',  #69586 ) ;
#24947 = ADVANCED_FACE ( 'NONE', ( #528 ), #21976, .T. ) ;
#24946 = CARTESIAN_POINT ( 'NONE',  ( 116.6457744947906860, 31.95847117670278692, 33.19741688322386608 ) ) ;
#24948 = B_SPLINE_CURVE_WITH_KNOTS ( 'NONE', 3,
 ( #37555, #53032, #68865, #10823, #68540, #10475, #42493, #42148, #26323, #5544, #26999, #63610, #20343, #48429, #57645, #15420, #36531, #263, #57985, #41468, #31945, #62922, #69218, #58316, #14722, #9802, #31263, #36186, #53373, #4516, #25979, #47411, #10135, #31592, #21043, #34028, #32631, #54765, #22421, #22075, #38246, #43515, #44210, #65695, #39304 ),
 .UNSPECIFIED., .F., .F.,
 ( 4, 2, 2, 1, 2, 2, 2, 2, 2, 2, 2, 2, 2, 2, 2, 2, 2, 2, 2, 2, 2, 2, 4 ),
 ( 0.02348395315094739533, 0.02495010856601299204, 0.02568318627354579040, 0.02641626398107858528, 0.02714934168861138364, 0.02788241939614417852, 0.02934857481120976483, 0.03008165251874255625, 0.03081473022627535113, 0.03228088564134094091, 0.03301396334887373579, 0.03374704105640652374, 0.03521319647147211351, 0.03667935188653769635, 0.03741242959407048430, 0.03814550730160327918, 0.03961166271666885508, 0.04107781813173443791, 0.04254397354680002075, 0.04327705125433280176, 0.04401012896186559664, 0.04547628437693117254, 0.04694243979199674843 ),
 .UNSPECIFIED. ) ;
#24949 = AXIS2_PLACEMENT_3D ( 'NONE', #49616, #17264, #39096 ) ;
#24951 = STYLED_ITEM ( 'NONE', ( #35913 ), #17690 ) ;
#24950 = DIRECTION ( 'NONE',  ( -0.000000000000000000, -0.000000000000000000, -1.000000000000000000 ) ) ;
#24952 = EDGE_CURVE ( 'NONE', #27671, #50073, #9562, .T. ) ;
#24953 = CARTESIAN_POINT ( 'NONE',  ( -118.3927673406137586, 41.74929850983308199, -69.02033445283595370 ) ) ;
#24954 = CIRCLE ( 'NONE', #66393, 300.0000000000000000 ) ;
#24955 = EDGE_CURVE ( 'NONE', #45299, #17268, #10380, .T. ) ;
#24956 = ORIENTED_EDGE ( 'NONE', *, *, #60521, .T. ) ;
#24957 = CARTESIAN_POINT ( 'NONE',  ( -3.000000000000006217, 2.936090700955778569E-15, 23.97499999999999787 ) ) ;
#24958 = CARTESIAN_POINT ( 'NONE',  ( 111.1767565371974769, 29.31586421952252053, -77.72348245422179502 ) ) ;
#24959 = DIRECTION ( 'NONE',  ( 0.000000000000000000, 0.000000000000000000, -1.000000000000000000 ) ) ;
#24960 = CARTESIAN_POINT ( 'NONE',  ( 133.8566784816069060, 42.60093787723653236, 2.665790248531674678 ) ) ;
#24961 = DIRECTION ( 'NONE',  ( 1.000000000000000000, 0.000000000000000000, 0.000000000000000000 ) ) ;
#24962 = CLOSED_SHELL ( 'NONE', ( #33525, #28753, #47220, #56709, #44214, #38210, #22698, #50856, #13299, #20495, #38344, #69389, #48124, #22682, #16983, #65683, #42644, #3041, #6911, #19118, #38202, #27699 ) ) ;
#24963 = ORIENTED_EDGE ( 'NONE', *, *, #24320, .F. ) ;
#24964 = CARTESIAN_POINT ( 'NONE',  ( 12.93264331410902379, 21.39501663729252456, 0.000000000000000000 ) ) ;
#24965 = VERTEX_POINT ( 'NONE', #39905 ) ;
#24966 = CARTESIAN_POINT ( 'NONE',  ( 70.26936813788617542, 15.51386666370914824, 62.18728408539558217 ) ) ;
#24967 = DIRECTION ( 'NONE',  ( -1.000000000000000000, -1.001918046209079887E-14, 9.729495617646301779E-15 ) ) ;
#24969 = ORIENTED_EDGE ( 'NONE', *, *, #7023, .T. ) ;
#24968 = DIRECTION ( 'NONE',  ( 0.000000000000000000, 0.000000000000000000, -1.000000000000000000 ) ) ;
#24970 = CARTESIAN_POINT ( 'NONE',  ( -12.50000000000002842, -18.06806526123148160, 378.0000000000000000 ) ) ;
#24971 = CARTESIAN_POINT ( 'NONE',  ( 230.9999999999999432, -57.00000000000007816, -2.000000000000000000 ) ) ;
#24972 = EDGE_CURVE ( 'NONE', #14304, #29783, #34291, .T. ) ;
#24973 = ADVANCED_FACE ( 'NONE', ( #28300 ), #38870, .F. ) ;
#24974 = CARTESIAN_POINT ( 'NONE',  ( 162.8142581494936110, 61.92799983924231810, -38.34020306277995616 ) ) ;
#24975 = ORIENTED_EDGE ( 'NONE', *, *, #62829, .T. ) ;
#24976 = EDGE_CURVE ( 'NONE', #43408, #44889, #29799, .T. ) ;
#24977 = DIRECTION ( 'NONE',  ( -0.04486483035051863633, 0.9989930665413144784, 0.000000000000000000 ) ) ;
#24978 = LINE ( 'NONE', #42767, #14390 ) ;
#24979 = CARTESIAN_POINT ( 'NONE',  ( 150.9494776551346149, 53.99791200760193988, -93.60193293775073187 ) ) ;
#24980 = FACE_OUTER_BOUND ( 'NONE', #13865, .T. ) ;
#24981 = CARTESIAN_POINT ( 'NONE',  ( -167.9889421625799741, 81.59140042431236850, 32.83227558599013207 ) ) ;
#24982 = B_SPLINE_CURVE_WITH_KNOTS ( 'NONE', 3,
 ( #59028, #58338, #63636, #63289 ),
 .UNSPECIFIED., .F., .F.,
 ( 4, 4 ),
 ( 9.900409499076797036E-07, 0.05658314289920114010 ),
 .UNSPECIFIED. ) ;
#24983 = CARTESIAN_POINT ( 'NONE',  ( 26.11269837220800127, -31.11269837220812562, 0.000000000000000000 ) ) ;
#24984 = CARTESIAN_POINT ( 'NONE',  ( 92.20490818459941806, 22.47175429302964744, 42.25219620519190755 ) ) ;
#24985 = ORIENTED_EDGE ( 'NONE', *, *, #58756, .T. ) ;
#24986 = CARTESIAN_POINT ( 'NONE',  ( -102.2801239173131052, 33.91021738430207222, 57.36362509687880618 ) ) ;
#24987 = CARTESIAN_POINT ( 'NONE',  ( -15.13211202216340823, 8.488266782358833140, 62.75077677020096445 ) ) ;
#24988 = ORIENTED_EDGE ( 'NONE', *, *, #67667, .T. ) ;
#24989 = AXIS2_PLACEMENT_3D ( 'NONE', #3486, #3157, #57992 ) ;
#24990 = CARTESIAN_POINT ( 'NONE',  ( 157.4703587214989113, 58.92748579479258808, -24.27963370867398396 ) ) ;
#24991 = CARTESIAN_POINT ( 'NONE',  ( 212.1913428512247322, 119.0779339498138114, -17.33593461546083603 ) ) ;
#24992 = CARTESIAN_POINT ( 'NONE',  ( 103.9685899589048290, 27.18106603025993095, 32.99486883808148008 ) ) ;
#24993 = STYLED_ITEM ( 'NONE', ( #58355 ), #20791 ) ;
#24994 = CARTESIAN_POINT ( 'NONE',  ( -6.840165690716691671, 7.836465889224642822, 30.16447760598867944 ) ) ;
#24995 = CARTESIAN_POINT ( 'NONE',  ( 60.45761612245340899, 12.09376662961991578, 83.94407422121982165 ) ) ;
#24996 = CARTESIAN_POINT ( 'NONE',  ( 187.2296622856351576, 86.53808614709456037, 5.657001796427024942 ) ) ;
#24997 = CARTESIAN_POINT ( 'NONE',  ( 212.0047492081760936, 116.9348962082588343, -45.54691903256296115 ) ) ;
#24999 = DIRECTION ( 'NONE',  ( 0.000000000000000000, 0.000000000000000000, 1.000000000000000000 ) ) ;
#24998 = CIRCLE ( 'NONE', #55301, 246.3582898394607525 ) ;
#25000 = CARTESIAN_POINT ( 'NONE',  ( -61.52143283897137849, 16.51181063611436528, 7.169046980359220278 ) ) ;
#25001 = ORIENTED_EDGE ( 'NONE', *, *, #26286, .T. ) ;
#25002 = FACE_OUTER_BOUND ( 'NONE', #18266, .T. ) ;
#25003 = ORIENTED_EDGE ( 'NONE', *, *, #21072, .F. ) ;
#25004 = DIRECTION ( 'NONE',  ( 1.000000000000000000, 0.000000000000000000, 0.000000000000000000 ) ) ;
#25005 = LINE ( 'NONE', #35552, #56810 ) ;
#25006 = CARTESIAN_POINT ( 'NONE',  ( -51.66904755831212981, -10.55634918610397222, 85.00100000000000477 ) ) ;
#25007 = CARTESIAN_POINT ( 'NONE',  ( -3.544435206134087135, 6.649906604172325153, 85.13781338574963797 ) ) ;
#25008 = AXIS2_PLACEMENT_3D ( 'NONE', #52962, #4787, #47683 ) ;
#25009 = CARTESIAN_POINT ( 'NONE',  ( 0.000000000000000000, 0.000000000000000000, -8.949444346342716017 ) ) ;
#25010 = ORIENTED_EDGE ( 'NONE', *, *, #24955, .T. ) ;
#25011 = CARTESIAN_POINT ( 'NONE',  ( 6.564829507346109594, 24.24955267099648992, 3.061616997868437868E-16 ) ) ;
#25012 = CARTESIAN_POINT ( 'NONE',  ( 8.828807734114020533, 74.48902371486721563, 170.0000000000000000 ) ) ;
#25013 = ORIENTED_EDGE ( 'NONE', *, *, #45188, .T. ) ;
#25014 = EDGE_LOOP ( 'NONE', ( #38138, #47832, #43400, #8505 ) ) ;
#25015 = DIRECTION ( 'NONE',  ( -0.000000000000000000, -0.000000000000000000, -1.000000000000000000 ) ) ;
#25016 = LINE ( 'NONE', #3216, #69238 ) ;
#25017 = CARTESIAN_POINT ( 'NONE',  ( 173.5843421840238534, 71.34465141434344559, -16.57726541804536069 ) ) ;
#25018 = CARTESIAN_POINT ( 'NONE',  ( -167.6524579626394598, 82.69702609844092933, 60.02780465990404934 ) ) ;
#25019 = EDGE_CURVE ( 'NONE', #66403, #30796, #66316, .T. ) ;
#25020 = DIRECTION ( 'NONE',  ( 1.000000000000000000, 0.000000000000000000, 0.000000000000000000 ) ) ;
#25021 = CARTESIAN_POINT ( 'NONE',  ( 59.08202327466404569, 12.82375733818951247, -9.985768006214025050 ) ) ;
#25022 = VERTEX_POINT ( 'NONE', #61011 ) ;
#25023 = LINE ( 'NONE', #23975, #6436 ) ;
#25024 = VERTEX_POINT ( 'NONE', #50461 ) ;
#25025 = CARTESIAN_POINT ( 'NONE',  ( 205.5004956747122264, 107.4493581495447927, 2.395320917533355409 ) ) ;
#25026 = DIRECTION ( 'NONE',  ( 1.000000000000000000, 0.000000000000000000, 0.000000000000000000 ) ) ;
#25027 = CARTESIAN_POINT ( 'NONE',  ( 206.6955592216991420, 109.1214665502618004, 29.46719048026987764 ) ) ;
#25028 = CARTESIAN_POINT ( 'NONE',  ( 14.94784401874210822, 6.475021042546637240, -89.24363180946468788 ) ) ;
#25029 = EDGE_CURVE ( 'NONE', #31022, #55566, #49739, .T. ) ;
#25030 = EDGE_CURVE ( 'NONE', #67530, #62756, #56764, .T. ) ;
#25031 = ORIENTED_EDGE ( 'NONE', *, *, #49375, .T. ) ;
#25032 = EDGE_CURVE ( 'NONE', #65565, #12486, #60661, .T. ) ;
#25033 = ORIENTED_EDGE ( 'NONE', *, *, #31787, .T. ) ;
#25034 = CARTESIAN_POINT ( 'NONE',  ( 113.9749324730388622, -21.78918450429459241, 3.050527833458433591 ) ) ;
#25035 = CARTESIAN_POINT ( 'NONE',  ( 29.69502258243350923, 57.82046033912877903, 170.0000000000000000 ) ) ;
#25036 = AXIS2_PLACEMENT_3D ( 'NONE', #29613, #46136, #34573 ) ;
#25037 = DIRECTION ( 'NONE',  ( -0.6910626489868580968, -0.7227948638273978821, 0.000000000000000000 ) ) ;
#25038 = CYLINDRICAL_SURFACE ( 'NONE', #15230, 7.500000000000020428 ) ;
#25039 = CARTESIAN_POINT ( 'NONE',  ( 22.84965234755525287, 6.829418951222932854, 88.65540587631463154 ) ) ;
#25040 = CARTESIAN_POINT ( 'NONE',  ( 82.74007713545064746, 18.13042311233562032, -76.58347899170844642 ) ) ;
#25041 = AXIS2_PLACEMENT_3D ( 'NONE', #25237, #46675, #9743 ) ;
#25042 = ORIENTED_EDGE ( 'NONE', *, *, #1162, .F. ) ;
#25043 = DIRECTION ( 'NONE',  ( -1.000000000000000000, 0.000000000000000000, 0.000000000000000000 ) ) ;
#25044 = CARTESIAN_POINT ( 'NONE',  ( 197.2847860006354779, 98.30530166401518954, -44.97716114296652989 ) ) ;
#25045 = EDGE_LOOP ( 'NONE', ( #41482, #58863, #31310, #40439 ) ) ;
#25046 = VECTOR ( 'NONE', #32275, 1000.000000000000000 ) ;
#25047 = CYLINDRICAL_SURFACE ( 'NONE', #47445, 7.500000000000020428 ) ;
#25048 = VERTEX_POINT ( 'NONE', #2618 ) ;
#25049 = CARTESIAN_POINT ( 'NONE',  ( -85.90441187606244000, 25.21188850826090899, -67.43018938941865770 ) ) ;
#25050 = CYLINDRICAL_SURFACE ( 'NONE', #5073, 65.36598343705435354 ) ;
#25051 = CIRCLE ( 'NONE', #57679, 242.4895526022646379 ) ;
#25052 = ORIENTED_EDGE ( 'NONE', *, *, #26667, .T. ) ;
#25053 = B_SPLINE_CURVE_WITH_KNOTS ( 'NONE', 3,
 ( #21806, #11249, #43250, #54499, #4946, #21462, #54145, #42906 ),
 .UNSPECIFIED., .F., .F.,
 ( 4, 2, 2, 4 ),
 ( 0.004673709593152147908, 0.005837709341827640799, 0.007001709090503134558, 0.009329708587854120341 ),
 .UNSPECIFIED. ) ;
#25054 = VECTOR ( 'NONE', #14935, 1000.000000000000000 ) ;
#25055 = VERTEX_POINT ( 'NONE', #24082 ) ;
#25056 = CARTESIAN_POINT ( 'NONE',  ( 9.827939172326077610, 6.382931149346553923, -38.43989651470956659 ) ) ;
#25057 = DIRECTION ( 'NONE',  ( 0.7071067811865475727, 5.551115123125781470E-17, -0.7071067811865474617 ) ) ;
#25058 = CARTESIAN_POINT ( 'NONE',  ( 20.36314374176837561, 6.689939636827347158, 4.706573874584005779 ) ) ;
#25059 = ORIENTED_EDGE ( 'NONE', *, *, #7324, .F. ) ;
#25060 = EDGE_CURVE ( 'NONE', #51452, #42318, #12478, .T. ) ;
#25061 = CARTESIAN_POINT ( 'NONE',  ( -63.73419499958981049, -12.83646726144931449, 170.0000000000000000 ) ) ;
#25062 = CARTESIAN_POINT ( 'NONE',  ( 173.7225111622554721, 72.84868911716897344, -69.10599538675619158 ) ) ;
#25063 = DIRECTION ( 'NONE',  ( -0.000000000000000000, -0.000000000000000000, -1.000000000000000000 ) ) ;
#25064 = CARTESIAN_POINT ( 'NONE',  ( 103.9652201950894721, 26.08439499369982428, -39.31135386676266563 ) ) ;
#25065 = CARTESIAN_POINT ( 'NONE',  ( 84.05289558242219528, 19.61733656419350069, -50.36921807815809160 ) ) ;
#25066 = CARTESIAN_POINT ( 'NONE',  ( -165.7102224864505615, 80.67993370857061564, -94.71298376253034235 ) ) ;
#25067 = ORIENTED_EDGE ( 'NONE', *, *, #42256, .T. ) ;
#25068 = VERTEX_POINT ( 'NONE', #1941 ) ;
#25069 = CARTESIAN_POINT ( 'NONE',  ( 40.38414441725701209, 8.538832720399536669, 18.02099439841263973 ) ) ;
#25070 = DIRECTION ( 'NONE',  ( -9.109522253334599209E-16, -1.000000000000000000, 0.000000000000000000 ) ) ;
#25071 = PLANE ( 'NONE',  #30112 ) ;
#25072 = DIRECTION ( 'NONE',  ( 1.000000000000000000, 0.000000000000000000, 0.000000000000000000 ) ) ;
#25073 = CARTESIAN_POINT ( 'NONE',  ( 7.632783294297949638E-15, 0.000000000000000000, 55.00000000000001421 ) ) ;
#25074 = CARTESIAN_POINT ( 'NONE',  ( -156.9252506979472912, 70.73559306219775067, 10.23206411029071461 ) ) ;
#25075 = CARTESIAN_POINT ( 'NONE',  ( -118.8392474096542486, 43.20060570451231285, -71.85748745244474378 ) ) ;
#25076 = CARTESIAN_POINT ( 'NONE',  ( 212.1734186221015932, 119.0499290057855291, 37.39989276221264447 ) ) ;
#25077 = CARTESIAN_POINT ( 'NONE',  ( -76.31381168750405664, 21.43908608416557726, -62.32252567794670028 ) ) ;
#25079 = DIRECTION ( 'NONE',  ( -0.000000000000000000, 1.000000000000000000, -0.000000000000000000 ) ) ;
#25078 = B_SPLINE_CURVE_WITH_KNOTS ( 'NONE', 3,
 ( #22624, #50056, #59893, #60261, #55322, #39506 ),
 .UNSPECIFIED., .F., .F.,
 ( 4, 2, 4 ),
 ( 2.380731629581200700E-07, 0.002336973833157563775, 0.004673709593152168724 ),
 .UNSPECIFIED. ) ;
#25080 = ORIENTED_EDGE ( 'NONE', *, *, #32573, .F. ) ;
#25081 =( GEOMETRIC_REPRESENTATION_CONTEXT ( 3 ) GLOBAL_UNCERTAINTY_ASSIGNED_CONTEXT ( ( #61342 ) ) GLOBAL_UNIT_ASSIGNED_CONTEXT ( ( #17832, #44191, #16771 ) ) REPRESENTATION_CONTEXT ( 'NONE', 'WORKASPACE' ) );
#25082 = CARTESIAN_POINT ( 'NONE',  ( 12.46490660984525611, 7.423426948220648747, -9.446422529437963789 ) ) ;
#25083 = ORIENTED_EDGE ( 'NONE', *, *, #59378, .T. ) ;
#25084 = CARTESIAN_POINT ( 'NONE',  ( 197.3707490726349647, 96.80690576410101755, -15.34896122626384596 ) ) ;
#25085 = ORIENTED_EDGE ( 'NONE', *, *, #2634, .T. ) ;
#25086 = FACE_OUTER_BOUND ( 'NONE', #32574, .T. ) ;
#25087 = CARTESIAN_POINT ( 'NONE',  ( -31.11269837220806878, 5.000000000000056843, 85.00100000000000477 ) ) ;
#25088 = CARTESIAN_POINT ( 'NONE',  ( -142.9843132609582597, 60.12226089556228459, 68.77572048107622038 ) ) ;
#25089 = FACE_OUTER_BOUND ( 'NONE', #24826, .T. ) ;
#25090 = CARTESIAN_POINT ( 'NONE',  ( 204.6977192012829789, 108.0580384837234931, -90.01503221354883522 ) ) ;
#25091 = CONICAL_SURFACE ( 'NONE', #22811, 8.000000000000000000, 1.047197551196600296 ) ;
#25092 = DIRECTION ( 'NONE',  ( -1.000000000000000000, 0.000000000000000000, 0.000000000000000000 ) ) ;
#25093 = CARTESIAN_POINT ( 'NONE',  ( 12.68603346975294954, 7.427591953486043508, -36.18624911206273254 ) ) ;
#25094 = CARTESIAN_POINT ( 'NONE',  ( 311.9975424824652350, 170.0000000000000284, 380.0000000000001137 ) ) ;
#25095 = VERTEX_POINT ( 'NONE', #60313 ) ;
#25096 = ADVANCED_FACE ( 'NONE', ( #23729 ), #33941, .F. ) ;
#25097 = VERTEX_POINT ( 'NONE', #55737 ) ;
#25098 = EDGE_CURVE ( 'NONE', #19832, #60092, #18601, .T. ) ;
#25099 = VECTOR ( 'NONE', #65152, 1000.000000000000114 ) ;
#25100 = CARTESIAN_POINT ( 'NONE',  ( -4.180838820195677208, -65.23214221112785083, 6.377659838150132077E-18 ) ) ;
#25101 = DIRECTION ( 'NONE',  ( 0.000000000000000000, 1.000000000000000000, 0.000000000000000000 ) ) ;
#25102 = EDGE_CURVE ( 'NONE', #18664, #17986, #61700, .T. ) ;
#25103 = VECTOR ( 'NONE', #47487, 1000.000000000000000 ) ;
#25104 = LINE ( 'NONE', #9611, #48688 ) ;
#25105 = ADVANCED_FACE ( 'NONE', ( #34979 ), #51160, .T. ) ;
#25106 = VECTOR ( 'NONE', #32595, 1000.000000000000000 ) ;
#25107 = PLANE ( 'NONE',  #12684 ) ;
#25108 = CARTESIAN_POINT ( 'NONE',  ( 11.30618213853385967, 74.15344055032308290, 43.58025477438756212 ) ) ;
#25109 = B_SPLINE_CURVE_WITH_KNOTS ( 'NONE', 3,
 ( #54744, #44898, #17459, #27666, #18518, #34005 ),
 .UNSPECIFIED., .F., .F.,
 ( 4, 2, 4 ),
 ( 0.03218941534092201184, 0.06469837595388618079, 0.09720733656685034973 ),
 .UNSPECIFIED. ) ;
#25110 = CARTESIAN_POINT ( 'NONE',  ( 15.78827728214693416, 6.500811158483284835, 56.85925826316891829 ) ) ;
#25111 = CARTESIAN_POINT ( 'NONE',  ( 210.5008983495072243, 116.4753531594350733, 14.62071003477614539 ) ) ;
#25112 = CARTESIAN_POINT ( 'NONE',  ( -180.5230320745700965, 95.76406004447552789, -43.46080055680893395 ) ) ;
#25113 = CARTESIAN_POINT ( 'NONE',  ( 89.22118407503262461, 20.32164250407901207, -9.435028923643752563 ) ) ;
#25114 = CARTESIAN_POINT ( 'NONE',  ( -25.48750459758501918, 9.705678256319572483, 59.97090248023433645 ) ) ;
#25115 = LINE ( 'NONE', #9621, #14934 ) ;
#25116 = CARTESIAN_POINT ( 'NONE',  ( -53.38256734720888375, 14.24001356352780689, 57.34620933837434364 ) ) ;
#25117 = B_SPLINE_CURVE_WITH_KNOTS ( 'NONE', 3,
 ( #9907, #53132, #53479, #10234, #63716, #69329, #31024, #9559, #31361, #52463, #15528, #26425, #368, #21152, #20442, #5310, #47867, #10576, #36981, #4285, #25748, #21476, #26769, #47178, #4961, #47510, #63371, #42597, #52792, #64049, #15860, #15179, #32397, #42922, #63018, #37307, #68636, #36642, #31697, #4616, #58418, #26080, #41908, #22, #20795, #53822 ),
 .UNSPECIFIED., .F., .F.,
 ( 4, 2, 2, 2, 2, 2, 2, 2, 2, 2, 2, 2, 2, 2, 2, 2, 2, 2, 2, 2, 2, 2, 4 ),
 ( 1.387778780781445676E-17, 0.003736383952885407537, 0.005604575929328104583, 0.007472767905770801196, 0.008406863893992139528, 0.009340959882213476992, 0.01120915185865615366, 0.01214324784687749979, 0.01307734383509884593, 0.01401143982332018860, 0.01494553581154153474, 0.01587963179976283751, 0.01681372778798414028, 0.01774782377620543958, 0.01868191976442676316, 0.01961601575264808675, 0.02055011174086940687, 0.02148420772909072698, 0.02241830371731204710, 0.02428649569375476713, 0.02615468767019748370, 0.02802287964664020026, 0.02989107162308291682 ),
 .UNSPECIFIED. ) ;
#25118 = ADVANCED_FACE ( 'NONE', ( #39562 ), #29021, .F. ) ;
#25119 = FACE_OUTER_BOUND ( 'NONE', #4121, .T. ) ;
#25120 = ORIENTED_EDGE ( 'NONE', *, *, #29225, .F. ) ;
#25121 = EDGE_CURVE ( 'NONE', #24590, #3542, #2874, .T. ) ;
#25122 = DIRECTION ( 'NONE',  ( -0.000000000000000000, -0.000000000000000000, -1.000000000000000000 ) ) ;
#25123 = CARTESIAN_POINT ( 'NONE',  ( 155.7265855639938650, 57.57443315515123317, 56.44615811012038620 ) ) ;
#25124 = CARTESIAN_POINT ( 'NONE',  ( -108.9145525555662743, 37.42858360505778847, -72.86609022197936270 ) ) ;
#25125 = CARTESIAN_POINT ( 'NONE',  ( -50.52927270563905182, 13.51486287463704450, -48.71881382000154304 ) ) ;
#25126 = PLANE ( 'NONE',  #31254 ) ;
#25127 = CARTESIAN_POINT ( 'NONE',  ( -0.7313957694713866253, 7.539606919072873836, 93.82462488541915491 ) ) ;
#25128 = ORIENTED_EDGE ( 'NONE', *, *, #63975, .F. ) ;
#25129 = CARTESIAN_POINT ( 'NONE',  ( -190.5273690078732329, 108.8856264335149859, -91.58113276652414925 ) ) ;
#25130 = FACE_OUTER_BOUND ( 'NONE', #21010, .T. ) ;
#25131 = ORIENTED_EDGE ( 'NONE', *, *, #7779, .T. ) ;
#25132 = ORIENTED_EDGE ( 'NONE', *, *, #41862, .F. ) ;
#25133 = VECTOR ( 'NONE', #13849, 1000.000000000000000 ) ;
#25134 = DIRECTION ( 'NONE',  ( -0.000000000000000000, -0.000000000000000000, -1.000000000000000000 ) ) ;
#25135 = CARTESIAN_POINT ( 'NONE',  ( -180.6011569556095822, 95.85968111394265634, -69.68656036792953046 ) ) ;
#25136 = DIRECTION ( 'NONE',  ( -1.000000000000000000, 0.000000000000000000, 0.000000000000000000 ) ) ;
#25137 = ORIENTED_EDGE ( 'NONE', *, *, #14642, .T. ) ;
#25138 = CARTESIAN_POINT ( 'NONE',  ( 61.62594073580573450, -21.79346734964915555, 43.58025477438756212 ) ) ;
#25139 = CARTESIAN_POINT ( 'NONE',  ( 21.98745393275190807, 71.71550996510528364, 73.58025477438755502 ) ) ;
#25140 = CARTESIAN_POINT ( 'NONE',  ( -5.871577929436022636, 6.771181646175755908, 18.02891427094515464 ) ) ;
#25141 = STYLED_ITEM ( 'NONE', ( #56926 ), #40015 ) ;
#25142 = CARTESIAN_POINT ( 'NONE',  ( 57.41085175769453741, 12.46982565415947697, -48.21039516881924669 ) ) ;
#25143 = LINE ( 'NONE', #67023, #4529 ) ;
#25144 = CARTESIAN_POINT ( 'NONE',  ( 152.1847562093922193, 53.65517908050956208, 85.26709633804618704 ) ) ;
#25145 = VECTOR ( 'NONE', #53081, 1000.000000000000000 ) ;
#25146 = CARTESIAN_POINT ( 'NONE',  ( 137.4117721579687839, 43.61242559081431835, 16.78681578490248327 ) ) ;
#25147 = VECTOR ( 'NONE', #24141, 1000.000000000000000 ) ;
#25148 = VERTEX_POINT ( 'NONE', #56780 ) ;
#25149 = AXIS2_PLACEMENT_3D ( 'NONE', #21215, #58830, #14889 ) ;
#25150 = CARTESIAN_POINT ( 'NONE',  ( -1.007969207232617206E-15, -0.7818963812180719231, 7.999999999999996447 ) ) ;
#25151 = AXIS2_PLACEMENT_3D ( 'NONE', #31684, #69315, #60843 ) ;
#25152 = CARTESIAN_POINT ( 'NONE',  ( 8.540853903193189822, 6.376814430361481989, 66.30478470236579369 ) ) ;
#25153 = CARTESIAN_POINT ( 'NONE',  ( 202.7540649946182896, 105.3989460363904698, 29.45258215039039484 ) ) ;
#25154 = CARTESIAN_POINT ( 'NONE',  ( -71.19449361276183197, 20.67900126374447467, 90.88156997529951298 ) ) ;
#25156 = ORIENTED_EDGE ( 'NONE', *, *, #14638, .T. ) ;
#25155 = CARTESIAN_POINT ( 'NONE',  ( -118.4669749820149605, 41.79437899234314813, 90.71051623639903028 ) ) ;
#25157 = CARTESIAN_POINT ( 'NONE',  ( 64.69738688745242428, 14.10375742873389093, 44.62596110400481564 ) ) ;
#25158 = ORIENTED_EDGE ( 'NONE', *, *, #6741, .T. ) ;
#25159 = AXIS2_PLACEMENT_3D ( 'NONE', #44364, #65847, #11656 ) ;
#25160 = ORIENTED_EDGE ( 'NONE', *, *, #54935, .F. ) ;
#25161 = CARTESIAN_POINT ( 'NONE',  ( -144.2029146819478456, 59.80706661873674079, 70.38930589792778392 ) ) ;
#25162 = CARTESIAN_POINT ( 'NONE',  ( 217.9999999999999716, 128.6235316737731296, -95.00000000000133582 ) ) ;
#25163 = DIRECTION ( 'NONE',  ( -0.000000000000000000, -0.000000000000000000, 1.000000000000000000 ) ) ;
#25164 = CARTESIAN_POINT ( 'NONE',  ( 15.78827728214693771, 7.507518794609575608, -62.36349468914946925 ) ) ;
#25165 = CARTESIAN_POINT ( 'NONE',  ( -122.7930600691577894, 44.48546375740912140, 71.80916449259312628 ) ) ;
#25166 = DIRECTION ( 'NONE',  ( 0.000000000000000000, 0.000000000000000000, 1.000000000000000000 ) ) ;
#25167 = CARTESIAN_POINT ( 'NONE',  ( 21.89475364395364565, 7.780723588097695043, -92.33322761029084802 ) ) ;
#25168 = B_SPLINE_CURVE_WITH_KNOTS ( 'NONE', 3,
 ( #50968, #67847, #29167, #13676, #28825, #55900, #18262, #45338, #24598, #8053, #66470, #46030, #35131, #35483, #40750, #24932, #50275, #50616, #29859, #51664, #56587, #61175, #41108, #34462, #8408, #39720, #30213, #46366, #13002, #67497, #29504, #24250, #40068, #7719, #19293, #61523, #19644, #2099, #62207, #56945, #2434, #3471, #23891, #45693 ),
 .UNSPECIFIED., .F., .F.,
 ( 4, 2, 2, 2, 2, 2, 2, 2, 2, 2, 2, 2, 2, 2, 2, 2, 2, 2, 2, 2, 2, 4 ),
 ( 6.938893903907228378E-18, 0.001476829494128773521, 0.002215244241193168630, 0.002953658988257563522, 0.004430488482386362413, 0.005907317976515161738, 0.007384147470643961063, 0.008122562217708370266, 0.008860976964772776868, 0.01033780645890160395, 0.01181463595303043276, 0.01255305070009485324, 0.01329146544715927719, 0.01476829494128812509, 0.01550670968835255251, 0.01624512443541697992, 0.01772195392954586599, 0.01919878342367475205, 0.01993719817073918640, 0.02067561291780362076, 0.02215244241193247213, 0.02362927190606132002 ),
 .UNSPECIFIED. ) ;
#25169 = CARTESIAN_POINT ( 'NONE',  ( -47.55256438668344288, 13.83151366677316219, 37.57512454685291914 ) ) ;
#25170 = EDGE_LOOP ( 'NONE', ( #52181, #7594, #42259, #33081 ) ) ;
#25171 = ORIENTED_EDGE ( 'NONE', *, *, #3754, .T. ) ;
#25172 = PLANE ( 'NONE',  #2831 ) ;
#25173 = DIRECTION ( 'NONE',  ( -1.000000000000000000, 0.000000000000000000, 0.000000000000000000 ) ) ;
#25174 = DIRECTION ( 'NONE',  ( 0.000000000000000000, 0.000000000000000000, 1.000000000000000000 ) ) ;
#25175 = CARTESIAN_POINT ( 'NONE',  ( 76.57571471437145760, 0.000000000000000000, -20.00000000000000000 ) ) ;
#25176 = DIRECTION ( 'NONE',  ( -0.000000000000000000, -0.000000000000000000, -1.000000000000000000 ) ) ;
#25177 = CARTESIAN_POINT ( 'NONE',  ( -1.666933348992582609, 64.97862212458815634, 133.5802547743875550 ) ) ;
#25178 = CARTESIAN_POINT ( 'NONE',  ( -145.4282275380300575, 62.09266785189831239, 85.60967048720104344 ) ) ;
#25179 = ORIENTED_EDGE ( 'NONE', *, *, #41634, .F. ) ;
#25180 = ORIENTED_EDGE ( 'NONE', *, *, #53016, .T. ) ;
#25181 = EDGE_CURVE ( 'NONE', #51034, #14895, #56566, .T. ) ;
#25182 = ORIENTED_EDGE ( 'NONE', *, *, #8591, .T. ) ;
#25183 = CIRCLE ( 'NONE', #6015, 4.999999999999997335 ) ;
#25184 = CARTESIAN_POINT ( 'NONE',  ( -12.50000000000002842, 207.5000000000000284, -2.000000000000000000 ) ) ;
#25185 = ADVANCED_FACE ( 'NONE', ( #57126 ), #31089, .F. ) ;
#25186 = CARTESIAN_POINT ( 'NONE',  ( 174.6519463786725339, 72.34076406854485697, -93.55046425245691921 ) ) ;
#25187 = CARTESIAN_POINT ( 'NONE',  ( 24.96873044429758082, -1.250000000000021982, 0.000000000000000000 ) ) ;
#25188 = CARTESIAN_POINT ( 'NONE',  ( 110.0000000000000284, -22.00000000000000000, 0.000000000000000000 ) ) ;
#25189 = CARTESIAN_POINT ( 'NONE',  ( -58.76099769480629220, 16.75353773354893150, 44.34096742449668938 ) ) ;
#25190 = ADVANCED_FACE ( 'NONE', ( #4352 ), #60157, .T. ) ;
#25191 = FACE_OUTER_BOUND ( 'NONE', #48784, .T. ) ;
#25192 = CIRCLE ( 'NONE', #34181, 8.000000000000000000 ) ;
#25193 = CARTESIAN_POINT ( 'NONE',  ( 33.03621582719333816, 7.666716336587122704, 60.28506365736417649 ) ) ;
#25194 = CARTESIAN_POINT ( 'NONE',  ( 46.09004436292335782, 9.373833359422084399, 87.69295583249557069 ) ) ;
#25195 = ORIENTED_EDGE ( 'NONE', *, *, #46964, .F. ) ;
#25196 = CARTESIAN_POINT ( 'NONE',  ( -4.504169684898453596, 6.697401007565306763, -36.18904655353872357 ) ) ;
#25197 = CARTESIAN_POINT ( 'NONE',  ( 186.2651679807462131, 84.00458780104315792, 58.20990309437074472 ) ) ;
#25198 = CARTESIAN_POINT ( 'NONE',  ( -124.1033713525885673, 45.32626312604503482, 18.56215417726921757 ) ) ;
#25199 = DIRECTION ( 'NONE',  ( -0.000000000000000000, -0.000000000000000000, -1.000000000000000000 ) ) ;
#25200 = VECTOR ( 'NONE', #31324, 1000.000000000000000 ) ;
#25201 = CARTESIAN_POINT ( 'NONE',  ( 17.72992212664810552, 6.570588738776101501, 57.11079023146151457 ) ) ;
#25202 = CARTESIAN_POINT ( 'NONE',  ( 22.51798020284707036, 7.817376421459706570, -19.49430492783765700 ) ) ;
#25203 = CARTESIAN_POINT ( 'NONE',  ( 201.9777685760379882, 102.6876480786893069, 56.55075970390274875 ) ) ;
#25204 = AXIS2_PLACEMENT_3D ( 'NONE', #60496, #21464, #64732 ) ;
#25205 = AXIS2_PLACEMENT_3D ( 'NONE', #34821, #52026, #41127 ) ;
#25206 = ADVANCED_FACE ( 'NONE', ( #8938 ), #25471, .F. ) ;
#25207 = ORIENTED_EDGE ( 'NONE', *, *, #69377, .F. ) ;
#25208 = CARTESIAN_POINT ( 'NONE',  ( 50.57199999999998852, 0.000000000000000000, 0.000000000000000000 ) ) ;
#25209 = APPLICATION_PROTOCOL_DEFINITION ( 'draft international standard', 'automotive_design', 1998, #48895 ) ;
#25210 = CARTESIAN_POINT ( 'NONE',  ( 132.9557829392754513, 42.05591979570419170, -50.98300341427673743 ) ) ;
#25211 = CARTESIAN_POINT ( 'NONE',  ( -126.8005235842505840, 47.09307471149450208, -34.95511893173629403 ) ) ;
#25212 = CARTESIAN_POINT ( 'NONE',  ( -105.4642082819536313, 35.56541171990214423, -35.70785606305261695 ) ) ;
#25213 = FACE_OUTER_BOUND ( 'NONE', #43198, .T. ) ;
#25214 = VERTEX_POINT ( 'NONE', #46207 ) ;
#25215 = ORIENTED_EDGE ( 'NONE', *, *, #59128, .T. ) ;
#25216 = CARTESIAN_POINT ( 'NONE',  ( -149.5074843970971017, 64.17983161892347255, -7.968279941028269420 ) ) ;
#25217 = DIRECTION ( 'NONE',  ( -1.000000000000000000, 0.000000000000000000, 0.000000000000000000 ) ) ;
#25218 = ORIENTED_EDGE ( 'NONE', *, *, #50991, .T. ) ;
#25219 = CARTESIAN_POINT ( 'NONE',  ( 164.5010389544228246, 64.64604269109669588, 87.96214707110127051 ) ) ;
#25220 = ORIENTED_EDGE ( 'NONE', *, *, #22390, .F. ) ;
#25221 = CARTESIAN_POINT ( 'NONE',  ( 126.3554864210862121, 38.22801630372152459, -70.13989239923940033 ) ) ;
#25222 = CARTESIAN_POINT ( 'NONE',  ( 133.3996297101684547, 41.14871796345732946, 44.51034083899536142 ) ) ;
#25223 = CARTESIAN_POINT ( 'NONE',  ( -149.5074843970971017, 65.50121172469319220, 45.72082123989907387 ) ) ;
#25224 = DIRECTION ( 'NONE',  ( -0.000000000000000000, -0.000000000000000000, -1.000000000000000000 ) ) ;
#25225 = DIRECTION ( 'NONE',  ( -0.000000000000000000, -0.000000000000000000, -1.000000000000000000 ) ) ;
#25227 = VERTEX_POINT ( 'NONE', #46908 ) ;
#25226 = DIRECTION ( 'NONE',  ( 0.2225209339563042066, 0.9749279121818259508, 0.000000000000000000 ) ) ;
#25228 = CARTESIAN_POINT ( 'NONE',  ( -36.11269837220809364, -15.55634918610397754, 85.00100000000000477 ) ) ;
#25229 = ORIENTED_EDGE ( 'NONE', *, *, #5071, .F. ) ;
#25230 = ORIENTED_EDGE ( 'NONE', *, *, #3399, .T. ) ;
#25231 = CARTESIAN_POINT ( 'NONE',  ( -166.7136514167008841, 81.71618216218794828, 7.570113361991930745 ) ) ;
#25232 = AXIS2_PLACEMENT_3D ( 'NONE', #51953, #25586, #47024 ) ;
#25233 = CARTESIAN_POINT ( 'NONE',  ( 204.6977192012829789, -170.0000000000000000, -70.67048162308527992 ) ) ;
#25235 = ORIENTED_EDGE ( 'NONE', *, *, #68387, .F. ) ;
#25234 = CARTESIAN_POINT ( 'NONE',  ( -132.0738857626834033, 51.93126104279147626, 60.70775882567303228 ) ) ;
#25236 = CARTESIAN_POINT ( 'NONE',  ( -102.9275459269102129, 34.24179444430608044, 84.23033673724052051 ) ) ;
#25237 = CARTESIAN_POINT ( 'NONE',  ( 41.66904755831212981, 15.55634918610394379, 85.00100000000000477 ) ) ;
#25238 = VECTOR ( 'NONE', #8325, 1000.000000000000000 ) ;
#25239 = VERTEX_POINT ( 'NONE', #67688 ) ;
#25240 = EDGE_CURVE ( 'NONE', #12998, #50390, #5127, .T. ) ;
#25241 = DIRECTION ( 'NONE',  ( -0.000000000000000000, 1.000000000000000000, -0.000000000000000000 ) ) ;
#25242 = VECTOR ( 'NONE', #26591, 1000.000000000000114 ) ;
#25243 = CARTESIAN_POINT ( 'NONE',  ( -131.6253556217205016, 51.61436399519948282, -74.12161565071266978 ) ) ;
#25244 = CARTESIAN_POINT ( 'NONE',  ( 117.7417271423229863, 33.63613196344607559, 37.64637180083228429 ) ) ;
#25245 = VECTOR ( 'NONE', #30754, 1000.000000000000000 ) ;
#25246 = DIRECTION ( 'NONE',  ( 4.314083075427411048E-32, 1.000000000000000000, 6.123233995736763571E-17 ) ) ;
#25247 = CARTESIAN_POINT ( 'NONE',  ( 70.46579300139241298, 15.56614468937218732, -69.06676961812144100 ) ) ;
#25248 = ORIENTED_EDGE ( 'NONE', *, *, #13459, .F. ) ;
#25249 = ORIENTED_EDGE ( 'NONE', *, *, #46747, .T. ) ;
#25250 = DIRECTION ( 'NONE',  ( 0.000000000000000000, 0.000000000000000000, -1.000000000000000000 ) ) ;
#25251 = DIRECTION ( 'NONE',  ( -0.6234898018587431423, 0.7818314824680220321, 0.000000000000000000 ) ) ;
#25252 = DIRECTION ( 'NONE',  ( 0.000000000000000000, 0.000000000000000000, 1.000000000000000000 ) ) ;
#25253 = DIRECTION ( 'NONE',  ( -1.000000000000000000, -1.110223024625155594E-14, 1.110223024625155594E-14 ) ) ;
#25254 = CARTESIAN_POINT ( 'NONE',  ( -49.97682018836099616, 14.41498301761731327, -90.86710540830219429 ) ) ;
#25255 = CYLINDRICAL_SURFACE ( 'NONE', #16880, 25.00000000000296296 ) ;
#25256 = CARTESIAN_POINT ( 'NONE',  ( 69.49112875363883290, 15.30845942322121722, -47.01275429639923686 ) ) ;
#25257 = EDGE_CURVE ( 'NONE', #29332, #27359, #3651, .T. ) ;
#25258 = CYLINDRICAL_SURFACE ( 'NONE', #59802, 65.00000000000000000 ) ;
#25259 = CARTESIAN_POINT ( 'NONE',  ( 210.9506883977751954, 115.3310071214937125, 59.40277579576930833 ) ) ;
#25260 = EDGE_LOOP ( 'NONE', ( #66624, #46215, #27917, #36035 ) ) ;
#25261 = LINE ( 'NONE', #67147, #37722 ) ;
#25262 = ADVANCED_FACE ( 'NONE', ( #90 ), #5380, .F. ) ;
#25263 = ORIENTED_EDGE ( 'NONE', *, *, #11979, .F. ) ;
#25264 = CARTESIAN_POINT ( 'NONE',  ( -200.0000000000000000, 2.449293598294706434E-14, -10.00000000000000000 ) ) ;
#25265 = DIRECTION ( 'NONE',  ( -0.000000000000000000, 1.000000000000000000, -0.000000000000000000 ) ) ;
#25266 = VERTEX_POINT ( 'NONE', #48955 ) ;
#25267 = CARTESIAN_POINT ( 'NONE',  ( -84.48447130825533691, 24.62360807013167729, -91.56658158870699538 ) ) ;
#25268 = CARTESIAN_POINT ( 'NONE',  ( -190.4966031023458868, 108.8421921967458559, -64.77830472940530626 ) ) ;
#25269 = CARTESIAN_POINT ( 'NONE',  ( 262.2516123306975260, 190.0000000000000000, -91.28179539054376335 ) ) ;
#25270 = LINE ( 'NONE', #30198, #23738 ) ;
#25271 = CARTESIAN_POINT ( 'NONE',  ( 38.42020198992003799, 8.283430712587433575, 3.117809402762283355 ) ) ;
#25272 = LINE ( 'NONE', #68185, #5273 ) ;
#25273 = EDGE_CURVE ( 'NONE', #66442, #66077, #65802, .T. ) ;
#25274 = CARTESIAN_POINT ( 'NONE',  ( -78.66644367742111399, 23.39876645725286863, 72.26275173013684139 ) ) ;
#25275 = ORIENTED_EDGE ( 'NONE', *, *, #55841, .T. ) ;
#25276 = CARTESIAN_POINT ( 'NONE',  ( -120.8704515857978521, 44.46077770807175256, -90.51607353834583591 ) ) ;
#25277 = VERTEX_POINT ( 'NONE', #26835 ) ;
#25278 = DIRECTION ( 'NONE',  ( 0.000000000000000000, -0.000000000000000000, 1.000000000000000000 ) ) ;
#25279 = CARTESIAN_POINT ( 'NONE',  ( 8.337549025192448227, 7.382630697225775585, -70.85121512598109916 ) ) ;
#25280 = CARTESIAN_POINT ( 'NONE',  ( -23.99924996210629047, 8.487987924059027023, 11.85155207052061321 ) ) ;
#25281 = CARTESIAN_POINT ( 'NONE',  ( -2.700000000000004619, 0.000000000000000000, -25.00000000000000711 ) ) ;
#25282 = CARTESIAN_POINT ( 'NONE',  ( -14.19447842053094533, 7.389800932646228837, -65.79454045135867091 ) ) ;
#25283 = CARTESIAN_POINT ( 'NONE',  ( -99.97541017369788108, 31.62502926470686049, -8.517426260003034599 ) ) ;
#25284 = CARTESIAN_POINT ( 'NONE',  ( 152.8672128926848188, 55.41186463791520822, -49.55020588636439527 ) ) ;
#25285 = VECTOR ( 'NONE', #30430, 1000.000000000000000 ) ;
#25286 = B_SPLINE_CURVE_WITH_KNOTS ( 'NONE', 3,
 ( #1992, #61062, #6558, #23448, #28002, #49446, #45228, #44886, #23782, #39611, #12889, #45575, #29067, #50512, #24133, #66706, #66367, #1279, #18158, #44170, #67057, #29401, #22736, #34351, #12187, #55791, #2332, #7616, #18502, #13235, #39956, #33651, #61412, #34696, #50163, #65657, #66020, #56131 ),
 .UNSPECIFIED., .F., .F.,
 ( 4, 2, 2, 2, 2, 2, 2, 2, 2, 2, 2, 2, 2, 2, 2, 2, 2, 2, 4 ),
 ( 0.000000000000000000, 0.001559859933532175419, 0.003119719867064350838, 0.004679579800596527124, 0.006239439734128701676, 0.007799299667660877095, 0.008579229634426983886, 0.009359159601193090677, 0.01091901953472530599, 0.01169894950149142840, 0.01247887946825755080, 0.01403873940178979561, 0.01559859933532203868, 0.01715845926885430431, 0.01871831920238656646, 0.02027817913591883209, 0.02183803906945109771, 0.02339789900298335987, 0.02495775893651562202 ),
 .UNSPECIFIED. ) ;
#25287 = EDGE_CURVE ( 'NONE', #46531, #42019, #21216, .T. ) ;
#25288 = ORIENTED_EDGE ( 'NONE', *, *, #67750, .F. ) ;
#25289 = CARTESIAN_POINT ( 'NONE',  ( 620.5071894358228519, 928.5915846175156503, 739.5068267248771008 ) ) ;
#25290 = CARTESIAN_POINT ( 'NONE',  ( -155.2836587093738956, 70.59655508952970138, 60.27484905456947928 ) ) ;
#25292 = EDGE_CURVE ( 'NONE', #62027, #15785, #59515, .T. ) ;
#25291 = CARTESIAN_POINT ( 'NONE',  ( 173.6024011093110175, 72.73634049052007811, -17.48363501179885660 ) ) ;
#25293 = EDGE_CURVE ( 'NONE', #5765, #62805, #64462, .T. ) ;
#25294 = CARTESIAN_POINT ( 'NONE',  ( -118.5043919384112030, 41.81711884544881030, 39.43039629447052619 ) ) ;
#25295 = DIRECTION ( 'NONE',  ( 9.115745035929406798E-64, -3.469446951953612956E-17, 1.000000000000000000 ) ) ;
#25296 = ORIENTED_EDGE ( 'NONE', *, *, #29875, .F. ) ;
#25298 = CARTESIAN_POINT ( 'NONE',  ( -180.6209674222603212, 97.47999311542517376, -69.22316660788568754 ) ) ;
#25297 = VECTOR ( 'NONE', #36315, 1000.000000000000000 ) ;
#25299 = CIRCLE ( 'NONE', #64583, 25.12245591505646303 ) ;
#25300 = CARTESIAN_POINT ( 'NONE',  ( 86.62931800182293784, 19.42108912189596381, 56.55663816294300261 ) ) ;
#25301 = CARTESIAN_POINT ( 'NONE',  ( 116.0773578185793298, 31.67580513411751042, 32.37210107868605036 ) ) ;
#25302 = VECTOR ( 'NONE', #13545, 1000.000000000000000 ) ;
#25303 = CARTESIAN_POINT ( 'NONE',  ( 188.9999999999999432, -2.000000000000001776, 72.99999999999998579 ) ) ;
#25304 = CONICAL_SURFACE ( 'NONE', #34338, 65.00000000000000000, 0.7853981633974497223 ) ;
#25305 = CARTESIAN_POINT ( 'NONE',  ( -173.1211646369891071, 87.12891641440859303, -34.71195716474998960 ) ) ;
#25306 = ORIENTED_EDGE ( 'NONE', *, *, #51572, .T. ) ;
#25307 = CARTESIAN_POINT ( 'NONE',  ( 197.6316695787930939, 97.13022718399024313, 39.23981542666417255 ) ) ;
#25308 = CARTESIAN_POINT ( 'NONE',  ( 117.6865880453676283, 32.48051379280607875, -71.32223984317171528 ) ) ;
#25309 = DIRECTION ( 'NONE',  ( 0.3090169943749447312, 0.9510565162951545304, 0.000000000000000000 ) ) ;
#25310 = CARTESIAN_POINT ( 'NONE',  ( 139.7883986595927581, 46.32091287009613723, 5.569321396343120512 ) ) ;
#25311 = LINE ( 'NONE', #40090, #13940 ) ;
#25312 = ORIENTED_EDGE ( 'NONE', *, *, #16244, .T. ) ;
#25313 = AXIS2_PLACEMENT_3D ( 'NONE', #51311, #24582, #65752 ) ;
#25314 = CARTESIAN_POINT ( 'NONE',  ( 180.6713229637342408, 79.61878926895393249, 56.15314469597510794 ) ) ;
#25315 = ORIENTED_EDGE ( 'NONE', *, *, #33239, .F. ) ;
#25316 = CARTESIAN_POINT ( 'NONE',  ( 67.93317348534928612, 14.90531593353391848, 69.84145773790685041 ) ) ;
#25317 = CARTESIAN_POINT ( 'NONE',  ( -24.39249304643438521, 60.24953346690454481, 133.5802547743875550 ) ) ;
#25319 = ORIENTED_EDGE ( 'NONE', *, *, #35331, .T. ) ;
#25318 = FACE_OUTER_BOUND ( 'NONE', #5684, .T. ) ;
#25320 = CARTESIAN_POINT ( 'NONE',  ( -175.9852529046322616, 90.37283472601130541, 45.26617804551248270 ) ) ;
#25321 = CARTESIAN_POINT ( 'NONE',  ( 0.000000000000000000, 0.000000000000000000, 0.000000000000000000 ) ) ;
#25322 = DIRECTION ( 'NONE',  ( 0.1342332658176522420, 0.9909497617679351444, 0.000000000000000000 ) ) ;
#25323 = EDGE_LOOP ( 'NONE', ( #24171, #21768, #25033, #65250 ) ) ;
#25324 = ADVANCED_FACE ( 'NONE', ( #69397 ), #63786, .F. ) ;
#25325 = DIRECTION ( 'NONE',  ( 1.000000000000000000, 0.000000000000000000, -0.000000000000000000 ) ) ;
#25326 = CARTESIAN_POINT ( 'NONE',  ( 55.65927616287137170, 12.11203904137339471, 89.50322596452608082 ) ) ;
#25327 = EDGE_CURVE ( 'NONE', #4383, #48419, #5712, .T. ) ;
#25328 = CARTESIAN_POINT ( 'NONE',  ( 15.78827728214693416, 7.507518794609575608, 45.01470767270524931 ) ) ;
#25329 = VECTOR ( 'NONE', #39410, 1000.000000000000000 ) ;
#25330 = CARTESIAN_POINT ( 'NONE',  ( -74.81012118577218928, -5.477980300263996405, 43.58025477438756212 ) ) ;
#25331 = DIRECTION ( 'NONE',  ( -0.000000000000000000, -0.000000000000000000, -1.000000000000000000 ) ) ;
#25332 = CARTESIAN_POINT ( 'NONE',  ( 151.1873096904021168, 52.92629247302095763, 67.85776711895714186 ) ) ;
#25333 = DIRECTION ( 'NONE',  ( 0.000000000000000000, -1.000000000000000000, 0.000000000000000000 ) ) ;
#25334 = ORIENTED_EDGE ( 'NONE', *, *, #52548, .T. ) ;
#25335 = CARTESIAN_POINT ( 'NONE',  ( -95.88693721180807472, 30.76307528361165566, 68.79313100246496049 ) ) ;
#25336 = CARTESIAN_POINT ( 'NONE',  ( 15.55634918610411610, 51.66904755831205875, 2.000000000000001776 ) ) ;
#25337 = ORIENTED_EDGE ( 'NONE', *, *, #45618, .T. ) ;
#25338 = AXIS2_PLACEMENT_3D ( 'NONE', #1536, #44081, #33566 ) ;
#25339 = CARTESIAN_POINT ( 'NONE',  ( 157.2533363798599737, 58.75760182111577024, -24.27963370867399107 ) ) ;
#25340 = CARTESIAN_POINT ( 'NONE',  ( 207.2640160519426615, 111.6867652229576322, -24.03161405320629029 ) ) ;
#25341 = AXIS2_PLACEMENT_3D ( 'NONE', #23286, #44731, #17999 ) ;
#25342 = CARTESIAN_POINT ( 'NONE',  ( 109.3047140914111708, 29.55674059952506738, 44.56730977590374465 ) ) ;
#25343 = CARTESIAN_POINT ( 'NONE',  ( 46.66904755831207297, -15.55634918610412853, 0.000000000000000000 ) ) ;
#25344 = LINE ( 'NONE', #68251, #44913 ) ;
#25345 = CARTESIAN_POINT ( 'NONE',  ( 188.2962140587030149, 87.71627202537838741, 7.885122216152835151 ) ) ;
#25346 = EDGE_CURVE ( 'NONE', #58728, #2957, #58481, .T. ) ;
#25347 = CARTESIAN_POINT ( 'NONE',  ( 211.8476521439974078, 116.6941316755177525, -41.53835296956879830 ) ) ;
#25348 = AXIS2_PLACEMENT_3D ( 'NONE', #40012, #49860, #1689 ) ;
#25349 = CARTESIAN_POINT ( 'NONE',  ( 173.6710158776850506, 71.42507420636735560, 8.787227813904088691 ) ) ;
#25350 = EDGE_CURVE ( 'NONE', #42408, #13782, #21544, .T. ) ;
#25351 = ORIENTED_EDGE ( 'NONE', *, *, #449, .F. ) ;
#25353 = VECTOR ( 'NONE', #17614, 1000.000000000000227 ) ;
#25352 = CARTESIAN_POINT ( 'NONE',  ( 41.66904755831212981, 20.55634918610394379, 0.000000000000000000 ) ) ;
#25354 = ORIENTED_EDGE ( 'NONE', *, *, #25760, .F. ) ;
#25355 = CARTESIAN_POINT ( 'NONE',  ( -73.63128929564827274, 21.53548093502884697, 70.32671424837877794 ) ) ;
#25356 = EDGE_CURVE ( 'NONE', #8504, #66166, #69033, .T. ) ;
#25357 = PLANE ( 'NONE',  #12981 ) ;
#25358 = CARTESIAN_POINT ( 'NONE',  ( 26.11269837220806167, -6.375108774214766072E-14, 0.000000000000000000 ) ) ;
#25359 = DIRECTION ( 'NONE',  ( -1.000000000000000000, 0.000000000000000000, 0.000000000000000000 ) ) ;
#25360 = CARTESIAN_POINT ( 'NONE',  ( -14.46762367737944288, 7.414939723119872816, 87.80640566984232009 ) ) ;
#25361 = CARTESIAN_POINT ( 'NONE',  ( -108.5248383251030475, 37.21456094989611785, -19.83122018436582934 ) ) ;
#25362 = ORIENTED_EDGE ( 'NONE', *, *, #61391, .F. ) ;
#25363 = CARTESIAN_POINT ( 'NONE',  ( -73.63346300764936814, 20.46798018699517385, 59.19690935554574196 ) ) ;
#25364 = CARTESIAN_POINT ( 'NONE',  ( 198.7554884879576491, 98.53603447819021710, -92.93361033491551382 ) ) ;
#25365 = ORIENTED_EDGE ( 'NONE', *, *, #60091, .F. ) ;
#25366 = VERTEX_POINT ( 'NONE', #16955 ) ;
#25367 = CARTESIAN_POINT ( 'NONE',  ( -156.6819053601226130, 70.51177710383656461, 40.47953577721239071 ) ) ;
#25368 = CARTESIAN_POINT ( 'NONE',  ( -62.31345272479909880, 18.49415068377641447, 40.00000000000003553 ) ) ;
#25369 = CARTESIAN_POINT ( 'NONE',  ( 176.6258282025054598, 74.21441092921635629, -22.91608747162088733 ) ) ;
#25370 = CARTESIAN_POINT ( 'NONE',  ( -417.6627218934913230, 399.9999999999998295, 113.5502958579882602 ) ) ;
#25371 = LINE ( 'NONE', #13081, #10550 ) ;
#25372 = VERTEX_POINT ( 'NONE', #43343 ) ;
#25373 = EDGE_CURVE ( 'NONE', #52541, #65894, #57911, .T. ) ;
#25374 = EDGE_CURVE ( 'NONE', #61489, #8739, #53412, .T. ) ;
#25375 = EDGE_CURVE ( 'NONE', #6967, #62563, #11334, .T. ) ;
#25376 = CARTESIAN_POINT ( 'NONE',  ( 6.400000000000000355, 0.000000000000000000, 0.000000000000000000 ) ) ;
#25377 = VERTEX_POINT ( 'NONE', #6055 ) ;
#25378 = CARTESIAN_POINT ( 'NONE',  ( 212.1931396682533375, 117.2245435827729239, 10.17688792897256356 ) ) ;
#25379 = CARTESIAN_POINT ( 'NONE',  ( 13.83281508467570831, 7.452090093180183672, 71.61672662805924006 ) ) ;
#25380 = DIRECTION ( 'NONE',  ( 9.109522253334613014E-16, 1.000000000000000000, -3.889846672687432470E-31 ) ) ;
#25381 = FACE_BOUND ( 'NONE', #45624, .T. ) ;
#25382 = ADVANCED_FACE ( 'NONE', ( #22249 ), #65162, .F. ) ;
#25383 = PRODUCT ( 'Belt1-2', 'Belt1-2', '', ( #62124 ) ) ;
#25384 = AXIS2_PLACEMENT_3D ( 'NONE', #63645, #59634, #32918 ) ;
#25385 = ORIENTED_EDGE ( 'NONE', *, *, #66005, .F. ) ;
#25386 = ORIENTED_EDGE ( 'NONE', *, *, #1020, .F. ) ;
#25387 = CARTESIAN_POINT ( 'NONE',  ( 181.0840389613909736, -170.0000000000000000, -36.22505766587961062 ) ) ;
#25388 = CARTESIAN_POINT ( 'NONE',  ( -127.0966118282843809, 48.50115527717463948, 84.40066604616777113 ) ) ;
#25389 = CIRCLE ( 'NONE', #1834, 25.12245591505646303 ) ;
#25390 = CARTESIAN_POINT ( 'NONE',  ( -166.5686015187718567, 80.11916873959170005, -11.70817783129956879 ) ) ;
#25391 = CARTESIAN_POINT ( 'NONE',  ( -176.3856149167965555, 92.38076834121982017, 18.24363522339888988 ) ) ;
#25392 = CARTESIAN_POINT ( 'NONE',  ( 22.93685557200797831, 6.834779360682496474, 93.49618427415832400 ) ) ;
#25393 = DIRECTION ( 'NONE',  ( 0.000000000000000000, 0.000000000000000000, 1.000000000000000000 ) ) ;
#25394 = AXIS2_PLACEMENT_3D ( 'NONE', #26904, #42732, #21283 ) ;
#25395 = ORIENTED_EDGE ( 'NONE', *, *, #24622, .T. ) ;
#25396 = DIRECTION ( 'NONE',  ( 0.000000000000000000, 0.000000000000000000, -1.000000000000000000 ) ) ;
#25397 = AXIS2_PLACEMENT_3D ( 'NONE', #59467, #11278, #33100 ) ;
#25398 = CARTESIAN_POINT ( 'NONE',  ( -97.47339919287391297, 30.40512551257289076, 70.64169830722899235 ) ) ;
#25399 = ORIENTED_EDGE ( 'NONE', *, *, #67294, .F. ) ;
#25400 = CARTESIAN_POINT ( 'NONE',  ( -80.54757501605357106, 23.04700348514570152, 18.33782076323183219 ) ) ;
#25401 = VERTEX_POINT ( 'NONE', #20864 ) ;
#25402 = VECTOR ( 'NONE', #7157, 1000.000000000000000 ) ;
#25403 = CARTESIAN_POINT ( 'NONE',  ( -56.02289203441038978, 15.98631679403371741, -8.418896321847350706 ) ) ;
#25404 = ORIENTED_EDGE ( 'NONE', *, *, #30518, .T. ) ;
#25405 = ORIENTED_EDGE ( 'NONE', *, *, #53348, .F. ) ;
#25406 = CARTESIAN_POINT ( 'NONE',  ( 8.336031647119272137, 6.376437040857336314, -42.04032280401278854 ) ) ;
#25407 = CARTESIAN_POINT ( 'NONE',  ( -109.2504972001306101, 37.61384092494594000, -93.42565027757478902 ) ) ;
#25408 = CARTESIAN_POINT ( 'NONE',  ( 130.3019683985926349, 39.31883119822049366, 57.23370010971977706 ) ) ;
#25409 = VERTEX_POINT ( 'NONE', #42323 ) ;
#25410 = CARTESIAN_POINT ( 'NONE',  ( -37.53974046071399329, 10.67241809297004806, 86.99493448681049301 ) ) ;
#25411 = ADVANCED_FACE ( 'NONE', ( #15594 ), #10642, .F. ) ;
#25412 = CARTESIAN_POINT ( 'NONE',  ( 174.6307688320643479, 73.70327352126999187, -74.40040851124921062 ) ) ;
#25413 = CARTESIAN_POINT ( 'NONE',  ( -125.8938041572051389, 46.49392987655492249, 30.61994787315706290 ) ) ;
#25414 = CARTESIAN_POINT ( 'NONE',  ( 110.2429982417149432, 28.88204397445229077, -35.92243756565368784 ) ) ;
#25415 = CARTESIAN_POINT ( 'NONE',  ( 81.05403189674298403, 18.64820877954959499, -48.36183566878465712 ) ) ;
#25416 = CARTESIAN_POINT ( 'NONE',  ( 311.8713128290285113, 188.0000000000000000, -151.4173447659616443 ) ) ;
#25417 = ORIENTED_EDGE ( 'NONE', *, *, #37702, .F. ) ;
#25418 = CARTESIAN_POINT ( 'NONE',  ( 35.43132475791147584, -14.63273365840185924, 13.32819397642333037 ) ) ;
#25419 = CARTESIAN_POINT ( 'NONE',  ( -78.66644367742111399, 23.39876645725286153, -61.96000122218157458 ) ) ;
#25420 = CARTESIAN_POINT ( 'NONE',  ( 178.1888264190355073, 77.13727704498029425, 16.89608322330665047 ) ) ;
#25421 = CARTESIAN_POINT ( 'NONE',  ( 447.3372781065086201, 0.000000000000000000, -116.4497041420118393 ) ) ;
#25422 = DIRECTION ( 'NONE',  ( 0.000000000000000000, -0.000000000000000000, -1.000000000000000000 ) ) ;
#25423 = CARTESIAN_POINT ( 'NONE',  ( 126.4324872316703363, 37.11876756822024959, 11.26176343780550404 ) ) ;
#25424 = CARTESIAN_POINT ( 'NONE',  ( 32.35876450276292360, 7.597628455623533839, -94.19814380599602543 ) ) ;
#25425 = EDGE_CURVE ( 'NONE', #21633, #39050, #47926, .T. ) ;
#25426 = DIRECTION ( 'NONE',  ( -1.000000000000000000, 0.000000000000000000, 0.000000000000000000 ) ) ;
#25427 = DIRECTION ( 'NONE',  ( -0.000000000000000000, 1.000000000000000000, -0.000000000000000000 ) ) ;
#25428 = FACE_OUTER_BOUND ( 'NONE', #28709, .T. ) ;
#25429 = CARTESIAN_POINT ( 'NONE',  ( 63.72039997003725631, -12.83396383267754537, 170.0000000000000000 ) ) ;
#25430 = VERTEX_POINT ( 'NONE', #54943 ) ;
#25431 = VECTOR ( 'NONE', #51457, 1000.000000000000000 ) ;
#25432 = CONTEXT_DEPENDENT_SHAPE_REPRESENTATION ( #35486, #44541 ) ;
#25433 = CARTESIAN_POINT ( 'NONE',  ( -62.48837791900216132, 17.85349220731796649, 92.54043131072742767 ) ) ;
#25434 = VERTEX_POINT ( 'NONE', #49658 ) ;
#25435 = EDGE_CURVE ( 'NONE', #6675, #35022, #18019, .T. ) ;
#25436 = CARTESIAN_POINT ( 'NONE',  ( 199.7255144154428308, 99.76581417577200739, -22.61533049155591613 ) ) ;
#25437 = ORIENTED_EDGE ( 'NONE', *, *, #52443, .T. ) ;
#25438 = ADVANCED_FACE ( 'NONE', ( #2535 ), #44034, .F. ) ;
#25439 = DIRECTION ( 'NONE',  ( 0.000000000000000000, 0.000000000000000000, -1.000000000000000000 ) ) ;
#25440 = VECTOR ( 'NONE', #44732, 1000.000000000000000 ) ;
#25441 = CARTESIAN_POINT ( 'NONE',  ( 8.000000000000007105, 249.8719672152120381, -95.00000000000133582 ) ) ;
#25442 = CARTESIAN_POINT ( 'NONE',  ( 45.82394788922869822, -46.11928342727429708, 170.0000000000000000 ) ) ;
#25443 = DIRECTION ( 'NONE',  ( -0.000000000000000000, 1.000000000000000000, -0.000000000000000000 ) ) ;
#25444 = CARTESIAN_POINT ( 'NONE',  ( 36.31593203568479566, 8.028139509847015631, -49.95989190410476510 ) ) ;
#25445 = CARTESIAN_POINT ( 'NONE',  ( 2.337278106504167230, 395.0000000000000000, -341.4497041420117966 ) ) ;
#25446 = CARTESIAN_POINT ( 'NONE',  ( 8.767814708128309320, 7.383611927972544287, -45.66910925475413308 ) ) ;
#25448 = DIRECTION ( 'NONE',  ( 0.000000000000000000, 0.000000000000000000, 1.000000000000000000 ) ) ;
#25447 = PRODUCT_DEFINITION_FORMATION_WITH_SPECIFIED_SOURCE ( 'ANY', '', #65900, .NOT_KNOWN. ) ;
#25449 = CARTESIAN_POINT ( 'NONE',  ( 132.7179291807800894, 40.74118679001688292, -50.93987571790520974 ) ) ;
#25450 = ORIENTED_EDGE ( 'NONE', *, *, #49938, .F. ) ;
#25451 = ORIENTED_EDGE ( 'NONE', *, *, #40407, .F. ) ;
#25452 = CARTESIAN_POINT ( 'NONE',  ( 173.6387410343579347, 72.77029877349359310, 91.48744382001903830 ) ) ;
#25453 = VECTOR ( 'NONE', #44543, 1000.000000000000000 ) ;
#25454 = CARTESIAN_POINT ( 'NONE',  ( -78.66644367742109978, 22.32174330031321574, 72.26275173013684139 ) ) ;
#25455 = CARTESIAN_POINT ( 'NONE',  ( -24.70911172866234651, 8.583078995053019966, -73.00837023266150538 ) ) ;
#25456 = UNCERTAINTY_MEASURE_WITH_UNIT (LENGTH_MEASURE( 1.000000000000000082E-05 ), #48934, 'distance_accuracy_value', 'NONE');
#25457 = CARTESIAN_POINT ( 'NONE',  ( 9.288975942802416341, 6.379608420846962780, 14.42107178552651270 ) ) ;
#25458 = CARTESIAN_POINT ( 'NONE',  ( 44.34362023773822159, 10.12115849931653599, -75.62784561966921615 ) ) ;
#25459 = CYLINDRICAL_SURFACE ( 'NONE', #23371, 7.500000000000013323 ) ;
#25460 = CARTESIAN_POINT ( 'NONE',  ( 178.1903523079567435, 75.72906488635190669, -77.50250463138750945 ) ) ;
#25461 =( LENGTH_UNIT ( ) NAMED_UNIT ( * ) SI_UNIT ( .MILLI., .METRE. ) );
#25462 = DIRECTION ( 'NONE',  ( 0.000000000000000000, 0.000000000000000000, -1.000000000000000000 ) ) ;
#25463 = CARTESIAN_POINT ( 'NONE',  ( 86.62931800182293784, 19.42108912189600645, -8.977013608448025650 ) ) ;
#25464 = DIRECTION ( 'NONE',  ( -0.8118923937861950435, -0.5838071093367415143, 0.000000000000000000 ) ) ;
#25465 = DIRECTION ( 'NONE',  ( 0.000000000000000000, 0.000000000000000000, 1.000000000000000000 ) ) ;
#25466 = ADVANCED_FACE ( 'NONE', ( #33516 ), #23307, .F. ) ;
#25467 = DIRECTION ( 'NONE',  ( 0.000000000000000000, 0.000000000000000000, 1.000000000000000000 ) ) ;
#25468 = VERTEX_POINT ( 'NONE', #44393 ) ;
#25469 = CARTESIAN_POINT ( 'NONE',  ( 51.85299110299440173, 39.21848821248450179, 170.0000000000000000 ) ) ;
#25470 = LINE ( 'NONE', #46907, #22869 ) ;
#25471 = CYLINDRICAL_SURFACE ( 'NONE', #19750, 7.500000000000013323 ) ;
#25472 = CARTESIAN_POINT ( 'NONE',  ( -417.6627218934917778, 400.0000000000064801, -111.4497041420121661 ) ) ;
#25473 = FACE_BOUND ( 'NONE', #27153, .T. ) ;
#25474 = CARTESIAN_POINT ( 'NONE',  ( -15.55634918610400597, 20.55634918610405748, 0.000000000000000000 ) ) ;
#25475 = VERTEX_POINT ( 'NONE', #34898 ) ;
#25476 = CARTESIAN_POINT ( 'NONE',  ( -189.6704649493768216, 107.6868404312579486, -93.25980815284229664 ) ) ;
#25477 = CARTESIAN_POINT ( 'NONE',  ( -58.76005811686688673, 15.70653557534867595, 71.19953605005537156 ) ) ;
#25478 = VERTEX_POINT ( 'NONE', #39469 ) ;
#25479 = VECTOR ( 'NONE', #14348, 1000.000000000000000 ) ;
#25480 = ORIENTED_EDGE ( 'NONE', *, *, #1028, .T. ) ;
#25481 = CARTESIAN_POINT ( 'NONE',  ( 180.2572128312848179, 77.77323980479702925, -51.19118848864500393 ) ) ;
#25482 = CARTESIAN_POINT ( 'NONE',  ( -179.2177980985565000, 94.18084789436636584, -73.43254121296298820 ) ) ;
#25483 = DIRECTION ( 'NONE',  ( 0.000000000000000000, 0.000000000000000000, 1.000000000000000000 ) ) ;
#25484 = EDGE_LOOP ( 'NONE', ( #39915, #52107, #61469, #50 ) ) ;
#25485 = VECTOR ( 'NONE', #35910, 1000.000000000000000 ) ;
#25486 = CYLINDRICAL_SURFACE ( 'NONE', #27770, 7.500000000000013323 ) ;
#25487 = CARTESIAN_POINT ( 'NONE',  ( 23.17627457812085723, 71.32923872213659422, 0.000000000000000000 ) ) ;
#25488 = CARTESIAN_POINT ( 'NONE',  ( 55.76255201544533691, 12.13275766515752707, -45.19241930457960166 ) ) ;
#25489 = CARTESIAN_POINT ( 'NONE',  ( -82.93126516400698733, 25.07709093823494229, 31.74405965836805876 ) ) ;
#25490 = AXIS2_PLACEMENT_3D ( 'NONE', #62551, #46704, #67830 ) ;
#25491 = CARTESIAN_POINT ( 'NONE',  ( -26.50207385662994852, 9.849226639603649858, -21.64023079453380305 ) ) ;
#25492 = PRODUCT_RELATED_PRODUCT_CATEGORY ( 'part', '', ( #45703 ) ) ;
#25493 = CARTESIAN_POINT ( 'NONE',  ( 94.11746922806584337, 22.11341285603782580, 37.70410127150352508 ) ) ;
#25494 = DIRECTION ( 'NONE',  ( 0.000000000000000000, 0.000000000000000000, -1.000000000000000000 ) ) ;
#25495 = ADVANCED_FACE ( 'NONE', ( #7479 ), #66919, .F. ) ;
#25496 = VERTEX_POINT ( 'NONE', #65880 ) ;
#25497 = AXIS2_PLACEMENT_3D ( 'NONE', #12987, #22832, #33037 ) ;
#25498 = EDGE_CURVE ( 'NONE', #20522, #52890, #61274, .T. ) ;
#25499 = CARTESIAN_POINT ( 'NONE',  ( 9.288975942802411012, 6.379608420846962780, 68.11017296645387376 ) ) ;
#25500 = CARTESIAN_POINT ( 'NONE',  ( -26.88234027341226451, 9.904106450608205492, 31.73948476484182635 ) ) ;
#25501 = DIRECTION ( 'NONE',  ( 0.5773502691896258421, -0.5773502691896258421, 0.5773502691896258421 ) ) ;
#25502 = CARTESIAN_POINT ( 'NONE',  ( -71.23338454616570914, 20.69243496265646698, 90.55446336941628260 ) ) ;
#25504 = ORIENTED_EDGE ( 'NONE', *, *, #61774, .F. ) ;
#25503 = DIRECTION ( 'NONE',  ( 0.000000000000000000, 0.000000000000000000, 1.000000000000000000 ) ) ;
#25505 = DIRECTION ( 'NONE',  ( 0.5407162030609374836, -0.6444004775717707689, -0.5407162030609372616 ) ) ;
#25506 = VERTEX_POINT ( 'NONE', #50715 ) ;
#25507 = EDGE_LOOP ( 'NONE', ( #64848, #58184 ) ) ;
#25508 = CARTESIAN_POINT ( 'NONE',  ( 117.6853163455685234, 33.60747889659832310, -69.20596546345770150 ) ) ;
#25509 = DIRECTION ( 'NONE',  ( -0.000000000000000000, 0.000000000000000000, -1.000000000000000000 ) ) ;
#25510 = FACE_BOUND ( 'NONE', #4101, .T. ) ;
#25511 = CARTESIAN_POINT ( 'NONE',  ( 0.000000000000000000, 0.000000000000000000, 170.0000000000000000 ) ) ;
#25512 = PLANE ( 'NONE',  #26435 ) ;
#25513 = CARTESIAN_POINT ( 'NONE',  ( -83.13046924527390047, 25.15778674529014936, -21.80259833107481526 ) ) ;
#25514 = CARTESIAN_POINT ( 'NONE',  ( 0.000000000000000000, 0.000000000000000000, -9.474599999999998801 ) ) ;
#25515 = LINE ( 'NONE', #35020, #46374 ) ;
#25516 = ORIENTED_EDGE ( 'NONE', *, *, #901, .F. ) ;
#25517 = ADVANCED_FACE ( 'NONE', ( #55292 ), #55642, .T. ) ;
#25518 = ORIENTED_EDGE ( 'NONE', *, *, #48997, .F. ) ;
#25519 = EDGE_CURVE ( 'NONE', #18819, #51047, #28028, .T. ) ;
#25520 = CARTESIAN_POINT ( 'NONE',  ( -102.2801239173131052, 33.91021738430207222, 18.67452391595144334 ) ) ;
#25521 = CARTESIAN_POINT ( 'NONE',  ( -78.66644367742109978, 23.39876645725290061, -35.11545063171788428 ) ) ;
#25522 = CARTESIAN_POINT ( 'NONE',  ( 103.4225970396116452, 25.85249226022213520, 87.66116462355037697 ) ) ;
#25523 = DIRECTION ( 'NONE',  ( 0.000000000000000000, 0.000000000000000000, -1.000000000000000000 ) ) ;
#25524 = DIRECTION ( 'NONE',  ( -1.020422603260505347E-14, 1.000000000000000000, 5.551115123125782702E-17 ) ) ;
#25525 = CARTESIAN_POINT ( 'NONE',  ( -190.6985136298601731, 109.1272424661242582, -95.00000000000133582 ) ) ;
#25526 = CARTESIAN_POINT ( 'NONE',  ( 6.123233995736766282E-16, 50.00000000000000000, 5.000000000000000000 ) ) ;
#25527 = ORIENTED_EDGE ( 'NONE', *, *, #69155, .T. ) ;
#25528 = PRODUCT_DEFINITION_SHAPE ( 'NONE', 'NONE',  #69625 ) ;
#25529 = ORIENTED_EDGE ( 'NONE', *, *, #8181, .F. ) ;
#25530 = ORIENTED_EDGE ( 'NONE', *, *, #31760, .T. ) ;
#25531 = VECTOR ( 'NONE', #68513, 1000.000000000000000 ) ;
#25532 = CARTESIAN_POINT ( 'NONE',  ( -150.3831389294225005, 66.25266777263972529, -22.92020021732201229 ) ) ;
#25533 = DIRECTION ( 'NONE',  ( 1.000000000000000000, 0.000000000000000000, 0.000000000000000000 ) ) ;
#25534 = DIRECTION ( 'NONE',  ( -0.000000000000000000, 1.000000000000000000, -0.000000000000000000 ) ) ;
#25535 = AXIS2_PLACEMENT_3D ( 'NONE', #56860, #18876, #18529 ) ;
#25536 = DIRECTION ( 'NONE',  ( -1.000000000000000000, 0.000000000000000000, 0.000000000000000000 ) ) ;
#25537 = CARTESIAN_POINT ( 'NONE',  ( -156.0300823189601829, 69.91528270335481920, -19.20893955606299386 ) ) ;
#25538 = VECTOR ( 'NONE', #18984, 1000.000000000000000 ) ;
#25539 = CARTESIAN_POINT ( 'NONE',  ( 32.56927464314651388, 7.618924692399912324, 61.15594928078879633 ) ) ;
#25540 = CARTESIAN_POINT ( 'NONE',  ( 15.78827728214693416, 6.500811158483284835, -23.67439350822212774 ) ) ;
#25541 = ORIENTED_EDGE ( 'NONE', *, *, #15732, .F. ) ;
#25542 = VECTOR ( 'NONE', #33738, 1000.000000000000000 ) ;
#25543 = CARTESIAN_POINT ( 'NONE',  ( 23.24047374271772881, 7.861801299833793166, 11.64928986029708646 ) ) ;
#25544 = CARTESIAN_POINT ( 'NONE',  ( 188.4389256074243804, 86.37278721358588029, 65.15060996993756248 ) ) ;
#25545 = CARTESIAN_POINT ( 'NONE',  ( -125.0023254877051784, 45.90912477771773581, 3.814780357039786018 ) ) ;
#25546 = CARTESIAN_POINT ( 'NONE',  ( 67.56108154898466012, 13.77276756375642819, -64.07949261852301959 ) ) ;
#25547 = LINE ( 'NONE', #41707, #11705 ) ;
#25548 = CARTESIAN_POINT ( 'NONE',  ( 123.4242852856285566, 0.000000000000000000, -20.00000000000000000 ) ) ;
#25549 = FACE_OUTER_BOUND ( 'NONE', #6343, .T. ) ;
#25550 = VECTOR ( 'NONE', #43028, 1000.000000000000000 ) ;
#25551 = B_SPLINE_CURVE_WITH_KNOTS ( 'NONE', 3,
 ( #50777, #2598, #40568, #66984, #18776, #19113 ),
 .UNSPECIFIED., .F., .F.,
 ( 4, 2, 4 ),
 ( 2.380731629556566600E-07, 0.002336973833157566377, 0.004673709593152176531 ),
 .UNSPECIFIED. ) ;
#25552 = ORIENTED_EDGE ( 'NONE', *, *, #17726, .T. ) ;
#25553 = DIRECTION ( 'NONE',  ( -0.000000000000000000, -0.000000000000000000, -1.000000000000000000 ) ) ;
#25554 = APPLICATION_PROTOCOL_DEFINITION ( 'draft international standard', 'automotive_design', 1998, #34152 ) ;
#25555 = CARTESIAN_POINT ( 'NONE',  ( 127.2107679985236501, 38.70844091144996213, -40.00839590869377105 ) ) ;
#25556 = DIRECTION ( 'NONE',  ( -0.000000000000000000, 1.000000000000000000, -0.000000000000000000 ) ) ;
#25557 = CARTESIAN_POINT ( 'NONE',  ( 169.9999999999999716, 3.680555555555560243, 4.000000000000000000 ) ) ;
#25558 = CARTESIAN_POINT ( 'NONE',  ( 186.2575601542430661, 85.47765906955507376, -38.28966198675566091 ) ) ;
#25559 = ORIENTED_EDGE ( 'NONE', *, *, #50885, .F. ) ;
#25560 = VERTEX_POINT ( 'NONE', #41893 ) ;
#25561 = CARTESIAN_POINT ( 'NONE',  ( 50.97490815085634352, 0.000000000000000000, -41.68900338898716740 ) ) ;
#25562 = DIRECTION ( 'NONE',  ( -1.000000000000000000, 0.000000000000000000, 0.000000000000000000 ) ) ;
#25563 = ORIENTED_EDGE ( 'NONE', *, *, #64988, .F. ) ;
#25564 = CARTESIAN_POINT ( 'NONE',  ( 117.7447573007802930, 32.50990724960316669, 64.44597210225181527 ) ) ;
#25565 = ORIENTED_EDGE ( 'NONE', *, *, #32697, .F. ) ;
#25566 = CARTESIAN_POINT ( 'NONE',  ( 126.4219470349616472, 38.26519385429185149, -69.34525928969384267 ) ) ;
#25567 = CARTESIAN_POINT ( 'NONE',  ( 131.6189313563687620, 40.08924984825279125, 44.18369947482882054 ) ) ;
#25568 = DIRECTION ( 'NONE',  ( 1.000000000000000000, 0.000000000000000000, -2.220446049250313081E-16 ) ) ;
#25570 = ADVANCED_FACE ( 'NONE', ( #51070 ), #29961, .F. ) ;
#25569 = CARTESIAN_POINT ( 'NONE',  ( -94.77925136849378873, 29.13093715379786985, 38.25092316674201953 ) ) ;
#25571 = CARTESIAN_POINT ( 'NONE',  ( -15.55634918610411077, -46.66904755831208718, 85.00100000000000477 ) ) ;
#25573 = VERTEX_POINT ( 'NONE', #3918 ) ;
#25572 = CARTESIAN_POINT ( 'NONE',  ( 0.000000000000000000, 0.000000000000000000, 0.000000000000000000 ) ) ;
#25574 = CARTESIAN_POINT ( 'NONE',  ( -24.40147488398712383, 5.437648709335531905, 0.000000000000000000 ) ) ;
#25575 = ADVANCED_FACE ( 'NONE', ( #14806 ), #25038, .F. ) ;
#25576 = ORIENTED_EDGE ( 'NONE', *, *, #60819, .T. ) ;
#25577 = EDGE_LOOP ( 'NONE', ( #4882, #38723 ) ) ;
#25578 = VECTOR ( 'NONE', #33319, 1000.000000000000000 ) ;
#25579 = CARTESIAN_POINT ( 'NONE',  ( -121.5921196778231348, 43.72569502503143468, -21.73089978396855315 ) ) ;
#25580 = EDGE_CURVE ( 'NONE', #13843, #33368, #20096, .T. ) ;
#25581 = CARTESIAN_POINT ( 'NONE',  ( 69.77839676787863255, 27.52340539440045575, 43.58025477438756923 ) ) ;
#25582 = DIRECTION ( 'NONE',  ( 0.000000000000000000, 1.000000000000000000, 0.000000000000000000 ) ) ;
#25583 = CIRCLE ( 'NONE', #34580, 5.000000000000004441 ) ;
#25585 = ORIENTED_EDGE ( 'NONE', *, *, #54699, .F. ) ;
#25584 = FACE_OUTER_BOUND ( 'NONE', #9045, .T. ) ;
#25586 = DIRECTION ( 'NONE',  ( -0.000000000000000000, 1.000000000000000000, -0.000000000000000000 ) ) ;
#25587 = EDGE_CURVE ( 'NONE', #39558, #31561, #19746, .T. ) ;
#25588 = DIRECTION ( 'NONE',  ( -0.000000000000000000, 1.000000000000000000, -0.000000000000000000 ) ) ;
#25589 = VECTOR ( 'NONE', #57751, 1000.000000000000000 ) ;
#25590 = VERTEX_POINT ( 'NONE', #46128 ) ;
#25591 = AXIS2_PLACEMENT_3D ( 'NONE', #7878, #29328, #34144 ) ;
#25592 = CARTESIAN_POINT ( 'NONE',  ( -56.97107423601133291, 15.20373812575556016, -23.13835194742880219 ) ) ;
#25593 = VECTOR ( 'NONE', #49971, 1000.000000000000000 ) ;
#25594 = CARTESIAN_POINT ( 'NONE',  ( -126.7944042662569331, 48.29830493043731821, -76.71781960598816852 ) ) ;
#25595 = LINE ( 'NONE', #64239, #54992 ) ;
#25596 = CARTESIAN_POINT ( 'NONE',  ( -452.6627218934913230, 399.9999999999997726, 83.55029585798818914 ) ) ;
#25597 = CARTESIAN_POINT ( 'NONE',  ( 66.73431804020511038, 14.60294556126670074, -76.58299347307310256 ) ) ;
#25598 = EDGE_CURVE ( 'NONE', #49220, #69425, #42191, .T. ) ;
#25599 = ORIENTED_EDGE ( 'NONE', *, *, #56469, .F. ) ;
#25600 = ORIENTED_EDGE ( 'NONE', *, *, #10230, .F. ) ;
#25601 = CARTESIAN_POINT ( 'NONE',  ( 186.6118452967671999, 84.37814701615438651, -65.47550467027663501 ) ) ;
#25602 = CARTESIAN_POINT ( 'NONE',  ( 149.4165763529819344, -26.99999999999998224, 108.9999999999999858 ) ) ;
#25603 = CARTESIAN_POINT ( 'NONE',  ( 47.99999999999997158, -19.99999999999997868, 4.000000000000000000 ) ) ;
#25604 = CARTESIAN_POINT ( 'NONE',  ( 15.78827728214693416, -170.0000000000000000, 30.01470767270522089 ) ) ;
#25605 = CARTESIAN_POINT ( 'NONE',  ( -76.10382222627279702, 22.43453174720079346, 44.97093298109892601 ) ) ;
#25606 = DIRECTION ( 'NONE',  ( 0.000000000000000000, 0.000000000000000000, 1.000000000000000000 ) ) ;
#25607 = CARTESIAN_POINT ( 'NONE',  ( 68.62997155117720638, 15.08415013720829023, -38.22382599589664665 ) ) ;
#25608 = CARTESIAN_POINT ( 'NONE',  ( -124.9915686518654638, 47.10215472274616388, 45.61994787315713040 ) ) ;
#25609 = CARTESIAN_POINT ( 'NONE',  ( -167.1534554062404254, 80.72263015867913793, -64.50659429279633628 ) ) ;
#25610 = ORIENTED_EDGE ( 'NONE', *, *, #11120, .F. ) ;
#25611 = CARTESIAN_POINT ( 'NONE',  ( 9.249622075198342230, 70.00000000000000000, 3.800590936420744193 ) ) ;
#25612 = VERTEX_POINT ( 'NONE', #68623 ) ;
#25613 = CARTESIAN_POINT ( 'NONE',  ( -38.92726670956012924, 10.94099576009806540, 10.38315399778749182 ) ) ;
#25614 = SURFACE_STYLE_USAGE ( .BOTH. , #15045 ) ;
#25615 = DIRECTION ( 'NONE',  ( 0.6910626489868685329, -0.7227948638273878901, 0.000000000000000000 ) ) ;
#25616 = DIRECTION ( 'NONE',  ( -0.7071067811865507924, 0.000000000000000000, 0.7071067811865441310 ) ) ;
#25617 = CARTESIAN_POINT ( 'NONE',  ( 36.99999522780156269, 9.122638774496634184, 3.460098081212315879 ) ) ;
#25618 = DIRECTION ( 'NONE',  ( -0.2225209339563184452, 0.9749279121818226201, 0.000000000000000000 ) ) ;
#25619 = B_SPLINE_CURVE_WITH_KNOTS ( 'NONE', 3,
 ( #60132, #34470, #11946, #66830, #65419, #34112, #44293, #44664, #13012, #23559, #18275, #17927, #39041, #39381, #55550, #2443, #7381, #42676, #26162, #21562, #52875, #31781, #42340, #57831, #52544, #47594, #63455, #69052, #43005, #41991, #37743, #26850, #43358, #10319, #64481, #58497, #53564, #37392, #64132, #15609, #4367, #4700, #47944 ),
 .UNSPECIFIED., .F., .F.,
 ( 4, 2, 2, 2, 2, 2, 2, 2, 1, 2, 2, 2, 2, 2, 2, 2, 2, 2, 2, 2, 2, 4 ),
 ( 0.000000000000000000, 0.001466540241398133155, 0.002199810362097199840, 0.002933080482796266309, 0.004399620724194398813, 0.005866160965592531751, 0.007332701206990664689, 0.008065971327689734627, 0.008799241448388802830, 0.009532511569087872769, 0.01026578168978694271, 0.01173232193118507391, 0.01319886217258320858, 0.01466540241398133979, 0.01539867253468040625, 0.01613194265537947272, 0.01759848289677760913, 0.01906502313817574554, 0.01979829325887481201, 0.02053156337957387848, 0.02199810362097201488, 0.02346464386237014782 ),
 .UNSPECIFIED. ) ;
#25620 = CARTESIAN_POINT ( 'NONE',  ( -447.6627218934913799, 369.9999999999998295, -141.4497041420117966 ) ) ;
#25621 = LINE ( 'NONE', #36505, #25531 ) ;
#25622 = LINE ( 'NONE', #37186, #56225 ) ;
#25623 = ORIENTED_EDGE ( 'NONE', *, *, #50443, .F. ) ;
#25624 = VECTOR ( 'NONE', #32981, 1000.000000000000000 ) ;
#25625 = LINE ( 'NONE', #52339, #45458 ) ;
#25626 = ORIENTED_EDGE ( 'NONE', *, *, #3558, .F. ) ;
#25627 = CARTESIAN_POINT ( 'NONE',  ( 9.850262805259839993, 200.0000000000000000, -1.724042536399416070 ) ) ;
#25628 = CARTESIAN_POINT ( 'NONE',  ( 9.045716588192249219, 7.384596431530731309, -66.54232190796312807 ) ) ;
#25629 = CARTESIAN_POINT ( 'NONE',  ( -29.04258984626622819, 9.210213971636683539, 3.760888133432336300 ) ) ;
#25630 = FACE_OUTER_BOUND ( 'NONE', #43956, .T. ) ;
#25631 = CARTESIAN_POINT ( 'NONE',  ( -61.37337919387653784, 16.46775785994717722, -92.36217547766979408 ) ) ;
#25632 = CARTESIAN_POINT ( 'NONE',  ( -94.89192151156323973, 29.18342430963126333, -16.98616732492110515 ) ) ;
#25633 = CIRCLE ( 'NONE', #14380, 2.999999999999981792 ) ;
#25634 = CARTESIAN_POINT ( 'NONE',  ( 150.7770046255792806, 53.87214803240242134, -40.23014915691795323 ) ) ;
#25635 = VECTOR ( 'NONE', #41114, 1000.000000000000000 ) ;
#25636 = ORIENTED_EDGE ( 'NONE', *, *, #34581, .F. ) ;
#25637 = CARTESIAN_POINT ( 'NONE',  ( 620.5071894358270583, 928.5915846175170145, 486.5068267248709049 ) ) ;
#25638 = CARTESIAN_POINT ( 'NONE',  ( -156.8773151811563196, 72.06122063279305223, 66.48491347657433437 ) ) ;
#25639 = DIRECTION ( 'NONE',  ( -0.000000000000000000, -0.000000000000000000, 1.000000000000000000 ) ) ;
#25640 = CARTESIAN_POINT ( 'NONE',  ( -102.2801239173131052, 33.91021738430207222, -8.170026674512225640 ) ) ;
#25641 = VECTOR ( 'NONE', #51873, 1000.000000000000000 ) ;
#25642 = CARTESIAN_POINT ( 'NONE',  ( -126.3453033442920912, 47.99870040347946087, -49.91370389823397602 ) ) ;
#25643 = EDGE_LOOP ( 'NONE', ( #43314, #13413, #2335, #37991 ) ) ;
#25644 = CARTESIAN_POINT ( 'NONE',  ( -178.5848962563134137, 94.99295350784007042, -63.89442975738296582 ) ) ;
#25645 = EDGE_CURVE ( 'NONE', #23880, #14487, #35930, .T. ) ;
#25646 = CARTESIAN_POINT ( 'NONE',  ( 89.22118407503262461, 20.32164250407901562, 71.09862284774732188 ) ) ;
#25647 = CARTESIAN_POINT ( 'NONE',  ( 115.0454575488273434, 31.16784721673997183, 31.34535846184481755 ) ) ;
#25648 = DIRECTION ( 'NONE',  ( -1.000000000000000000, 0.000000000000000000, 0.000000000000000000 ) ) ;
#25649 = AXIS2_PLACEMENT_3D ( 'NONE', #26881, #65569, #54646 ) ;
#25650 = CARTESIAN_POINT ( 'NONE',  ( 140.5781926063689298, 45.63383190293698988, 33.67300037928345802 ) ) ;
#25651 = ORIENTED_EDGE ( 'NONE', *, *, #27790, .T. ) ;
#25652 = CARTESIAN_POINT ( 'NONE',  ( 201.9777685760379882, 102.6876480786892500, 29.70620911343904780 ) ) ;
#25653 = CARTESIAN_POINT ( 'NONE',  ( 113.8748103246145433, 30.59837980920001854, -63.68721912812959118 ) ) ;
#25654 = CARTESIAN_POINT ( 'NONE',  ( 23.17627457812085723, 71.32923872213659422, 0.000000000000000000 ) ) ;
#25655 = CARTESIAN_POINT ( 'NONE',  ( 186.3581035978320131, 84.10482028537325050, -92.06749394508619844 ) ) ;
#25656 = DIRECTION ( 'NONE',  ( -0.000000000000000000, -0.000000000000000000, -1.000000000000000000 ) ) ;
#25657 = ORIENTED_EDGE ( 'NONE', *, *, #15706, .T. ) ;
#25658 = CARTESIAN_POINT ( 'NONE',  ( 179.0091171455097765, 77.94933395983134972, 56.43303025292213704 ) ) ;
#25659 = EDGE_CURVE ( 'NONE', #9838, #7089, #30309, .T. ) ;
#25660 = ORIENTED_EDGE ( 'NONE', *, *, #29287, .F. ) ;
#25661 = CARTESIAN_POINT ( 'NONE',  ( -109.7816385129979295, 36.75776661907239173, -43.01526495903692648 ) ) ;
#25662 = CARTESIAN_POINT ( 'NONE',  ( 127.2283196959457001, 37.56363777789739800, 87.17274213372091651 ) ) ;
#25663 = CARTESIAN_POINT ( 'NONE',  ( -62.45176220516619026, 16.79101814080731359, 39.06955276880188421 ) ) ;
#25665 = ORIENTED_EDGE ( 'NONE', *, *, #62080, .T. ) ;
#25664 = CARTESIAN_POINT ( 'NONE',  ( 183.2136430849848239, 0.000000000000000000, -9.435653166495541200 ) ) ;
#25666 = DIRECTION ( 'NONE',  ( 1.000000000000000000, 0.000000000000000000, -0.000000000000000000 ) ) ;
#25667 = EDGE_CURVE ( 'NONE', #68633, #66387, #51758, .T. ) ;
#25668 = PLANE ( 'NONE',  #46272 ) ;
#25669 = CARTESIAN_POINT ( 'NONE',  ( 116.0963032583227772, 32.80867113471310148, -48.13800676814181401 ) ) ;
#25670 = EDGE_LOOP ( 'NONE', ( #57020, #24001, #35380, #19167 ) ) ;
#25671 = DIRECTION ( 'NONE',  ( 1.000000000000000000, 1.019401483866766449E-14, -9.729483335668566592E-15 ) ) ;
#25672 = ADVANCED_BREP_SHAPE_REPRESENTATION ( '', ( #17690, #66832 ), #28752 ) ;
#25673 = CIRCLE ( 'NONE', #20040, 5.000000000000000888 ) ;
#25674 = PLANE ( 'NONE',  #9652 ) ;
#25675 = ORIENTED_EDGE ( 'NONE', *, *, #31957, .F. ) ;
#25676 = CARTESIAN_POINT ( 'NONE',  ( 140.5781926063689582, 45.63383190293701119, 60.51755096974717674 ) ) ;
#25677 = CARTESIAN_POINT ( 'NONE',  ( -165.6210506643949429, 79.15024150453837137, 38.62296396642691576 ) ) ;
#25678 = CARTESIAN_POINT ( 'NONE',  ( 152.8430172091323413, 54.14068524174419395, 57.84683868187476463 ) ) ;
#25679 = CARTESIAN_POINT ( 'NONE',  ( -5.767955557622883589E-14, -31.11269837220806878, 2.000000000000001776 ) ) ;
#25680 = EDGE_CURVE ( 'NONE', #34130, #145, #9193, .T. ) ;
#25681 = VERTEX_POINT ( 'NONE', #9543 ) ;
#25682 = VECTOR ( 'NONE', #63615, 1000.000000000000000 ) ;
#25683 = CARTESIAN_POINT ( 'NONE',  ( 41.80372346091802171, 9.750024116765237281, 17.67854651459926529 ) ) ;
#25684 = EDGE_LOOP ( 'NONE', ( #17308, #34791, #31778, #22052, #46432, #17710, #62604, #16695, #44227, #20708, #64791 ) ) ;
#25685 = EDGE_CURVE ( 'NONE', #54974, #43521, #69131, .T. ) ;
#25686 = CARTESIAN_POINT ( 'NONE',  ( 152.6804161981488619, 55.27286404993341051, -22.55585361910392095 ) ) ;
#25687 = VECTOR ( 'NONE', #63656, 1000.000000000000000 ) ;
#25688 = CARTESIAN_POINT ( 'NONE',  ( -58.41772555885023621, 15.60941139747057349, 84.79622561241443179 ) ) ;
#25689 = LINE ( 'NONE', #3520, #15581 ) ;
#25690 = CARTESIAN_POINT ( 'NONE',  ( -155.5978531700835674, 69.52241200678680855, -64.77328047304274605 ) ) ;
#25691 = CARTESIAN_POINT ( 'NONE',  ( 55.92341725501096761, 11.13877080681674414, 88.53962230442249393 ) ) ;
#25692 = CARTESIAN_POINT ( 'NONE',  ( 188.2086267457325448, 87.61890531228284829, 7.603719067856809843 ) ) ;
#25693 = CARTESIAN_POINT ( 'NONE',  ( 206.3125232506203304, 108.5822159704962218, -36.49056922416787785 ) ) ;
#25694 = CARTESIAN_POINT ( 'NONE',  ( 422.4999999999999432, 207.5000000000000284, 0.000000000000000000 ) ) ;
#25695 = ORIENTED_EDGE ( 'NONE', *, *, #5545, .F. ) ;
#25696 = DIRECTION ( 'NONE',  ( -1.000000000000000000, -0.000000000000000000, -0.000000000000000000 ) ) ;
#25697 = ORIENTED_EDGE ( 'NONE', *, *, #57101, .F. ) ;
#25698 = CARTESIAN_POINT ( 'NONE',  ( -76.79042791651912125, 22.68960395613480685, 72.02825304396196771 ) ) ;
#25699 = CARTESIAN_POINT ( 'NONE',  ( 188.1848725084043110, 87.59259440284084519, -95.00000000000133582 ) ) ;
#25700 = DIRECTION ( 'NONE',  ( 1.000000000000000000, 0.000000000000000000, 0.000000000000000000 ) ) ;
#25701 = FACE_OUTER_BOUND ( 'NONE', #67013, .T. ) ;
#25702 = CARTESIAN_POINT ( 'NONE',  ( -0.3421259600789157140, 6.519162826741678352, 91.90210512622793715 ) ) ;
#25703 = DIRECTION ( 'NONE',  ( 1.000000000000000000, 0.000000000000000000, 0.000000000000000000 ) ) ;
#25704 = ORIENTED_EDGE ( 'NONE', *, *, #62580, .T. ) ;
#25705 = CARTESIAN_POINT ( 'NONE',  ( -72.21652659655761397, 19.96855882996549525, 60.90274179765688700 ) ) ;
#25706 = CARTESIAN_POINT ( 'NONE',  ( -170.2747214445850261, 84.01465441107045251, 72.11803030135118320 ) ) ;
#25707 = ORIENTED_EDGE ( 'NONE', *, *, #31739, .F. ) ;
#25708 = VERTEX_POINT ( 'NONE', #20428 ) ;
#25709 = B_SPLINE_CURVE_WITH_KNOTS ( 'NONE', 3,
 ( #67184, #9805, #61865, #13693, #46042, #62218, #14039, #64295, #16103, #624 ),
 .UNSPECIFIED., .F., .F.,
 ( 4, 2, 2, 2, 4 ),
 ( 0.000000000000000000, 0.002514917400237022104, 0.005029834800474044208, 0.007544752200711065879, 0.01005966960094808842 ),
 .UNSPECIFIED. ) ;
#25710 = CARTESIAN_POINT ( 'NONE',  ( -149.9449619562961686, 64.55090813009799433, 30.72082123989904900 ) ) ;
#25711 = CARTESIAN_POINT ( 'NONE',  ( 57.08336938683660833, 11.37442068895386349, -38.60525425700638635 ) ) ;
#25712 = CARTESIAN_POINT ( 'NONE',  ( 127.7121523762017858, 37.83617439506281244, 94.99999999999866418 ) ) ;
#25713 = CARTESIAN_POINT ( 'NONE',  ( 181.0840389613909736, -170.0000000000000000, 9.964043515047732669 ) ) ;
#25714 = DIRECTION ( 'NONE',  ( 1.000000000000000000, -0.000000000000000000, 0.000000000000000000 ) ) ;
#25715 = ORIENTED_EDGE ( 'NONE', *, *, #37030, .F. ) ;
#25716 = CARTESIAN_POINT ( 'NONE',  ( -132.6092625803566989, 52.31125232006264980, 41.46967621612935773 ) ) ;
#25717 = ORIENTED_EDGE ( 'NONE', *, *, #61795, .F. ) ;
#25718 = CARTESIAN_POINT ( 'NONE',  ( 206.2980740120524388, 108.5619562183279925, 2.524772047937632102 ) ) ;
#25719 = CARTESIAN_POINT ( 'NONE',  ( 10.82760985890677219, 7.398654328676804504, 70.00562821550327897 ) ) ;
#25720 = CARTESIAN_POINT ( 'NONE',  ( 210.9506883977752523, 115.3310071214937267, 32.55822520530563224 ) ) ;
#25721 = EDGE_CURVE ( 'NONE', #60122, #11337, #2882, .T. ) ;
#25722 = DIRECTION ( 'NONE',  ( -1.000000000000000000, 0.000000000000000000, 0.000000000000000000 ) ) ;
#25723 = EDGE_CURVE ( 'NONE', #9408, #24552, #36625, .T. ) ;
#25724 = ORIENTED_EDGE ( 'NONE', *, *, #51957, .F. ) ;
#25725 = CIRCLE ( 'NONE', #58246, 2.999999999999981792 ) ;
#25726 = VERTEX_POINT ( 'NONE', #32033 ) ;
#25727 = CARTESIAN_POINT ( 'NONE',  ( 114.3366674800923732, -21.85806848808613267, 2.509805449637990016 ) ) ;
#25728 = CARTESIAN_POINT ( 'NONE',  ( -128.2034271809940549, 49.24731531185076250, 84.65107715705232749 ) ) ;
#25729 = CARTESIAN_POINT ( 'NONE',  ( 33.75794032130628608, 8.754084575552436576, -65.00099313904955523 ) ) ;
#25730 = CARTESIAN_POINT ( 'NONE',  ( 22.18075376363910323, 11.79626863379964696, 0.000000000000000000 ) ) ;
#25731 = CARTESIAN_POINT ( 'NONE',  ( 10.95123459301218816, 6.393971377372064779, 85.46269591332465154 ) ) ;
#25732 = CARTESIAN_POINT ( 'NONE',  ( 18.36632403430998295, 7.603901913571097460, 84.15309218088728471 ) ) ;
#25733 = AXIS2_PLACEMENT_3D ( 'NONE', #66482, #65782, #29181 ) ;
#25734 = EDGE_LOOP ( 'NONE', ( #14924, #64012, #58633, #54333 ) ) ;
#25736 = EDGE_CURVE ( 'NONE', #56977, #1254, #16191, .T. ) ;
#25735 = LINE ( 'NONE', #46828, #28064 ) ;
#25737 = CARTESIAN_POINT ( 'NONE',  ( -101.3492134984965389, 32.31003911421603192, 72.32043172286272181 ) ) ;
#25738 = ORIENTED_EDGE ( 'NONE', *, *, #7662, .F. ) ;
#25739 = ADVANCED_FACE ( 'NONE', ( #32380 ), #21465, .F. ) ;
#25740 = CARTESIAN_POINT ( 'NONE',  ( -81.67992981004165642, 23.49232121719083111, 4.201518040229789364 ) ) ;
#25741 = EDGE_LOOP ( 'NONE', ( #689, #12007 ) ) ;
#25742 = PLANE ( 'NONE',  #24181 ) ;
#25743 = EDGE_LOOP ( 'NONE', ( #67168, #54680, #60983, #6809 ) ) ;
#25744 = EDGE_CURVE ( 'NONE', #41626, #49164, #5296, .T. ) ;
#25745 = ORIENTED_EDGE ( 'NONE', *, *, #11405, .F. ) ;
#25746 = CARTESIAN_POINT ( 'NONE',  ( -122.8202784017355782, 45.69728649588468272, 18.12070328134850783 ) ) ;
#25747 = EDGE_CURVE ( 'NONE', #53100, #68618, #59439, .T. ) ;
#25748 = CARTESIAN_POINT ( 'NONE',  ( -180.6209440844958181, 95.88392769199012378, 65.48622505976561570 ) ) ;
#25749 = CARTESIAN_POINT ( 'NONE',  ( 133.6288034103009750, 41.28708886999548611, 56.35489142945903041 ) ) ;
#25750 = ORIENTED_EDGE ( 'NONE', *, *, #60981, .F. ) ;
#25751 = DIRECTION ( 'NONE',  ( 0.000000000000000000, 0.000000000000000000, 1.000000000000000000 ) ) ;
#25752 = CARTESIAN_POINT ( 'NONE',  ( 0.000000000000000000, 0.000000000000000000, 41.38025477438755928 ) ) ;
#25753 = LINE ( 'NONE', #3593, #35916 ) ;
#25754 = B_SPLINE_CURVE_WITH_KNOTS ( 'NONE', 3,
 ( #41609, #57789, #42302, #63764 ),
 .UNSPECIFIED., .F., .F.,
 ( 4, 4 ),
 ( 9.900409498950027967E-07, 0.05658314289920114010 ),
 .UNSPECIFIED. ) ;
#25755 = FACE_OUTER_BOUND ( 'NONE', #49209, .T. ) ;
#25756 = EDGE_CURVE ( 'NONE', #43631, #8543, #20778, .T. ) ;
#25757 = CARTESIAN_POINT ( 'NONE',  ( -29.75049355503753290, 9.320234381800291956, 30.40492039785981504 ) ) ;
#25758 = DIRECTION ( 'NONE',  ( -0.04486483035051862939, 0.9989930665413143673, 0.000000000000000000 ) ) ;
#25759 = ORIENTED_EDGE ( 'NONE', *, *, #13168, .F. ) ;
#25760 = EDGE_CURVE ( 'NONE', #26008, #61883, #47495, .T. ) ;
#25761 = ADVANCED_FACE ( 'NONE', ( #15513 ), #68956, .T. ) ;
#25762 = ADVANCED_FACE ( 'NONE', ( #27432 ), #22169, .F. ) ;
#25763 = DIRECTION ( 'NONE',  ( 9.110201094256374036E-19, -5.020134576618366632E-18, -1.000000000000000000 ) ) ;
#25764 = CARTESIAN_POINT ( 'NONE',  ( -81.00768240531206743, 24.30850321514432011, -76.58921506343186536 ) ) ;
#25765 = CARTESIAN_POINT ( 'NONE',  ( 175.8874477961783782, 74.89984466412600739, 15.39286893903958742 ) ) ;
#25766 = DIRECTION ( 'NONE',  ( 0.2225209339563184452, -0.9749279121818226201, 0.000000000000000000 ) ) ;
#25767 = LINE ( 'NONE', #47196, #53456 ) ;
#25768 = CARTESIAN_POINT ( 'NONE',  ( 129.6961120139403647, 38.96846414226716604, 3.921094800805867919 ) ) ;
#25769 = CARTESIAN_POINT ( 'NONE',  ( -149.5074843970971017, 64.17983161892347255, 18.87627064943540134 ) ) ;
#25770 = DIRECTION ( 'NONE',  ( 1.000000000000000000, 0.000000000000000000, 0.000000000000000000 ) ) ;
#25771 = CARTESIAN_POINT ( 'NONE',  ( 211.4997502125519304, 118.0043045815490075, 33.53397494038922844 ) ) ;
#25772 = CARTESIAN_POINT ( 'NONE',  ( 11.30618213853490239, -74.15344055032291237, 170.0000000000000000 ) ) ;
#25773 = CARTESIAN_POINT ( 'NONE',  ( -106.6781182590523400, 35.07133425426479079, 44.11266599922410592 ) ) ;
#25774 = VERTEX_POINT ( 'NONE', #7 ) ;
#25775 = CARTESIAN_POINT ( 'NONE',  ( -61.07136008913403202, 17.42761989316184668, 87.01993574156381328 ) ) ;
#25776 = EDGE_LOOP ( 'NONE', ( #63884, #9604, #44304, #46673 ) ) ;
#25777 = CARTESIAN_POINT ( 'NONE',  ( -78.66644367742111399, -170.0000000000000000, 3.573650549209445693 ) ) ;
#25778 = VERTEX_POINT ( 'NONE', #59093 ) ;
#25779 = B_SPLINE_CURVE_WITH_KNOTS ( 'NONE', 3,
 ( #3825, #62919, #31589, #51671, #53028, #24939, #15417, #3477 ),
 .UNSPECIFIED., .F., .F.,
 ( 4, 2, 2, 4 ),
 ( 0.004673709593152151377, 0.005837709341827642534, 0.007001709090503133691, 0.009329708587854115137 ),
 .UNSPECIFIED. ) ;
#25780 = VECTOR ( 'NONE', #50037, 1000.000000000000000 ) ;
#25781 = CARTESIAN_POINT ( 'NONE',  ( 23.28845814680233062, 7.864847136539614425, -70.35012750131396331 ) ) ;
#25782 = CARTESIAN_POINT ( 'NONE',  ( 8.000000000000007105, 249.8719672152120381, 94.99999999999866418 ) ) ;
#25783 = CARTESIAN_POINT ( 'NONE',  ( -146.1201263095600495, 62.66021356509619977, 71.76068813120549805 ) ) ;
#25784 = DIRECTION ( 'NONE',  ( -0.7071067811865476838, 6.441404958702661839E-16, -0.7071067811865474617 ) ) ;
#25786 = CARTESIAN_POINT ( 'NONE',  ( 140.2058232509808136, 46.59155168125935376, -39.49978839522578511 ) ) ;
#25785 = AXIS2_PLACEMENT_3D ( 'NONE', #14560, #2979, #2622 ) ;
#25787 = CARTESIAN_POINT ( 'NONE',  ( 33.75639351246966413, 7.742023566824293823, -48.08197975767080834 ) ) ;
#25788 = CARTESIAN_POINT ( 'NONE',  ( 8.288696687633805738, 7.382586467017841159, -43.51982814552570034 ) ) ;
#25789 = DIRECTION ( 'NONE',  ( 0.2225209339563184452, -0.9749279121818226201, 0.000000000000000000 ) ) ;
#25790 = DIRECTION ( 'NONE',  ( 0.000000000000000000, 0.000000000000000000, 1.000000000000000000 ) ) ;
#25791 = VERTEX_POINT ( 'NONE', #26067 ) ;
#25792 = ORIENTED_EDGE ( 'NONE', *, *, #46678, .T. ) ;
#25793 = CARTESIAN_POINT ( 'NONE',  ( 173.6288500197769338, 72.76107365126398463, 89.65482327789845840 ) ) ;
#25794 = CARTESIAN_POINT ( 'NONE',  ( -3.841371665203041630E-11, 0.000000000000000000, 0.000000000000000000 ) ) ;
#25795 = CARTESIAN_POINT ( 'NONE',  ( 127.5827380604433188, 38.91881311236849683, -93.08189994083937790 ) ) ;
#25796 = AXIS2_PLACEMENT_3D ( 'NONE', #38277, #65373, #44606 ) ;
#25797 = CARTESIAN_POINT ( 'NONE',  ( -20.55634918610403261, 2.818925648462311528E-14, 85.00100000000000477 ) ) ;
#25798 = CARTESIAN_POINT ( 'NONE',  ( 282.2165994398968110, 21.53656025449836520, -4.493648593974075567 ) ) ;
#25799 = CARTESIAN_POINT ( 'NONE',  ( 181.0840389613909451, 80.03940679743416808, -9.380507075415923879 ) ) ;
#25800 = LINE ( 'NONE', #15232, #43881 ) ;
#25801 = CARTESIAN_POINT ( 'NONE',  ( -2.645453300864630819E-14, -15.55634918610403616, 85.00100000000000477 ) ) ;
#25802 = CARTESIAN_POINT ( 'NONE',  ( 94.07616572255075482, 22.09777530676769430, -17.50139387669658220 ) ) ;
#25803 = DIRECTION ( 'NONE',  ( -0.000000000000000000, 1.000000000000000000, -0.000000000000000000 ) ) ;
#25804 = CARTESIAN_POINT ( 'NONE',  ( -42.32797523529043104, -61.85511477251480983, 41.38025477438755928 ) ) ;
#25805 = CARTESIAN_POINT ( 'NONE',  ( -2.645453300864630819E-14, -15.55634918610403616, 85.00100000000000477 ) ) ;
#25806 = EDGE_CURVE ( 'NONE', #42469, #55620, #16542, .T. ) ;
#25807 = ORIENTED_EDGE ( 'NONE', *, *, #50010, .F. ) ;
#25808 = LINE ( 'NONE', #69393, #58241 ) ;
#25809 = DIRECTION ( 'NONE',  ( -0.6427876096865403621, -0.7660444431189770143, 0.000000000000000000 ) ) ;
#25810 = CARTESIAN_POINT ( 'NONE',  ( 157.4703587214989398, 58.92748579479259519, 71.25401806271709404 ) ) ;
#25811 = DIRECTION ( 'NONE',  ( 0.000000000000000000, 0.000000000000000000, 1.000000000000000000 ) ) ;
#25812 = AXIS2_PLACEMENT_3D ( 'NONE', #28884, #50672, #29224 ) ;
#25813 = CARTESIAN_POINT ( 'NONE',  ( 39.40195752203892710, 9.424259417798131366, 3.069283715499574239 ) ) ;
#25814 = ORIENTED_EDGE ( 'NONE', *, *, #55858, .F. ) ;
#25816 = EDGE_CURVE ( 'NONE', #57474, #46683, #16878, .T. ) ;
#25815 = FACE_BOUND ( 'NONE', #52151, .T. ) ;
#25817 = ADVANCED_FACE ( 'NONE', ( #53806 ), #64374, .T. ) ;
#25818 = FACE_OUTER_BOUND ( 'NONE', #64013, .T. ) ;
#25819 = ORIENTED_EDGE ( 'NONE', *, *, #56960, .T. ) ;
#25820 = B_SPLINE_CURVE_WITH_KNOTS ( 'NONE', 3,
 ( #3948, #62344, #3261, #61648, #24375, #19423, #56031, #45818, #8884, #8188, #39847, #34595, #35618, #30335, #51787, #3598, #25066, #46496 ),
 .UNSPECIFIED., .F., .F.,
 ( 4, 2, 2, 2, 2, 2, 2, 2, 4 ),
 ( 0.01419378663595921401, 0.01762610661014687996, 0.01934226659724071207, 0.02105842658433454417, 0.02277458657142837628, 0.02449074655852220839, 0.02620690654561604049, 0.02706498653916294267, 0.02792306653270984484 ),
 .UNSPECIFIED. ) ;
#25821 = ORIENTED_EDGE ( 'NONE', *, *, #39306, .T. ) ;
#25822 = CARTESIAN_POINT ( 'NONE',  ( 32.01010588308077587, 8.573952726883749875, 92.53496508106553620 ) ) ;
#25823 = CARTESIAN_POINT ( 'NONE',  ( -1.298947065946362001, -170.0000000000000000, 94.99999999999866418 ) ) ;
#25824 = DIRECTION ( 'NONE',  ( 0.000000000000000000, 0.000000000000000000, 1.000000000000000000 ) ) ;
#25825 = ORIENTED_EDGE ( 'NONE', *, *, #47700, .T. ) ;
#25826 = CIRCLE ( 'NONE', #10091, 74.95140232871122521 ) ;
#25827 = EDGE_CURVE ( 'NONE', #42723, #25068, #10325, .T. ) ;
#25828 = CARTESIAN_POINT ( 'NONE',  ( -40.61870061263184084, 17.42188897416313154, -35.38129938736816626 ) ) ;
#25829 = DIRECTION ( 'NONE',  ( 0.000000000000000000, -1.000000000000000000, 0.000000000000000000 ) ) ;
#25830 = CARTESIAN_POINT ( 'NONE',  ( 37.00112095025829717, 8.109340230899350743, -9.165684967028395747 ) ) ;
#25831 = EDGE_CURVE ( 'NONE', #27030, #19968, #2742, .T. ) ;
#25832 = CARTESIAN_POINT ( 'NONE',  ( 174.6242782760050147, 73.69713439533578025, -39.90515018124950331 ) ) ;
#25833 = VECTOR ( 'NONE', #61281, 1000.000000000000000 ) ;
#25834 = CARTESIAN_POINT ( 'NONE',  ( -151.6648563624119390, 67.36546864992754990, -76.35397280829764100 ) ) ;
#25835 = CARTESIAN_POINT ( 'NONE',  ( -452.6627218934913230, 217.8591479523843475, -111.4497041420117966 ) ) ;
#25836 = EDGE_LOOP ( 'NONE', ( #39874, #31621, #61516, #35941 ) ) ;
#25837 = LINE ( 'NONE', #47951, #17694 ) ;
#25838 = CARTESIAN_POINT ( 'NONE',  ( 10.13405324523498763, 6.385324379632245417, 59.40699386941561499 ) ) ;
#25839 = CARTESIAN_POINT ( 'NONE',  ( 15.78827728214693416, 6.500811158483284835, 30.01470767270522089 ) ) ;
#25840 = CARTESIAN_POINT ( 'NONE',  ( 197.8588046850313447, 99.02485934465606476, 39.80106156302998954 ) ) ;
#25841 = CARTESIAN_POINT ( 'NONE',  ( -73.15154738012903124, 21.36451140970928364, 86.51439797908847140 ) ) ;
#25843 = ORIENTED_EDGE ( 'NONE', *, *, #5931, .F. ) ;
#25842 = PLANE ( 'NONE',  #8518 ) ;
#25844 = ORIENTED_EDGE ( 'NONE', *, *, #29862, .F. ) ;
#25845 = VECTOR ( 'NONE', #26789, 1000.000000000000114 ) ;
#25846 = ADVANCED_FACE ( 'NONE', ( #38698 ), #6277, .T. ) ;
#25847 = ORIENTED_EDGE ( 'NONE', *, *, #61538, .T. ) ;
#25848 = LINE ( 'NONE', #47963, #24537 ) ;
#25849 = DIRECTION ( 'NONE',  ( 0.000000000000000000, 0.000000000000000000, 1.000000000000000000 ) ) ;
#25850 = CARTESIAN_POINT ( 'NONE',  ( 203.1511228994172598, 104.2426341584999250, -78.05527855006161531 ) ) ;
#25851 = ADVANCED_FACE ( 'NONE', ( #1766 ), #7391, .T. ) ;
#25852 = DIRECTION ( 'NONE',  ( -0.000000000000000000, 0.000000000000000000, 1.000000000000000000 ) ) ;
#25853 = CARTESIAN_POINT ( 'NONE',  ( -118.7011677090247019, 41.93687969120208692, 62.82317554766216006 ) ) ;
#25854 = CARTESIAN_POINT ( 'NONE',  ( -81.24432217070641116, 24.40203426192926273, -8.723820200429852179 ) ) ;
#25855 = CARTESIAN_POINT ( 'NONE',  ( 19.53470118933706345, 6.649487981843460460, -22.67626940826310999 ) ) ;
#25856 = CARTESIAN_POINT ( 'NONE',  ( -156.9252506979472912, 70.73559306219776488, -43.45703707063664467 ) ) ;
#25857 = VERTEX_POINT ( 'NONE', #33075 ) ;
#25858 = ORIENTED_EDGE ( 'NONE', *, *, #29015, .T. ) ;
#25859 = DIRECTION ( 'NONE',  ( 1.000000000000000000, 0.000000000000000000, 0.000000000000000000 ) ) ;
#25860 = CARTESIAN_POINT ( 'NONE',  ( -80.54915509118112027, 24.12810583352864313, -49.87922971066491584 ) ) ;
#25861 = CARTESIAN_POINT ( 'NONE',  ( 162.8142581494936110, 61.92799983924231810, 69.03799929907479793 ) ) ;
#25862 = VECTOR ( 'NONE', #39872, 1000.000000000000000 ) ;
#25863 = CARTESIAN_POINT ( 'NONE',  ( -151.6797345123119101, 67.37848486615951060, 18.56841981061283420 ) ) ;
#25864 = LINE ( 'NONE', #63833, #9064 ) ;
#25865 = PLANE ( 'NONE',  #52791 ) ;
#25866 = CARTESIAN_POINT ( 'NONE',  ( -5.767955557622883589E-14, -31.11269837220806878, 2.000000000000001776 ) ) ;
#25867 = ORIENTED_EDGE ( 'NONE', *, *, #20731, .T. ) ;
#25868 = ORIENTED_EDGE ( 'NONE', *, *, #51003, .F. ) ;
#25869 = EDGE_LOOP ( 'NONE', ( #45941, #41775, #9574, #47154 ) ) ;
#25870 = FILL_AREA_STYLE ('',( #15308 ) ) ;
#25871 = CARTESIAN_POINT ( 'NONE',  ( 0.000000000000000000, 0.000000000000000000, 7.000000000000000000 ) ) ;
#25872 = CARTESIAN_POINT ( 'NONE',  ( -26.00000000000000000, 0.000000000000000000, -2.818925648462311923E-15 ) ) ;
#25873 = CARTESIAN_POINT ( 'NONE',  ( -35.17718245314462422, 11.25729435722176852, -63.15510929693514441 ) ) ;
#25874 = CARTESIAN_POINT ( 'NONE',  ( -156.1462053606562392, 70.02140399657014314, -11.96835739834466850 ) ) ;
#25875 = CIRCLE ( 'NONE', #2284, 25.12245591505646303 ) ;
#25876 = PRODUCT_RELATED_PRODUCT_CATEGORY ( 'part', '', ( #56359 ) ) ;
#25877 = CARTESIAN_POINT ( 'NONE',  ( -31.43908319763709969, 10.61114334766715572, 3.371903815725488585 ) ) ;
#25878 = CARTESIAN_POINT ( 'NONE',  ( 8.528421445032398296, 6.376778749352035369, -18.11991088350285395 ) ) ;
#25879 = CARTESIAN_POINT ( 'NONE',  ( 22.51798020284707391, 7.817376421459706570, 7.350245662626018195 ) ) ;
#25880 = CARTESIAN_POINT ( 'NONE',  ( 112.3013380801408800, 395.0000000000065938, -133.9497041420121377 ) ) ;
#25881 = CARTESIAN_POINT ( 'NONE',  ( -118.5043919384110893, 41.81711884544878188, 12.58584570400684832 ) ) ;
#25882 = DIRECTION ( 'NONE',  ( 1.850169831522831466E-16, -1.000000000000000000, 5.551115123125781470E-17 ) ) ;
#25883 = CARTESIAN_POINT ( 'NONE',  ( 126.8237978310704221, 37.33705012421151537, -14.06003659058230326 ) ) ;
#25885 = EDGE_CURVE ( 'NONE', #21982, #8644, #60671, .T. ) ;
#25884 = DIRECTION ( 'NONE',  ( 0.000000000000000000, 0.000000000000000000, 1.000000000000000000 ) ) ;
#25886 = CARTESIAN_POINT ( 'NONE',  ( 8.337549025192451779, 7.382630697225775585, 9.682436645409964626 ) ) ;
#25887 = EDGE_CURVE ( 'NONE', #59151, #36200, #34820, .T. ) ;
#25888 = EDGE_LOOP ( 'NONE', ( #58484, #63953, #22373, #1120 ) ) ;
#25889 = FACE_OUTER_BOUND ( 'NONE', #68337, .T. ) ;
#25890 = PRODUCT_CONTEXT ( 'NONE', #58769, 'mechanical' ) ;
#25891 = CARTESIAN_POINT ( 'NONE',  ( 173.8575673535406168, 71.59843387604338716, 34.78079572034797451 ) ) ;
#25892 = CARTESIAN_POINT ( 'NONE',  ( 63.01563776193091826, -170.0000000000000000, 10.46841034875760279 ) ) ;
#25893 = CARTESIAN_POINT ( 'NONE',  ( -109.7811201291769692, 37.90784085457602970, -42.28424908827382467 ) ) ;
#25894 = CARTESIAN_POINT ( 'NONE',  ( 184.0001683447903815, 83.06228184427187955, -50.64836551222349925 ) ) ;
#25895 = ORIENTED_EDGE ( 'NONE', *, *, #59468, .T. ) ;
#25896 = ORIENTED_EDGE ( 'NONE', *, *, #17060, .F. ) ;
#25898 = EDGE_CURVE ( 'NONE', #18637, #34501, #51466, .T. ) ;
#25897 = CARTESIAN_POINT ( 'NONE',  ( -27.70005010046228122, 9.007417901453010245, -9.466521581063075175 ) ) ;
#25899 = CARTESIAN_POINT ( 'NONE',  ( 202.7506655727289342, 105.3943386412348957, 17.11760266916378725 ) ) ;
#25900 = ORIENTED_EDGE ( 'NONE', *, *, #45020, .T. ) ;
#25901 = EDGE_CURVE ( 'NONE', #37545, #22341, #30926, .T. ) ;
#25902 = DIRECTION ( 'NONE',  ( 0.000000000000000000, 0.000000000000000000, 1.000000000000000000 ) ) ;
#25903 = VERTEX_POINT ( 'NONE', #9465 ) ;
#25904 = FACE_OUTER_BOUND ( 'NONE', #62998, .T. ) ;
#25905 = CARTESIAN_POINT ( 'NONE',  ( 128.3856248084844651, 38.21741401878865219, 31.85676776503090224 ) ) ;
#25906 = EDGE_CURVE ( 'NONE', #41593, #36484, #54799, .T. ) ;
#25907 = DIRECTION ( 'NONE',  ( 0.000000000000000000, 1.224646799147357891E-16, 1.000000000000000000 ) ) ;
#25908 = VECTOR ( 'NONE', #11840, 1000.000000000000114 ) ;
#25909 = DIRECTION ( 'NONE',  ( -1.000000000000000000, 0.000000000000000000, 0.000000000000000000 ) ) ;
#25910 = CARTESIAN_POINT ( 'NONE',  ( 6.375108774214766072E-14, 36.11269837220805812, 85.00100000000000477 ) ) ;
#25912 = ORIENTED_EDGE ( 'NONE', *, *, #19759, .F. ) ;
#25911 = DIRECTION ( 'NONE',  ( 1.000000000000000000, 0.000000000000000000, -0.000000000000000000 ) ) ;
#25913 = CARTESIAN_POINT ( 'NONE',  ( 447.3372781065086201, 400.0000000000044338, 113.5502958579838122 ) ) ;
#25914 = EDGE_LOOP ( 'NONE', ( #54426, #46786 ) ) ;
#25915 = ORIENTED_EDGE ( 'NONE', *, *, #54213, .F. ) ;
#25916 = CARTESIAN_POINT ( 'NONE',  ( -173.1211646369891355, 88.63826465341151106, 3.977144016177345254 ) ) ;
#25917 = LINE ( 'NONE', #18644, #51583 ) ;
#25918 = LINE ( 'NONE', #53306, #62997 ) ;
#25920 = ORIENTED_EDGE ( 'NONE', *, *, #4208, .T. ) ;
#25919 = CARTESIAN_POINT ( 'NONE',  ( -149.0732005398558044, 63.81212100765654327, -34.82227269216089383 ) ) ;
#25921 = DIRECTION ( 'NONE',  ( -0.000000000000000000, 1.000000000000000000, -0.000000000000000000 ) ) ;
#25922 = CARTESIAN_POINT ( 'NONE',  ( -52.13778968636736977, -39.42540649522066332, 3.125053320693577513E-16 ) ) ;
#25923 = ORIENTED_EDGE ( 'NONE', *, *, #50193, .T. ) ;
#25924 = FACE_OUTER_BOUND ( 'NONE', #63101, .T. ) ;
#25925 = EDGE_CURVE ( 'NONE', #32583, #28859, #69565, .T. ) ;
#25926 = CARTESIAN_POINT ( 'NONE',  ( -126.3495878770406478, 48.00153794568856824, -61.75825448869760947 ) ) ;
#25927 = CARTESIAN_POINT ( 'NONE',  ( -24.75616454008739709, -3.483147608717210630, 0.000000000000000000 ) ) ;
#25928 = CARTESIAN_POINT ( 'NONE',  ( -130.2071229607962266, 50.62285182196874445, 17.42881725291558936 ) ) ;
#25929 = CARTESIAN_POINT ( 'NONE',  ( -150.9154386825424865, 65.38313372076783025, -88.63248908416815652 ) ) ;
#25930 = EDGE_LOOP ( 'NONE', ( #58701, #62122 ) ) ;
#25931 = ORIENTED_EDGE ( 'NONE', *, *, #60345, .F. ) ;
#25932 = CARTESIAN_POINT ( 'NONE',  ( 188.5843222076478867, 86.53342480589840591, -70.27300197745584853 ) ) ;
#25933 = CARTESIAN_POINT ( 'NONE',  ( -165.6398193834832853, 79.16932278174807891, -42.82268507880024089 ) ) ;
#25934 = LINE ( 'NONE', #62172, #49710 ) ;
#25935 = CARTESIAN_POINT ( 'NONE',  ( 104.7227067006896561, 27.50728936118535728, -75.36740411498894332 ) ) ;
#25936 = AXIS2_PLACEMENT_3D ( 'NONE', #34116, #13356, #60833 ) ;
#25937 = CARTESIAN_POINT ( 'NONE',  ( -76.78104518372332166, 22.68568622761702258, 30.64349253551715080 ) ) ;
#25938 = CARTESIAN_POINT ( 'NONE',  ( -73.63128929564827274, 21.53548093502884697, -63.89603870393958829 ) ) ;
#25939 = CARTESIAN_POINT ( 'NONE',  ( -145.9095871962850310, 61.18682730038538864, 44.80555181577465618 ) ) ;
#25940 = CARTESIAN_POINT ( 'NONE',  ( -118.7011544766493643, 43.11604763363182968, 40.26125301860250261 ) ) ;
#25941 = CARTESIAN_POINT ( 'NONE',  ( -167.6386155194958292, 81.22597462185140671, -63.91328706315006514 ) ) ;
#25942 = PRODUCT_DEFINITION_SHAPE ( 'NONE', 'NONE',  #2684 ) ;
#25943 = ORIENTED_EDGE ( 'NONE', *, *, #22332, .F. ) ;
#25944 = CARTESIAN_POINT ( 'NONE',  ( -107.7893514267588273, 35.66840175773126731, -20.78274561057057568 ) ) ;
#25946 = ORIENTED_EDGE ( 'NONE', *, *, #1016, .F. ) ;
#25945 = B_SPLINE_CURVE_WITH_KNOTS ( 'NONE', 3,
 ( #14269, #56477, #68091, #8301, #19185, #35730, #24491, #45929, #40639, #46613, #35378, #8651, #30105, #51560, #8996, #30443, #51891, #3704, #25178, #19892, #41350, #43050, #20921, #59230, #64520, #63490, #26548, #53941, #53605, #15304, #5433, #26886, #68749, #9684, #11049, #16673, #38127, #5082, #48311, #53252, #32510, #144, #15645, #64169, #16330, #58536, #5764, #63835, #15983, #26200, #37096, #48659, #10355, #37785, #31149, #42374, #31821, #47980 ),
 .UNSPECIFIED., .F., .F.,
 ( 4, 2, 2, 2, 2, 2, 2, 2, 2, 2, 2, 2, 2, 2, 2, 2, 2, 2, 2, 2, 2, 2, 2, 2, 2, 2, 2, 2, 4 ),
 ( 0.000000000000000000, 0.002115217322790804468, 0.003172825984186181981, 0.004230434645581559495, 0.005288043306976936142, 0.006345651968372312789, 0.007403260629767689435, 0.008460869291163065214, 0.01057608661395382198, 0.01163369527534918041, 0.01269130393674454231, 0.01480652125953524009, 0.01692173858232593614, 0.01797934724372131712, 0.01903695590511669811, 0.02115217322790744967, 0.02220978188930281677, 0.02326739055069818735, 0.02538260787348892850, 0.02644021653488426091, 0.02749782519627959679, 0.02802662952697726820, 0.02855543385767493961, 0.02961304251907029977, 0.03014184684976798159, 0.03067065118046566341, 0.03172825984186106868, 0.03278586850325648089, 0.03384347716465187922 ),
 .UNSPECIFIED. ) ;
#25947 = AXIS2_PLACEMENT_3D ( 'NONE', #17145, #48799, #44229 ) ;
#25948 = CARTESIAN_POINT ( 'NONE',  ( -33.36721086971962080, 9.915747831546610769, 18.12394761578280367 ) ) ;
#25949 = SURFACE_STYLE_FILL_AREA ( #57266 ) ;
#25950 = FACE_OUTER_BOUND ( 'NONE', #68490, .T. ) ;
#25951 = CARTESIAN_POINT ( 'NONE',  ( -190.3061188229049208, 108.5745819235682035, -65.07512604326164762 ) ) ;
#25952 = CARTESIAN_POINT ( 'NONE',  ( 447.3372781065086201, 0.000000000000000000, -116.4497041420118393 ) ) ;
#25953 = LINE ( 'NONE', #52667, #3547 ) ;
#25954 = FACE_OUTER_BOUND ( 'NONE', #27294, .T. ) ;
#25955 = CARTESIAN_POINT ( 'NONE',  ( -95.63694837622350065, 30.64472169584719197, -65.86884539641842196 ) ) ;
#25956 = CARTESIAN_POINT ( 'NONE',  ( -37.39246151129642470, 11.66872370876246201, -11.38479204114821286 ) ) ;
#25957 = EDGE_CURVE ( 'NONE', #30445, #50693, #63586, .T. ) ;
#25958 = VERTEX_POINT ( 'NONE', #9813 ) ;
#25959 = CARTESIAN_POINT ( 'NONE',  ( -36.11269837220804391, 15.55634918610408945, 85.00100000000000477 ) ) ;
#25960 = ORIENTED_EDGE ( 'NONE', *, *, #1192, .T. ) ;
#25961 = CARTESIAN_POINT ( 'NONE',  ( 61.09977118998600787, 13.26754120022606642, 56.90226584646475061 ) ) ;
#25962 = CARTESIAN_POINT ( 'NONE',  ( 8.763528846667103522, 7.383598436776581231, -67.22465256489064700 ) ) ;
#25963 = CARTESIAN_POINT ( 'NONE',  ( 259.4165763529819060, 225.8585178651493948, 128.9999999999999716 ) ) ;
#25964 = CARTESIAN_POINT ( 'NONE',  ( 0.000000000000000000, 0.000000000000000000, 170.0000000000000000 ) ) ;
#25966 = ADVANCED_FACE ( 'NONE', ( #32302 ), #21385, .T. ) ;
#25965 = CARTESIAN_POINT ( 'NONE',  ( -10.23867141318106455, 7.059827648235817321, -76.88073892781783059 ) ) ;
#25967 = CARTESIAN_POINT ( 'NONE',  ( -95.04120270830169659, 29.25306318840326725, -13.64142617559394388 ) ) ;
#25968 = CARTESIAN_POINT ( 'NONE',  ( 150.0516754638056227, 53.34587188591233797, -44.75957873094871076 ) ) ;
#25969 = EDGE_CURVE ( 'NONE', #65764, #52913, #26292, .T. ) ;
#25970 = EDGE_LOOP ( 'NONE', ( #55663, #24678, #30062, #5035 ) ) ;
#25971 = EDGE_CURVE ( 'NONE', #9014, #22785, #68123, .T. ) ;
#25972 = CARTESIAN_POINT ( 'NONE',  ( 848.0071894358306963, 629.9915846175190381, 569.0068267248676648 ) ) ;
#25973 = FACE_OUTER_BOUND ( 'NONE', #53635, .T. ) ;
#25974 = CARTESIAN_POINT ( 'NONE',  ( 174.9099402067542997, 73.96774984027638311, -12.61427854525189929 ) ) ;
#25975 = PLANE ( 'NONE',  #3141 ) ;
#25976 = CARTESIAN_POINT ( 'NONE',  ( 169.9999999999999716, 3.680555555555560243, 0.000000000000000000 ) ) ;
#25977 = ORIENTED_EDGE ( 'NONE', *, *, #59630, .T. ) ;
#25978 = CARTESIAN_POINT ( 'NONE',  ( 39.77028211725739482, 51.87520073220942862, 41.38025477438755928 ) ) ;
#25979 = CARTESIAN_POINT ( 'NONE',  ( -1.083610669212420996, 6.545642299653492202, -12.75074224467104322 ) ) ;
#25980 = CARTESIAN_POINT ( 'NONE',  ( 200.8383807319521566, 102.8517715783673623, -23.42650824558267075 ) ) ;
#25981 = CARTESIAN_POINT ( 'NONE',  ( -156.3413281584584809, 70.19975255048969132, 94.99999999999866418 ) ) ;
#25982 = B_SPLINE_CURVE_WITH_KNOTS ( 'NONE', 3,
 ( #14573, #14235, #14907, #2639, #36375, #36029 ),
 .UNSPECIFIED., .F., .F.,
 ( 4, 2, 4 ),
 ( 1.095770181106998147E-06, 0.03239442681617711595, 0.06478775786217312593 ),
 .UNSPECIFIED. ) ;
#25983 = ADVANCED_FACE ( 'NONE', ( #51169 ), #2629, .F. ) ;
#25984 = CARTESIAN_POINT ( 'NONE',  ( 134.3172730033263349, 41.70277427218489663, 44.51034083899535432 ) ) ;
#25985 = EDGE_CURVE ( 'NONE', #60940, #58006, #29655, .T. ) ;
#25986 = ORIENTED_EDGE ( 'NONE', *, *, #46747, .F. ) ;
#25987 = DIRECTION ( 'NONE',  ( 0.000000000000000000, -1.000000000000000000, 0.000000000000000000 ) ) ;
#25988 = DIRECTION ( 'NONE',  ( 0.000000000000000000, -1.000000000000000000, 0.000000000000000000 ) ) ;
#25989 = EDGE_CURVE ( 'NONE', #41887, #51139, #8948, .T. ) ;
#25990 = CARTESIAN_POINT ( 'NONE',  ( 187.2296622856351860, 86.53808614709454616, 32.50155238689070814 ) ) ;
#25991 = CARTESIAN_POINT ( 'NONE',  ( 164.1352994389932576, 64.33767534192701021, 6.615417748415636012 ) ) ;
#25992 = CARTESIAN_POINT ( 'NONE',  ( 6.375108774214766072E-14, 36.11269837220805812, 0.000000000000000000 ) ) ;
#25993 = AXIS2_PLACEMENT_3D ( 'NONE', #13856, #55735, #56778 ) ;
#25994 = CIRCLE ( 'NONE', #64136, 5.000000000000004441 ) ;
#25995 = ORIENTED_EDGE ( 'NONE', *, *, #52728, .F. ) ;
#25996 = CARTESIAN_POINT ( 'NONE',  ( 41.72486082342750535, 50.31647622756258187, 6.377659838150125143E-18 ) ) ;
#25997 = CIRCLE ( 'NONE', #4637, 10.00000000000000000 ) ;
#25998 = ORIENTED_EDGE ( 'NONE', *, *, #56446, .F. ) ;
#25999 = LINE ( 'NONE', #21391, #26624 ) ;
#26000 = CARTESIAN_POINT ( 'NONE',  ( -27.00000000000000355, 26.99999999999999289, 12.00000000000000000 ) ) ;
#26001 = CARTESIAN_POINT ( 'NONE',  ( -57.42615654242915468, 15.33060010148603070, 44.93600813576141206 ) ) ;
#26003 = ORIENTED_EDGE ( 'NONE', *, *, #49305, .F. ) ;
#26002 = CARTESIAN_POINT ( 'NONE',  ( 197.6319840686292082, 98.73992647122672395, -95.00000000000133582 ) ) ;
#26004 = CARTESIAN_POINT ( 'NONE',  ( -180.2252811616041583, 95.40045830523430936, 40.74347283216714288 ) ) ;
#26005 = MECHANICAL_DESIGN_GEOMETRIC_PRESENTATION_REPRESENTATION (  '', ( #33887 ), #30515 ) ;
#26006 = DIRECTION ( 'NONE',  ( 0.000000000000000000, 0.000000000000000000, -1.000000000000000000 ) ) ;
#26007 = CARTESIAN_POINT ( 'NONE',  ( 116.0822834687217124, 32.80169113915573575, -38.68990360584331967 ) ) ;
#26008 = VERTEX_POINT ( 'NONE', #4694 ) ;
#26009 = LINE ( 'NONE', #42847, #40098 ) ;
#26010 = CARTESIAN_POINT ( 'NONE',  ( 0.000000000000000000, 3.000000000000030198, 0.000000000000000000 ) ) ;
#26011 = CARTESIAN_POINT ( 'NONE',  ( 136.1310312718401008, 42.81430973242785143, 71.01667174595678489 ) ) ;
#26012 = CARTESIAN_POINT ( 'NONE',  ( -125.8938041572051389, -170.0000000000000000, -69.25825448869763079 ) ) ;
#26013 = CARTESIAN_POINT ( 'NONE',  ( 133.8566784816069344, -170.0000000000000000, 63.85489142945905172 ) ) ;
#26014 = LINE ( 'NONE', #4214, #21501 ) ;
#26015 = ORIENTED_EDGE ( 'NONE', *, *, #33592, .F. ) ;
#26016 = CARTESIAN_POINT ( 'NONE',  ( 46.84154678921881043, 10.51341196666389344, 9.587434892585696034 ) ) ;
#26017 = ORIENTED_EDGE ( 'NONE', *, *, #28408, .T. ) ;
#26018 = CARTESIAN_POINT ( 'NONE',  ( 153.2523375521184619, 55.69936538551848315, -22.98567760057999365 ) ) ;
#26019 = CARTESIAN_POINT ( 'NONE',  ( 212.1978255065451151, 119.0880569674902745, -16.63249047809884473 ) ) ;
#26020 = CARTESIAN_POINT ( 'NONE',  ( -45.14452651541945727, 49.02628140145412772, 34.48241795236665297 ) ) ;
#26021 = CARTESIAN_POINT ( 'NONE',  ( -156.6692143066620986, 70.50016761530888232, -71.40156983480068220 ) ) ;
#26022 = CARTESIAN_POINT ( 'NONE',  ( -109.7844028549000370, 36.75929263860175666, 91.49416231544373090 ) ) ;
#26023 = CARTESIAN_POINT ( 'NONE',  ( 183.7875981612220073, 82.83906702837188618, 16.96311135807992798 ) ) ;
#26024 = CARTESIAN_POINT ( 'NONE',  ( 212.1535111375854399, 117.1635556319084657, -42.99501597635795491 ) ) ;
#26025 = FACE_BOUND ( 'NONE', #6271, .T. ) ;
#26026 = EDGE_LOOP ( 'NONE', ( #27056, #21125, #21992, #4159 ) ) ;
#26027 = FACE_OUTER_BOUND ( 'NONE', #64676, .T. ) ;
#26028 = ORIENTED_EDGE ( 'NONE', *, *, #59785, .F. ) ;
#26029 = CARTESIAN_POINT ( 'NONE',  ( -74.79539698934962644, 21.95498232236881719, 58.33441674758699236 ) ) ;
#26030 =( REPRESENTATION_RELATIONSHIP ('NONE','NONE', #40274, #35767 ) REPRESENTATION_RELATIONSHIP_WITH_TRANSFORMATION ( #50197 )SHAPE_REPRESENTATION_RELATIONSHIP( ) );
#26031 = CARTESIAN_POINT ( 'NONE',  ( -95.50384525802328994, 29.46973564057716288, -39.28996472385307470 ) ) ;
#26032 = CARTESIAN_POINT ( 'NONE',  ( 59.29615173875417611, 11.84060224810187911, -76.58255111298183238 ) ) ;
#26033 = LINE ( 'NONE', #57699, #23798 ) ;
#26034 = CARTESIAN_POINT ( 'NONE',  ( 409.0783954480987177, 190.0000000000000000, 174.7010307253932808 ) ) ;
#26035 = CARTESIAN_POINT ( 'NONE',  ( 16.77104078056616032, 7.540619757007628543, 44.96607726379911441 ) ) ;
#26036 = VECTOR ( 'NONE', #40164, 1000.000000000000000 ) ;
#26037 = DIRECTION ( 'NONE',  ( -0.000000000000000000, 1.000000000000000000, -0.000000000000000000 ) ) ;
#26038 = EDGE_LOOP ( 'NONE', ( #47584, #50216, #24524, #3079 ) ) ;
#26039 = VECTOR ( 'NONE', #52286, 1000.000000000000000 ) ;
#26040 = DIRECTION ( 'NONE',  ( -0.000000000000000000, -0.000000000000000000, -1.000000000000000000 ) ) ;
#26041 = CARTESIAN_POINT ( 'NONE',  ( -171.4814970982680791, 85.32124710276292490, 72.49661911005092918 ) ) ;
#26042 = ORIENTED_EDGE ( 'NONE', *, *, #15554, .F. ) ;
#26043 = ORIENTED_EDGE ( 'NONE', *, *, #51492, .T. ) ;
#26045 = ADVANCED_FACE ( 'NONE', ( #9286 ), #51850, .T. ) ;
#26044 = CARTESIAN_POINT ( 'NONE',  ( -30.94745021534356155, 10.53010394565407282, -62.16174795566551126 ) ) ;
#26046 = CARTESIAN_POINT ( 'NONE',  ( 21.98745393275189386, 71.71550996510525522, 43.58025477438756923 ) ) ;
#26048 = PLANE ( 'NONE',  #855 ) ;
#26047 = AXIS2_PLACEMENT_3D ( 'NONE', #24810, #68075, #13220 ) ;
#26049 = AXIS2_PLACEMENT_3D ( 'NONE', #20771, #32027, #65071 ) ;
#26050 = PLANE ( 'NONE',  #30567 ) ;
#26051 = CARTESIAN_POINT ( 'NONE',  ( -142.0062637385110236, 58.06920992247432167, 11.92674320627384255 ) ) ;
#26052 = EDGE_CURVE ( 'NONE', #33038, #66237, #47588, .T. ) ;
#26053 = VECTOR ( 'NONE', #47424, 1000.000000000000000 ) ;
#26054 = ORIENTED_EDGE ( 'NONE', *, *, #58344, .F. ) ;
#26055 = CARTESIAN_POINT ( 'NONE',  ( -133.3944793432480367, 52.87251459353622352, 38.37487159473982246 ) ) ;
#26056 = ORIENTED_EDGE ( 'NONE', *, *, #37626, .T. ) ;
#26057 = CARTESIAN_POINT ( 'NONE',  ( 209.6877167158270652, 113.4449353909247264, 15.46721332339767585 ) ) ;
#26058 = CARTESIAN_POINT ( 'NONE',  ( 184.5140223535449309, 83.60465277292396991, -90.70322354721781721 ) ) ;
#26059 = SURFACE_STYLE_USAGE ( .BOTH. , #41541 ) ;
#26060 = CARTESIAN_POINT ( 'NONE',  ( -5.183193881612060849, 7.740932022135019963, 71.48359962217394070 ) ) ;
#26061 = EDGE_CURVE ( 'NONE', #62951, #57182, #11904, .T. ) ;
#26062 = ORIENTED_EDGE ( 'NONE', *, *, #56326, .T. ) ;
#26063 = ORIENTED_EDGE ( 'NONE', *, *, #59692, .F. ) ;
#26064 = CARTESIAN_POINT ( 'NONE',  ( 114.8388622179743805, -21.96384902133207362, 1.301157935232943430 ) ) ;
#26065 = CARTESIAN_POINT ( 'NONE',  ( -119.1064753703575718, 43.36500113374746945, 94.99999999999866418 ) ) ;
#26066 = CARTESIAN_POINT ( 'NONE',  ( 36.08914434112045200, 9.014684630517857400, -63.23120754001776334 ) ) ;
#26067 = CARTESIAN_POINT ( 'NONE',  ( 26.99999999999999645, 26.99999999999999645, 12.00000000000000000 ) ) ;
#26068 = CARTESIAN_POINT ( 'NONE',  ( 70.38121440378668581, 14.50253793787158507, 38.79010627313403603 ) ) ;
#26069 = CARTESIAN_POINT ( 'NONE',  ( 16.12102920665804362, 7.518218183539778998, 83.70402026746120328 ) ) ;
#26070 = ORIENTED_EDGE ( 'NONE', *, *, #52935, .F. ) ;
#26071 = CARTESIAN_POINT ( 'NONE',  ( 3.673940397442059178E-15, 0.000000000000000000, 30.00000000000000000 ) ) ;
#26072 = CARTESIAN_POINT ( 'NONE',  ( 427.4999999999999432, 207.5000000000000284, 378.0000000000000000 ) ) ;
#26073 = VERTEX_POINT ( 'NONE', #47251 ) ;
#26074 = B_SPLINE_CURVE_WITH_KNOTS ( 'NONE', 3,
 ( #34437, #28084, #38648, #40041, #45667, #67145, #55516, #7693, #12615, #61500, #60089, #66099, #13317, #8028, #6636, #33729, #34774, #55878, #65741, #49527, #11910, #44621, #66794, #33387, #1713, #17893, #39348, #29481, #2756, #7344, #24219, #60451, #39007, #12267, #55162, #28438, #1362, #6985, #49890, #66449, #50248, #28800, #60791, #2070, #44964 ),
 .UNSPECIFIED., .F., .F.,
 ( 4, 2, 2, 2, 2, 2, 2, 2, 2, 2, 2, 1, 2, 2, 2, 2, 2, 2, 2, 2, 2, 2, 4 ),
 ( 0.000000000000000000, 0.001512548138464676417, 0.002268822207697016903, 0.003025096276929357172, 0.004537644415394002581, 0.005293918484626342416, 0.006050192553858681384, 0.007562740692323361054, 0.009075288830788039857, 0.01058783696925271953, 0.01134411103848505589, 0.01210038510771739399, 0.01285665917694972689, 0.01361293324618205978, 0.01512548138464670650, 0.01588175545387902204, 0.01663802952311134106, 0.01815057766157596175, 0.01966312580004058938, 0.02041939986927290493, 0.02117567393850521701, 0.02268822207696980994, 0.02420077021543439941 ),
 .UNSPECIFIED. ) ;
#26075 = CARTESIAN_POINT ( 'NONE',  ( -78.66644367742109978, 22.32174330031319442, 3.573650549209446137 ) ) ;
#26076 = ORIENTED_EDGE ( 'NONE', *, *, #44634, .F. ) ;
#26077 = VERTEX_POINT ( 'NONE', #40953 ) ;
#26078 = EDGE_LOOP ( 'NONE', ( #10229, #35989, #54763, #6051 ) ) ;
#26079 = CARTESIAN_POINT ( 'NONE',  ( -118.4709174626548531, 42.97515378817185194, 12.38156042881829677 ) ) ;
#26080 = CARTESIAN_POINT ( 'NONE',  ( -175.1920326508032986, 89.46239303019289935, 57.94521480769297739 ) ) ;
#26081 = CARTESIAN_POINT ( 'NONE',  ( 133.3996297101684831, 41.14871796345732946, 71.35489142945908725 ) ) ;
#26082 = AXIS2_PLACEMENT_3D ( 'NONE', #54517, #7044, #54163 ) ;
#26083 = EDGE_LOOP ( 'NONE', ( #575, #21551 ) ) ;
#26084 = CARTESIAN_POINT ( 'NONE',  ( -38.93122880031071276, 10.94177517338562389, 90.93378199072627410 ) ) ;
#26085 = CARTESIAN_POINT ( 'NONE',  ( -56.44201257846630426, 32.26641783793562723, 41.38025477438755928 ) ) ;
#26086 = FACE_OUTER_BOUND ( 'NONE', #62478, .T. ) ;
#26087 = CARTESIAN_POINT ( 'NONE',  ( 105.8022841538864185, 26.88074187880708621, -49.48557371029213670 ) ) ;
#26088 = CARTESIAN_POINT ( 'NONE',  ( -25.50312845906834980, 8.692070753302669317, 33.12567030776318688 ) ) ;
#26089 = CARTESIAN_POINT ( 'NONE',  ( -7.306921498789654024, -37.63116382989763764, 13.32819299319722894 ) ) ;
#26090 = VERTEX_POINT ( 'NONE', #19847 ) ;
#26091 = AXIS2_PLACEMENT_3D ( 'NONE', #25913, #52290, #4450 ) ;
#26092 = DIRECTION ( 'NONE',  ( 0.000000000000000000, 1.000000000000000000, 0.000000000000000000 ) ) ;
#26093 = CARTESIAN_POINT ( 'NONE',  ( -81.01931326044683601, 24.31309346877660715, -62.33462428330359728 ) ) ;
#26094 = CARTESIAN_POINT ( 'NONE',  ( 173.5844030397475706, 72.71952271766126330, 9.659088270331640302 ) ) ;
#26095 = CARTESIAN_POINT ( 'NONE',  ( 149.0250918491436778, 6.000000000000000000, -14.43565316649551811 ) ) ;
#26096 = EDGE_CURVE ( 'NONE', #21122, #21979, #37053, .T. ) ;
#26097 = CARTESIAN_POINT ( 'NONE',  ( -83.51110947562231956, 25.31252704029285283, 5.343194909942403648 ) ) ;
#26098 = CARTESIAN_POINT ( 'NONE',  ( 132.0582325211145189, 40.34869848118184166, 17.46102436708167360 ) ) ;
#26099 = CARTESIAN_POINT ( 'NONE',  ( -152.2964402771109178, 66.58174574061955298, 18.34200323450853531 ) ) ;
#26100 = CARTESIAN_POINT ( 'NONE',  ( 197.3671887352768408, 98.40825776222057186, 88.79584330558347460 ) ) ;
#26101 = CARTESIAN_POINT ( 'NONE',  ( 69.73342236697679652, 14.33173522011652601, 7.097129799427905006 ) ) ;
#26102 = CARTESIAN_POINT ( 'NONE',  ( -65.36598343705435354, 0.000000000000000000, 41.38025477438755928 ) ) ;
#26103 = LINE ( 'NONE', #58442, #63477 ) ;
#26105 = ORIENTED_EDGE ( 'NONE', *, *, #1246, .F. ) ;
#26104 = EDGE_CURVE ( 'NONE', #46943, #19302, #14565, .T. ) ;
#26106 = ITEM_DEFINED_TRANSFORMATION ( 'NONE', 'NONE', #11864,  #66832 ) ;
#26107 = CARTESIAN_POINT ( 'NONE',  ( -60.23623261180705413, 17.18081742568415038, 86.05829893146599829 ) ) ;
#26108 = ORIENTED_EDGE ( 'NONE', *, *, #27692, .T. ) ;
#26109 = DIRECTION ( 'NONE',  ( 0.000000000000000000, 0.000000000000000000, 1.000000000000000000 ) ) ;
#26110 = EDGE_LOOP ( 'NONE', ( #32584, #25697 ) ) ;
#26111 = CARTESIAN_POINT ( 'NONE',  ( 22.15926701483429895, 7.796117250416235933, -65.89848683517405448 ) ) ;
#26112 = CARTESIAN_POINT ( 'NONE',  ( -168.1811549361197251, 83.25427431521137578, 32.67343048873900102 ) ) ;
#26113 = DIRECTION ( 'NONE',  ( -4.258099457802062126E-18, 2.810746842852082347E-18, -1.000000000000000000 ) ) ;
#26114 = CARTESIAN_POINT ( 'NONE',  ( 134.3135005523732559, 42.87884033955815966, -51.01290741596099565 ) ) ;
#26115 = DIRECTION ( 'NONE',  ( -1.000000000000000000, -1.001918046209079887E-14, 9.729495617646301779E-15 ) ) ;
#26116 = CARTESIAN_POINT ( 'NONE',  ( -1.666933348992582609, 64.97862212458815634, 170.0000000000000000 ) ) ;
#26117 = DIRECTION ( 'NONE',  ( 0.3930250316539278255, -0.9195277725514487965, 0.000000000000000000 ) ) ;
#26118 = CARTESIAN_POINT ( 'NONE',  ( 8.000000000000000000, 4.618802153516997855, -9.500000000000000000 ) ) ;
#26119 = ORIENTED_EDGE ( 'NONE', *, *, #52323, .F. ) ;
#26120 = ADVANCED_FACE ( 'NONE', ( #52199 ), #24782, .F. ) ;
#26121 = VERTEX_POINT ( 'NONE', #26157 ) ;
#26122 = EDGE_CURVE ( 'NONE', #18870, #51157, #20874, .T. ) ;
#26123 = CARTESIAN_POINT ( 'NONE',  ( 174.8710133519038550, 73.93068202503360453, 94.71388927649152834 ) ) ;
#26124 = FACE_OUTER_BOUND ( 'NONE', #23115, .T. ) ;
#26125 = CARTESIAN_POINT ( 'NONE',  ( 130.2230634515710790, 40.43733067189506869, -90.64009857926562574 ) ) ;
#26126 = PRODUCT_DEFINITION_CONTEXT ( 'detailed design', #23376, 'design' ) ;
#26127 = VECTOR ( 'NONE', #10915, 1000.000000000000000 ) ;
#26128 = EDGE_CURVE ( 'NONE', #43797, #26875, #19490, .T. ) ;
#26129 = DIRECTION ( 'NONE',  ( 0.9578262852211514300, 0.000000000000000000, 0.2873478855663451625 ) ) ;
#26130 = CARTESIAN_POINT ( 'NONE',  ( -36.11269837220801548, 31.11269837220812207, 2.000000000000000000 ) ) ;
#26131 = CARTESIAN_POINT ( 'NONE',  ( 181.9411407973024950, 80.91291802046383452, -9.380507075415929208 ) ) ;
#26132 = CARTESIAN_POINT ( 'NONE',  ( 174.6176230994777825, 72.30829341023250834, -66.73030761740862715 ) ) ;
#26133 = CIRCLE ( 'NONE', #65448, 74.95140232871122521 ) ;
#26134 = CARTESIAN_POINT ( 'NONE',  ( 0.3173508448886623312, -8.480771745766416458, -1.310872448937996593 ) ) ;
#26135 = CARTESIAN_POINT ( 'NONE',  ( 93.71772995179816235, 21.96265635001559602, -14.01375245968642957 ) ) ;
#26136 = DIRECTION ( 'NONE',  ( 0.000000000000000000, 0.000000000000000000, 1.000000000000000000 ) ) ;
#26137 = LINE ( 'NONE', #47571, #2599 ) ;
#26138 = CARTESIAN_POINT ( 'NONE',  ( 163.2911130186311084, 63.63047778106599139, 68.49022856848731067 ) ) ;
#26139 = VECTOR ( 'NONE', #18432, 1000.000000000000000 ) ;
#26140 = B_SPLINE_CURVE_WITH_KNOTS ( 'NONE', 3,
 ( #38913, #11815, #1614, #65644, #57080, #8892 ),
 .UNSPECIFIED., .F., .F.,
 ( 4, 2, 4 ),
 ( 0.03218945466321617571, 0.06469840457090975105, 0.09720735447860334721 ),
 .UNSPECIFIED. ) ;
#26141 = EDGE_CURVE ( 'NONE', #45146, #51895, #60214, .T. ) ;
#26142 = ORIENTED_EDGE ( 'NONE', *, *, #1113, .T. ) ;
#26143 = CARTESIAN_POINT ( 'NONE',  ( -124.9927180788553613, 45.90286323198617424, -34.95429498894391429 ) ) ;
#26144 = FACE_OUTER_BOUND ( 'NONE', #50341, .T. ) ;
#26145 = LINE ( 'NONE', #47577, #21747 ) ;
#26146 = DIRECTION ( 'NONE',  ( 1.000000000000000000, 0.000000000000000000, 0.000000000000000000 ) ) ;
#26147 = CARTESIAN_POINT ( 'NONE',  ( 149.9552318077303994, 52.03645901322386891, 10.08806978535764109 ) ) ;
#26148 = EDGE_CURVE ( 'NONE', #11547, #62136, #5391, .T. ) ;
#26149 = EDGE_CURVE ( 'NONE', #30965, #61262, #22603, .T. ) ;
#26150 = CARTESIAN_POINT ( 'NONE',  ( -13.12090985667452969, 8.303654651054307223, 85.96412694177334402 ) ) ;
#26151 = ORIENTED_EDGE ( 'NONE', *, *, #17053, .F. ) ;
#26152 = CARTESIAN_POINT ( 'NONE',  ( 0.08285530295198713369, 1.570896314769989255, 7.999999999999998224 ) ) ;
#26153 = CARTESIAN_POINT ( 'NONE',  ( 0.000000000000000000, 0.000000000000000000, 5.000000000000000000 ) ) ;
#26154 = VERTEX_POINT ( 'NONE', #16287 ) ;
#26155 = ORIENTED_EDGE ( 'NONE', *, *, #16888, .T. ) ;
#26156 = CARTESIAN_POINT ( 'NONE',  ( 46.58804170569938918, 10.47239957174000047, 88.93053816599565664 ) ) ;
#26157 = CARTESIAN_POINT ( 'NONE',  ( -173.1211646369891355, 88.63826465341151106, -88.40105834567734178 ) ) ;
#26158 = DIRECTION ( 'NONE',  ( -0.8118923937861950435, -0.5838071093367415143, 0.000000000000000000 ) ) ;
#26159 = EDGE_LOOP ( 'NONE', ( #52272, #69149, #41528, #37177 ) ) ;
#26160 = DIRECTION ( 'NONE',  ( -0.000000000000000000, -0.000000000000000000, -1.000000000000000000 ) ) ;
#26161 = CARTESIAN_POINT ( 'NONE',  ( 24.34427655538957680, -5.688250960945929080, 0.000000000000000000 ) ) ;
#26162 = CARTESIAN_POINT ( 'NONE',  ( -0.5783162822156601157, 7.534184941292926929, 12.71782406034808588 ) ) ;
#26163 = CARTESIAN_POINT ( 'NONE',  ( 158.3636111008086402, 59.62671916656141491, 44.40946747225338243 ) ) ;
#26164 = CARTESIAN_POINT ( 'NONE',  ( -154.6085044440278580, 69.98390342970668598, -74.66063903122440593 ) ) ;
#26165 = DIRECTION ( 'NONE',  ( -0.000000000000000000, 0.000000000000000000, -1.000000000000000000 ) ) ;
#26166 = VERTEX_POINT ( 'NONE', #16627 ) ;
#26167 = CARTESIAN_POINT ( 'NONE',  ( 0.000000000000000000, 0.000000000000000000, 41.38025477438755928 ) ) ;
#26168 = AXIS2_PLACEMENT_3D ( 'NONE', #35653, #57105, #55184 ) ;
#26169 = FACE_OUTER_BOUND ( 'NONE', #12650, .T. ) ;
#26170 = CARTESIAN_POINT ( 'NONE',  ( 12.46490660984525078, 7.423426948220647859, 44.24267865148938483 ) ) ;
#26171 = FACE_OUTER_BOUND ( 'NONE', #21818, .T. ) ;
#26172 = CARTESIAN_POINT ( 'NONE',  ( -86.09946351606596693, 26.38487962042298207, 90.55497946160751610 ) ) ;
#26174 = ORIENTED_EDGE ( 'NONE', *, *, #1352, .T. ) ;
#26173 = DIRECTION ( 'NONE',  ( 0.000000000000000000, 0.000000000000000000, 1.000000000000000000 ) ) ;
#26175 = EDGE_LOOP ( 'NONE', ( #60541, #35415, #59872, #54035 ) ) ;
#26176 = MECHANICAL_DESIGN_GEOMETRIC_PRESENTATION_REPRESENTATION (  '', ( #58740 ), #28427 ) ;
#26177 = EDGE_LOOP ( 'NONE', ( #50058, #37190 ) ) ;
#26178 = VECTOR ( 'NONE', #23778, 1000.000000000000000 ) ;
#26179 = CARTESIAN_POINT ( 'NONE',  ( 116.8917656767876565, 33.20682060519245482, -66.78745051061426352 ) ) ;
#26180 = FACE_OUTER_BOUND ( 'NONE', #63459, .T. ) ;
#26181 = ADVANCED_FACE ( 'NONE', ( #54244 ), #44503, .T. ) ;
#26182 = CARTESIAN_POINT ( 'NONE',  ( 198.7084915431529737, 98.47675983942191635, -75.19271672455441546 ) ) ;
#26183 = CARTESIAN_POINT ( 'NONE',  ( -33.36965723649377935, 10.93726715887724232, 57.30962576113447682 ) ) ;
#26184 = AXIS2_PLACEMENT_3D ( 'NONE', #54403, #54757, #22414 ) ;
#26185 = CARTESIAN_POINT ( 'NONE',  ( -10.92576759990585167, 8.121994053275074066, -9.239980494406424327 ) ) ;
#26186 = CARTESIAN_POINT ( 'NONE',  ( 150.2809931605061990, 52.27058242113233888, -72.62185156043770462 ) ) ;
#26187 = DIRECTION ( 'NONE',  ( -0.000000000000000000, -0.000000000000000000, -1.000000000000000000 ) ) ;
#26188 = EDGE_CURVE ( 'NONE', #8527, #68125, #53559, .T. ) ;
#26189 = VECTOR ( 'NONE', #63343, 1000.000000000000000 ) ;
#26190 = CARTESIAN_POINT ( 'NONE',  ( -149.5074843970971301, 64.17983161892345834, -49.81283053149198992 ) ) ;
#26191 = EDGE_LOOP ( 'NONE', ( #31822, #43272, #20732, #25085 ) ) ;
#26192 = ORIENTED_EDGE ( 'NONE', *, *, #28005, .F. ) ;
#26193 = CARTESIAN_POINT ( 'NONE',  ( 70.11969827741707206, 15.47408882293423638, -13.92140172406558030 ) ) ;
#26194 = DIRECTION ( 'NONE',  ( 0.000000000000000000, 1.000000000000000000, 0.000000000000000000 ) ) ;
#26195 = CIRCLE ( 'NONE', #46421, 243.4957430088094839 ) ;
#26196 = CARTESIAN_POINT ( 'NONE',  ( 103.6419690634046589, 25.94571131443040102, 94.42721007842214931 ) ) ;
#26197 = CARTESIAN_POINT ( 'NONE',  ( -153.1031717208032319, 68.63449618039567213, 4.790432509985504517 ) ) ;
#26198 = CARTESIAN_POINT ( 'NONE',  ( -29.70166638324966968, 57.83280658984257627, 170.0000000000000000 ) ) ;
#26199 = CARTESIAN_POINT ( 'NONE',  ( 19.53470118933705990, 6.649487981843464013, 31.01283177266423152 ) ) ;
#26200 = CARTESIAN_POINT ( 'NONE',  ( -157.0038757045938667, 72.17867991799593597, 91.61780177421432825 ) ) ;
#26201 = EDGE_LOOP ( 'NONE', ( #16513, #59322 ) ) ;
#26202 = EDGE_CURVE ( 'NONE', #2304, #30365, #452, .T. ) ;
#26203 = ORIENTED_EDGE ( 'NONE', *, *, #44624, .T. ) ;
#26204 = ORIENTED_EDGE ( 'NONE', *, *, #4439, .F. ) ;
#26205 = EDGE_CURVE ( 'NONE', #46223, #15646, #47936, .T. ) ;
#26206 = CARTESIAN_POINT ( 'NONE',  ( 38.90907126433564400, 9.359889524363177671, -35.61981746542775795 ) ) ;
#26207 = CARTESIAN_POINT ( 'NONE',  ( 110.2429982417149432, 28.88204397445230853, -89.61153874658103291 ) ) ;
#26208 = EDGE_CURVE ( 'NONE', #45426, #16958, #26845, .T. ) ;
#26209 = CARTESIAN_POINT ( 'NONE',  ( 111.9975424824652634, 295.8720703627916464, 535.5371946177799600 ) ) ;
#26210 = CARTESIAN_POINT ( 'NONE',  ( 203.1423857108908066, 105.9238244286949850, 56.20468668297329629 ) ) ;
#26211 = ORIENTED_EDGE ( 'NONE', *, *, #34000, .T. ) ;
#26212 = CARTESIAN_POINT ( 'NONE',  ( 32.67604581760325999, 7.629767527669977234, 67.58595727477110415 ) ) ;
#26213 = CARTESIAN_POINT ( 'NONE',  ( 9.057575839850580124, 6.378493414438676012, -12.85657236994559582 ) ) ;
#26214 =( NAMED_UNIT ( * ) PLANE_ANGLE_UNIT ( ) SI_UNIT ( $, .RADIAN. ) );
#26215 = CARTESIAN_POINT ( 'NONE',  ( 19.75315861330098244, 7.667327050329334703, 4.299178115857797522 ) ) ;
#26216 = CARTESIAN_POINT ( 'NONE',  ( 188.2076037774874351, 86.11782719225436722, 61.28972546789033515 ) ) ;
#26217 = DIRECTION ( 'NONE',  ( 1.000000000000000000, 1.387778780781445922E-16, 0.000000000000000000 ) ) ;
#26218 = CARTESIAN_POINT ( 'NONE',  ( -85.75222301046099460, 25.14826148333819233, -40.10669955425598943 ) ) ;
#26219 = CARTESIAN_POINT ( 'NONE',  ( 23.03864809957654103, 6.841061756139153793, 66.29383730662293317 ) ) ;
#26220 = CARTESIAN_POINT ( 'NONE',  ( -422.6627218934913230, 399.9999999999997726, 113.5502958579881891 ) ) ;
#26221 = CARTESIAN_POINT ( 'NONE',  ( 110.2429982417149574, 29.99119854320843714, 17.76666361527367499 ) ) ;
#26222 = CIRCLE ( 'NONE', #9354, 10.00000000000000000 ) ;
#26223 = ORIENTED_EDGE ( 'NONE', *, *, #43178, .F. ) ;
#26225 = CARTESIAN_POINT ( 'NONE',  ( 187.5272808203428099, 85.37192123373904451, 6.087187552396759571 ) ) ;
#26224 = COLOUR_RGB ( '',0.7921568627450980005, 0.8196078431372548767, 0.9333333333333333481 ) ;
#26226 = SHAPE_DEFINITION_REPRESENTATION ( #30409, #46431 ) ;
#26227 = CARTESIAN_POINT ( 'NONE',  ( 0.000000000000000000, 0.000000000000000000, 40.00000000000003553 ) ) ;
#26228 = CARTESIAN_POINT ( 'NONE',  ( -31.93169728792081941, 10.69234447276976674, -35.31719736520182806 ) ) ;
#26229 = EDGE_CURVE ( 'NONE', #24394, #9160, #27179, .T. ) ;
#26230 = CARTESIAN_POINT ( 'NONE',  ( -105.8879245385188312, 35.79035667534148502, -35.92177053218349414 ) ) ;
#26231 = EDGE_CURVE ( 'NONE', #47253, #20436, #21226, .T. ) ;
#26232 = CYLINDRICAL_SURFACE ( 'NONE', #50132, 2.999999999999999112 ) ;
#26233 = ORIENTED_EDGE ( 'NONE', *, *, #48709, .F. ) ;
#26234 = VECTOR ( 'NONE', #51646, 1000.000000000000000 ) ;
#26235 = ORIENTED_EDGE ( 'NONE', *, *, #38259, .T. ) ;
#26236 = EDGE_CURVE ( 'NONE', #22374, #16361, #21556, .T. ) ;
#26237 = AXIS2_PLACEMENT_3D ( 'NONE', #53077, #41860, #4564 ) ;
#26238 = CARTESIAN_POINT ( 'NONE',  ( -25.98312968277007684, 8.759224980175270403, -21.12456965610049053 ) ) ;
#26239 = VECTOR ( 'NONE', #24432, 1000.000000000000000 ) ;
#26240 = CARTESIAN_POINT ( 'NONE',  ( 174.0302671031634247, 71.75925975512330979, 87.94198868075041275 ) ) ;
#26241 = ORIENTED_EDGE ( 'NONE', *, *, #42162, .T. ) ;
#26242 = CIRCLE ( 'NONE', #59909, 8.000000000000000000 ) ;
#26243 = B_SPLINE_CURVE_WITH_KNOTS ( 'NONE', 3,
 ( #48291, #53922, #38106, #49692, #55326, #54630, #65196, #16649, #27906, #16991, #48992, #59550, #11719, #12084, #38460, #832, #6457, #37762, #16309, #11367, #59207, #44429, #32834, #6091, #33192, #17345, #49342, #11027, #32491, #5745, #479, #7150, #1522, #33551, #27200, #1175, #54265, #21927, #22630, #27550, #44069, #48635, #64849, #122, #60614 ),
 .UNSPECIFIED., .F., .F.,
 ( 4, 2, 2, 2, 2, 2, 2, 2, 1, 2, 2, 2, 2, 2, 2, 2, 2, 2, 2, 2, 2, 2, 4 ),
 ( 0.000000000000000000, 0.001467747071934226953, 0.002201620607901337394, 0.002935494143868447835, 0.004403241215802664379, 0.005870988287736880057, 0.007338735359671097469, 0.008072608895638206175, 0.008806482431605313146, 0.009540355967572421853, 0.01027422950353953056, 0.01174197657547374797, 0.01247585011144085147, 0.01320972364740795497, 0.01467747071934215851, 0.01541134425530925681, 0.01614521779127635684, 0.01761296486321056037, 0.01908071193514476738, 0.01981458547111187435, 0.02054845900707898479, 0.02201620607901318832, 0.02348395315094739533 ),
 .UNSPECIFIED. ) ;
#26244 = CARTESIAN_POINT ( 'NONE',  ( 150.5165549438847563, 53.68267614960137024, 93.43292638355033830 ) ) ;
#26245 = ORIENTED_EDGE ( 'NONE', *, *, #51938, .T. ) ;
#26246 = CARTESIAN_POINT ( 'NONE',  ( 447.3372781065085633, 400.0000000000000568, -116.4497041420118393 ) ) ;
#26247 = PLANE ( 'NONE',  #37354 ) ;
#26248 = CARTESIAN_POINT ( 'NONE',  ( -95.54114085644955878, 30.59949910443587839, 94.99999999999866418 ) ) ;
#26249 = VECTOR ( 'NONE', #54300, 1000.000000000000000 ) ;
#26250 = CARTESIAN_POINT ( 'NONE',  ( -99.31850058233800382, 31.30166762705811223, 44.91357497810577115 ) ) ;
#26251 = DIRECTION ( 'NONE',  ( 1.387778780781445922E-16, -1.000000000000000000, -1.232595164407830946E-32 ) ) ;
#26253 = ORIENTED_EDGE ( 'NONE', *, *, #63510, .F. ) ;
#26252 = LINE ( 'NONE', #37483, #4983 ) ;
#26254 = DIRECTION ( 'NONE',  ( 0.3090169943749447312, 0.9510565162951544194, -0.000000000000000000 ) ) ;
#26255 = VERTEX_POINT ( 'NONE', #43001 ) ;
#26256 = ORIENTED_EDGE ( 'NONE', *, *, #3499, .F. ) ;
#26257 = CARTESIAN_POINT ( 'NONE',  ( -48.00000000000000711, -20.00000000000000355, 4.000000000000000000 ) ) ;
#26258 = CARTESIAN_POINT ( 'NONE',  ( -59.09450113343241640, 27.07101652673493319, 170.0000000000000000 ) ) ;
#26259 = CARTESIAN_POINT ( 'NONE',  ( -178.2381786520593323, 93.01028335822120141, -9.878879645691533540 ) ) ;
#26260 = CYLINDRICAL_SURFACE ( 'NONE', #57872, 10.00000000000000178 ) ;
#26262 = VERTEX_POINT ( 'NONE', #65173 ) ;
#26261 = CARTESIAN_POINT ( 'NONE',  ( -149.5074843970971017, 64.17983161892347255, -34.81283053149196149 ) ) ;
#26263 = CARTESIAN_POINT ( 'NONE',  ( -109.7868734384453973, 37.91103670584237051, 91.81079717178241140 ) ) ;
#26264 = VERTEX_POINT ( 'NONE', #11005 ) ;
#26265 = CARTESIAN_POINT ( 'NONE',  ( -55.54058841405667835, 14.81234591756537533, -8.371773407996172978 ) ) ;
#26266 = CARTESIAN_POINT ( 'NONE',  ( -132.4896623150434607, 52.22616402022729432, -65.67901329176390846 ) ) ;
#26267 = EDGE_CURVE ( 'NONE', #937, #19006, #37989, .T. ) ;
#26269 = CARTESIAN_POINT ( 'NONE',  ( 56.74421265833558436, 32.44697398030905333, 6.377659838150106654E-18 ) ) ;
#26268 = VECTOR ( 'NONE', #1870, 1000.000000000000000 ) ;
#26270 = CARTESIAN_POINT ( 'NONE',  ( -94.77925136849377452, 29.13093715379787696, 11.40637257627832213 ) ) ;
#26271 = CARTESIAN_POINT ( 'NONE',  ( -417.6627218934913230, 399.9999999999997726, 113.5502958579881891 ) ) ;
#26272 = VERTEX_POINT ( 'NONE', #1152 ) ;
#26273 = ORIENTED_EDGE ( 'NONE', *, *, #19805, .F. ) ;
#26274 = CIRCLE ( 'NONE', #27413, 65.36598343705435354 ) ;
#26275 = CARTESIAN_POINT ( 'NONE',  ( 183.1865184929770862, 80.75677158533825661, -77.77206949057716656 ) ) ;
#26276 = DIRECTION ( 'NONE',  ( -1.000000000000000000, 0.000000000000000000, 0.000000000000000000 ) ) ;
#26277 = DIRECTION ( 'NONE',  ( 0.000000000000000000, -1.000000000000000000, 0.000000000000000000 ) ) ;
#26278 = VECTOR ( 'NONE', #59499, 1000.000000000000000 ) ;
#26279 = CARTESIAN_POINT ( 'NONE',  ( -86.05211524933166345, -170.0000000000000000, -95.00000000000133582 ) ) ;
#26280 = DIRECTION ( 'NONE',  ( -0.9749279121818259508, 0.2225209339563041788, 0.000000000000000000 ) ) ;
#26281 = CARTESIAN_POINT ( 'NONE',  ( 85.67138972405899722, 19.09593469918315023, 29.75815417200340818 ) ) ;
#26282 = CARTESIAN_POINT ( 'NONE',  ( 211.7634543339367781, 116.5654349622355141, -95.00000000000133582 ) ) ;
#26283 = VECTOR ( 'NONE', #6909, 1000.000000000000000 ) ;
#26284 = CARTESIAN_POINT ( 'NONE',  ( 42.03719354205839664, 9.783015072457470040, -36.09375209584154476 ) ) ;
#26285 = CARTESIAN_POINT ( 'NONE',  ( 212.1700216741373879, 117.1889356120871071, 62.82458332484058872 ) ) ;
#26286 = EDGE_CURVE ( 'NONE', #21328, #23006, #53899, .T. ) ;
#26287 = ORIENTED_EDGE ( 'NONE', *, *, #60185, .F. ) ;
#26289 = DIRECTION ( 'NONE',  ( 0.000000000000000000, 0.000000000000000000, 1.000000000000000000 ) ) ;
#26288 = AXIS2_PLACEMENT_3D ( 'NONE', #49577, #6, #48520 ) ;
#26290 = ORIENTED_EDGE ( 'NONE', *, *, #25029, .T. ) ;
#26291 = CARTESIAN_POINT ( 'NONE',  ( -15.08468253268400439, 7.472949889606721463, -44.86592640746919614 ) ) ;
#26292 = B_SPLINE_CURVE_WITH_KNOTS ( 'NONE', 3,
 ( #6860, #41820, #63622, #31272, #52699, #4526, #15432, #47420, #58324, #10142, #53043, #40262, #67355, #24095, #67015, #8609, #45187, #19146, #33952, #13868, #35334, #23742, #66665, #7910, #24445, #1952, #40601, #45534, #7576, #34303, #34990, #17771, #55385, #50123, #18808, #1583, #34658, #39228, #7214, #29030, #50471, #39913, #2292, #55748, #13194, #62053, #45886, #61709, #13535, #18465 ),
 .UNSPECIFIED., .F., .F.,
 ( 4, 2, 2, 2, 2, 2, 2, 2, 2, 2, 2, 2, 2, 2, 2, 2, 2, 2, 2, 2, 2, 2, 2, 2, 4 ),
 ( 0.02688458561150008225, 0.02770990876165290925, 0.02853523191180573973, 0.03018587821211140762, 0.03183652451241707898, 0.03266184766256991640, 0.03348717081272276075, 0.03513781711302837313, 0.03678846341333399245, 0.03761378656348677435, 0.03843910971363955625, 0.03926443286379233816, 0.04008975601394512006, 0.04174040231425066305, 0.04256572546440344496, 0.04339104861455622686, 0.04421637176470900876, 0.04504169491486179067, 0.04586701806501457257, 0.04669234121516735447, 0.04834298751547297379, 0.04916831066562575570, 0.04999363381577853066, 0.05164428011608408753, 0.05329492641638965134 ),
 .UNSPECIFIED. ) ;
#26293 = VECTOR ( 'NONE', #17590, 1000.000000000000000 ) ;
#26294 = FACE_OUTER_BOUND ( 'NONE', #58559, .T. ) ;
#26295 = EDGE_CURVE ( 'NONE', #37698, #18334, #32814, .T. ) ;
#26296 = CARTESIAN_POINT ( 'NONE',  ( 92.20490818459941806, 22.47175429302963678, 69.09674679565556232 ) ) ;
#26297 = CARTESIAN_POINT ( 'NONE',  ( 157.0336341255055856, 57.31169401067818825, -24.27963370867398751 ) ) ;
#26298 = DIRECTION ( 'NONE',  ( -1.110223024625155594E-14, 0.000000000000000000, -1.000000000000000000 ) ) ;
#26299 = EDGE_CURVE ( 'NONE', #14641, #41303, #24283, .T. ) ;
#26300 = CARTESIAN_POINT ( 'NONE',  ( 0.000000000000000000, 0.000000000000000000, 2.000000000000001776 ) ) ;
#26301 = CARTESIAN_POINT ( 'NONE',  ( 35.65775178405255019, 7.951994368745591402, -76.46754290437888812 ) ) ;
#26302 = CARTESIAN_POINT ( 'NONE',  ( 0.000000000000000000, 0.000000000000000000, 40.00000000000003553 ) ) ;
#26303 = AXIS2_PLACEMENT_3D ( 'NONE', #48245, #16254, #26816 ) ;
#26304 = CARTESIAN_POINT ( 'NONE',  ( -33.85171821065140563, 11.02091558840054653, -8.854690906676584206 ) ) ;
#26305 = ORIENTED_EDGE ( 'NONE', *, *, #69066, .T. ) ;
#26306 = LINE ( 'NONE', #40742, #52191 ) ;
#26307 = ORIENTED_EDGE ( 'NONE', *, *, #52408, .F. ) ;
#26308 = CARTESIAN_POINT ( 'NONE',  ( 0.000000000000000000, 0.000000000000000000, 43.58025477438756212 ) ) ;
#26309 =( NAMED_UNIT ( * ) PLANE_ANGLE_UNIT ( ) SI_UNIT ( $, .RADIAN. ) );
#26310 = CARTESIAN_POINT ( 'NONE',  ( -189.2739965869453442, 107.1373753350176514, 10.69858136700815621 ) ) ;
#26311 = CARTESIAN_POINT ( 'NONE',  ( -2.116120943112233643, 74.98056102853672655, 133.5802547743875550 ) ) ;
#26312 = CARTESIAN_POINT ( 'NONE',  ( -0.3249717932738299675, 6.518578686837485314, 38.10374936827246728 ) ) ;
#26313 = LINE ( 'NONE', #47743, #36723 ) ;
#26314 = CARTESIAN_POINT ( 'NONE',  ( 154.0281735872262061, 56.28213428456461287, -36.95677541368942087 ) ) ;
#26315 = ORIENTED_EDGE ( 'NONE', *, *, #62074, .F. ) ;
#26316 = DIRECTION ( 'NONE',  ( -0.9798635308855324633, -0.1996683771670854646, 9.099544109286944284E-15 ) ) ;
#26317 = LINE ( 'NONE', #59347, #34079 ) ;
#26318 = CARTESIAN_POINT ( 'NONE',  ( 175.0634607207818760, 74.11351956991630630, -12.40074815326527791 ) ) ;
#26319 = LINE ( 'NONE', #58312, #9859 ) ;
#26320 = DIRECTION ( 'NONE',  ( -0.000000000000000000, -0.000000000000000000, -1.000000000000000000 ) ) ;
#26321 = VERTEX_POINT ( 'NONE', #26501 ) ;
#26322 = DIRECTION ( 'NONE',  ( 0.000000000000000000, 0.000000000000000000, -1.000000000000000000 ) ) ;
#26323 = CARTESIAN_POINT ( 'NONE',  ( -4.081377963939787357, 6.676029627840612157, -22.57677576480380921 ) ) ;
#26324 = EDGE_CURVE ( 'NONE', #15602, #68802, #807, .T. ) ;
#26325 = CARTESIAN_POINT ( 'NONE',  ( 197.6341357773624168, 98.74251867088339907, -14.44262121195315096 ) ) ;
#26326 = CARTESIAN_POINT ( 'NONE',  ( -142.0521142816473059, 58.10507551552675665, 91.07448709527056963 ) ) ;
#26327 = AXIS2_PLACEMENT_3D ( 'NONE', #3005, #24115, #45553 ) ;
#26328 = DIRECTION ( 'NONE',  ( 0.000000000000000000, 0.000000000000000000, -1.000000000000000000 ) ) ;
#26329 = ORIENTED_EDGE ( 'NONE', *, *, #24708, .F. ) ;
#26330 = LINE ( 'NONE', #10140, #43516 ) ;
#26331 = CYLINDRICAL_SURFACE ( 'NONE', #28330, 7.500000000000013323 ) ;
#26332 = CARTESIAN_POINT ( 'NONE',  ( 160.9097745014958036, 61.67033591969549633, 16.73367501025392912 ) ) ;
#26333 = DIRECTION ( 'NONE',  ( 0.000000000000000000, -1.000000000000000000, 0.000000000000000000 ) ) ;
#26334 = CONICAL_SURFACE ( 'NONE', #57761, 65.00000000000000000, 0.7853981633974497223 ) ;
#26335 = VERTEX_POINT ( 'NONE', #59878 ) ;
#26336 = VECTOR ( 'NONE', #40479, 1000.000000000000000 ) ;
#26337 = CARTESIAN_POINT ( 'NONE',  ( 173.7263186949343776, 72.85225335320951956, 62.17071978413066091 ) ) ;
#26338 = CIRCLE ( 'NONE', #56613, 65.00000000000000000 ) ;
#26339 = VERTEX_POINT ( 'NONE', #65527 ) ;
#26340 = CARTESIAN_POINT ( 'NONE',  ( -109.7793173546316723, 36.75648380851384900, -42.23093992832588839 ) ) ;
#26341 = CARTESIAN_POINT ( 'NONE',  ( 65.62848231372478836, 13.29388722724788430, -77.09954622703783400 ) ) ;
#26342 = AXIS2_PLACEMENT_3D ( 'NONE', #7582, #8260, #40267 ) ;
#26343 = CARTESIAN_POINT ( 'NONE',  ( -55.05276343752909440, 14.68156374112637863, 45.31732777293115788 ) ) ;
#26345 = EDGE_LOOP ( 'NONE', ( #52381, #61044 ) ) ;
#26344 = DIRECTION ( 'NONE',  ( -1.000000000000000000, -1.387778780781445922E-16, 0.000000000000000000 ) ) ;
#26346 = CARTESIAN_POINT ( 'NONE',  ( -173.9656771507954716, 88.06879734510549440, 45.82169460664104577 ) ) ;
#26347 = PLANE ( 'NONE',  #15945 ) ;
#26348 = CARTESIAN_POINT ( 'NONE',  ( 117.0069443446175512, 33.26475960880694061, -40.17220626710923170 ) ) ;
#26349 = ORIENTED_EDGE ( 'NONE', *, *, #3344, .F. ) ;
#26350 = CARTESIAN_POINT ( 'NONE',  ( -84.49322488516129681, 0.000000000000000000, 43.58025477438756212 ) ) ;
#26351 = EDGE_CURVE ( 'NONE', #6937, #910, #17323, .T. ) ;
#26352 = ADVANCED_FACE ( 'NONE', ( #15942 ), #13450, .T. ) ;
#26353 = CARTESIAN_POINT ( 'NONE',  ( 140.2332932573541484, 45.41010019581509027, 67.83493447615286698 ) ) ;
#26354 = EDGE_CURVE ( 'NONE', #8516, #25726, #45450, .T. ) ;
#26355 = CARTESIAN_POINT ( 'NONE',  ( -168.7150276173047700, 82.35404041280327192, 44.40934749284262750 ) ) ;
#26356 = CARTESIAN_POINT ( 'NONE',  ( 131.6115093721024891, 41.25402743071398959, 56.69510300717567475 ) ) ;
#26357 = CARTESIAN_POINT ( 'NONE',  ( 26.99999999999999289, 29.99999999999999645, 0.000000000000000000 ) ) ;
#26358 = ORIENTED_EDGE ( 'NONE', *, *, #43892, .T. ) ;
#26359 = CARTESIAN_POINT ( 'NONE',  ( 45.89232972083999584, 10.36128169546909561, 6.802839851248819514 ) ) ;
#26360 = ORIENTED_EDGE ( 'NONE', *, *, #58904, .F. ) ;
#26361 = ORIENTED_EDGE ( 'NONE', *, *, #21212, .F. ) ;
#26362 = CARTESIAN_POINT ( 'NONE',  ( -102.2801239173131052, 33.91021738430208643, -88.70367844590326456 ) ) ;
#26363 = CARTESIAN_POINT ( 'NONE',  ( -62.43534356913686878, 16.78604954659376247, 92.86776280466541778 ) ) ;
#26364 = CARTESIAN_POINT ( 'NONE',  ( -39.40355428794429571, 43.02169521020481824, 27.58472315868180402 ) ) ;
#26365 = CYLINDRICAL_SURFACE ( 'NONE', #10837, 7.500000000000013323 ) ;
#26366 = CARTESIAN_POINT ( 'NONE',  ( -109.0191069781766657, 36.33811634972921922, 94.99999999999866418 ) ) ;
#26367 = CARTESIAN_POINT ( 'NONE',  ( 185.5457097283155008, 84.70846743303870596, 16.01068182946670149 ) ) ;
#26368 = CYLINDRICAL_SURFACE ( 'NONE', #11406, 5.000000000000004441 ) ;
#26369 = PLANE ( 'NONE',  #35485 ) ;
#26370 = ORIENTED_EDGE ( 'NONE', *, *, #1043, .F. ) ;
#26371 = VECTOR ( 'NONE', #10768, 999.9999999999998863 ) ;
#26372 = CARTESIAN_POINT ( 'NONE',  ( 0.000000000000000000, 0.000000000000000000, 43.58025477438756212 ) ) ;
#26373 = VERTEX_POINT ( 'NONE', #24359 ) ;
#26374 = CARTESIAN_POINT ( 'NONE',  ( -76.32456871438915869, 22.51591205926310479, 57.62160030318823090 ) ) ;
#26375 = ADVANCED_FACE ( 'NONE', ( #66584 ), #18724, .F. ) ;
#26376 = CARTESIAN_POINT ( 'NONE',  ( -95.61819996182572368, 29.52346081122276900, -39.06019279122138244 ) ) ;
#26377 = B_SPLINE_CURVE_WITH_KNOTS ( 'NONE', 3,
 ( #53657, #10406, #30848, #47345, #37144, #52294, #20282, #4114, #37486, #25579, #57920, #68803, #9737, #20618, #10073, #47686, #31199, #52631, #53304, #4453, #16033, #15695, #15356, #36814, #48032, #31532, #58256, #64220, #26596, #4791, #69150, #20974, #58588, #31876, #69493, #58936, #54343, #54701, #49768, #33962, #32906, #65628, #60686, #12504, #5481, #55052 ),
 .UNSPECIFIED., .F., .F.,
 ( 4, 2, 2, 2, 2, 2, 2, 2, 2, 2, 2, 2, 2, 2, 2, 2, 2, 2, 2, 2, 2, 2, 4 ),
 ( 0.02584318557310392658, 0.02743529570732763587, 0.02823135077443949398, 0.02902740584155135556, 0.03061951597577504403, 0.03221162610999873943, 0.03380373624422242790, 0.03459979131133428948, 0.03539584637844615800, 0.03619190144555801958, 0.03698795651266988116, 0.03858006664689359738, 0.03937612171400545896, 0.04017217678111731360, 0.04096823184822917518, 0.04176428691534103677, 0.04335639704956475993, 0.04494850718378848309, 0.04654061731801220625, 0.04813272745223592941, 0.04892878251934780487, 0.04972483758645968033, 0.05131694772068347982 ),
 .UNSPECIFIED. ) ;
#26378 = CARTESIAN_POINT ( 'NONE',  ( 59.08638499266955080, 11.79550614876701786, -76.45822759883306219 ) ) ;
#26379 = EDGE_CURVE ( 'NONE', #19049, #53174, #33529, .T. ) ;
#26380 = PLANE ( 'NONE',  #24383 ) ;
#26381 = CARTESIAN_POINT ( 'NONE',  ( 17.73567516211396722, 7.577454475141605528, 30.25539365111569978 ) ) ;
#26382 = CARTESIAN_POINT ( 'NONE',  ( 160.9097745014957752, 61.67033591969547501, -63.79997676113709559 ) ) ;
#26383 = VECTOR ( 'NONE', #39548, 1000.000000000000000 ) ;
#26384 = ORIENTED_EDGE ( 'NONE', *, *, #54356, .T. ) ;
#26385 = CARTESIAN_POINT ( 'NONE',  ( -73.10694748374054086, 20.28107308417881427, 59.70508575492568326 ) ) ;
#26386 = CARTESIAN_POINT ( 'NONE',  ( -172.3018509397888636, 86.22053936367350957, 72.63294570045411547 ) ) ;
#26387 = ORIENTED_EDGE ( 'NONE', *, *, #28912, .T. ) ;
#26388 = CIRCLE ( 'NONE', #7261, 65.00000000000000000 ) ;
#26389 = ORIENTED_EDGE ( 'NONE', *, *, #43751, .T. ) ;
#26390 = VECTOR ( 'NONE', #35245, 1000.000000000000000 ) ;
#26391 = CARTESIAN_POINT ( 'NONE',  ( -31.43908319763711390, 10.61114334766715928, 18.37190381572551701 ) ) ;
#26392 = DIRECTION ( 'NONE',  ( -0.000000000000000000, -0.000000000000000000, -1.000000000000000000 ) ) ;
#26393 = FACE_OUTER_BOUND ( 'NONE', #15842, .T. ) ;
#26394 = CARTESIAN_POINT ( 'NONE',  ( -29.49715813532712971, -42.41725772201189670, 26.66469104408689361 ) ) ;
#26395 = VECTOR ( 'NONE', #69234, 1000.000000000000000 ) ;
#26396 = DIRECTION ( 'NONE',  ( 0.000000000000000000, 0.000000000000000000, -1.000000000000000000 ) ) ;
#26397 = ORIENTED_EDGE ( 'NONE', *, *, #58421, .T. ) ;
#26398 = EDGE_LOOP ( 'NONE', ( #1482, #37700, #51981, #34010 ) ) ;
#26399 = DIRECTION ( 'NONE',  ( 0.000000000000000000, 0.000000000000000000, -1.000000000000000000 ) ) ;
#26400 = VERTEX_POINT ( 'NONE', #67281 ) ;
#26401 = LINE ( 'NONE', #43241, #3175 ) ;
#26402 = CARTESIAN_POINT ( 'NONE',  ( 0.000000000000000000, 1.502314598737159031E-15, -8.000000000000000000 ) ) ;
#26403 = DIRECTION ( 'NONE',  ( -1.000000000000000000, 0.000000000000000000, -1.734723475976805517E-15 ) ) ;
#26404 = DIRECTION ( 'NONE',  ( 0.000000000000000000, 0.000000000000000000, 1.000000000000000000 ) ) ;
#26405 = CARTESIAN_POINT ( 'NONE',  ( -40.13282190614798850, -1.847197903505587038E-12, -5.000000000000000000 ) ) ;
#26406 = CARTESIAN_POINT ( 'NONE',  ( -78.66644367742111399, -170.0000000000000000, -8.270900041254199309 ) ) ;
#26407 = ORIENTED_EDGE ( 'NONE', *, *, #26758, .T. ) ;
#26408 = EDGE_LOOP ( 'NONE', ( #53608, #14949, #45531, #52922 ) ) ;
#26409 = CARTESIAN_POINT ( 'NONE',  ( 157.4703587214989113, 57.65129005721575339, -24.27963370867398396 ) ) ;
#26410 = CARTESIAN_POINT ( 'NONE',  ( -4.613603609465545041, 74.86839895266042788, 73.58025477438755502 ) ) ;
#26411 = CARTESIAN_POINT ( 'NONE',  ( -166.2028193222418793, 79.74385139484274987, -18.27775044557155582 ) ) ;
#26412 = DIRECTION ( 'NONE',  ( -0.7227948638273978821, 0.6910626489868580968, 0.000000000000000000 ) ) ;
#26413 = DIRECTION ( 'NONE',  ( 0.000000000000000000, 0.7071067811865475727, 0.7071067811865475727 ) ) ;
#26414 = CARTESIAN_POINT ( 'NONE',  ( 0.000000000000000000, 190.0000000000000000, 0.000000000000000000 ) ) ;
#26415 = ORIENTED_EDGE ( 'NONE', *, *, #19611, .T. ) ;
#26416 = FACE_OUTER_BOUND ( 'NONE', #3044, .T. ) ;
#26417 = DIRECTION ( 'NONE',  ( 1.000000000000000000, 0.000000000000000000, 0.000000000000000000 ) ) ;
#26418 = ORIENTED_EDGE ( 'NONE', *, *, #53401, .F. ) ;
#26419 = FACE_BOUND ( 'NONE', #53781, .T. ) ;
#26420 = VERTEX_POINT ( 'NONE', #50036 ) ;
#26421 = VECTOR ( 'NONE', #7137, 999.9999999999998863 ) ;
#26422 = AXIS2_PLACEMENT_3D ( 'NONE', #30265, #66183, #45744 ) ;
#26423 = ORIENTED_EDGE ( 'NONE', *, *, #50443, .T. ) ;
#26424 = CARTESIAN_POINT ( 'NONE',  ( 9.416603677636258496, 6.380307115728825806, -46.98271897290301524 ) ) ;
#26425 = CARTESIAN_POINT ( 'NONE',  ( -179.2262621278718200, 94.19039042964669761, 69.55156446434544648 ) ) ;
#26426 = EDGE_CURVE ( 'NONE', #32477, #68560, #44735, .T. ) ;
#26427 = CARTESIAN_POINT ( 'NONE',  ( 127.6144785300460711, 37.78099129859916872, 59.68968456894913288 ) ) ;
#26428 = CIRCLE ( 'NONE', #10694, 10.00000000000000000 ) ;
#26429 = AXIS2_PLACEMENT_3D ( 'NONE', #63942, #42141, #63605 ) ;
#26430 = ORIENTED_EDGE ( 'NONE', *, *, #54938, .F. ) ;
#26431 = VECTOR ( 'NONE', #14575, 1000.000000000000000 ) ;
#26432 = EDGE_CURVE ( 'NONE', #9968, #53834, #55658, .T. ) ;
#26433 =( NAMED_UNIT ( * ) SI_UNIT ( $, .STERADIAN. ) SOLID_ANGLE_UNIT ( ) );
#26434 = DIRECTION ( 'NONE',  ( -0.000000000000000000, -1.000000000000000000, -0.000000000000000000 ) ) ;
#26435 = AXIS2_PLACEMENT_3D ( 'NONE', #52223, #20215, #57166 ) ;
#26436 = EDGE_CURVE ( 'NONE', #30631, #46713, #28941, .T. ) ;
#26437 = DIRECTION ( 'NONE',  ( -0.000000000000000000, -0.000000000000000000, -1.000000000000000000 ) ) ;
#26438 = CARTESIAN_POINT ( 'NONE',  ( 103.0026233023292832, 25.67408295205787994, -45.44575129055834850 ) ) ;
#26439 = CARTESIAN_POINT ( 'NONE',  ( -24.70354720400823823, 8.582324684301861240, 41.05222872378217147 ) ) ;
#26440 = CARTESIAN_POINT ( 'NONE',  ( 99.71998884745383407, 188.0000000000000000, 0.000000000000000000 ) ) ;
#26441 = ORIENTED_EDGE ( 'NONE', *, *, #7821, .T. ) ;
#26442 = ADVANCED_FACE ( 'NONE', ( #33863 ), #7829, .T. ) ;
#26443 = DIRECTION ( 'NONE',  ( -0.000000000000000000, -1.000000000000000000, -0.000000000000000000 ) ) ;
#26444 = CARTESIAN_POINT ( 'NONE',  ( -2.644994884459114459, 7.710515798486365036, -9.417753204360289843 ) ) ;
#26445 = CARTESIAN_POINT ( 'NONE',  ( -15.55634918610400597, 15.55634918610405748, 2.000000000000001776 ) ) ;
#26446 = CARTESIAN_POINT ( 'NONE',  ( -125.8938041572051105, 47.69968343338781835, -34.91370389823391918 ) ) ;
#26447 = LINE ( 'NONE', #47884, #15324 ) ;
#26448 = CARTESIAN_POINT ( 'NONE',  ( 133.6288034103010318, 41.28708886999551453, 2.665790248531665352 ) ) ;
#26449 = CARTESIAN_POINT ( 'NONE',  ( -154.7998111145352311, 68.80117179139330119, 6.040483385297001462 ) ) ;
#26450 = CARTESIAN_POINT ( 'NONE',  ( -118.6302575928420140, 43.07263081214307476, -67.37114707264666436 ) ) ;
#26451 = CARTESIAN_POINT ( 'NONE',  ( -125.8938041572051389, -170.0000000000000000, 64.96449846362078517 ) ) ;
#26452 = CARTESIAN_POINT ( 'NONE',  ( -78.66644367742111399, 23.39876645725286863, 72.26275173013684139 ) ) ;
#26453 = CARTESIAN_POINT ( 'NONE',  ( 44.33335936148068868, 10.11981604950586622, -91.15432397735798986 ) ) ;
#26454 = ORIENTED_EDGE ( 'NONE', *, *, #52390, .F. ) ;
#26455 = CARTESIAN_POINT ( 'NONE',  ( 8.000000000000007105, 249.8719672152120381, -95.00000000000133582 ) ) ;
#26456 = ORIENTED_EDGE ( 'NONE', *, *, #41862, .T. ) ;
#26457 = DIRECTION ( 'NONE',  ( -0.000000000000000000, -1.000000000000000000, -0.000000000000000000 ) ) ;
#26458 = EDGE_LOOP ( 'NONE', ( #42578, #31480, #34661, #36762 ) ) ;
#26459 = EDGE_CURVE ( 'NONE', #35148, #30648, #6080, .T. ) ;
#26460 = CARTESIAN_POINT ( 'NONE',  ( 22.51849650178394668, 7.817407610814550267, -66.54469324731199720 ) ) ;
#26461 = DIRECTION ( 'NONE',  ( -0.000000000000000000, -0.000000000000000000, -1.000000000000000000 ) ) ;
#26462 = DIRECTION ( 'NONE',  ( -0.000000000000000000, 1.000000000000000000, -0.000000000000000000 ) ) ;
#26463 = CARTESIAN_POINT ( 'NONE',  ( 69.73342236697681074, 14.33173522011652423, -19.74742079103577552 ) ) ;
#26464 = CARTESIAN_POINT ( 'NONE',  ( 25.39413431650373099, 1.224646799147353256E-15, -9.999999999999998224 ) ) ;
#26465 = CARTESIAN_POINT ( 'NONE',  ( -50.14523569787234436, 14.45648954445650780, -75.25403677891537768 ) ) ;
#26466 = DIRECTION ( 'NONE',  ( -0.000000000000000000, 1.000000000000000000, -0.000000000000000000 ) ) ;
#26467 = CARTESIAN_POINT ( 'NONE',  ( -25.03927907554148291, -61.76276460681540925, 34.48241823986843713 ) ) ;
#26468 = ORIENTED_EDGE ( 'NONE', *, *, #8595, .T. ) ;
#26469 = ORIENTED_EDGE ( 'NONE', *, *, #53883, .T. ) ;
#26470 = CARTESIAN_POINT ( 'NONE',  ( 66.30567821786758032, 13.45988234822861251, -36.47644505420841909 ) ) ;
#26471 = VECTOR ( 'NONE', #27986, 1000.000000000000000 ) ;
#26472 = CARTESIAN_POINT ( 'NONE',  ( 181.5278511219383688, 80.49241794770389902, 83.00548516787387143 ) ) ;
#26473 = CARTESIAN_POINT ( 'NONE',  ( -169.8972248494843029, 85.08697738648014308, -8.580859100646367921 ) ) ;
#26474 = AXIS2_PLACEMENT_3D ( 'NONE', #54106, #21771, #27392 ) ;
#26475 = CARTESIAN_POINT ( 'NONE',  ( 65.02425260195224155, 14.18239149161751733, -89.67225535254971192 ) ) ;
#26476 = CARTESIAN_POINT ( 'NONE',  ( 25.39413431650373099, 1.224646799147353059E-15, 5.000000000000000000 ) ) ;
#26477 = VECTOR ( 'NONE', #60734, 1000.000000000000000 ) ;
#26478 = VECTOR ( 'NONE', #19395, 1000.000000000000000 ) ;
#26479 = CARTESIAN_POINT ( 'NONE',  ( -15.31363169557738679, 7.494880774892001440, 63.97268137111493047 ) ) ;
#26480 = CARTESIAN_POINT ( 'NONE',  ( 204.6977192012829505, 108.0580384837234931, 2.363170148305746565 ) ) ;
#26481 =( NAMED_UNIT ( * ) PLANE_ANGLE_UNIT ( ) SI_UNIT ( $, .RADIAN. ) );
#26482 = CARTESIAN_POINT ( 'NONE',  ( -85.97236666747350853, 26.33140062794030811, -94.54850636960576082 ) ) ;
#26483 = CARTESIAN_POINT ( 'NONE',  ( 42.71504753277075395, 8.863481902720387495, -9.542259995937373063 ) ) ;
#26484 = CARTESIAN_POINT ( 'NONE',  ( 429.8372781065087906, 388.0000000000066507, -128.9497041420121093 ) ) ;
#26485 = DIRECTION ( 'NONE',  ( 0.7071067811865473507, 0.000000000000000000, -0.7071067811865477948 ) ) ;
#26486 = CARTESIAN_POINT ( 'NONE',  ( -419.7337897053570828, 394.9999999999957367, 80.62136366985768632 ) ) ;
#26487 = EDGE_LOOP ( 'NONE', ( #18280, #549, #49916, #22838 ) ) ;
#26488 = FACE_OUTER_BOUND ( 'NONE', #30619, .T. ) ;
#26489 = CYLINDRICAL_SURFACE ( 'NONE', #23775, 65.36598343705435354 ) ;
#26490 = DIRECTION ( 'NONE',  ( 0.000000000000000000, 1.000000000000000000, 0.000000000000000000 ) ) ;
#26491 = CARTESIAN_POINT ( 'NONE',  ( -60.41792053122248518, -24.01035990323518021, 170.0000000000000000 ) ) ;
#26492 = CARTESIAN_POINT ( 'NONE',  ( 150.0889146124742979, 52.13243511955544562, 8.708654298008204009 ) ) ;
#26493 = CARTESIAN_POINT ( 'NONE',  ( -13.95225484952729822, 8.378029245909427658, 86.96665100290213957 ) ) ;
#26494 = EDGE_CURVE ( 'NONE', #33732, #4217, #46834, .T. ) ;
#26495 = ORIENTED_EDGE ( 'NONE', *, *, #4036, .T. ) ;
#26496 = CARTESIAN_POINT ( 'NONE',  ( -44.39004539972346208, 1.224646799147353059E-15, -5.000000000000000000 ) ) ;
#26497 = CARTESIAN_POINT ( 'NONE',  ( -56.92000000000000171, -36.09918303830819752, 0.000000000000000000 ) ) ;
#26498 = ORIENTED_EDGE ( 'NONE', *, *, #19047, .T. ) ;
#26499 = VERTEX_POINT ( 'NONE', #8870 ) ;
#26500 = CARTESIAN_POINT ( 'NONE',  ( 37.78224319576848700, 9.218056077237706702, 83.77244032528042794 ) ) ;
#26501 = CARTESIAN_POINT ( 'NONE',  ( 70.60157554497457966, 25.16207943727196295, 41.38025477438755928 ) ) ;
#26502 = DIRECTION ( 'NONE',  ( 0.000000000000000000, 0.000000000000000000, 1.000000000000000000 ) ) ;
#26503 = VERTEX_POINT ( 'NONE', #35598 ) ;
#26504 = CARTESIAN_POINT ( 'NONE',  ( -60.97011009284707939, 16.34812508431679134, -64.92641111431414913 ) ) ;
#26505 = CARTESIAN_POINT ( 'NONE',  ( -7.825402957745085430, 6.891034867348157178, 18.27103044898354511 ) ) ;
#26506 = CARTESIAN_POINT ( 'NONE',  ( 35.65775178405256440, 7.951994368745586961, -22.77844172345153595 ) ) ;
#26507 = CARTESIAN_POINT ( 'NONE',  ( 175.5429257635130966, 74.57009623370761631, -38.64485354243735316 ) ) ;
#26508 = CARTESIAN_POINT ( 'NONE',  ( -4.000000000000013323, 6.928203230275504332, -9.500000000000000000 ) ) ;
#26509 = CARTESIAN_POINT ( 'NONE',  ( 86.62931800182293784, 19.42108912189597092, 29.71208757247930521 ) ) ;
#26510 = PRODUCT ( 'angular contact ball bearing_68_iso_ISO 15 ABB - 1740 - 38,SI,NC,38_68', 'angular contact ball bearing_68_iso_ISO 15 ABB - 1740 - 38,SI,NC,38_68', '', ( #36097 ) ) ;
#26511 = VERTEX_POINT ( 'NONE', #57392 ) ;
#26512 = EDGE_CURVE ( 'NONE', #16392, #29739, #41904, .T. ) ;
#26513 = VECTOR ( 'NONE', #67553, 1000.000000000000000 ) ;
#26514 = DIRECTION ( 'NONE',  ( 0.000000000000000000, 0.000000000000000000, 1.000000000000000000 ) ) ;
#26515 = DIRECTION ( 'NONE',  ( 1.000000000000000000, 0.000000000000000000, 0.000000000000000000 ) ) ;
#26516 = CARTESIAN_POINT ( 'NONE',  ( 203.9228889538744625, 106.9879579748727991, 29.23739942787593193 ) ) ;
#26517 = CARTESIAN_POINT ( 'NONE',  ( 79.43147385343415579, 17.08938890961555046, 88.76640830538551086 ) ) ;
#26518 = AXIS2_PLACEMENT_3D ( 'NONE', #66455, #67482, #35466 ) ;
#26520 = VERTEX_POINT ( 'NONE', #14815 ) ;
#26519 = CARTESIAN_POINT ( 'NONE',  ( 112.3013380801407379, 395.0000000000010800, 101.0502958579874644 ) ) ;
#26521 = EDGE_LOOP ( 'NONE', ( #54947, #46379 ) ) ;
#26522 = ADVANCED_FACE ( 'NONE', ( #40868 ), #25050, .T. ) ;
#26523 = VECTOR ( 'NONE', #62744, 1000.000000000000000 ) ;
#26524 = VECTOR ( 'NONE', #42241, 1000.000000000000000 ) ;
#26525 = ORIENTED_EDGE ( 'NONE', *, *, #9687, .T. ) ;
#26526 = CARTESIAN_POINT ( 'NONE',  ( -188.8754233303960746, 108.3048424661242137, 94.99999999999866418 ) ) ;
#26527 = LINE ( 'NONE', #16993, #32262 ) ;
#26528 = DIRECTION ( 'NONE',  ( -1.000000000000000000, 0.000000000000000000, 0.000000000000000000 ) ) ;
#26529 = AXIS2_PLACEMENT_3D ( 'NONE', #23474, #7977, #56501 ) ;
#26531 = CARTESIAN_POINT ( 'NONE',  ( -34.06637338149494809, 11.05895377318623218, 57.53204137510643790 ) ) ;
#26530 = AXIS2_PLACEMENT_3D ( 'NONE', #6451, #16986, #44783 ) ;
#26532 = PLANE ( 'NONE',  #64647 ) ;
#26533 = CARTESIAN_POINT ( 'NONE',  ( 156.5977259323288990, 56.97512126940428345, -77.93088349121646274 ) ) ;
#26534 = CARTESIAN_POINT ( 'NONE',  ( 0.7145311798163198613, -4.618802153516998743, 7.999999999999998224 ) ) ;
#26535 = CIRCLE ( 'NONE', #42303, 20.30000000000000071 ) ;
#26536 = CARTESIAN_POINT ( 'NONE',  ( -156.9910258076866114, 70.79617246506499839, -42.88647977470814965 ) ) ;
#26537 = ORIENTED_EDGE ( 'NONE', *, *, #58850, .T. ) ;
#26538 = VERTEX_POINT ( 'NONE', #36286 ) ;
#26539 = EDGE_CURVE ( 'NONE', #67789, #64323, #57742, .T. ) ;
#26540 = CARTESIAN_POINT ( 'NONE',  ( 69.36287815987334682, 15.27486453472191563, -20.37900260559285215 ) ) ;
#26541 = CARTESIAN_POINT ( 'NONE',  ( -80.56139928459658961, 24.13290941644246601, -35.35486284265729040 ) ) ;
#26542 = CARTESIAN_POINT ( 'NONE',  ( 157.4703587214989113, 57.65129005721576050, 71.25401806271709404 ) ) ;
#26544 = ADVANCED_FACE ( 'NONE', ( #62322 ), #50018, .T. ) ;
#26543 = CARTESIAN_POINT ( 'NONE',  ( -154.7826623253030505, 70.14150242829518334, 6.039344387218765320 ) ) ;
#26545 = ADVANCED_FACE ( 'NONE', ( #67960 ), #25742, .T. ) ;
#26546 = CARTESIAN_POINT ( 'NONE',  ( 188.0141161196705752, 85.90515114331880397, -40.84309500477795751 ) ) ;
#26547 = DIRECTION ( 'NONE',  ( 1.000000000000000000, 0.000000000000000000, 0.000000000000000000 ) ) ;
#26548 = CARTESIAN_POINT ( 'NONE',  ( -150.1466931226166537, 66.04887306281342774, 84.43241108380165372 ) ) ;
#26549 = EDGE_LOOP ( 'NONE', ( #13148, #43088 ) ) ;
#26550 = ORIENTED_EDGE ( 'NONE', *, *, #58407, .F. ) ;
#26551 = ORIENTED_EDGE ( 'NONE', *, *, #3730, .T. ) ;
#26552 = CARTESIAN_POINT ( 'NONE',  ( -155.7457403566965581, 71.01814553754121562, -19.66200801844618695 ) ) ;
#26553 = CARTESIAN_POINT ( 'NONE',  ( 32.09610685027467980, 8.582590950734839907, -44.83291474007333477 ) ) ;
#26554 = CARTESIAN_POINT ( 'NONE',  ( -35.99019277275120032, 10.38248800679342132, 70.54226521342960154 ) ) ;
#26555 = CARTESIAN_POINT ( 'NONE',  ( -152.5067928559255108, 66.76529500553620267, -22.35681670066612270 ) ) ;
#26556 = ORIENTED_EDGE ( 'NONE', *, *, #21450, .T. ) ;
#26557 = CARTESIAN_POINT ( 'NONE',  ( 36.09137906183517686, 8.001963043161767430, 57.52411210887189696 ) ) ;
#26558 = CARTESIAN_POINT ( 'NONE',  ( 410.0000000000000000, 190.0000000000000000, 175.2157797990580832 ) ) ;
#26559 = CARTESIAN_POINT ( 'NONE',  ( -7.330587818645180498, 7.867004275019547244, -35.41807073194381417 ) ) ;
#26560 = CARTESIAN_POINT ( 'NONE',  ( 0.000000000000000000, 0.000000000000000000, 0.000000000000000000 ) ) ;
#26561 = CARTESIAN_POINT ( 'NONE',  ( 0.000000000000000000, 0.000000000000000000, 0.000000000000000000 ) ) ;
#26562 = CARTESIAN_POINT ( 'NONE',  ( -81.00507684688697907, 23.22613445438386037, -35.48540021743968254 ) ) ;
#26563 = DIRECTION ( 'NONE',  ( 1.000000000000000000, 0.000000000000000000, 0.000000000000000000 ) ) ;
#26564 = LINE ( 'NONE', #69113, #7409 ) ;
#26565 = CARTESIAN_POINT ( 'NONE',  ( 13.37708032728285978, 7.441924986912761497, 3.564073605040367632 ) ) ;
#26566 = CIRCLE ( 'NONE', #34474, 299.9999999999999432 ) ;
#26567 = ORIENTED_EDGE ( 'NONE', *, *, #4964, .T. ) ;
#26568 = VECTOR ( 'NONE', #29247, 1000.000000000000000 ) ;
#26569 = CYLINDRICAL_SURFACE ( 'NONE', #18151, 65.36598343705435354 ) ;
#26570 = CARTESIAN_POINT ( 'NONE',  ( 178.1999009735082495, 75.73911533785330619, 43.73541319493209301 ) ) ;
#26571 = CARTESIAN_POINT ( 'NONE',  ( -132.2352756077771687, 50.81350938245627447, -46.42641520675586264 ) ) ;
#26572 = CARTESIAN_POINT ( 'NONE',  ( -105.4487797565983982, 35.55724615608639283, -49.32840306322937352 ) ) ;
#26573 = FACE_OUTER_BOUND ( 'NONE', #36664, .T. ) ;
#26574 = ORIENTED_EDGE ( 'NONE', *, *, #46200, .F. ) ;
#26575 = EDGE_CURVE ( 'NONE', #42734, #19578, #47171, .T. ) ;
#26576 = VECTOR ( 'NONE', #59651, 1000.000000000000000 ) ;
#26577 = ORIENTED_EDGE ( 'NONE', *, *, #9927, .T. ) ;
#26578 = CARTESIAN_POINT ( 'NONE',  ( -24.33435124463267485, 8.532637995283108623, -13.55733912248031992 ) ) ;
#26579 = CARTESIAN_POINT ( 'NONE',  ( 197.3119541548906852, 98.33923235143193153, 8.549100434825948724 ) ) ;
#26580 = ORIENTED_EDGE ( 'NONE', *, *, #627, .T. ) ;
#26581 = EDGE_CURVE ( 'NONE', #10664, #19486, #68632, .T. ) ;
#26582 = AXIS2_PLACEMENT_3D ( 'NONE', #36904, #68231, #42176 ) ;
#26583 = CARTESIAN_POINT ( 'NONE',  ( -61.41100614348627573, -43.07262267896732766, 43.58025477438756212 ) ) ;
#26584 = ORIENTED_EDGE ( 'NONE', *, *, #67580, .F. ) ;
#26585 = DIRECTION ( 'NONE',  ( 0.000000000000000000, -0.000000000000000000, -1.000000000000000000 ) ) ;
#26586 = DIRECTION ( 'NONE',  ( 0.000000000000000000, 0.000000000000000000, 1.000000000000000000 ) ) ;
#26587 = DIRECTION ( 'NONE',  ( -1.000000000000000000, -0.000000000000000000, -0.000000000000000000 ) ) ;
#26588 = B_SPLINE_CURVE_WITH_KNOTS ( 'NONE', 3,
 ( #37597, #5252, #15805, #32675, #5923, #53419 ),
 .UNSPECIFIED., .F., .F.,
 ( 4, 2, 4 ),
 ( 0.03218950539619244711, 0.06469844149454670457, 0.09720737759290096203 ),
 .UNSPECIFIED. ) ;
#26589 = CARTESIAN_POINT ( 'NONE',  ( 11.29825944729730303, 74.09495289493001735, 41.38025477438755928 ) ) ;
#26590 = CARTESIAN_POINT ( 'NONE',  ( 93.33480479917542993, 21.81892021443993812, -39.92446842644995542 ) ) ;
#26591 = DIRECTION ( 'NONE',  ( -0.9839295885986321100, 0.1785568947986229116, 0.000000000000000000 ) ) ;
#26592 = EDGE_CURVE ( 'NONE', #16384, #21098, #56703, .T. ) ;
#26593 = ORIENTED_EDGE ( 'NONE', *, *, #62583, .T. ) ;
#26595 = ORIENTED_EDGE ( 'NONE', *, *, #35835, .F. ) ;
#26594 = EDGE_CURVE ( 'NONE', #62220, #26511, #67610, .T. ) ;
#26596 = CARTESIAN_POINT ( 'NONE',  ( -118.6849742182705540, 41.92701402439732306, -13.48273187576209153 ) ) ;
#26597 = FACE_BOUND ( 'NONE', #6641, .T. ) ;
#26598 = CARTESIAN_POINT ( 'NONE',  ( -180.6009936245623635, 95.85948119829089364, -14.73603367312734846 ) ) ;
#26599 = EDGE_CURVE ( 'NONE', #21961, #3417, #32061, .T. ) ;
#26600 = DIRECTION ( 'NONE',  ( -0.000000000000000000, -0.000000000000000000, -1.000000000000000000 ) ) ;
#26602 = ORIENTED_EDGE ( 'NONE', *, *, #68461, .T. ) ;
#26601 = CARTESIAN_POINT ( 'NONE',  ( 0.000000000000000000, 200.0000000000000000, 0.000000000000000000 ) ) ;
#26603 = CARTESIAN_POINT ( 'NONE',  ( 60.63380853769238144, 13.16344960520422092, 3.352510954306818558 ) ) ;
#26604 = EDGE_CURVE ( 'NONE', #3562, #11717, #47522, .T. ) ;
#26605 = ORIENTED_EDGE ( 'NONE', *, *, #60899, .T. ) ;
#26606 = CARTESIAN_POINT ( 'NONE',  ( 55.53366667017859015, 12.08690898290841709, 91.85515229178750474 ) ) ;
#26607 = CARTESIAN_POINT ( 'NONE',  ( -61.75956139478098095, 16.58288496614413177, -19.23791488395762528 ) ) ;
#26608 = CARTESIAN_POINT ( 'NONE',  ( 79.19132716134491545, 17.01584750883626995, -17.47194662292698553 ) ) ;
#26609 = AXIS2_PLACEMENT_3D ( 'NONE', #26302, #48758, #58631 ) ;
#26610 = CARTESIAN_POINT ( 'NONE',  ( -130.1938957973835613, 50.61368074696265751, -75.42079035589019043 ) ) ;
#26611 = CARTESIAN_POINT ( 'NONE',  ( -2.116120943112233643, 74.98056102853672655, 170.0000000000000000 ) ) ;
#26612 = DIRECTION ( 'NONE',  ( -1.000000000000000000, -1.001918046209079887E-14, 9.729495617646301779E-15 ) ) ;
#26613 = CARTESIAN_POINT ( 'NONE',  ( -97.49219489034499020, 30.41416107059309937, -75.15255229431038231 ) ) ;
#26614 = ORIENTED_EDGE ( 'NONE', *, *, #45495, .F. ) ;
#26615 = EDGE_LOOP ( 'NONE', ( #66360, #17795, #45988, #44079 ) ) ;
#26616 = ADVANCED_FACE ( 'NONE', ( #14839 ), #20459, .F. ) ;
#26617 = AXIS2_PLACEMENT_3D ( 'NONE', #50273, #29165, #29855 ) ;
#26618 = FACE_OUTER_BOUND ( 'NONE', #24877, .T. ) ;
#26619 = CARTESIAN_POINT ( 'NONE',  ( -78.66644367742111399, 22.32174330031318377, 57.26275173013680586 ) ) ;
#26620 = CARTESIAN_POINT ( 'NONE',  ( -165.6393662153604964, 79.16886183052817216, -41.60625904825717214 ) ) ;
#26622 = EDGE_CURVE ( 'NONE', #54229, #29750, #15876, .T. ) ;
#26621 = CARTESIAN_POINT ( 'NONE',  ( -40.27405704175634327, 63.28161525591265502, 170.0000000000000000 ) ) ;
#26623 = ADVANCED_FACE ( 'NONE', ( #63385 ), #68324, .T. ) ;
#26624 = VECTOR ( 'NONE', #42511, 1000.000000000000000 ) ;
#26625 = CARTESIAN_POINT ( 'NONE',  ( 108.3942953861066627, 29.14039925067521608, -77.55066643792520154 ) ) ;
#26626 = CARTESIAN_POINT ( 'NONE',  ( -73.10086105983762650, 21.34631349770503306, 42.96954990387450835 ) ) ;
#26627 = CARTESIAN_POINT ( 'NONE',  ( 83.38067517854670996, 18.33799117207140128, 30.44781216307082872 ) ) ;
#26628 = VECTOR ( 'NONE', #40735, 1000.000000000000000 ) ;
#26629 = CARTESIAN_POINT ( 'NONE',  ( 68.63585058221465829, 15.08566240483130727, -48.21148126164135306 ) ) ;
#26630 = CARTESIAN_POINT ( 'NONE',  ( 40.38495044702529668, 9.554194848483446023, -50.57113278200800721 ) ) ;
#26631 = DIRECTION ( 'NONE',  ( 0.7041338076821838099, -0.7100673072878299630, 0.000000000000000000 ) ) ;
#26632 = ORIENTED_EDGE ( 'NONE', *, *, #50604, .T. ) ;
#26633 = FACE_OUTER_BOUND ( 'NONE', #21522, .T. ) ;
#26634 = ORIENTED_EDGE ( 'NONE', *, *, #52628, .F. ) ;
#26636 = VECTOR ( 'NONE', #61732, 1000.000000000000000 ) ;
#26635 = CARTESIAN_POINT ( 'NONE',  ( -13.78293860383719327, 7.352367295275509029, -38.33539452421117488 ) ) ;
#26637 = DIRECTION ( 'NONE',  ( -1.000000000000000000, 0.000000000000000000, 0.000000000000000000 ) ) ;
#26638 = CARTESIAN_POINT ( 'NONE',  ( 91.50468583833759340, 22.21368636549395958, 58.33610043527986733 ) ) ;
#26639 = CARTESIAN_POINT ( 'NONE',  ( 150.8925291903903485, 52.71218673668931842, -20.42211489697474036 ) ) ;
#26640 = CARTESIAN_POINT ( 'NONE',  ( 34.82939798935585429, 8.870855050008907838, 16.53448816255987097 ) ) ;
#26641 = LINE ( 'NONE', #17742, #22157 ) ;
#26642 = FACE_OUTER_BOUND ( 'NONE', #55023, .T. ) ;
#26643 = CARTESIAN_POINT ( 'NONE',  ( 111.7895558633182702, 30.71656550562548205, -89.76251668449653209 ) ) ;
#26644 = ORIENTED_EDGE ( 'NONE', *, *, #19067, .T. ) ;
#26645 = CARTESIAN_POINT ( 'NONE',  ( 209.9999999999999716, 190.0000000000000000, 93.99999999999998579 ) ) ;
#26646 = ORIENTED_EDGE ( 'NONE', *, *, #7947, .T. ) ;
#26647 = CARTESIAN_POINT ( 'NONE',  ( 59.73312635112158375, 12.96464920523511744, 57.39663913394880268 ) ) ;
#26648 = DIRECTION ( 'NONE',  ( 0.000000000000000000, 0.000000000000000000, 1.000000000000000000 ) ) ;
#26649 = CARTESIAN_POINT ( 'NONE',  ( 5.799999999999999822, 6.928203230275505220, 4.000000000000006217 ) ) ;
#26650 = CARTESIAN_POINT ( 'NONE',  ( -3.244108878396733342, 6.635632329121485817, 43.57411160445457199 ) ) ;
#26651 = CARTESIAN_POINT ( 'NONE',  ( -94.79534239005248253, 29.13842790650041792, -16.21322624192772111 ) ) ;
#26652 = CARTESIAN_POINT ( 'NONE',  ( 93.99303524761531037, 23.14219721139955865, 89.43772427296207184 ) ) ;
#26653 = ORIENTED_EDGE ( 'NONE', *, *, #2163, .F. ) ;
#26654 = DIRECTION ( 'NONE',  ( 0.000000000000000000, 0.000000000000000000, 1.000000000000000000 ) ) ;
#26655 = CYLINDRICAL_SURFACE ( 'NONE', #1481, 7.500000000000020428 ) ;
#26656 = CARTESIAN_POINT ( 'NONE',  ( -132.2199390322348620, 50.80243550247268303, 15.33512913661918020 ) ) ;
#26657 = CARTESIAN_POINT ( 'NONE',  ( -109.6752351740181837, 37.84903014964775281, 66.14036768415373047 ) ) ;
#26658 = CONTEXT_DEPENDENT_SHAPE_REPRESENTATION ( #42656, #29980 ) ;
#26659 = CARTESIAN_POINT ( 'NONE',  ( -131.2955621888335429, 51.38237199780171238, -47.63902616610417340 ) ) ;
#26660 = ORIENTED_EDGE ( 'NONE', *, *, #2953, .T. ) ;
#26661 = CARTESIAN_POINT ( 'NONE',  ( 0.000000000000000000, 70.00000000000000000, 0.000000000000000000 ) ) ;
#26662 = CARTESIAN_POINT ( 'NONE',  ( 93.92910382125421620, 22.04227458821882024, 65.79627513581792186 ) ) ;
#26663 = AXIS2_PLACEMENT_3D ( 'NONE', #3564, #52770, #58399 ) ;
#26664 =( LENGTH_UNIT ( ) NAMED_UNIT ( * ) SI_UNIT ( .MILLI., .METRE. ) );
#26665 = CARTESIAN_POINT ( 'NONE',  ( -149.3419259515906674, 64.03919805169483936, 84.40698907434087062 ) ) ;
#26666 = CIRCLE ( 'NONE', #16557, 60.00000000000000000 ) ;
#26667 = EDGE_CURVE ( 'NONE', #1187, #19020, #62700, .T. ) ;
#26668 = DIRECTION ( 'NONE',  ( 1.000000000000000000, 0.000000000000000000, 0.000000000000000000 ) ) ;
#26669 = EDGE_LOOP ( 'NONE', ( #22485, #26976 ) ) ;
#26670 = DIRECTION ( 'NONE',  ( 0.000000000000000000, 0.000000000000000000, -1.000000000000000000 ) ) ;
#26671 = CARTESIAN_POINT ( 'NONE',  ( 81.05403189674299824, 18.64820877954959499, 5.327265512142696835 ) ) ;
#26672 = VECTOR ( 'NONE', #34888, 1000.000000000000114 ) ;
#26673 = CARTESIAN_POINT ( 'NONE',  ( 158.3516718297675538, 59.61984652322052369, 2.603653821445219840 ) ) ;
#26674 = CARTESIAN_POINT ( 'NONE',  ( -15.55634918610405748, -15.55634918610400774, 0.000000000000000000 ) ) ;
#26675 = AXIS2_PLACEMENT_3D ( 'NONE', #29286, #51445, #25751 ) ;
#26676 = EDGE_LOOP ( 'NONE', ( #37774, #69182 ) ) ;
#26677 = AXIS2_PLACEMENT_3D ( 'NONE', #6700, #11269, #59457 ) ;
#26678 = EDGE_CURVE ( 'NONE', #49819, #54192, #47880, .T. ) ;
#26679 = CARTESIAN_POINT ( 'NONE',  ( 174.4912080999799002, 73.57140295268875718, 67.23920894112048074 ) ) ;
#26680 = VERTEX_POINT ( 'NONE', #20811 ) ;
#26681 = VECTOR ( 'NONE', #32929, 1000.000000000000000 ) ;
#26682 = CARTESIAN_POINT ( 'NONE',  ( -106.6940984894958149, 35.07986071359380986, -48.59687766299582279 ) ) ;
#26683 = CARTESIAN_POINT ( 'NONE',  ( 64.93495251696903381, 13.12601614965099195, -77.31956637496439555 ) ) ;
#26684 = EDGE_CURVE ( 'NONE', #28328, #6711, #31711, .T. ) ;
#26685 = CARTESIAN_POINT ( 'NONE',  ( 133.8566784816069060, 42.60093787723654657, -62.86786152285933582 ) ) ;
#26686 = ADVANCED_FACE ( 'NONE', ( #57760 ), #15193, .F. ) ;
#26688 = ORIENTED_EDGE ( 'NONE', *, *, #56614, .T. ) ;
#26687 = CARTESIAN_POINT ( 'NONE',  ( 151.7783534118502189, 54.60545177578661935, 14.95502099461759293 ) ) ;
#26689 = FACE_OUTER_BOUND ( 'NONE', #11075, .T. ) ;
#26690 = DIRECTION ( 'NONE',  ( -0.000000000000000000, 1.000000000000000000, -0.000000000000000000 ) ) ;
#26691 = CARTESIAN_POINT ( 'NONE',  ( 117.6853163455684665, 33.60747889659833021, -42.36141487299401120 ) ) ;
#26692 = ORIENTED_EDGE ( 'NONE', *, *, #63838, .F. ) ;
#26693 = DIRECTION ( 'NONE',  ( -1.000000000000000000, 0.000000000000000000, 0.000000000000000000 ) ) ;
#26694 = PLANE ( 'NONE',  #45448 ) ;
#26695 = CARTESIAN_POINT ( 'NONE',  ( -170.2747214445849693, 84.01465441107040988, 45.27347971088749290 ) ) ;
#26696 = CARTESIAN_POINT ( 'NONE',  ( -37.07086358537074489, 10.58360809068250141, -64.68456555099868410 ) ) ;
#26697 = ORIENTED_EDGE ( 'NONE', *, *, #54212, .F. ) ;
#26698 = CARTESIAN_POINT ( 'NONE',  ( 43.14669449386823175, 9.942681284149131216, 17.08585798182755511 ) ) ;
#26699 = EDGE_LOOP ( 'NONE', ( #9310, #57928, #46994, #22955 ) ) ;
#26700 = ORIENTED_EDGE ( 'NONE', *, *, #46307, .F. ) ;
#26702 = ADVANCED_FACE ( 'NONE', ( #48211 ), #5329, .T. ) ;
#26701 = LINE ( 'NONE', #22459, #10400 ) ;
#26703 = CARTESIAN_POINT ( 'NONE',  ( -49.04224900313972313, 13.15187391237128800, 87.00896093370914741 ) ) ;
#26704 = DIRECTION ( 'NONE',  ( -1.020422603260505347E-14, 1.000000000000000000, 5.551115123125782702E-17 ) ) ;
#26705 = CARTESIAN_POINT ( 'NONE',  ( -154.2585856850056132, 68.31650218414625897, -74.96551107100964373 ) ) ;
#26706 = VECTOR ( 'NONE', #49488, 1000.000000000000000 ) ;
#26707 = CARTESIAN_POINT ( 'NONE',  ( 70.21064619801208551, 14.45739791461312507, 88.85860685527731562 ) ) ;
#26708 = EDGE_CURVE ( 'NONE', #22983, #24137, #26784, .T. ) ;
#26709 = DIRECTION ( 'NONE',  ( 0.000000000000000000, 0.000000000000000000, 1.000000000000000000 ) ) ;
#26710 = CARTESIAN_POINT ( 'NONE',  ( -131.6133495896317243, 50.37677745548730712, 69.82229305692996491 ) ) ;
#26711 = CARTESIAN_POINT ( 'NONE',  ( 125.0000000000000000, 0.000000000000000000, 5.000000000000000000 ) ) ;
#26712 = ORIENTED_EDGE ( 'NONE', *, *, #47001, .F. ) ;
#26713 = VECTOR ( 'NONE', #23557, 1000.000000000000000 ) ;
#26714 = DIRECTION ( 'NONE',  ( -0.000000000000000000, -0.000000000000000000, -1.000000000000000000 ) ) ;
#26715 = VERTEX_POINT ( 'NONE', #30683 ) ;
#26716 = CARTESIAN_POINT ( 'NONE',  ( -74.18622060908364801, 21.73430079572372975, 58.72855139418935977 ) ) ;
#26717 = CARTESIAN_POINT ( 'NONE',  ( 183.3913492984167419, 80.96922346472075560, 29.66909328504869237 ) ) ;
#26718 = CARTESIAN_POINT ( 'NONE',  ( 42.48820792780865219, 9.847387255477759282, -23.11522967762586234 ) ) ;
#26719 = CIRCLE ( 'NONE', #30097, 65.36598343705435354 ) ;
#26720 = CARTESIAN_POINT ( 'NONE',  ( -73.10694748374055507, 20.28107308417883559, 6.015984573998315099 ) ) ;
#26721 = CARTESIAN_POINT ( 'NONE',  ( -119.5563837756079835, 43.64229894412653721, 69.00696829185407921 ) ) ;
#26722 = CARTESIAN_POINT ( 'NONE',  ( 8.000000000000007105, 249.8719672152120381, -95.00000000000133582 ) ) ;
#26723 = CARTESIAN_POINT ( 'NONE',  ( 442.3372781065081654, 367.0710678118697388, 108.5502958579838975 ) ) ;
#26724 = PLANE ( 'NONE',  #1849 ) ;
#26725 = VERTEX_POINT ( 'NONE', #69344 ) ;
#26726 = LINE ( 'NONE', #65050, #37570 ) ;
#26727 = DIRECTION ( 'NONE',  ( 9.740878893424455404E-21, -6.106226635438359986E-16, 1.000000000000000000 ) ) ;
#26728 = ORIENTED_EDGE ( 'NONE', *, *, #53903, .T. ) ;
#26729 = EDGE_LOOP ( 'NONE', ( #26653, #60522, #8655, #3370 ) ) ;
#26730 = CARTESIAN_POINT ( 'NONE',  ( -25.07901552294942960, 9.649193085547778992, -65.67922684374194375 ) ) ;
#26731 = CARTESIAN_POINT ( 'NONE',  ( 56.19211641164836379, 11.19288081156168424, -46.34333600376012896 ) ) ;
#26732 = CARTESIAN_POINT ( 'NONE',  ( -31.11269837220801193, 31.11269837220812207, 85.00100000000000477 ) ) ;
#26733 = CARTESIAN_POINT ( 'NONE',  ( 157.4703587214989398, -170.0000000000000000, -51.12418429913766005 ) ) ;
#26734 = AXIS2_PLACEMENT_3D ( 'NONE', #12098, #11042, #33211 ) ;
#26735 = DIRECTION ( 'NONE',  ( -0.000000000000000000, 1.000000000000000000, -0.000000000000000000 ) ) ;
#26736 = EDGE_LOOP ( 'NONE', ( #26550, #10533, #28170, #67433 ) ) ;
#26737 = ORIENTED_EDGE ( 'NONE', *, *, #43705, .F. ) ;
#26738 = CARTESIAN_POINT ( 'NONE',  ( 22.25657943806483274, -170.0000000000000000, 94.99999999999866418 ) ) ;
#26739 = ORIENTED_EDGE ( 'NONE', *, *, #56025, .T. ) ;
#26740 = CARTESIAN_POINT ( 'NONE',  ( 207.8675797643809062, 110.7908513421271550, 16.67352291382450957 ) ) ;
#26741 = CARTESIAN_POINT ( 'NONE',  ( -142.1332311300252798, 59.44822332309653490, 36.82517692171189339 ) ) ;
#26742 = CARTESIAN_POINT ( 'NONE',  ( 57.08336938683662964, 11.37442068895389014, 68.77294810484833931 ) ) ;
#26743 = DIRECTION ( 'NONE',  ( 0.000000000000000000, 1.000000000000000000, -0.000000000000000000 ) ) ;
#26744 = ADVANCED_FACE ( 'NONE', ( #36306 ), #21165, .F. ) ;
#26745 = CARTESIAN_POINT ( 'NONE',  ( 46.66904755831212981, 20.55634918610394379, 0.000000000000000000 ) ) ;
#26746 = PLANE ( 'NONE',  #54075 ) ;
#26747 = EDGE_CURVE ( 'NONE', #32676, #58236, #9228, .T. ) ;
#26748 = DIRECTION ( 'NONE',  ( -0.000000000000000000, 1.000000000000000000, -0.000000000000000000 ) ) ;
#26749 = ORIENTED_EDGE ( 'NONE', *, *, #22162, .T. ) ;
#26750 = ORIENTED_EDGE ( 'NONE', *, *, #42928, .T. ) ;
#26751 = DIRECTION ( 'NONE',  ( 0.000000000000000000, -0.5000000000000013323, -0.8660254037844379305 ) ) ;
#26752 = CARTESIAN_POINT ( 'NONE',  ( 86.62931800182293784, -170.0000000000000000, 37.21208757247931942 ) ) ;
#26753 = CARTESIAN_POINT ( 'NONE',  ( -167.6386155194958576, 81.22597462185134987, -10.22418588222271474 ) ) ;
#26754 = DIRECTION ( 'NONE',  ( 0.1342332658176522420, 0.9909497617679351444, 0.000000000000000000 ) ) ;
#26755 = CARTESIAN_POINT ( 'NONE',  ( 424.8372781065089043, 395.0000000000065938, -123.9497041420121235 ) ) ;
#26756 = CARTESIAN_POINT ( 'NONE',  ( 10.95373880336383543, 7.400264897461164004, 85.46052647922621759 ) ) ;
#26757 = VERTEX_POINT ( 'NONE', #64065 ) ;
#26758 = EDGE_CURVE ( 'NONE', #52558, #38915, #7732, .T. ) ;
#26759 = CARTESIAN_POINT ( 'NONE',  ( -98.67723517640902742, 30.98797878696539598, 71.44587722449948330 ) ) ;
#26760 = EDGE_LOOP ( 'NONE', ( #62287, #42499, #51598, #14867 ) ) ;
#26762 = LINE ( 'NONE', #723, #12671 ) ;
#26761 = CONICAL_SURFACE ( 'NONE', #14418, 8.000000000000001776, 1.047197551196595855 ) ;
#26763 = ORIENTED_EDGE ( 'NONE', *, *, #10304, .F. ) ;
#26764 = EDGE_CURVE ( 'NONE', #53791, #62932, #42270, .T. ) ;
#26765 = CIRCLE ( 'NONE', #69438, 65.00000000000000000 ) ;
#26766 = EDGE_CURVE ( 'NONE', #27252, #45135, #63733, .T. ) ;
#26767 = ORIENTED_EDGE ( 'NONE', *, *, #50744, .F. ) ;
#26768 = CARTESIAN_POINT ( 'NONE',  ( -119.2949674747224975, 43.48097822533564738, 14.87828489523786857 ) ) ;
#26769 = CARTESIAN_POINT ( 'NONE',  ( -180.6011569556094969, 95.85968111394261371, 64.53619258438885709 ) ) ;
#26770 = CIRCLE ( 'NONE', #66119, 19.99999999999998934 ) ;
#26771 = CARTESIAN_POINT ( 'NONE',  ( 126.5710838895481345, 37.19597237024179748, 62.05496881366955364 ) ) ;
#26772 = ORIENTED_EDGE ( 'NONE', *, *, #59613, .F. ) ;
#26773 = B_SPLINE_CURVE_WITH_KNOTS ( 'NONE', 3,
 ( #18526, #18873, #40321, #67083, #61766, #60733, #12553, #39631, #60393, #29087, #3048, #13592, #29424, #24156, #2354, #45247, #39976, #35052, #56494, #65679, #34013, #51230 ),
 .UNSPECIFIED., .F., .F.,
 ( 4, 2, 2, 2, 2, 2, 2, 2, 2, 2, 4 ),
 ( 9.309503074677274191E-17, 0.001318139496345222808, 0.001977209244517771219, 0.002636278992690319848, 0.003954418489035408865, 0.005272557985380498316, 0.005931627733553053450, 0.006590697481725609451, 0.007908836978070743137, 0.009226976474415879426, 0.01054511597076101224 ),
 .UNSPECIFIED. ) ;
#26774 = LINE ( 'NONE', #47870, #18899 ) ;
#26775 = CARTESIAN_POINT ( 'NONE',  ( 149.9838583332408177, 52.05699766415859386, 36.38096985813713502 ) ) ;
#26776 = CARTESIAN_POINT ( 'NONE',  ( -74.58602291351368763, 7.967916035251062290, 43.58025477438756212 ) ) ;
#26777 = DIRECTION ( 'NONE',  ( -1.000000000000000000, 0.000000000000000000, 0.000000000000000000 ) ) ;
#26778 = DIRECTION ( 'NONE',  ( -0.3738650651659383151, 0.9230658208099267181, -0.09041240789275073464 ) ) ;
#26779 = CARTESIAN_POINT ( 'NONE',  ( 86.62931800182293784, -170.0000000000000000, -97.01066537983908233 ) ) ;
#26780 = CARTESIAN_POINT ( 'NONE',  ( -25.35398647985413589, 8.671412257862211703, 33.32529752127744871 ) ) ;
#26781 = CARTESIAN_POINT ( 'NONE',  ( -142.8556048422594813, 60.01994222009838609, -65.68255109197973240 ) ) ;
#26782 = VERTEX_POINT ( 'NONE', #64761 ) ;
#26783 = DIRECTION ( 'NONE',  ( 1.000000000000000000, 0.000000000000000000, 0.000000000000000000 ) ) ;
#26784 = LINE ( 'NONE', #36, #28688 ) ;
#26785 = DIRECTION ( 'NONE',  ( -0.000000000000000000, -0.000000000000000000, -1.000000000000000000 ) ) ;
#26786 = CARTESIAN_POINT ( 'NONE',  ( 0.3194001229790418561, 3.115132258388588760, 8.000000000000001776 ) ) ;
#26787 = CARTESIAN_POINT ( 'NONE',  ( -120.6420427933462207, 44.31795133507804962, -47.77366304952625597 ) ) ;
#26788 = CARTESIAN_POINT ( 'NONE',  ( -85.12122836439577611, 25.97531040437156946, 14.92485516287107217 ) ) ;
#26789 = DIRECTION ( 'NONE',  ( 0.9989930665413143673, 0.04486483035051862939, -0.000000000000000000 ) ) ;
#26790 = EDGE_CURVE ( 'NONE', #34571, #45847, #7064, .T. ) ;
#26791 = CARTESIAN_POINT ( 'NONE',  ( 114.3399910931246950, 21.85871988289598988, 2.504349266409138242 ) ) ;
#26792 = CARTESIAN_POINT ( 'NONE',  ( -78.24476289916013627, 22.16113887290258333, -88.80455181264525777 ) ) ;
#26793 = DIRECTION ( 'NONE',  ( -0.000000000000000000, 1.000000000000000000, -0.000000000000000000 ) ) ;
#26794 = CARTESIAN_POINT ( 'NONE',  ( 160.4963793545269368, 60.04225845346905288, 3.187966924173012195 ) ) ;
#26795 = CARTESIAN_POINT ( 'NONE',  ( 45.79927714077020795, 10.34658019240735705, -92.88875141923965373 ) ) ;
#26796 = VERTEX_POINT ( 'NONE', #59120 ) ;
#26797 = CARTESIAN_POINT ( 'NONE',  ( -3.306248862503413655, 500.0000000000000000, -91.64566090791306863 ) ) ;
#26798 = VERTEX_POINT ( 'NONE', #12344 ) ;
#26799 = CARTESIAN_POINT ( 'NONE',  ( -62.66631205405158767, -18.59153367093452403, 3.125053320693551382E-16 ) ) ;
#26800 = ORIENTED_EDGE ( 'NONE', *, *, #64624, .T. ) ;
#26801 = CARTESIAN_POINT ( 'NONE',  ( 18.43272992546528855, 7.606837839440253823, -62.84086927382109877 ) ) ;
#26802 = CARTESIAN_POINT ( 'NONE',  ( 111.5555719986353864, 30.60523913099746451, 83.38823749445282374 ) ) ;
#26803 = DIRECTION ( 'NONE',  ( -0.4738686624729966379, -0.8805955318567391110, 0.000000000000000000 ) ) ;
#26804 = FACE_OUTER_BOUND ( 'NONE', #68530, .T. ) ;
#26805 = CARTESIAN_POINT ( 'NONE',  ( -190.6985136298601731, 109.1272424661242582, 94.99999999999866418 ) ) ;
#26806 = CARTESIAN_POINT ( 'NONE',  ( 210.1064829626521941, 115.8779605595242970, -92.30285115593483170 ) ) ;
#26807 = CARTESIAN_POINT ( 'NONE',  ( 8.000000000000007105, 249.8719672152120381, -95.00000000000133582 ) ) ;
#26808 = CARTESIAN_POINT ( 'NONE',  ( -21.77424121867212392, -54.12382879860719243, 27.58472369383527578 ) ) ;
#26809 = ORIENTED_EDGE ( 'NONE', *, *, #49285, .F. ) ;
#26810 = ORIENTED_EDGE ( 'NONE', *, *, #34660, .F. ) ;
#26811 = DIRECTION ( 'NONE',  ( 0.000000000000000000, 1.000000000000000000, -0.000000000000000000 ) ) ;
#26812 = CARTESIAN_POINT ( 'NONE',  ( 174.3147410850615131, 73.40482959803648555, 93.74842768471017962 ) ) ;
#26813 = DIRECTION ( 'NONE',  ( -0.000000000000000000, 0.000000000000000000, 1.000000000000000000 ) ) ;
#26814 = CIRCLE ( 'NONE', #49237, 25.12245591505646303 ) ;
#26815 = PRODUCT_DEFINITION_CONTEXT ( 'detailed design', #59285, 'design' ) ;
#26816 = DIRECTION ( 'NONE',  ( 0.000000000000000000, -0.000000000000000000, -1.000000000000000000 ) ) ;
#26817 = ORIENTED_EDGE ( 'NONE', *, *, #42848, .F. ) ;
#26818 = EDGE_CURVE ( 'NONE', #44398, #46298, #9556, .T. ) ;
#26819 = STYLED_ITEM ( 'NONE', ( #50586 ), #64175 ) ;
#26820 = CARTESIAN_POINT ( 'NONE',  ( 90.91356992076215704, 21.99794663086828805, 16.52815484461689266 ) ) ;
#26821 = CARTESIAN_POINT ( 'NONE',  ( -10.23402954931276376, 7.059791383763807104, 71.56709959516479103 ) ) ;
#26822 = CARTESIAN_POINT ( 'NONE',  ( 212.1734186221016500, 119.0499290057855291, 10.55534217174901812 ) ) ;
#26823 = CARTESIAN_POINT ( 'NONE',  ( -55.15976438495108169, -34.41253982194112382, 0.000000000000000000 ) ) ;
#26824 = CARTESIAN_POINT ( 'NONE',  ( 46.84183314611287585, 9.494161546644496852, -15.29600076990992541 ) ) ;
#26825 = CARTESIAN_POINT ( 'NONE',  ( 208.5889601154908917, 111.8333159387241693, -23.40665082623701920 ) ) ;
#26826 = FACE_BOUND ( 'NONE', #14343, .T. ) ;
#26827 = CARTESIAN_POINT ( 'NONE',  ( 159.2325040199867487, 60.31699144791976153, 71.09951541772399253 ) ) ;
#26828 = EDGE_CURVE ( 'NONE', #33435, #19003, #52196, .T. ) ;
#26829 = EDGE_CURVE ( 'NONE', #27522, #21766, #28158, .T. ) ;
#26830 = EDGE_LOOP ( 'NONE', ( #6257, #29472, #37040, #61712 ) ) ;
#26831 = FACE_OUTER_BOUND ( 'NONE', #26159, .T. ) ;
#26832 = CARTESIAN_POINT ( 'NONE',  ( 88.28889510440060917, 21.05995314109331318, -36.00360628347565495 ) ) ;
#26833 = ADVANCED_FACE ( 'NONE', ( #60530 ), #55240, .F. ) ;
#26834 = DIRECTION ( 'NONE',  ( -0.000000000000000000, 1.000000000000000000, -0.000000000000000000 ) ) ;
#26835 = CARTESIAN_POINT ( 'NONE',  ( -66.97713359923307053, -33.64188291209072190, 41.38025477438755928 ) ) ;
#26836 = CARTESIAN_POINT ( 'NONE',  ( 151.6351261592328683, 53.25263237790402826, 14.78337374240360447 ) ) ;
#26837 = CARTESIAN_POINT ( 'NONE',  ( 313.9975424824652350, 295.8720703627917601, 535.5371946177799600 ) ) ;
#26838 = B_SPLINE_CURVE_WITH_KNOTS ( 'NONE', 3,
 ( #69514, #21335, #58276, #26625, #43129, #53686, #31901, #64251, #54014, #42448, #20646, #25935, #5506, #5844, #42107, #63906, #68497, #20301, #37168, #58616, #15031, #16059, #53332, #4478, #48386, #36489, #58965, #47368, #64601, #26959, #47715, #10779, #68823, #21680, #16409, #63565, #37866, #15376, #59314, #36837 ),
 .UNSPECIFIED., .F., .F.,
 ( 4, 2, 2, 2, 2, 2, 2, 2, 2, 2, 2, 2, 2, 2, 2, 2, 2, 2, 2, 4 ),
 ( 0.02472759712254454789, 0.02626001169882803687, 0.02779242627511152933, 0.02932484085139501831, 0.03009104813953675586, 0.03085725542767849341, 0.03238967000396194423, 0.03315587729210369566, 0.03392208458024545403, 0.03545449915652894302, 0.03698691373281243200, 0.03851932830909592098, 0.04005174288537940996, 0.04158415746166289895, 0.04311657203794638793, 0.04464898661422987691, 0.04541519390237162834, 0.04618140119051337977, 0.04771381576679688957, 0.04924623034308040631 ),
 .UNSPECIFIED. ) ;
#26839 = VERTEX_POINT ( 'NONE', #16219 ) ;
#26840 = DIRECTION ( 'NONE',  ( 0.000000000000000000, 0.000000000000000000, 1.000000000000000000 ) ) ;
#26841 = CARTESIAN_POINT ( 'NONE',  ( 0.4969600502617519400, 8.860760056385744932, 0.6527133886630308579 ) ) ;
#26842 = ORIENTED_EDGE ( 'NONE', *, *, #25736, .T. ) ;
#26843 = ORIENTED_EDGE ( 'NONE', *, *, #5096, .F. ) ;
#26844 = CARTESIAN_POINT ( 'NONE',  ( 40.72999892410475553, 9.601203897218297811, 83.71404436111639313 ) ) ;
#26845 = LINE ( 'NONE', #11696, #4096 ) ;
#26846 = CARTESIAN_POINT ( 'NONE',  ( 103.1567541746301373, 25.73937982110322409, 34.60279117723898423 ) ) ;
#26847 = ADVANCED_FACE ( 'NONE', ( #32751 ), #56290, .F. ) ;
#26848 = ORIENTED_EDGE ( 'NONE', *, *, #50040, .T. ) ;
#26849 = CARTESIAN_POINT ( 'NONE',  ( -56.02358673658414290, 14.94347049174936437, -77.01342999705896375 ) ) ;
#26850 = CARTESIAN_POINT ( 'NONE',  ( -2.172839205444464294, 7.595638683704372340, 5.816862989022147268 ) ) ;
#26851 = CIRCLE ( 'NONE', #23503, 8.000000000000000000 ) ;
#26852 = DIRECTION ( 'NONE',  ( 1.000000000000000000, 0.000000000000000000, 0.000000000000000000 ) ) ;
#26853 = CARTESIAN_POINT ( 'NONE',  ( 164.9036507189915710, 63.66930857265032273, 91.66500914631893693 ) ) ;
#26854 = CARTESIAN_POINT ( 'NONE',  ( 93.32502112557682494, 21.81526022999038972, 33.79663101393975921 ) ) ;
#26855 = EDGE_LOOP ( 'NONE', ( #39743, #43103, #60080, #60764 ) ) ;
#26856 = CARTESIAN_POINT ( 'NONE',  ( 105.4134760436918157, 27.80903124201757493, -10.81885116605370989 ) ) ;
#26857 = CARTESIAN_POINT ( 'NONE',  ( 290.0000000000000568, 0.000000000000000000, 0.000000000000000000 ) ) ;
#26858 = CARTESIAN_POINT ( 'NONE',  ( -35.00000000000002842, -35.00000000000000000, 380.0000000000000000 ) ) ;
#26859 = CARTESIAN_POINT ( 'NONE',  ( -1.298947065946361112, 7.560777410219321482, 94.99999999999866418 ) ) ;
#26860 = AXIS2_PLACEMENT_3D ( 'NONE', #49201, #37972, #7011 ) ;
#26861 = CARTESIAN_POINT ( 'NONE',  ( -83.52199252699273302, 25.31691946248441383, 85.88269580995972774 ) ) ;
#26863 = VERTEX_POINT ( 'NONE', #56994 ) ;
#26862 = CARTESIAN_POINT ( 'NONE',  ( 14.07802349576188483, 39.28261617699831731, 13.79046340968177198 ) ) ;
#26864 = ORIENTED_EDGE ( 'NONE', *, *, #56195, .F. ) ;
#26865 = AXIS2_PLACEMENT_3D ( 'NONE', #12224, #49484, #66749 ) ;
#26866 = ORIENTED_EDGE ( 'NONE', *, *, #51543, .F. ) ;
#26867 = CARTESIAN_POINT ( 'NONE',  ( 110.2429982417149574, 29.99119854320844425, -62.76698815611734972 ) ) ;
#26868 = CARTESIAN_POINT ( 'NONE',  ( 447.3372781065086201, 0.000000000000000000, -111.4497041420118251 ) ) ;
#26869 = CARTESIAN_POINT ( 'NONE',  ( -190.6985136298602015, 109.1272424661243434, -37.65993730791821292 ) ) ;
#26870 = LINE ( 'NONE', #11370, #32136 ) ;
#26871 = CARTESIAN_POINT ( 'NONE',  ( -34.74023699876257609, 11.17830703027882855, 57.80909291234753056 ) ) ;
#26872 = DIRECTION ( 'NONE',  ( -1.110223024625156294E-16, 0.000000000000000000, 1.000000000000000000 ) ) ;
#26873 = CARTESIAN_POINT ( 'NONE',  ( 150.2794558856211040, 52.26944788078752424, -68.26897188648571557 ) ) ;
#26874 = CARTESIAN_POINT ( 'NONE',  ( 0.000000000000000000, 0.000000000000000000, 170.0000000000000000 ) ) ;
#26875 = VERTEX_POINT ( 'NONE', #17975 ) ;
#26876 = CARTESIAN_POINT ( 'NONE',  ( 0.000000000000000000, 0.000000000000000000, 41.38025477438755928 ) ) ;
#26877 = ORIENTED_EDGE ( 'NONE', *, *, #44619, .T. ) ;
#26878 = ORIENTED_EDGE ( 'NONE', *, *, #43017, .T. ) ;
#26879 = CARTESIAN_POINT ( 'NONE',  ( 69.83617901654359628, 15.39919709983077389, -19.50531207266840639 ) ) ;
#26880 = CARTESIAN_POINT ( 'NONE',  ( -84.21836162213173793, 25.60181819557221417, -47.68121567810126038 ) ) ;
#26881 = CARTESIAN_POINT ( 'NONE',  ( 149.4165763529819344, 225.8585178651493663, 129.0000000000000000 ) ) ;
#26882 = CARTESIAN_POINT ( 'NONE',  ( -156.8728827992624986, 72.05711009495561825, 9.933813873631594404 ) ) ;
#26883 = EDGE_CURVE ( 'NONE', #44841, #14663, #38743, .T. ) ;
#26884 = DIRECTION ( 'NONE',  ( 0.000000000000000000, -1.000000000000000000, 0.000000000000000000 ) ) ;
#26885 = CARTESIAN_POINT ( 'NONE',  ( 23.24028701062093916, 6.853614888934261629, 38.49265168136174253 ) ) ;
#26886 = CARTESIAN_POINT ( 'NONE',  ( -152.9826564381572211, 68.52733426032347097, 85.25801961117713290 ) ) ;
#26887 = ORIENTED_EDGE ( 'NONE', *, *, #5392, .F. ) ;
#26888 = ORIENTED_EDGE ( 'NONE', *, *, #18356, .F. ) ;
#26889 = VERTEX_POINT ( 'NONE', #45391 ) ;
#26890 = CARTESIAN_POINT ( 'NONE',  ( -13.78293860383719505, 7.352367295275509029, 15.35370665671618973 ) ) ;
#26891 = CARTESIAN_POINT ( 'NONE',  ( 86.62931800182292363, 20.48449268398425716, -89.51066537983906812 ) ) ;
#26892 = CARTESIAN_POINT ( 'NONE',  ( -38.55214349681827457, 10.86754840574841552, 62.13239515233281196 ) ) ;
#26893 = CIRCLE ( 'NONE', #23554, 65.00000000000000000 ) ;
#26894 = DIRECTION ( 'NONE',  ( -0.000000000000000000, 1.000000000000000000, -0.000000000000000000 ) ) ;
#26895 = ORIENTED_EDGE ( 'NONE', *, *, #38675, .F. ) ;
#26896 = CARTESIAN_POINT ( 'NONE',  ( -65.13282190615095146, -1.847197903505587038E-12, -5.000000000000000000 ) ) ;
#26897 = CARTESIAN_POINT ( 'NONE',  ( -55.05276343752910151, 14.68156374112636620, 3.472777182467474244 ) ) ;
#26898 =( NAMED_UNIT ( * ) SI_UNIT ( $, .STERADIAN. ) SOLID_ANGLE_UNIT ( ) );
#26899 = CARTESIAN_POINT ( 'NONE',  ( 19.54326199789021601, 7.657220834818549093, 4.173189189204250304 ) ) ;
#26900 = CARTESIAN_POINT ( 'NONE',  ( 110.2429982417149432, 28.88204397445229432, 17.76666361527367499 ) ) ;
#26901 = CARTESIAN_POINT ( 'NONE',  ( 0.000000000000000000, 0.000000000000000000, 41.38025477438755928 ) ) ;
#26902 = CARTESIAN_POINT ( 'NONE',  ( -86.17927978631389863, 25.32700573188344251, -42.60343115903025790 ) ) ;
#26903 = CARTESIAN_POINT ( 'NONE',  ( 181.0840389613909736, 78.60582251573003987, 44.30859410551141764 ) ) ;
#26904 = CARTESIAN_POINT ( 'NONE',  ( 0.000000000000000000, -31.50328976398030534, -5.000000000000000000 ) ) ;
#26905 = CARTESIAN_POINT ( 'NONE',  ( 13.14401442664831166, 6.430459733718342896, -62.84079615501572391 ) ) ;
#26906 = EDGE_CURVE ( 'NONE', #67175, #61739, #8461, .T. ) ;
#26907 = ORIENTED_EDGE ( 'NONE', *, *, #52948, .T. ) ;
#26908 = CARTESIAN_POINT ( 'NONE',  ( 12.93264331410934354, -21.39501663729232916, 0.000000000000000000 ) ) ;
#26909 = SHAPE_DEFINITION_REPRESENTATION ( #1877, #22184 ) ;
#26910 = ADVANCED_FACE ( 'NONE', ( #61229 ), #24302, .F. ) ;
#26911 = DIRECTION ( 'NONE',  ( -2.437361367520486303E-16, 5.563118268671760803E-17, 1.000000000000000000 ) ) ;
#26912 = CARTESIAN_POINT ( 'NONE',  ( -132.9409505933031994, 51.31241517713431222, -45.03336911783197394 ) ) ;
#26913 = CARTESIAN_POINT ( 'NONE',  ( 46.13320811200730276, 9.380653113584049407, -73.30836824486340220 ) ) ;
#26914 = AXIS2_PLACEMENT_3D ( 'NONE', #25561, #14305, #40337 ) ;
#26915 = CARTESIAN_POINT ( 'NONE',  ( 182.7686108735401262, 81.77235358504611895, -51.04580610545474428 ) ) ;
#26916 = ORIENTED_EDGE ( 'NONE', *, *, #13190, .F. ) ;
#26917 = ORIENTED_EDGE ( 'NONE', *, *, #39776, .F. ) ;
#26918 = CARTESIAN_POINT ( 'NONE',  ( -31.43908319763710679, 9.591432048623756756, -8.472646774738153752 ) ) ;
#26919 = CARTESIAN_POINT ( 'NONE',  ( 173.7154822107653445, 71.46636395518601148, 89.08536180762163781 ) ) ;
#26920 = ORIENTED_EDGE ( 'NONE', *, *, #21820, .T. ) ;
#26921 = VERTEX_POINT ( 'NONE', #8108 ) ;
#26922 = CARTESIAN_POINT ( 'NONE',  ( 115.7746371641014775, 31.52600568297704697, 69.04386463718626032 ) ) ;
#26923 = ADVANCED_FACE ( 'NONE', ( #51714 ), #2833, .T. ) ;
#26924 = ORIENTED_EDGE ( 'NONE', *, *, #7048, .T. ) ;
#26925 = CARTESIAN_POINT ( 'NONE',  ( 127.4669243510812890, 38.85312661085428232, -66.40869171650194858 ) ) ;
#26926 = DIRECTION ( 'NONE',  ( -0.04486483035051862939, 0.9989930665413143673, 0.000000000000000000 ) ) ;
#26927 = CARTESIAN_POINT ( 'NONE',  ( 139.7883986595928434, 46.32091287009617986, 59.25842257727051532 ) ) ;
#26928 = CARTESIAN_POINT ( 'NONE',  ( 111.9975424824652634, 170.0000000000000284, 354.1673509436691347 ) ) ;
#26929 = AXIS2_PLACEMENT_3D ( 'NONE', #54810, #49171, #18233 ) ;
#26930 = CARTESIAN_POINT ( 'NONE',  ( -102.2801239173131194, 32.78103895658057354, 45.51907450641513009 ) ) ;
#26931 = DIRECTION ( 'NONE',  ( -0.000000000000000000, 1.000000000000000000, -0.000000000000000000 ) ) ;
#26932 = DIRECTION ( 'NONE',  ( 1.000000000000000000, 0.000000000000000000, -0.000000000000000000 ) ) ;
#26933 = EDGE_LOOP ( 'NONE', ( #3694, #23505, #37821, #60412 ) ) ;
#26934 = ORIENTED_EDGE ( 'NONE', *, *, #3754, .F. ) ;
#26935 = DIRECTION ( 'NONE',  ( 1.000000000000000000, 0.000000000000000000, 0.000000000000000000 ) ) ;
#26936 = FACE_OUTER_BOUND ( 'NONE', #36952, .T. ) ;
#26937 = APPLICATION_CONTEXT ( 'automotive_design' ) ;
#26938 = CARTESIAN_POINT ( 'NONE',  ( 181.0840389613909736, 80.03940679743416808, -78.06960825634331513 ) ) ;
#26939 = CARTESIAN_POINT ( 'NONE',  ( -165.6397095829521788, 80.60756690931940227, -69.66568759875811168 ) ) ;
#26941 = VERTEX_POINT ( 'NONE', #19350 ) ;
#26940 = CARTESIAN_POINT ( 'NONE',  ( -142.0685766576042113, 58.11789490499572963, -41.20363413018768028 ) ) ;
#26942 = LINE ( 'NONE', #17065, #16210 ) ;
#26943 = VECTOR ( 'NONE', #33019, 1000.000000000000000 ) ;
#26944 = VERTEX_POINT ( 'NONE', #2147 ) ;
#26945 = CARTESIAN_POINT ( 'NONE',  ( -129.6001310305489085, 48.98284622040321068, 44.64431382829574346 ) ) ;
#26946 = CARTESIAN_POINT ( 'NONE',  ( -71.97767679134960872, 19.88555875055813971, 94.99999999999866418 ) ) ;
#26947 = CARTESIAN_POINT ( 'NONE',  ( 84.97343609940688225, 18.86260005312943733, -9.158222328408974988 ) ) ;
#26948 = FACE_OUTER_BOUND ( 'NONE', #4909, .T. ) ;
#26949 = CARTESIAN_POINT ( 'NONE',  ( 0.000000000000000000, 0.000000000000000000, 43.58025477438756212 ) ) ;
#26950 = CARTESIAN_POINT ( 'NONE',  ( -94.79166046756728292, 29.13671350128075588, 11.66547666712828857 ) ) ;
#26951 = CARTESIAN_POINT ( 'NONE',  ( -98.67723517640901321, 30.98797878696538888, -62.77687572781893977 ) ) ;
#26952 = ORIENTED_EDGE ( 'NONE', *, *, #31156, .F. ) ;
#26953 = EDGE_LOOP ( 'NONE', ( #42216, #27102, #39010, #67899, #28667, #37534 ) ) ;
#26954 = CARTESIAN_POINT ( 'NONE',  ( 188.4937788906149194, 86.43336847120859545, -69.37079316943395213 ) ) ;
#26955 = CARTESIAN_POINT ( 'NONE',  ( 10.13405324523498585, 6.385324379632243641, 32.56244327895191049 ) ) ;
#26956 = DIRECTION ( 'NONE',  ( 0.000000000000000000, 0.000000000000000000, 1.000000000000000000 ) ) ;
#26957 = SPHERICAL_SURFACE ( 'NONE', #13830, 3.000000000000000000 ) ;
#26958 = CIRCLE ( 'NONE', #6733, 5.000000000000004441 ) ;
#26959 = CARTESIAN_POINT ( 'NONE',  ( 105.4134760436918441, 27.80903124201756427, -64.50795234698105673 ) ) ;
#26960 = EDGE_CURVE ( 'NONE', #35779, #58062, #34525, .T. ) ;
#26961 = CARTESIAN_POINT ( 'NONE',  ( 82.74007713545064746, 18.13042311233563808, 30.79472337014629346 ) ) ;
#26962 = DIRECTION ( 'NONE',  ( -1.000000000000000000, -1.387778780781445429E-16, 0.000000000000000000 ) ) ;
#26963 = CARTESIAN_POINT ( 'NONE',  ( -120.4666325602656087, 44.20829586446610904, 32.93748705592776815 ) ) ;
#26964 = CARTESIAN_POINT ( 'NONE',  ( 206.3125232506203304, 108.5822159704962360, 70.88763313768686203 ) ) ;
#26965 = EDGE_LOOP ( 'NONE', ( #21661, #49937 ) ) ;
#26966 = FACE_OUTER_BOUND ( 'NONE', #14073, .T. ) ;
#26967 = ORIENTED_EDGE ( 'NONE', *, *, #55000, .T. ) ;
#26968 = ADVANCED_FACE ( 'NONE', ( #23602 ), #40806, .T. ) ;
#26969 = CARTESIAN_POINT ( 'NONE',  ( -31.92580063159127590, 9.671320706097196407, 3.371903815725487252 ) ) ;
#26970 = CARTESIAN_POINT ( 'NONE',  ( -83.97920458302543523, 24.41672699001660263, 86.30411619380763000 ) ) ;
#26971 = CARTESIAN_POINT ( 'NONE',  ( 94.06699947028486974, 23.17027898120150198, 63.05914927619607369 ) ) ;
#26972 = CARTESIAN_POINT ( 'NONE',  ( 149.9872551245001375, 52.05943539582082025, -16.20506168770759459 ) ) ;
#26973 = CARTESIAN_POINT ( 'NONE',  ( 32.37980458033285913, 8.611076697115695566, 13.21509809174489547 ) ) ;
#26974 = CARTESIAN_POINT ( 'NONE',  ( -95.21085197937823352, 30.44372064875429373, -66.80218551204211508 ) ) ;
#26975 = CARTESIAN_POINT ( 'NONE',  ( -20.55634918610411077, -46.66904755831208718, 2.000000000000001776 ) ) ;
#26976 = ORIENTED_EDGE ( 'NONE', *, *, #64141, .F. ) ;
#26977 = FACE_OUTER_BOUND ( 'NONE', #36129, .T. ) ;
#26978 = DIRECTION ( 'NONE',  ( -0.000000000000000000, 1.000000000000000000, -0.000000000000000000 ) ) ;
#26979 = VERTEX_POINT ( 'NONE', #8814 ) ;
#26980 = DIRECTION ( 'NONE',  ( -0.000000000000000000, 0.000000000000000000, 1.000000000000000000 ) ) ;
#26981 = CARTESIAN_POINT ( 'NONE',  ( 14.80291736570134731, 7.477373894757626260, -62.41206896596168718 ) ) ;
#26982 = DIRECTION ( 'NONE',  ( 0.000000000000000000, -1.000000000000000000, 0.000000000000000000 ) ) ;
#26983 = EDGE_CURVE ( 'NONE', #1313, #7482, #42095, .T. ) ;
#26984 = CARTESIAN_POINT ( 'NONE',  ( -27.00000000000000355, 26.99999999999999645, 12.00000000000000000 ) ) ;
#26985 = LINE ( 'NONE', #53709, #43324 ) ;
#26986 = LINE ( 'NONE', #28027, #17639 ) ;
#26987 = EDGE_CURVE ( 'NONE', #8573, #8018, #48796, .T. ) ;
#26988 = CARTESIAN_POINT ( 'NONE',  ( 94.13654418975937688, 23.19669502308961029, 90.80720038674762407 ) ) ;
#26989 = ORIENTED_EDGE ( 'NONE', *, *, #6166, .F. ) ;
#26990 = CARTESIAN_POINT ( 'NONE',  ( 542.2259808184929852, 965.7112456033421495, 626.5068267248706206 ) ) ;
#26991 = EDGE_CURVE ( 'NONE', #47843, #8605, #4555, .T. ) ;
#26992 = CARTESIAN_POINT ( 'NONE',  ( -190.3074740493607635, 108.5764897054613698, -19.14891730205166809 ) ) ;
#26993 = CARTESIAN_POINT ( 'NONE',  ( -102.2801239173131052, 33.91021738430207932, -76.85912785543962400 ) ) ;
#26994 = CARTESIAN_POINT ( 'NONE',  ( -105.4642082819535887, 35.56541171990215844, 71.67034629880215846 ) ) ;
#26995 = CONTEXT_DEPENDENT_SHAPE_REPRESENTATION ( #39078, #33305 ) ;
#26996 = CARTESIAN_POINT ( 'NONE',  ( -180.6099868604459573, 95.87049015238672212, 92.56375689375346383 ) ) ;
#26997 = VERTEX_POINT ( 'NONE', #47448 ) ;
#26998 = CARTESIAN_POINT ( 'NONE',  ( 157.4703587214989398, -170.0000000000000000, -43.62418429913764584 ) ) ;
#26999 = CARTESIAN_POINT ( 'NONE',  ( -3.252497086158844031, 6.636017118948017490, -22.03862939399687093 ) ) ;
#27000 = SURFACE_SIDE_STYLE ('',( #31946 ) ) ;
#27001 = CARTESIAN_POINT ( 'NONE',  ( -156.5309640077389304, 70.37330322764253765, 89.25824053272464198 ) ) ;
#27002 = CARTESIAN_POINT ( 'NONE',  ( 139.6359093656973585, 45.02518919224740301, 41.79700139785594359 ) ) ;
#27003 = EDGE_CURVE ( 'NONE', #9227, #57612, #16049, .T. ) ;
#27004 = ORIENTED_EDGE ( 'NONE', *, *, #11327, .T. ) ;
#27005 = PLANE ( 'NONE',  #40125 ) ;
#27006 = CARTESIAN_POINT ( 'NONE',  ( 83.37782009939532202, 19.39546426214658226, 17.13040966651107055 ) ) ;
#27007 = CARTESIAN_POINT ( 'NONE',  ( 163.5944442552010116, 63.88381951184479846, 14.40178751837228077 ) ) ;
#27008 = LINE ( 'NONE', #21386, #30819 ) ;
#27009 = EDGE_CURVE ( 'NONE', #41527, #1580, #16825, .T. ) ;
#27010 = ADVANCED_FACE ( 'NONE', ( #48816 ), #11537, .F. ) ;
#27011 = EDGE_CURVE ( 'NONE', #39558, #40674, #54448, .T. ) ;
#27012 = ORIENTED_EDGE ( 'NONE', *, *, #31514, .F. ) ;
#27013 = FACE_OUTER_BOUND ( 'NONE', #56550, .T. ) ;
#27014 = ORIENTED_EDGE ( 'NONE', *, *, #13522, .F. ) ;
#27015 = CARTESIAN_POINT ( 'NONE',  ( -72.78737098446268305, 20.16853011470089641, -20.45466042152229846 ) ) ;
#27016 = CARTESIAN_POINT ( 'NONE',  ( 157.4703587214989113, 58.92748579479260229, 44.40946747225338953 ) ) ;
#27018 = ORIENTED_EDGE ( 'NONE', *, *, #12915, .F. ) ;
#27017 = CARTESIAN_POINT ( 'NONE',  ( 447.3372781065085633, 399.9999999999998863, 78.55029585798817493 ) ) ;
#27019 = CARTESIAN_POINT ( 'NONE',  ( 157.9160637431159557, 57.99786926216935967, 44.40946747225338953 ) ) ;
#27020 = AXIS2_PLACEMENT_3D ( 'NONE', #2940, #61673, #13492 ) ;
#27021 = DIRECTION ( 'NONE',  ( 0.000000000000000000, 1.000000000000000000, 0.000000000000000000 ) ) ;
#27022 = CARTESIAN_POINT ( 'NONE',  ( -5.066666666666671759, 8.000000000000000000, -11.86666666666666536 ) ) ;
#27023 = VERTEX_POINT ( 'NONE', #49521 ) ;
#27024 = COLOUR_RGB ( '',0.7921568627450980005, 0.8196078431372548767, 0.9333333333333333481 ) ;
#27025 = CARTESIAN_POINT ( 'NONE',  ( 0.000000000000000000, 0.000000000000000000, 40.00000000000003553 ) ) ;
#27026 = AXIS2_PLACEMENT_3D ( 'NONE', #41140, #56624, #18295 ) ;
#27027 = CARTESIAN_POINT ( 'NONE',  ( 134.7697261969508418, 41.97802808873665015, 56.39672482949090693 ) ) ;
#27028 = CARTESIAN_POINT ( 'NONE',  ( -178.2328124332056234, 94.56955476227572888, 32.81359777475018547 ) ) ;
#27029 = CARTESIAN_POINT ( 'NONE',  ( -33.37566357177429666, 9.916833145467595756, -76.92377550660138752 ) ) ;
#27030 = VERTEX_POINT ( 'NONE', #64680 ) ;
#27031 = ORIENTED_EDGE ( 'NONE', *, *, #62234, .T. ) ;
#27032 = ORIENTED_EDGE ( 'NONE', *, *, #44122, .F. ) ;
#27033 = CARTESIAN_POINT ( 'NONE',  ( -14.27739076362511206, -30.22315722928984627, 6.893343212288939093 ) ) ;
#27034 = CARTESIAN_POINT ( 'NONE',  ( -47.78549779818827403, 12.85263308667515680, 89.62398069324977712 ) ) ;
#27035 = DIRECTION ( 'NONE',  ( -0.000000000000000000, -1.000000000000000000, 0.000000000000000000 ) ) ;
#27036 = CARTESIAN_POINT ( 'NONE',  ( -107.7020481907979530, 35.62148549414491328, 86.51664613115644897 ) ) ;
#27037 = DIRECTION ( 'NONE',  ( -6.405132834375901070E-16, 1.000000000000000000, 6.405132834375902056E-16 ) ) ;
#27038 = CARTESIAN_POINT ( 'NONE',  ( 10.55634918610397577, -31.11269837220809364, 85.00100000000000477 ) ) ;
#27039 = DIRECTION ( 'NONE',  ( 1.000000000000000000, 0.000000000000000000, 0.000000000000000000 ) ) ;
#27040 = EDGE_LOOP ( 'NONE', ( #15559, #28469 ) ) ;
#27041 = EDGE_CURVE ( 'NONE', #7559, #36317, #22809, .T. ) ;
#27042 = CARTESIAN_POINT ( 'NONE',  ( 111.9975424824652634, 20.00000000000003197, 536.6193948016162949 ) ) ;
#27043 = ORIENTED_EDGE ( 'NONE', *, *, #57077, .F. ) ;
#27044 = FACE_OUTER_BOUND ( 'NONE', #28807, .T. ) ;
#27045 = CARTESIAN_POINT ( 'NONE',  ( 212.0739503583954217, 117.0412199804969617, -72.06906948032111870 ) ) ;
#27046 = DIRECTION ( 'NONE',  ( 1.000000000000000000, 0.000000000000000000, -0.000000000000000000 ) ) ;
#27047 = VECTOR ( 'NONE', #16153, 1000.000000000000000 ) ;
#27048 = CARTESIAN_POINT ( 'NONE',  ( 417.3372781065085633, 395.0000000000000568, -116.4497041420117824 ) ) ;
#27049 = CARTESIAN_POINT ( 'NONE',  ( -35.47329415418259657, 10.28840791552277700, -90.18009615600030315 ) ) ;
#27050 = DIRECTION ( 'NONE',  ( 0.000000000000000000, 0.000000000000000000, 1.000000000000000000 ) ) ;
#27051 = CARTESIAN_POINT ( 'NONE',  ( -190.6985136298601731, 109.1272424661242582, -73.40678087856149148 ) ) ;
#27052 = CYLINDRICAL_SURFACE ( 'NONE', #2999, 5.000000000000004441 ) ;
#27053 = ORIENTED_EDGE ( 'NONE', *, *, #2926, .T. ) ;
#27054 = CARTESIAN_POINT ( 'NONE',  ( 15.55634918610403261, -3.079134169858832593E-14, 2.000000000000001776 ) ) ;
#27055 = DIRECTION ( 'NONE',  ( -1.000000000000000000, 0.000000000000000000, 0.000000000000000000 ) ) ;
#27056 = ORIENTED_EDGE ( 'NONE', *, *, #3959, .F. ) ;
#27057 = VERTEX_POINT ( 'NONE', #21758 ) ;
#27058 = ADVANCED_FACE ( 'NONE', ( #37592 ), #65734, .T. ) ;
#27059 = EDGE_CURVE ( 'NONE', #4597, #295, #42858, .T. ) ;
#27060 = CARTESIAN_POINT ( 'NONE',  ( -24.71645982722742474, 9.599558729461499240, -66.32750219526168678 ) ) ;
#27061 = CARTESIAN_POINT ( 'NONE',  ( 56.66775172211444556, 11.28938863449060115, -39.21877147530136654 ) ) ;
#27062 = EDGE_CURVE ( 'NONE', #10488, #18148, #1008, .T. ) ;
#27063 = CYLINDRICAL_SURFACE ( 'NONE', #60880, 65.00000000000000000 ) ;
#27064 = CARTESIAN_POINT ( 'NONE',  ( -142.5211356634642073, 58.47296527616906303, 8.634676124789878671 ) ) ;
#27065 = EDGE_CURVE ( 'NONE', #63745, #34735, #37941, .T. ) ;
#27066 = ORIENTED_EDGE ( 'NONE', *, *, #42498, .T. ) ;
#27067 = AXIS2_PLACEMENT_3D ( 'NONE', #61611, #38772, #60565 ) ;
#27068 = ORIENTED_EDGE ( 'NONE', *, *, #30420, .T. ) ;
#27069 = CARTESIAN_POINT ( 'NONE',  ( -10.00000000000000000, 1.224646799147353256E-15, 5.000000000000000000 ) ) ;
#27070 = ORIENTED_EDGE ( 'NONE', *, *, #34346, .T. ) ;
#27071 = FACE_OUTER_BOUND ( 'NONE', #24700, .T. ) ;
#27072 = CARTESIAN_POINT ( 'NONE',  ( -142.9756886485677683, 60.11539876121631920, 34.52562815318861311 ) ) ;
#27073 = AXIS2_PLACEMENT_3D ( 'NONE', #1493, #33523, #22954 ) ;
#27074 = CARTESIAN_POINT ( 'NONE',  ( 149.0250918491436778, 6.000000000000000000, -4.435653166495538535 ) ) ;
#27075 = FACE_OUTER_BOUND ( 'NONE', #67313, .T. ) ;
#27076 = CARTESIAN_POINT ( 'NONE',  ( -31.01172313875360587, 10.54069851409512282, -89.00629854612918734 ) ) ;
#27077 = AXIS2_PLACEMENT_3D ( 'NONE', #65906, #17705, #1883 ) ;
#27079 = AXIS2_PLACEMENT_3D ( 'NONE', #10622, #9607, #68680 ) ;
#27078 = CARTESIAN_POINT ( 'NONE',  ( -13.32397999418070533, 63.99361958670518646, 6.377659838150144402E-18 ) ) ;
#27080 = LINE ( 'NONE', #16184, #12161 ) ;
#27081 = VERTEX_POINT ( 'NONE', #65381 ) ;
#27082 = ORIENTED_EDGE ( 'NONE', *, *, #43644, .F. ) ;
#27083 = FACE_OUTER_BOUND ( 'NONE', #63229, .T. ) ;
#27084 = CYLINDRICAL_SURFACE ( 'NONE', #44032, 7.500000000000013323 ) ;
#27085 = DIRECTION ( 'NONE',  ( 0.000000000000000000, -0.7071067811865475727, 0.7071067811865475727 ) ) ;
#27086 = CARTESIAN_POINT ( 'NONE',  ( 134.3159642998340075, 41.70198410084976359, -77.86786152285935714 ) ) ;
#27087 = CARTESIAN_POINT ( 'NONE',  ( 64.69649025047539226, 13.06878919510320891, 29.99968890139355082 ) ) ;
#27088 = CIRCLE ( 'NONE', #28195, 25.00000000000000000 ) ;
#27089 = EDGE_CURVE ( 'NONE', #64204, #59065, #5950, .T. ) ;
#27090 = CARTESIAN_POINT ( 'NONE',  ( 18.97570931738674815, 7.630744579664928473, 84.40680895099953318 ) ) ;
#27091 = EDGE_CURVE ( 'NONE', #1572, #34467, #19178, .T. ) ;
#27092 = ORIENTED_EDGE ( 'NONE', *, *, #67370, .F. ) ;
#27093 = ADVANCED_FACE ( 'NONE', ( #3696 ), #25172, .F. ) ;
#27094 = DIRECTION ( 'NONE',  ( 0.000000000000000000, 0.000000000000000000, 1.000000000000000000 ) ) ;
#27095 = VERTEX_POINT ( 'NONE', #35723 ) ;
#27096 = DIRECTION ( 'NONE',  ( -0.000000000000000000, -0.000000000000000000, -1.000000000000000000 ) ) ;
#27097 = EDGE_LOOP ( 'NONE', ( #27994, #16498, #33704, #24014 ) ) ;
#27098 = ORIENTED_EDGE ( 'NONE', *, *, #56275, .F. ) ;
#27099 = CARTESIAN_POINT ( 'NONE',  ( 12.03317402819681803, 6.409531826169462931, -49.51584580361413401 ) ) ;
#27100 = DIRECTION ( 'NONE',  ( 0.000000000000000000, 0.000000000000000000, -1.000000000000000000 ) ) ;
#27101 = CARTESIAN_POINT ( 'NONE',  ( -125.8938041572051105, 47.69968343338781125, -88.60280507916129977 ) ) ;
#27102 = ORIENTED_EDGE ( 'NONE', *, *, #126, .F. ) ;
#27104 =( BOUNDED_CURVE ( )  B_SPLINE_CURVE ( 3, ( #16374, #43440, #27263, #6521 ),
 .UNSPECIFIED., .F., .F. ) 
 B_SPLINE_CURVE_WITH_KNOTS ( ( 4, 4 ),
 ( 5.539652957384106458, 5.943546125472697561 ),
 .UNSPECIFIED. ) 
 CURVE ( )  GEOMETRIC_REPRESENTATION_ITEM ( )  RATIONAL_B_SPLINE_CURVE ( ( 1.000000000000000000, 0.9864519964717846090, 0.9864519964717846090, 1.000000000000000000 ) ) 
 REPRESENTATION_ITEM ( '' )  );
#27103 = CARTESIAN_POINT ( 'NONE',  ( 103.0463737467386665, -170.0000000000000000, -95.00000000000133582 ) ) ;
#27105 = DIRECTION ( 'NONE',  ( -1.000000000000000000, 0.000000000000000000, -0.000000000000000000 ) ) ;
#27106 = CARTESIAN_POINT ( 'NONE',  ( 69.36287815987333261, 15.27486453472191208, 33.31009857533451424 ) ) ;
#27107 = CARTESIAN_POINT ( 'NONE',  ( -31.11269837220806878, 5.594483210025202879E-14, 0.000000000000000000 ) ) ;
#27108 = DIRECTION ( 'NONE',  ( -0.000000000000000000, 1.000000000000000000, -0.000000000000000000 ) ) ;
#27109 = DIRECTION ( 'NONE',  ( 0.000000000000000000, 1.000000000000000000, -0.000000000000000000 ) ) ;
#27110 = CARTESIAN_POINT ( 'NONE',  ( -26.50364027666004318, 8.832969329054181529, 32.04808994178188897 ) ) ;
#27111 = DIRECTION ( 'NONE',  ( 1.000000000000000000, 0.000000000000000000, 0.000000000000000000 ) ) ;
#27112 = B_SPLINE_CURVE_WITH_KNOTS ( 'NONE', 3,
 ( #65301, #32594, #64255, #42453, #16063, #49095, #26284, #21339, #37517, #32934, #22035, #38560, #21683, #38214, #53689, #48746, #54019, #5847, #10782, #64604, #32256, #22382, #15724, #43133, #69519, #584, #16412, #31906, #27303, #59652, #17091, #11467, #54376, #60006, #53336, #6202, #27654, #11827, #4815, #69180, #5167, #26630, #48064, #39612 ),
 .UNSPECIFIED., .F., .F.,
 ( 4, 2, 2, 2, 2, 2, 2, 2, 2, 2, 2, 2, 2, 2, 2, 2, 2, 2, 2, 2, 2, 4 ),
 ( 0.000000000000000000, 0.001472974678681631235, 0.002209462018022446961, 0.002945949357363262470, 0.004418924036044874840, 0.005891898714726486776, 0.007364873393408098712, 0.008101360732748905114, 0.008837848072089711515, 0.01031082275077132258, 0.01178379742945293539, 0.01252028476879375046, 0.01325677210813456554, 0.01472974678681621824, 0.01546623412615704372, 0.01620272146549786921, 0.01767569614417952364, 0.01914867082286117461, 0.01988515816220199489, 0.02062164550154281517, 0.02209462018022445920, 0.02356759485890609976 ),
 .UNSPECIFIED. ) ;
#27113 = ORIENTED_EDGE ( 'NONE', *, *, #42588, .T. ) ;
#27114 = VECTOR ( 'NONE', #2616, 1000.000000000000114 ) ;
#27115 = FACE_BOUND ( 'NONE', #39361, .T. ) ;
#27116 = CARTESIAN_POINT ( 'NONE',  ( -0.3747453031323932926, 6.520267647591907689, -70.75102776234530211 ) ) ;
#27117 = CARTESIAN_POINT ( 'NONE',  ( -180.6215424137751882, 97.48070480470862265, 65.47218828009727076 ) ) ;
#27118 = CARTESIAN_POINT ( 'NONE',  ( 25.97682105948609532, 21.03539606394572914, 6.893343212288937316 ) ) ;
#27119 = DIRECTION ( 'NONE',  ( -0.000000000000000000, -0.000000000000000000, 1.000000000000000000 ) ) ;
#27120 = FACE_OUTER_BOUND ( 'NONE', #55847, .T. ) ;
#27121 = LINE ( 'NONE', #11635, #66284 ) ;
#27122 = CARTESIAN_POINT ( 'NONE',  ( 114.3363611114016578, 21.85800776086857411, -2.510326265702867765 ) ) ;
#27123 = CARTESIAN_POINT ( 'NONE',  ( -76.57217434633363951, 21.53469935507370181, -89.09026432457217481 ) ) ;
#27125 = CARTESIAN_POINT ( 'NONE',  ( 66.73594759725088466, 13.56641407806656296, 16.98519729053115412 ) ) ;
#27124 = VECTOR ( 'NONE', #47441, 1000.000000000000000 ) ;
#27126 =( GEOMETRIC_REPRESENTATION_CONTEXT ( 3 ) GLOBAL_UNCERTAINTY_ASSIGNED_CONTEXT ( ( #38855 ) ) GLOBAL_UNIT_ASSIGNED_CONTEXT ( ( #27409, #21785, #37621 ) ) REPRESENTATION_CONTEXT ( 'NONE', 'WORKASPACE' ) );
#27127 = DIRECTION ( 'NONE',  ( -0.000000000000000000, 0.000000000000000000, -1.000000000000000000 ) ) ;
#27128 = CARTESIAN_POINT ( 'NONE',  ( 90.30732934992394689, 21.77797012484618833, -9.923057525364814779 ) ) ;
#27129 = ORIENTED_EDGE ( 'NONE', *, *, #61637, .F. ) ;
#27130 = ADVANCED_FACE ( 'NONE', ( #68085 ), #41343, .T. ) ;
#27131 = CARTESIAN_POINT ( 'NONE',  ( -33.38294402636583413, 10.93918551420889251, 18.13226767664806971 ) ) ;
#27132 = ORIENTED_EDGE ( 'NONE', *, *, #40932, .T. ) ;
#27133 = CARTESIAN_POINT ( 'NONE',  ( -20.63749999999999574, 0.000000000000000000, -23.50000000000000000 ) ) ;
#27134 = ORIENTED_EDGE ( 'NONE', *, *, #39308, .F. ) ;
#27135 = CARTESIAN_POINT ( 'NONE',  ( 82.94816950786174914, 19.25538918181906922, -63.62716752535860110 ) ) ;
#27136 = CARTESIAN_POINT ( 'NONE',  ( 102.9205852613134482, 26.73239185155387432, 92.46039132013983419 ) ) ;
#27137 = CARTESIAN_POINT ( 'NONE',  ( -148.0058283997321666, 64.22864592525512251, 57.71403787313865053 ) ) ;
#27138 = CARTESIAN_POINT ( 'NONE',  ( 68.93219921887765622, 14.12322281954860870, -20.99186324365028611 ) ) ;
#27139 = VECTOR ( 'NONE', #46790, 1000.000000000000000 ) ;
#27140 = CARTESIAN_POINT ( 'NONE',  ( -23.95089599695169014, 9.496585844566149959, -43.30571257647613947 ) ) ;
#27141 = CARTESIAN_POINT ( 'NONE',  ( -47.60266343315663562, 13.84328785304053433, -68.56165223857558999 ) ) ;
#27142 = CARTESIAN_POINT ( 'NONE',  ( 204.6977192012829789, -170.0000000000000000, -9.481380442157897548 ) ) ;
#27143 = CARTESIAN_POINT ( 'NONE',  ( -121.5928001448269384, 44.91559452735374691, -9.407046580589417673 ) ) ;
#27144 = ORIENTED_EDGE ( 'NONE', *, *, #32916, .T. ) ;
#27145 = VERTEX_POINT ( 'NONE', #62091 ) ;
#27146 = ADVANCED_FACE ( 'NONE', ( #3359 ), #24817, .F. ) ;
#27147 = CARTESIAN_POINT ( 'NONE',  ( 36.77024545412684375, 9.095083943590502429, 57.23105213408622660 ) ) ;
#27148 = CARTESIAN_POINT ( 'NONE',  ( -170.2951623264596890, 85.51757001115473145, 72.12628606607438542 ) ) ;
#27149 = DIRECTION ( 'NONE',  ( -1.000000000000000000, 0.000000000000000000, 0.000000000000000000 ) ) ;
#27150 = EDGE_CURVE ( 'NONE', #49790, #27706, #7301, .T. ) ;
#27151 = EDGE_CURVE ( 'NONE', #35812, #35756, #23063, .T. ) ;
#27152 = CARTESIAN_POINT ( 'NONE',  ( 68.19664458616936997, 14.97277333049207826, -91.47147629385359835 ) ) ;
#27153 = EDGE_LOOP ( 'NONE', ( #8837, #18090 ) ) ;
#27154 = CARTESIAN_POINT ( 'NONE',  ( 93.87111289824404992, 23.09598275302506920, 12.38314846173391004 ) ) ;
#27155 = CARTESIAN_POINT ( 'NONE',  ( 188.5842358232186200, 88.03712271786933741, -17.17993020127526549 ) ) ;
#27156 = CARTESIAN_POINT ( 'NONE',  ( 211.7357196141372242, 118.3691710715567069, 12.47229085737326848 ) ) ;
#27157 = DIRECTION ( 'NONE',  ( 0.000000000000000000, 0.000000000000000000, 1.000000000000000000 ) ) ;
#27158 = LINE ( 'NONE', #43677, #52084 ) ;
#27159 = CARTESIAN_POINT ( 'NONE',  ( 207.4696221732442325, 110.2206209205162111, -23.96229707863594882 ) ) ;
#27160 = CARTESIAN_POINT ( 'NONE',  ( 110.0000000000000284, 21.42428528562853529, -5.000000000000004441 ) ) ;
#27161 = CARTESIAN_POINT ( 'NONE',  ( 161.7031777507227162, 62.31724004902786618, 69.96241716275324052 ) ) ;
#27162 = ORIENTED_EDGE ( 'NONE', *, *, #31602, .F. ) ;
#27163 = CYLINDRICAL_SURFACE ( 'NONE', #45899, 65.00000000000000000 ) ;
#27164 = CARTESIAN_POINT ( 'NONE',  ( -63.76691715686636996, 29.79383981485516841, -25.00000000000000711 ) ) ;
#27165 = CARTESIAN_POINT ( 'NONE',  ( -53.13788504024110182, 15.21566150156364472, 57.39441362419945847 ) ) ;
#27166 = DIRECTION ( 'NONE',  ( -0.000000000000000000, -0.000000000000000000, -1.000000000000000000 ) ) ;
#27167 = LINE ( 'NONE', #38426, #39751 ) ;
#27168 = CARTESIAN_POINT ( 'NONE',  ( -2.077198674172494819, 7.591450106608311543, 86.44301495747437514 ) ) ;
#27169 = VECTOR ( 'NONE', #1695, 1000.000000000000000 ) ;
#27170 = ORIENTED_EDGE ( 'NONE', *, *, #34058, .T. ) ;
#27171 = ADVANCED_FACE ( 'NONE', ( #33723 ), #57515, .F. ) ;
#27172 = CARTESIAN_POINT ( 'NONE',  ( 60.40277045393654021, 12.08176563382370006, 17.50278692932749180 ) ) ;
#27173 = CARTESIAN_POINT ( 'NONE',  ( -7.825402957745087207, 6.891034867348160731, -62.26262132240749736 ) ) ;
#27174 = ORIENTED_EDGE ( 'NONE', *, *, #3418, .F. ) ;
#27175 = VECTOR ( 'NONE', #15968, 1000.000000000000000 ) ;
#27176 = VECTOR ( 'NONE', #24860, 1000.000000000000000 ) ;
#27177 = ORIENTED_EDGE ( 'NONE', *, *, #14616, .F. ) ;
#27178 = CARTESIAN_POINT ( 'NONE',  ( 44.27343555294838495, 10.11032640759955825, 85.36175225958380963 ) ) ;
#27179 = LINE ( 'NONE', #49321, #32146 ) ;
#27180 = LINE ( 'NONE', #60590, #24625 ) ;
#27181 = VERTEX_POINT ( 'NONE', #6979 ) ;
#27182 = VECTOR ( 'NONE', #54516, 1000.000000000000000 ) ;
#27183 = CARTESIAN_POINT ( 'NONE',  ( -58.76005811686687963, 15.70653557534867595, -63.02321690226305151 ) ) ;
#27184 = CLOSED_SHELL ( 'NONE', ( #24973, #17151, #68702, #54270, #30981, #9457, #11328, #37451, #19224, #44858, #13301, #69305, #28429, #1207, #35836, #35349, #26686, #57261, #12223, #67538, #9380, #69481, #31758, #36687, #43403, #10542, #66011, #36763, #44521, #42877, #26545, #57743, #17375, #36957, #32405, #39442, #11987, #43506, #50980, #19545, #63721, #4601, #55821, #61105, #51052 ) ) ;
#27185 = CARTESIAN_POINT ( 'NONE',  ( 31.96227686234410470, 7.558148489540043258, -17.25635040805548215 ) ) ;
#27186 = CARTESIAN_POINT ( 'NONE',  ( 173.6700117628887483, 72.79957362875117610, -42.55458116747357167 ) ) ;
#27187 = CARTESIAN_POINT ( 'NONE',  ( -149.5074843970971017, 65.50121172469319220, -76.65738112195568021 ) ) ;
#27188 = CARTESIAN_POINT ( 'NONE',  ( 89.22118407503259618, 20.32164250407898010, 44.25407225728361738 ) ) ;
#27189 = EDGE_LOOP ( 'NONE', ( #61034, #13006, #9167, #32258 ) ) ;
#27190 = CARTESIAN_POINT ( 'NONE',  ( -47.60266343315662141, 13.84328785304053255, -41.71710164811194943 ) ) ;
#27191 = CARTESIAN_POINT ( 'NONE',  ( 209.9999999999999716, -2.000000000000001776, 72.99999999999998579 ) ) ;
#27192 = DIRECTION ( 'NONE',  ( 0.9839295885986321100, -0.1785568947986229116, 0.000000000000000000 ) ) ;
#27193 = DIRECTION ( 'NONE',  ( 0.000000000000000000, 0.000000000000000000, 1.000000000000000000 ) ) ;
#27194 = CARTESIAN_POINT ( 'NONE',  ( 39.40195752203892710, 8.409560354027398432, -23.77526687496409608 ) ) ;
#27195 = FACE_OUTER_BOUND ( 'NONE', #19407, .T. ) ;
#27197 = ORIENTED_EDGE ( 'NONE', *, *, #7613, .F. ) ;
#27196 = CARTESIAN_POINT ( 'NONE',  ( 200.0000000000000000, 3.000000000000030198, -46.99999999999997158 ) ) ;
#27198 = ORIENTED_EDGE ( 'NONE', *, *, #12957, .T. ) ;
#27199 = ORIENTED_EDGE ( 'NONE', *, *, #67117, .F. ) ;
#27200 = CARTESIAN_POINT ( 'NONE',  ( -12.77647591501652435, 7.263973827022343066, -21.72877552418942315 ) ) ;
#27201 = CARTESIAN_POINT ( 'NONE',  ( -174.5218377053110430, 90.22516661118194747, 84.63846801733375003 ) ) ;
#27202 = FACE_OUTER_BOUND ( 'NONE', #58884, .T. ) ;
#27203 = CARTESIAN_POINT ( 'NONE',  ( 0.000000000000000000, 0.000000000000000000, 0.000000000000000000 ) ) ;
#27204 = EDGE_CURVE ( 'NONE', #33686, #63697, #46603, .T. ) ;
#27205 = CARTESIAN_POINT ( 'NONE',  ( -62.14837099232444473, 17.75045801599139850, -40.27407517813967530 ) ) ;
#27206 = ADVANCED_FACE ( 'NONE', ( #21594 ), #38782, .T. ) ;
#27207 = CARTESIAN_POINT ( 'NONE',  ( -15.13211202216340645, 8.488266782358815377, -17.78287500119007447 ) ) ;
#27208 = CARTESIAN_POINT ( 'NONE',  ( 154.0293889979056985, 55.02370422818217577, -77.14919040647539816 ) ) ;
#27209 = FACE_OUTER_BOUND ( 'NONE', #47502, .T. ) ;
#27210 = VERTEX_POINT ( 'NONE', #52576 ) ;
#27211 = EDGE_CURVE ( 'NONE', #31046, #12220, #37424, .T. ) ;
#27212 = CARTESIAN_POINT ( 'NONE',  ( 196.9999999999999716, 6.000000000000000000, -46.99999999999997158 ) ) ;
#27213 = VERTEX_POINT ( 'NONE', #53934 ) ;
#27214 = ORIENTED_EDGE ( 'NONE', *, *, #15115, .F. ) ;
#27215 = DIRECTION ( 'NONE',  ( -0.000000000000000000, -0.000000000000000000, -1.000000000000000000 ) ) ;
#27216 = CIRCLE ( 'NONE', #66569, 5.000000000000004441 ) ;
#27217 = CARTESIAN_POINT ( 'NONE',  ( -15.55634918610396866, 36.11269837220808654, 85.00100000000000477 ) ) ;
#27218 = CARTESIAN_POINT ( 'NONE',  ( -25.74393077470917746, 9.741270655232812103, 86.48243346646731311 ) ) ;
#27219 = CARTESIAN_POINT ( 'NONE',  ( -154.0833774771448930, 69.51012195447350450, 17.33764892392960277 ) ) ;
#27220 = AXIS2_PLACEMENT_3D ( 'NONE', #23517, #45303, #60444 ) ;
#27221 = CARTESIAN_POINT ( 'NONE',  ( -46.66904755831212981, -15.55634918610397222, 2.000000000000001776 ) ) ;
#27222 = CARTESIAN_POINT ( 'NONE',  ( 22.80839748737788497, 6.826915557457463812, 34.86363334158694727 ) ) ;
#27223 = CARTESIAN_POINT ( 'NONE',  ( -189.2776534485022069, 108.4862893474047638, -95.00000000000133582 ) ) ;
#27224 = ORIENTED_EDGE ( 'NONE', *, *, #35882, .T. ) ;
#27225 = ORIENTED_EDGE ( 'NONE', *, *, #30249, .F. ) ;
#27226 = VERTEX_POINT ( 'NONE', #43041 ) ;
#27227 = AXIS2_PLACEMENT_3D ( 'NONE', #50247, #29480, #44620 ) ;
#27228 = FACE_OUTER_BOUND ( 'NONE', #54661, .T. ) ;
#27229 = CARTESIAN_POINT ( 'NONE',  ( 32.15613847490628530, 8.588587416860166357, -45.07158521509305160 ) ) ;
#27230 = EDGE_CURVE ( 'NONE', #56047, #22100, #50075, .T. ) ;
#27231 = B_SPLINE_CURVE_WITH_KNOTS ( 'NONE', 3,
 ( #8271, #24457, #29720, #1962 ),
 .UNSPECIFIED., .F., .F.,
 ( 4, 4 ),
 ( 9.900409499187197193E-07, 0.05658314289920116785 ),
 .UNSPECIFIED. ) ;
#27232 = EDGE_CURVE ( 'NONE', #61740, #66549, #31140, .T. ) ;
#27233 = CARTESIAN_POINT ( 'NONE',  ( 4.165045035621076863, -64.88046627338039229, 170.0000000000000000 ) ) ;
#27234 = DIRECTION ( 'NONE',  ( 1.850169831522831466E-16, -1.000000000000000000, 5.551115123125781470E-17 ) ) ;
#27235 = ORIENTED_EDGE ( 'NONE', *, *, #20114, .F. ) ;
#27236 = CARTESIAN_POINT ( 'NONE',  ( 188.5651904823862139, 88.01586411309102687, 64.26411188446218148 ) ) ;
#27237 = CARTESIAN_POINT ( 'NONE',  ( -155.2912910578197057, 69.24479901948500071, 69.84663848284604626 ) ) ;
#27238 = CARTESIAN_POINT ( 'NONE',  ( -5.888165822225390755, 7.780336669456525023, -35.66840708012240668 ) ) ;
#27239 = DIRECTION ( 'NONE',  ( -1.000000000000000000, 0.000000000000000000, 0.000000000000000000 ) ) ;
#27240 = CARTESIAN_POINT ( 'NONE',  ( -81.83265147652316784, 46.58665115056960815, 133.5802547743875550 ) ) ;
#27241 = CARTESIAN_POINT ( 'NONE',  ( -85.10774223992955001, 24.88053943842882632, -46.46551204592482520 ) ) ;
#27242 = DIRECTION ( 'NONE',  ( -0.000000000000000000, -0.000000000000000000, -1.000000000000000000 ) ) ;
#27243 = FACE_OUTER_BOUND ( 'NONE', #5927, .T. ) ;
#27244 = DIRECTION ( 'NONE',  ( 0.000000000000000000, 0.000000000000000000, 1.000000000000000000 ) ) ;
#27245 = EDGE_LOOP ( 'NONE', ( #3879, #50922, #4958, #32073 ) ) ;
#27246 = CARTESIAN_POINT ( 'NONE',  ( 11.98601804829804607, 14.28438006995819443, -11.98601804829804607 ) ) ;
#27247 = APPLICATION_PROTOCOL_DEFINITION ( 'draft international standard', 'automotive_design', 1998, #435 ) ;
#27248 = CARTESIAN_POINT ( 'NONE',  ( -30.00000000000000355, 29.99999999999999645, 12.00000000000000000 ) ) ;
#27249 = CARTESIAN_POINT ( 'NONE',  ( -128.9925397612932727, 48.56800623462827815, -49.24758187794226671 ) ) ;
#27250 = DIRECTION ( 'NONE',  ( 5.551115123125781716E-16, -3.469446951953605561E-17, 1.000000000000000000 ) ) ;
#27251 = CARTESIAN_POINT ( 'NONE',  ( 55.76255201544532980, 12.13275766515752174, -72.03696989504328485 ) ) ;
#27252 = VERTEX_POINT ( 'NONE', #37779 ) ;
#27253 = VERTEX_POINT ( 'NONE', #21255 ) ;
#27254 = LINE ( 'NONE', #32542, #46000 ) ;
#27255 = CARTESIAN_POINT ( 'NONE',  ( 174.3253633919052277, 72.03478936859502824, 93.75446226051346343 ) ) ;
#27256 = ORIENTED_EDGE ( 'NONE', *, *, #44792, .T. ) ;
#27257 = VERTEX_POINT ( 'NONE', #47287 ) ;
#27258 = CARTESIAN_POINT ( 'NONE',  ( 181.0840389613909736, 80.03940679743416808, 29.30859410551139277 ) ) ;
#27259 = DIRECTION ( 'NONE',  ( 0.000000000000000000, 0.000000000000000000, -1.000000000000000000 ) ) ;
#27260 = EDGE_LOOP ( 'NONE', ( #17708, #51712, #2931, #28767 ) ) ;
#27261 = FACE_OUTER_BOUND ( 'NONE', #33826, .T. ) ;
#27262 = CARTESIAN_POINT ( 'NONE',  ( 103.8956072042905276, 27.14952820414103840, -93.09487571133699646 ) ) ;
#27263 = CARTESIAN_POINT ( 'NONE',  ( -47.57182537987935689, 17.67134260003773960, -35.17198294190094288 ) ) ;
#27264 = CARTESIAN_POINT ( 'NONE',  ( -74.17694007417655655, 20.66176641130876845, -36.58787508697967183 ) ) ;
#27265 = CARTESIAN_POINT ( 'NONE',  ( 80.95159210695670993, 17.56111694104498611, -92.09322649547419815 ) ) ;
#27266 = CARTESIAN_POINT ( 'NONE',  ( 94.02921784728462740, 22.08005910033066499, -42.07469127671826215 ) ) ;
#27267 = CIRCLE ( 'NONE', #2589, 243.4957430088094839 ) ;
#27268 = DIRECTION ( 'NONE',  ( 0.000000000000000000, 1.000000000000000000, 0.000000000000000000 ) ) ;
#27270 = VERTEX_POINT ( 'NONE', #48652 ) ;
#27269 = B_SPLINE_CURVE_WITH_KNOTS ( 'NONE', 3,
 ( #68875, #20700, #15433, #36890, #58668, #47771, #42503, #22084, #54779, #43525, #28399, #6947, #11511, #1322, #44928, #23135, #12233, #22777, #44220, #49142, #65003, #17496, #32984, #39314, #33697, #28763, #6246, #23489, #39656, #18203, #1673, #17136, #633, #33348, #38254, #55125 ),
 .UNSPECIFIED., .F., .F.,
 ( 4, 2, 2, 2, 2, 2, 2, 2, 2, 2, 2, 2, 2, 2, 2, 2, 2, 4 ),
 ( 1.551583845779545699E-17, 0.001548367318450204286, 0.003096734636900392960, 0.004645101955350582068, 0.006193469273800770308, 0.007741836592250959416, 0.008516020251476042260, 0.009290203910701125972, 0.01083857122915127431, 0.01238693854760142092, 0.01393530586605156926, 0.01548367318450171587, 0.01703204050295186248, 0.01858040782140200908, 0.02012877513985215569, 0.02167714245830229883, 0.02322550977675244543, 0.02477387709520258857 ),
 .UNSPECIFIED. ) ;
#27271 = VERTEX_POINT ( 'NONE', #9678 ) ;
#27272 = DIRECTION ( 'NONE',  ( -0.000000000000000000, -0.000000000000000000, 1.000000000000000000 ) ) ;
#27273 = AXIS2_PLACEMENT_3D ( 'NONE', #30730, #2964, #46902 ) ;
#27274 = FACE_BOUND ( 'NONE', #51990, .T. ) ;
#27275 = CARTESIAN_POINT ( 'NONE',  ( -144.9417090887490929, 61.69631066549399634, -48.26759783987280628 ) ) ;
#27276 = DIRECTION ( 'NONE',  ( -1.000000000000000000, 0.000000000000000000, 0.000000000000000000 ) ) ;
#27278 = VERTEX_POINT ( 'NONE', #58877 ) ;
#27277 = DIRECTION ( 'NONE',  ( -0.000000000000000000, -0.000000000000000000, -1.000000000000000000 ) ) ;
#27279 = CARTESIAN_POINT ( 'NONE',  ( -149.5074843970971301, -170.0000000000000000, -69.15738112195565179 ) ) ;
#27280 = VECTOR ( 'NONE', #12093, 999.9999999999998863 ) ;
#27281 = ORIENTED_EDGE ( 'NONE', *, *, #51556, .F. ) ;
#27282 = CARTESIAN_POINT ( 'NONE',  ( 31.11269837220812562, 31.11269837220800483, 0.000000000000000000 ) ) ;
#27283 = FACE_OUTER_BOUND ( 'NONE', #35849, .T. ) ;
#27284 = CARTESIAN_POINT ( 'NONE',  ( -2.914335439641035288E-14, 0.000000000000000000, -104.9999999999999858 ) ) ;
#27285 = B_SPLINE_CURVE_WITH_KNOTS ( 'NONE', 3,
 ( #20601, #32543, #21298, #15680, #27255, #179, #5801, #14984, #68786, #42063, #63522, #37128, #36798, #53291, #58239, #10056, #26919, #48345, #31515, #4772, #26240, #47672, #48016, #69478, #58920, #10737, #55381, #7571, #17401, #33603, #64910, #65971, #27606, #65249, #33948, #55033, #44489, #38512, #22685, #50118, #1232, #38877, #6855, #21985, #60321, #43432, #16704, #60668, #12141, #39223, #28306, #49746, #61018, #17767, #12485, #39567, #7209, #1577, #38161, #23043, #59602, #18111, #28665, #1947, #23403, #44839, #66323, #49404, #29026, #59959 ),
 .UNSPECIFIED., .F., .F.,
 ( 4, 2, 2, 2, 2, 2, 2, 2, 2, 2, 2, 2, 2, 2, 2, 2, 2, 2, 2, 2, 2, 2, 2, 2, 2, 2, 2, 2, 2, 2, 2, 2, 2, 2, 4 ),
 ( 0.000000000000000000, 0.001217324661923814902, 0.001825986992885731026, 0.002434649323847647151, 0.003651973985771530141, 0.004260636316733491802, 0.004869298647695453897, 0.006086623309619333851, 0.006695285640581253445, 0.007303947971543172171, 0.007912610302505092633, 0.008521272633467011359, 0.009738597295390867895, 0.01095592195731472270, 0.01217324661923857923, 0.01339057128116243577, 0.01460789594308629057, 0.01704254526693400537, 0.01825986992885789487, 0.01947719459078178089, 0.02191184391462955988, 0.02312916857655346325, 0.02434649323847737010, 0.02678114256232515256, 0.02799846722424905593, 0.02921579188617295930, 0.03043311654809685574, 0.03165044121002075911, 0.03225910354098271426, 0.03286776587194466942, 0.03408509053386857973, 0.03530241519579249004, 0.03651973985771640036, 0.03773706451964031067, 0.03895438918156422098 ),
 .UNSPECIFIED. ) ;
#27286 = EDGE_CURVE ( 'NONE', #48080, #62663, #31471, .T. ) ;
#27287 = CARTESIAN_POINT ( 'NONE',  ( 136.9798231265810387, 43.34196232604177368, -23.51336826870209507 ) ) ;
#27288 = CARTESIAN_POINT ( 'NONE',  ( 230.9999999999999432, 0.000000000000000000, 380.0000000000000000 ) ) ;
#27289 = CARTESIAN_POINT ( 'NONE',  ( 6.400000000000000355, 4.618802153517004960, 8.000000000000000000 ) ) ;
#27290 = EDGE_CURVE ( 'NONE', #57264, #45595, #19744, .T. ) ;
#27291 = FACE_OUTER_BOUND ( 'NONE', #9591, .T. ) ;
#27292 = CARTESIAN_POINT ( 'NONE',  ( -99.11448999425219597, 31.20120877265622283, -76.17449768191258386 ) ) ;
#27293 = ORIENTED_EDGE ( 'NONE', *, *, #5063, .F. ) ;
#27294 = EDGE_LOOP ( 'NONE', ( #47721, #19861, #48475, #40549 ) ) ;
#27295 = EDGE_CURVE ( 'NONE', #7511, #37504, #28655, .T. ) ;
#27296 = CARTESIAN_POINT ( 'NONE',  ( 43.96465529479667822, 9.046527005589350523, 31.44099358552342949 ) ) ;
#27297 = DIRECTION ( 'NONE',  ( 1.000000000000000000, 0.000000000000000000, 0.000000000000000000 ) ) ;
#27298 = CARTESIAN_POINT ( 'NONE',  ( 24.39800339187930334, -60.26242556095670722, 43.58025477438756923 ) ) ;
#27299 = LINE ( 'NONE', #27650, #37411 ) ;
#27300 = LINE ( 'NONE', #48742, #7503 ) ;
#27301 = CARTESIAN_POINT ( 'NONE',  ( -78.18897186942403721, 23.21604822208489338, -61.96000122218158168 ) ) ;
#27302 = CARTESIAN_POINT ( 'NONE',  ( 63.99027454648599189, 13.93445177372598565, -50.67285947261250811 ) ) ;
#27303 = CARTESIAN_POINT ( 'NONE',  ( 46.12611922993085045, 10.39838587005582404, -46.45098542691543031 ) ) ;
#27304 = LINE ( 'NONE', #37872, #68906 ) ;
#27305 = EDGE_LOOP ( 'NONE', ( #34975, #64561, #7006, #35825 ) ) ;
#27306 = CARTESIAN_POINT ( 'NONE',  ( 432.4999999999999432, 207.5000000000000284, 378.0000000000000000 ) ) ;
#27307 = EDGE_LOOP ( 'NONE', ( #67039, #11870 ) ) ;
#27308 = CARTESIAN_POINT ( 'NONE',  ( -12.39701069459754379, 7.231688578592715189, -48.88370839588166916 ) ) ;
#27309 = PRESENTATION_LAYER_ASSIGNMENT (  '', '', ( #11587 ) ) ;
#27310 =( NAMED_UNIT ( * ) PLANE_ANGLE_UNIT ( ) SI_UNIT ( $, .RADIAN. ) );
#27311 = CARTESIAN_POINT ( 'NONE',  ( 92.53033045403535084, 22.59263332688195902, 59.40129347602972842 ) ) ;
#27312 = EDGE_CURVE ( 'NONE', #7485, #37971, #6810, .T. ) ;
#27313 = CARTESIAN_POINT ( 'NONE',  ( 152.8558173410470147, 54.14978343559393892, -10.84730958789643829 ) ) ;
#27314 = DIRECTION ( 'NONE',  ( -0.6234898018587318180, -0.7818314824680311359, 0.000000000000000000 ) ) ;
#27315 = DIRECTION ( 'NONE',  ( 0.7530714660036195163, -0.6579387259397027066, 0.000000000000000000 ) ) ;
#27316 = FACE_OUTER_BOUND ( 'NONE', #35034, .T. ) ;
#27317 = CARTESIAN_POINT ( 'NONE',  ( 211.5170725404452412, 116.1892283197351645, 87.25311100178144841 ) ) ;
#27318 = LINE ( 'NONE', #49110, #9518 ) ;
#27319 = VERTEX_POINT ( 'NONE', #28624 ) ;
#27320 = DIRECTION ( 'NONE',  ( 0.3090169943749582759, -0.9510565162951499785, 0.000000000000000000 ) ) ;
#27321 = SURFACE_STYLE_USAGE ( .BOTH. , #48412 ) ;
#27322 = CARTESIAN_POINT ( 'NONE',  ( 31.22608621030911280, -41.16111794767503085, 26.66469104408689006 ) ) ;
#27323 = VECTOR ( 'NONE', #18679, 1000.000000000000000 ) ;
#27324 = CARTESIAN_POINT ( 'NONE',  ( 39.89582146299187571, 9.488756994579086168, -62.46436805589146957 ) ) ;
#27325 = CARTESIAN_POINT ( 'NONE',  ( -5.871577929436018195, 6.771181646175757685, 44.87346486140882718 ) ) ;
#27326 = CARTESIAN_POINT ( 'NONE',  ( 412.3372781065085633, 400.0000000000000568, -111.4497041420117682 ) ) ;
#27327 = VECTOR ( 'NONE', #54051, 1000.000000000000000 ) ;
#27328 = CARTESIAN_POINT ( 'NONE',  ( 93.72616975926867156, 23.04113753715060398, 88.45117781230963772 ) ) ;
#27329 = AXIS2_PLACEMENT_3D ( 'NONE', #2274, #60654, #66310 ) ;
#27330 = VERTEX_POINT ( 'NONE', #60972 ) ;
#27331 = B_SPLINE_CURVE_WITH_KNOTS ( 'NONE', 3,
 ( #3911, #8499, #63690, #8851, #25027, #52764, #9884, #68282, #14114, #57721, #20421, #67942, #36612, #35923, #35577, #25720, #41885, #57036, #29951, #24684, #62994, #46118, #51750, #19388, #19736, #30994, #9533, #15154, #4591, #67589, #30302, #41197, #62658, #14466, #57374, #52441, #9186, #68945, #30643, #20086, #42228, #6318, #10204, #69301, #47838, #701, #33063, #2996, #31672, #48170 ),
 .UNSPECIFIED., .F., .F.,
 ( 4, 2, 2, 2, 2, 2, 2, 2, 2, 2, 2, 2, 2, 2, 2, 2, 2, 2, 2, 2, 2, 2, 2, 2, 4 ),
 ( 0.03126542424884323074, 0.03330676804260265106, 0.03534811183636207832, 0.03738945563012149864, 0.03943079942388091896, 0.04045147132076062912, 0.04147214321764033929, 0.04249281511452004945, 0.04351348701139975961, 0.04555483080515919381, 0.04657550270203893172, 0.04759617459891865576, 0.04810651054735851084, 0.04861684649579836592, 0.04963751839267807608, 0.05065819028955779318, 0.05167886218643750335, 0.05269953408331721351, 0.05372020598019692367, 0.05474087787707663383, 0.05576154977395634399, 0.05780289356771584064, 0.05984423736147533035, 0.06188558115523482006, 0.06392692494899430977 ),
 .UNSPECIFIED. ) ;
#27333 = VECTOR ( 'NONE', #21521, 1000.000000000000000 ) ;
#27332 = DIRECTION ( 'NONE',  ( -1.005272254328559869E-14, 1.000000000000000000, 3.996802888650564334E-15 ) ) ;
#27334 = CARTESIAN_POINT ( 'NONE',  ( -190.0468231512975592, 108.2116162189844601, -18.66563101447177431 ) ) ;
#27335 = CARTESIAN_POINT ( 'NONE',  ( -133.3958821919892728, 51.63629593114587379, 10.76119976374093312 ) ) ;
#27336 = CARTESIAN_POINT ( 'NONE',  ( -166.0012244511291328, 80.97916541034756222, -44.58685355227834890 ) ) ;
#27337 = ITEM_DEFINED_TRANSFORMATION ( 'NONE', 'NONE', #31010,  #66832 ) ;
#27338 = CARTESIAN_POINT ( 'NONE',  ( -132.9126122820979390, 52.52752252041130276, -45.07027942257388986 ) ) ;
#27339 = ORIENTED_EDGE ( 'NONE', *, *, #25816, .F. ) ;
#27340 = DIRECTION ( 'NONE',  ( 1.001917982681609001E-14, -1.000000000000000000, -5.551115123125782702E-17 ) ) ;
#27341 = PLANE ( 'NONE',  #10505 ) ;
#27342 = CARTESIAN_POINT ( 'NONE',  ( 199.3764470687682433, 100.9548044849098858, -11.69055677975092067 ) ) ;
#27343 = CARTESIAN_POINT ( 'NONE',  ( -150.6746572836342182, 65.17487362867251477, 84.48152048434670291 ) ) ;
#27344 = DIRECTION ( 'NONE',  ( 0.1785568947986370669, -0.9839295885986296675, 5.102127870520021999E-18 ) ) ;
#27345 = ORIENTED_EDGE ( 'NONE', *, *, #5761, .T. ) ;
#27346 = DIRECTION ( 'NONE',  ( 0.000000000000000000, 0.000000000000000000, 1.000000000000000000 ) ) ;
#27347 = CARTESIAN_POINT ( 'NONE',  ( -2.700000000000004619, 3.024877593893962577E-15, 24.69999999999999929 ) ) ;
#27348 = CARTESIAN_POINT ( 'NONE',  ( -149.7268278745401346, 65.68859631971236013, 30.72082123989904900 ) ) ;
#27349 = ORIENTED_EDGE ( 'NONE', *, *, #18491, .T. ) ;
#27350 = EDGE_CURVE ( 'NONE', #26757, #43605, #36256, .T. ) ;
#27351 = DIRECTION ( 'NONE',  ( 0.000000000000000000, 0.000000000000000000, -1.000000000000000000 ) ) ;
#27352 = EDGE_LOOP ( 'NONE', ( #16728, #59994, #35474, #19756 ) ) ;
#27353 = EDGE_LOOP ( 'NONE', ( #2114, #20924, #45858, #54114 ) ) ;
#27354 = CARTESIAN_POINT ( 'NONE',  ( -123.0615383220166024, 44.65678520910835658, -89.14556082492318012 ) ) ;
#27355 = CIRCLE ( 'NONE', #4926, 4.999999999999997335 ) ;
#27356 = CARTESIAN_POINT ( 'NONE',  ( 50.97490815085634352, 0.000000000000000000, -46.68900338898716029 ) ) ;
#27357 =( GEOMETRIC_REPRESENTATION_CONTEXT ( 3 ) GLOBAL_UNCERTAINTY_ASSIGNED_CONTEXT ( ( #1552 ) ) GLOBAL_UNIT_ASSIGNED_CONTEXT ( ( #45317, #2761, #13323 ) ) REPRESENTATION_CONTEXT ( 'NONE', 'WORKASPACE' ) );
#27359 = VERTEX_POINT ( 'NONE', #22296 ) ;
#27358 = DIRECTION ( 'NONE',  ( -0.9749279121818226201, -0.2225209339563184452, 0.000000000000000000 ) ) ;
#27360 = CARTESIAN_POINT ( 'NONE',  ( 164.0158927577712689, 62.92463143894071465, 33.20978262532335634 ) ) ;
#27361 = DIRECTION ( 'NONE',  ( 0.000000000000000000, 0.000000000000000000, 1.000000000000000000 ) ) ;
#27362 = FACE_OUTER_BOUND ( 'NONE', #65436, .T. ) ;
#27363 = EDGE_LOOP ( 'NONE', ( #50072, #53278, #12256, #35084 ) ) ;
#27364 = CYLINDRICAL_SURFACE ( 'NONE', #33371, 4.999999999999997335 ) ;
#27366 = EDGE_CURVE ( 'NONE', #14174, #4675, #6470, .T. ) ;
#27365 = CIRCLE ( 'NONE', #66730, 5.000000000000000888 ) ;
#27367 = AXIS2_PLACEMENT_3D ( 'NONE', #2194, #23991, #60921 ) ;
#27368 = EDGE_CURVE ( 'NONE', #67388, #16433, #11379, .T. ) ;
#27369 = CARTESIAN_POINT ( 'NONE',  ( -38.26732153931116187, 10.81230693396213560, -19.08489745522991043 ) ) ;
#27370 = CARTESIAN_POINT ( 'NONE',  ( -180.3114074031036296, 97.09758726817787533, 36.16720739342910917 ) ) ;
#27371 = CIRCLE ( 'NONE', #14987, 5.000000000000000000 ) ;
#27372 = CARTESIAN_POINT ( 'NONE',  ( -36.37663950036512261, 10.45389057208229033, -63.99519408383326180 ) ) ;
#27373 = ORIENTED_EDGE ( 'NONE', *, *, #36201, .T. ) ;
#27374 = ORIENTED_EDGE ( 'NONE', *, *, #31321, .F. ) ;
#27375 = ORIENTED_EDGE ( 'NONE', *, *, #58715, .T. ) ;
#27376 = EDGE_CURVE ( 'NONE', #11698, #57527, #38835, .T. ) ;
#27377 = SURFACE_STYLE_FILL_AREA ( #16138 ) ;
#27378 = CARTESIAN_POINT ( 'NONE',  ( -103.2061297292848963, 34.38496953192505146, 3.717327809790629267 ) ) ;
#27379 = CARTESIAN_POINT ( 'NONE',  ( 2.694222958124177204E-15, 35.00000000000000000, 22.00000000000000355 ) ) ;
#27380 = LINE ( 'NONE', #31634, #46805 ) ;
#27381 = CARTESIAN_POINT ( 'NONE',  ( -109.3054070592207125, 36.49501222209682538, 94.41388992448162298 ) ) ;
#27382 = LINE ( 'NONE', #48820, #11174 ) ;
#27383 = DIRECTION ( 'NONE',  ( -0.000000000000000000, -0.000000000000000000, 1.000000000000000000 ) ) ;
#27384 = CARTESIAN_POINT ( 'NONE',  ( 86.14852828165534504, 19.25704475759651757, 71.55663816294307367 ) ) ;
#27385 = ORIENTED_EDGE ( 'NONE', *, *, #22243, .F. ) ;
#27386 = DIRECTION ( 'NONE',  ( -1.387778780781445429E-16, 1.000000000000000000, 3.081487911019577365E-33 ) ) ;
#27387 = ORIENTED_EDGE ( 'NONE', *, *, #54850, .T. ) ;
#27388 = LINE ( 'NONE', #60095, #16120 ) ;
#27389 = CARTESIAN_POINT ( 'NONE',  ( 208.9781236209186943, 112.4006213943320063, -64.49528624921919118 ) ) ;
#27390 = EDGE_CURVE ( 'NONE', #55620, #13308, #27919, .T. ) ;
#27391 = B_SPLINE_CURVE_WITH_KNOTS ( 'NONE', 3,
 ( #17874, #53748, #17156, #2738, #24553, #35441, #61482, #2054, #19249, #55496, #66776, #50232, #62159, #23506, #45989, #35089, #44948, #28782 ),
 .UNSPECIFIED., .F., .F.,
 ( 4, 2, 2, 2, 2, 2, 2, 2, 4 ),
 ( 0.000000000000000000, 0.001462886883184502792, 0.002194330324776737600, 0.002925773766368972625, 0.004388660649553535915, 0.005851547532738099640, 0.008777321299107172445, 0.01024020818229175525, 0.01170309506547633979 ),
 .UNSPECIFIED. ) ;
#27392 = DIRECTION ( 'NONE',  ( -1.000000000000000000, 0.000000000000000000, 0.000000000000000000 ) ) ;
#27393 = CARTESIAN_POINT ( 'NONE',  ( -76.77329340382465261, 21.60914066444074422, 18.34659420984980471 ) ) ;
#27394 = CARTESIAN_POINT ( 'NONE',  ( 15.55634918610409656, 36.11269837220803680, 0.000000000000000000 ) ) ;
#27395 = CARTESIAN_POINT ( 'NONE',  ( -54.57280099357649306, 14.55288945003959178, 3.472777182467475576 ) ) ;
#27396 = CARTESIAN_POINT ( 'NONE',  ( 198.3476137557912864, 98.02317921105191090, 94.40621084052870060 ) ) ;
#27397 = EDGE_CURVE ( 'NONE', #60665, #30714, #8508, .T. ) ;
#27398 = DIRECTION ( 'NONE',  ( -0.000000000000000000, -1.000000000000000000, -0.000000000000000000 ) ) ;
#27399 = EDGE_CURVE ( 'NONE', #47203, #25401, #65210, .T. ) ;
#27400 = CARTESIAN_POINT ( 'NONE',  ( -7.825402957745087207, -170.0000000000000000, -69.76262132240751157 ) ) ;
#27401 = ORIENTED_EDGE ( 'NONE', *, *, #26594, .T. ) ;
#27402 = LINE ( 'NONE', #22834, #53274 ) ;
#27403 = DIRECTION ( 'NONE',  ( -1.000000000000000000, 0.000000000000000000, 0.000000000000000000 ) ) ;
#27404 = ORIENTED_EDGE ( 'NONE', *, *, #68661, .F. ) ;
#27405 = ORIENTED_EDGE ( 'NONE', *, *, #51492, .F. ) ;
#27406 = CARTESIAN_POINT ( 'NONE',  ( -85.45399718454962112, 25.02415453493131636, 41.11853589859573788 ) ) ;
#27407 = DIRECTION ( 'NONE',  ( 0.000000000000000000, -0.000000000000000000, -1.000000000000000000 ) ) ;
#27408 = DIRECTION ( 'NONE',  ( -0.6427876096865403621, -0.7660444431189770143, 0.000000000000000000 ) ) ;
#27409 =( LENGTH_UNIT ( ) NAMED_UNIT ( * ) SI_UNIT ( .MILLI., .METRE. ) );
#27410 = AXIS2_PLACEMENT_3D ( 'NONE', #36126, #30500, #4462 ) ;
#27411 = PLANE ( 'NONE',  #64531 ) ;
#27412 = ORIENTED_EDGE ( 'NONE', *, *, #58454, .T. ) ;
#27413 = AXIS2_PLACEMENT_3D ( 'NONE', #62460, #4066, #4406 ) ;
#27414 = VERTEX_POINT ( 'NONE', #44442 ) ;
#27415 = CARTESIAN_POINT ( 'NONE',  ( 447.3372781065085633, 370.0000000000001137, -146.4497041420116830 ) ) ;
#27416 = VERTEX_POINT ( 'NONE', #55697 ) ;
#27417 = CARTESIAN_POINT ( 'NONE',  ( 205.5105258529713126, 107.4632495673648549, 17.33006175898614032 ) ) ;
#27418 = CARTESIAN_POINT ( 'NONE',  ( 181.4357232180614403, 80.39782411996594647, -89.91415884680694148 ) ) ;
#27419 = AXIS2_PLACEMENT_3D ( 'NONE', #55017, #18098, #23391 ) ;
#27420 = CARTESIAN_POINT ( 'NONE',  ( 55.56474667084419394, 11.06706367715628581, 65.15011283490898109 ) ) ;
#27421 = CARTESIAN_POINT ( 'NONE',  ( 140.0012045870120687, 46.45892655944614091, 94.99999999999866418 ) ) ;
#27422 = AXIS2_PLACEMENT_3D ( 'NONE', #65402, #49544, #10531 ) ;
#27423 = CARTESIAN_POINT ( 'NONE',  ( -27.58705350908502396, 10.00788090876177172, -90.06758292199550908 ) ) ;
#27424 = AXIS2_PLACEMENT_3D ( 'NONE', #46219, #25134, #62052 ) ;
#27425 = DIRECTION ( 'NONE',  ( 1.000000000000000000, 0.000000000000000000, 0.000000000000000000 ) ) ;
#27426 = CARTESIAN_POINT ( 'NONE',  ( 0.000000000000000000, 0.000000000000000000, 170.0000000000000000 ) ) ;
#27427 = ORIENTED_EDGE ( 'NONE', *, *, #24400, .T. ) ;
#27428 = EDGE_LOOP ( 'NONE', ( #44043, #27846 ) ) ;
#27429 = DIRECTION ( 'NONE',  ( 0.000000000000000000, 0.04541273895899305968, -0.9989683093773508160 ) ) ;
#27430 = CARTESIAN_POINT ( 'NONE',  ( -72.29721455218883364, -19.95276341750119897, 43.58025477438756212 ) ) ;
#27431 = CARTESIAN_POINT ( 'NONE',  ( 0.000000000000000000, 0.000000000000000000, 41.38025477438755928 ) ) ;
#27432 = FACE_OUTER_BOUND ( 'NONE', #42884, .T. ) ;
#27433 = CARTESIAN_POINT ( 'NONE',  ( 63.98971758354224448, 12.90030016320048212, 44.76545530976716236 ) ) ;
#27434 = ORIENTED_EDGE ( 'NONE', *, *, #56725, .T. ) ;
#27435 = EDGE_CURVE ( 'NONE', #40675, #31531, #58055, .T. ) ;
#27436 = CARTESIAN_POINT ( 'NONE',  ( 85.67452303415198855, 19.09699411916382772, 17.82172837155005141 ) ) ;
#27437 = VERTEX_POINT ( 'NONE', #62716 ) ;
#27438 = CARTESIAN_POINT ( 'NONE',  ( -77.02372450489322375, 21.70271995013165522, 30.59644576040608399 ) ) ;
#27439 = VERTEX_POINT ( 'NONE', #57091 ) ;
#27440 = ADVANCED_FACE ( 'NONE', ( #46175 ), #28741, .T. ) ;
#27441 = VERTEX_POINT ( 'NONE', #30701 ) ;
#27442 = CARTESIAN_POINT ( 'NONE',  ( -122.8011284400168108, 45.68452922414294193, 4.427239656831918779 ) ) ;
#27443 = FACE_OUTER_BOUND ( 'NONE', #46456, .T. ) ;
#27444 = DIRECTION ( 'NONE',  ( 1.000000000000000000, 1.387778780781443950E-16, 0.000000000000000000 ) ) ;
#27445 = VERTEX_POINT ( 'NONE', #57433 ) ;
#27446 = PLANE ( 'NONE',  #24438 ) ;
#27447 = ADVANCED_FACE ( 'NONE', ( #35287 ), #14519, .F. ) ;
#27448 = EDGE_CURVE ( 'NONE', #19844, #4383, #65804, .T. ) ;
#27449 = CARTESIAN_POINT ( 'NONE',  ( 150.2076397309211302, 52.21780102759852582, 35.01788660041049894 ) ) ;
#27450 = TOROIDAL_SURFACE ( 'NONE', #51081, 22.50000000000000000, 1.500000000000000444 ) ;
#27451 = LINE ( 'NONE', #23248, #68975 ) ;
#27452 = CARTESIAN_POINT ( 'NONE',  ( 417.3372781065085633, 394.9999999999999432, 83.55029585798834546 ) ) ;
#27453 = DIRECTION ( 'NONE',  ( -0.000000000000000000, -0.000000000000000000, -1.000000000000000000 ) ) ;
#27454 = DIRECTION ( 'NONE',  ( -0.000000000000000000, -0.000000000000000000, -1.000000000000000000 ) ) ;
#27456 = EDGE_LOOP ( 'NONE', ( #49518, #62100, #56589, #22181 ) ) ;
#27455 = EDGE_CURVE ( 'NONE', #25496, #39558, #40907, .T. ) ;
#27457 = DIRECTION ( 'NONE',  ( -0.000000000000000000, -0.000000000000000000, -1.000000000000000000 ) ) ;
#27458 = LINE ( 'NONE', #34850, #23176 ) ;
#27459 = ORIENTED_EDGE ( 'NONE', *, *, #66369, .T. ) ;
#27460 = FACE_BOUND ( 'NONE', #29118, .T. ) ;
#27461 = CARTESIAN_POINT ( 'NONE',  ( -0.7215816834507551292, 6.532459459468099361, -72.18059463655460206 ) ) ;
#27462 = VECTOR ( 'NONE', #21360, 1000.000000000000000 ) ;
#27463 = CARTESIAN_POINT ( 'NONE',  ( -180.6209674222602359, 97.47999311542517376, 64.99958634443271421 ) ) ;
#27464 = CARTESIAN_POINT ( 'NONE',  ( 116.1047574213934439, 31.68944982538900135, -92.41450183877563518 ) ) ;
#27465 = CARTESIAN_POINT ( 'NONE',  ( -121.2119672714299696, 44.67540322905996675, -36.53450468182285960 ) ) ;
#27466 = CARTESIAN_POINT ( 'NONE',  ( -80.56139928459660382, 24.13290941644248022, 18.33423833827008309 ) ) ;
#27467 = DIRECTION ( 'NONE',  ( 1.000000000000000000, 0.000000000000000000, 0.000000000000000000 ) ) ;
#27468 = VECTOR ( 'NONE', #34789, 1000.000000000000000 ) ;
#27469 = CARTESIAN_POINT ( 'NONE',  ( 41.66904755831208007, -15.55634918610412853, 2.000000000000001776 ) ) ;
#27470 = CYLINDRICAL_SURFACE ( 'NONE', #37269, 65.36598343705435354 ) ;
#27471 = CARTESIAN_POINT ( 'NONE',  ( 70.26722489419893236, 14.47234958177331343, 8.490884802020540079 ) ) ;
#27472 = CARTESIAN_POINT ( 'NONE',  ( 164.7250737226290767, 63.51898362052166647, 11.98738555690816732 ) ) ;
#27473 = CARTESIAN_POINT ( 'NONE',  ( 94.06416612695409185, 23.16920323269612325, -15.45855970408906011 ) ) ;
#27474 = ORIENTED_EDGE ( 'NONE', *, *, #55904, .F. ) ;
#27476 = CIRCLE ( 'NONE', #15094, 10.00000000000000178 ) ;
#27475 = CARTESIAN_POINT ( 'NONE',  ( -37.05762690088739220, 11.60527003175540628, 5.897699859483924278 ) ) ;
#27477 = ORIENTED_EDGE ( 'NONE', *, *, #65209, .F. ) ;
#27478 = FACE_OUTER_BOUND ( 'NONE', #11260, .T. ) ;
#27479 = B_SPLINE_CURVE_WITH_KNOTS ( 'NONE', 3,
 ( #41680, #31472, #5427, #53247, #25860, #10349, #47629, #42367, #48304, #139, #20916, #31814, #30787, #26880, #68743, #47288, #57517, #52907, #10691, #42023, #20559, #68420, #14940, #5074, #9325, #69083, #4057, #63139, #63483, #15298, #36406, #32166, #58530, #63828, #57859, #58201, #53596, #21596, #43042, #10021, #14600, #26541, #64164, #9679, #47974, #25521 ),
 .UNSPECIFIED., .F., .F.,
 ( 4, 2, 2, 2, 2, 2, 2, 2, 2, 2, 2, 2, 2, 2, 2, 2, 2, 2, 2, 2, 2, 2, 4 ),
 ( 0.02420077021543442022, 0.02572112563160194529, 0.02648130333968569047, 0.02724148104776943566, 0.02876183646393689480, 0.02952201417202062611, 0.03028219188010435395, 0.03180254729627184085, 0.03332290271243932428, 0.03408308042052305559, 0.03484325812860679383, 0.03636361354477425645, 0.03712379125285799469, 0.03788396896094173294, 0.03864414666902546425, 0.03940432437710920249, 0.04092467979327665817, 0.04244503520944410691, 0.04396539062561156258, 0.04548574604177901826, 0.04624592374986272181, 0.04700610145794643924, 0.04852645687411389491 ),
 .UNSPECIFIED. ) ;
#27480 = CARTESIAN_POINT ( 'NONE',  ( 86.62931800182293784, 20.48449268398422163, -62.66611478937537782 ) ) ;
#27481 = CARTESIAN_POINT ( 'NONE',  ( 104.7547004776452582, 27.52138740370904912, 85.67756394359689409 ) ) ;
#27482 = DIRECTION ( 'NONE',  ( -0.000000000000000000, 1.000000000000000000, -0.000000000000000000 ) ) ;
#27483 = DIRECTION ( 'NONE',  ( -1.000000000000000000, 0.000000000000000000, 0.000000000000000000 ) ) ;
#27484 = EDGE_CURVE ( 'NONE', #13320, #29891, #1776, .T. ) ;
#27485 = EDGE_CURVE ( 'NONE', #634, #17560, #45485, .T. ) ;
#27486 = CARTESIAN_POINT ( 'NONE',  ( -30.46358361599564191, 10.45190018822943756, -35.36507249517946860 ) ) ;
#27487 = CARTESIAN_POINT ( 'NONE',  ( -47.94960849910474820, 13.92522873833625674, -67.10330844354571411 ) ) ;
#27488 = DIRECTION ( 'NONE',  ( -0.000000000000000000, -1.000000000000000000, -0.000000000000000000 ) ) ;
#27489 = ADVANCED_FACE ( 'NONE', ( #29315 ), #66966, .T. ) ;
#27490 = CARTESIAN_POINT ( 'NONE',  ( -122.3759299995709426, 45.41285412136513600, -22.20987056239383506 ) ) ;
#27491 = VERTEX_POINT ( 'NONE', #18764 ) ;
#27492 = ORIENTED_EDGE ( 'NONE', *, *, #34347, .F. ) ;
#27493 = CARTESIAN_POINT ( 'NONE',  ( 8.000000000000001776, 0.000000000000000000, 0.000000000000000000 ) ) ;
#27494 = CARTESIAN_POINT ( 'NONE',  ( 177.0024338932394130, 74.57605685449964028, 69.96155076402908435 ) ) ;
#27495 = CARTESIAN_POINT ( 'NONE',  ( -165.7149569557575717, 80.68479365246975021, 66.38705370719434029 ) ) ;
#27496 = CARTESIAN_POINT ( 'NONE',  ( -165.7713056973201446, 80.74264649718243447, -13.84472355417442024 ) ) ;
#27497 = PRODUCT_DEFINITION_CONTEXT ( 'detailed design', #37723, 'design' ) ;
#27498 = CARTESIAN_POINT ( 'NONE',  ( 450.2085304802404835, 2.000000000000001776, -219.9999999999999147 ) ) ;
#27499 = ORIENTED_EDGE ( 'NONE', *, *, #45433, .F. ) ;
#27500 = CARTESIAN_POINT ( 'NONE',  ( 55.00000000000000000, 16.00000000000000000, -5.803681084894614095 ) ) ;
#27501 = CARTESIAN_POINT ( 'NONE',  ( -12.39413342787890748, 7.231444436041486235, 70.42808861608598647 ) ) ;
#27502 = CARTESIAN_POINT ( 'NONE',  ( 212.1488570093002011, 119.0116247937291405, 8.991641410805247148 ) ) ;
#27503 =( NAMED_UNIT ( * ) SI_UNIT ( $, .STERADIAN. ) SOLID_ANGLE_UNIT ( ) );
#27504 = LINE ( 'NONE', #56241, #18354 ) ;
#27505 = CARTESIAN_POINT ( 'NONE',  ( 46.89006465517228150, 9.501960077668739402, -15.78642848764656392 ) ) ;
#27506 = CARTESIAN_POINT ( 'NONE',  ( 209.6525588430077676, 113.3929734759396837, -22.61648424082018494 ) ) ;
#27507 = CARTESIAN_POINT ( 'NONE',  ( 157.4703587214989398, -170.0000000000000000, -70.46873488960132192 ) ) ;
#27508 = CARTESIAN_POINT ( 'NONE',  ( 163.5944155533005926, 63.88379440759430139, 59.41703486054432659 ) ) ;
#27509 = ORIENTED_EDGE ( 'NONE', *, *, #15323, .F. ) ;
#27510 = DIRECTION ( 'NONE',  ( -1.850371928290090422E-16, 1.000000000000000000, 1.110223024625156171E-16 ) ) ;
#27511 = CARTESIAN_POINT ( 'NONE',  ( -31.43908319763710679, -170.0000000000000000, -42.81719736520184938 ) ) ;
#27512 = AXIS2_PLACEMENT_3D ( 'NONE', #40631, #62794, #4055 ) ;
#27513 = CARTESIAN_POINT ( 'NONE',  ( -47.80251179448168131, 13.89045662648309865, 66.64588604812638550 ) ) ;
#27514 = DIRECTION ( 'NONE',  ( -0.000000000000000000, -6.405132834375902056E-16, 1.000000000000000000 ) ) ;
#27515 = CARTESIAN_POINT ( 'NONE',  ( 156.5909039492009924, 56.96742803863246252, 17.56491688178971344 ) ) ;
#27516 = CARTESIAN_POINT ( 'NONE',  ( -7.174370261180697206, 7.857450515965657800, 83.82589638950733502 ) ) ;
#27517 = AXIS2_PLACEMENT_3D ( 'NONE', #15632, #5065, #10681 ) ;
#27518 = ORIENTED_EDGE ( 'NONE', *, *, #16439, .T. ) ;
#27519 = AXIS2_PLACEMENT_3D ( 'NONE', #33234, #54664, #27939 ) ;
#27520 = CARTESIAN_POINT ( 'NONE',  ( 56.66438910147189034, 11.28870326331393592, 6.471904661552231985 ) ) ;
#27521 = PLANE ( 'NONE',  #28230 ) ;
#27522 = VERTEX_POINT ( 'NONE', #51808 ) ;
#27523 = VERTEX_POINT ( 'NONE', #51471 ) ;
#27524 = EDGE_CURVE ( 'NONE', #46420, #68404, #40218, .T. ) ;
#27525 = VECTOR ( 'NONE', #34674, 1000.000000000000000 ) ;
#27526 = CARTESIAN_POINT ( 'NONE',  ( -78.66644367742109978, 22.32174330031320508, -61.96000122218157458 ) ) ;
#27527 = DIRECTION ( 'NONE',  ( -0.000000000000000000, 1.000000000000000000, -0.000000000000000000 ) ) ;
#27528 = CARTESIAN_POINT ( 'NONE',  ( 108.3819860115547300, 28.02992728837240577, 29.83061142536935506 ) ) ;
#27529 = ORIENTED_EDGE ( 'NONE', *, *, #45169, .F. ) ;
#27530 = CARTESIAN_POINT ( 'NONE',  ( 63.50537371531940778, 13.81987663608982331, 71.65751152968502424 ) ) ;
#27531 = ORIENTED_EDGE ( 'NONE', *, *, #47455, .T. ) ;
#27532 = CARTESIAN_POINT ( 'NONE',  ( 0.000000000000000000, 0.000000000000000000, 0.000000000000000000 ) ) ;
#27533 = CARTESIAN_POINT ( 'NONE',  ( 164.6561571795775478, 64.77723933022096503, 39.12902952882128460 ) ) ;
#27534 = CARTESIAN_POINT ( 'NONE',  ( -156.8728827992623849, 72.05711009495558983, -70.59983789775942853 ) ) ;
#27535 = FACE_OUTER_BOUND ( 'NONE', #48237, .T. ) ;
#27536 = CARTESIAN_POINT ( 'NONE',  ( 0.000000000000000000, 0.000000000000000000, 380.0000000000000000 ) ) ;
#27537 = ADVANCED_FACE ( 'NONE', ( #25086 ), #46523, .F. ) ;
#27538 = B_SPLINE_CURVE_WITH_KNOTS ( 'NONE', 3,
 ( #19822, #52170, #24756, #14538, #3988, #57110, #67669, #40572, #19465, #46539, #68357, #2603, #46893, #19116, #25457, #40923, #30029, #35997, #62026, #68015, #20160, #56406, #18778, #62382, #41274, #57448, #62734, #30372, #24414, #41615, #36341, #3296, #45857, #40236, #61682, #8582, #24062, #51822, #63070, #57793, #29676, #9613, #31076 ),
 .UNSPECIFIED., .F., .F.,
 ( 4, 2, 2, 2, 2, 2, 2, 2, 1, 2, 2, 2, 2, 2, 2, 2, 2, 2, 2, 2, 2, 4 ),
 ( 0.000000000000000000, 0.001465684626643342118, 0.002198526939965013936, 0.002931369253286685971, 0.004397053879930031342, 0.005862738506573376279, 0.007328423133216720349, 0.008061265446538396287, 0.008794107759860071358, 0.009526950073181746428, 0.01025979238650341976, 0.01172547701314676297, 0.01319116163979010443, 0.01465684626643344590, 0.01538968857975511750, 0.01612253089307678910, 0.01758821551972013578, 0.01905390014636348245, 0.01978674245968515405, 0.02051958477300682565, 0.02198526939965016538, 0.02345095402629350512 ),
 .UNSPECIFIED. ) ;
#27539 = CARTESIAN_POINT ( 'NONE',  ( -48.34500911884040875, 14.01939034823941199, -39.35210440960034362 ) ) ;
#27540 = DIRECTION ( 'NONE',  ( -0.000000000000000000, -0.000000000000000000, 1.000000000000000000 ) ) ;
#27541 = ADVANCED_FACE ( 'NONE', ( #45839 ), #29659, .F. ) ;
#27542 = CARTESIAN_POINT ( 'NONE',  ( -28.35957743809535003, 10.12373109553627870, 30.87345809538040697 ) ) ;
#27543 = LINE ( 'NONE', #53576, #42791 ) ;
#27544 = EDGE_CURVE ( 'NONE', #68729, #44045, #32078, .T. ) ;
#27545 = DIRECTION ( 'NONE',  ( 1.000000000000000000, 1.019401483866766449E-14, -9.729483335668566592E-15 ) ) ;
#27547 = ORIENTED_EDGE ( 'NONE', *, *, #66502, .T. ) ;
#27546 = CARTESIAN_POINT ( 'NONE',  ( 259.4165763529819060, -27.00000000000000355, 138.9999999999999716 ) ) ;
#27548 = ORIENTED_EDGE ( 'NONE', *, *, #43186, .F. ) ;
#27549 = VERTEX_POINT ( 'NONE', #53 ) ;
#27550 = CARTESIAN_POINT ( 'NONE',  ( -10.91976120871578004, 7.112268444252501709, -22.90984318353010352 ) ) ;
#27551 = CARTESIAN_POINT ( 'NONE',  ( -173.5307404820223951, 89.09910556100925305, 84.51787358894112856 ) ) ;
#27552 = DIRECTION ( 'NONE',  ( 1.940875045995544638E-32, -1.110223024625156171E-16, 1.000000000000000000 ) ) ;
#27553 = CARTESIAN_POINT ( 'NONE',  ( 427.4999999999999432, 207.5000000000000284, 378.0000000000000000 ) ) ;
#27554 = CARTESIAN_POINT ( 'NONE',  ( -59.57462349605616225, 16.98779896904798292, -48.71995552614745151 ) ) ;
#27555 = CARTESIAN_POINT ( 'NONE',  ( -21.03405120204975276, 13.73704776265648775, 3.061616997868437868E-16 ) ) ;
#27556 = CARTESIAN_POINT ( 'NONE',  ( -71.97767679134960872, 20.95111989827391596, 94.99999999999866418 ) ) ;
#27557 = CARTESIAN_POINT ( 'NONE',  ( 22.89234820949993932, 6.832052815347870123, -18.59162056771186400 ) ) ;
#27558 = ORIENTED_EDGE ( 'NONE', *, *, #1603, .F. ) ;
#27559 = VECTOR ( 'NONE', #62418, 1000.000000000000000 ) ;
#27560 = FACE_OUTER_BOUND ( 'NONE', #53483, .T. ) ;
#27561 = ORIENTED_EDGE ( 'NONE', *, *, #50212, .F. ) ;
#27562 = ORIENTED_EDGE ( 'NONE', *, *, #37558, .F. ) ;
#27563 = CARTESIAN_POINT ( 'NONE',  ( 442.3372781065086201, 0.000000000000000000, -116.4497041420118393 ) ) ;
#27564 = VECTOR ( 'NONE', #49705, 1000.000000000000000 ) ;
#27565 =( LENGTH_UNIT ( ) NAMED_UNIT ( * ) SI_UNIT ( .MILLI., .METRE. ) );
#27566 = CARTESIAN_POINT ( 'NONE',  ( 116.8407179855993263, 32.05539589248573407, 94.43210676044013496 ) ) ;
#27567 = DIRECTION ( 'NONE',  ( -0.000000000000000000, 1.000000000000000000, -0.000000000000000000 ) ) ;
#27568 = EDGE_CURVE ( 'NONE', #57138, #33166, #24427, .T. ) ;
#27569 = CARTESIAN_POINT ( 'NONE',  ( -109.6660553119434951, 36.69391917620600196, 12.50300354649735723 ) ) ;
#27570 = CARTESIAN_POINT ( 'NONE',  ( 23.23895241123075195, 6.853530908437178049, 36.52650928985956114 ) ) ;
#27571 = ADVANCED_FACE ( 'NONE', ( #15209 ), #4995, .F. ) ;
#27572 = FACE_OUTER_BOUND ( 'NONE', #5799, .T. ) ;
#27573 = ORIENTED_EDGE ( 'NONE', *, *, #27568, .T. ) ;
#27574 = ORIENTED_EDGE ( 'NONE', *, *, #33111, .T. ) ;
#27575 = AXIS2_PLACEMENT_3D ( 'NONE', #26601, #37844, #5142 ) ;
#27576 = VERTEX_POINT ( 'NONE', #69362 ) ;
#27577 = CARTESIAN_POINT ( 'NONE',  ( 3.000000000000028866, 0.000000000000000000, -3.000000000000030198 ) ) ;
#27578 = VECTOR ( 'NONE', #57333, 1000.000000000000000 ) ;
#27579 = CARTESIAN_POINT ( 'NONE',  ( -152.5101325120252795, 68.10842280990927122, -8.581351422625143499 ) ) ;
#27580 = CARTESIAN_POINT ( 'NONE',  ( 33.46033188299905703, 8.722678254080108218, -47.70326261524692768 ) ) ;
#27581 = B_SPLINE_CURVE_WITH_KNOTS ( 'NONE', 3,
 ( #38711, #60155, #32734, #54874 ),
 .UNSPECIFIED., .F., .F.,
 ( 4, 4 ),
 ( 9.900409499218689877E-07, 0.05658314289920114704 ),
 .UNSPECIFIED. ) ;
#27582 = CARTESIAN_POINT ( 'NONE',  ( -37.92511097250854135, 10.74631978746599970, 68.33491338229495682 ) ) ;
#27583 = CARTESIAN_POINT ( 'NONE',  ( 157.4703587214989398, -170.0000000000000000, 36.90946747225337532 ) ) ;
#27584 = EDGE_LOOP ( 'NONE', ( #16935, #49691, #68807, #54606 ) ) ;
#27585 = CARTESIAN_POINT ( 'NONE',  ( 447.3372781065085633, 399.9999999999998863, 78.55029585798817493 ) ) ;
#27586 = CARTESIAN_POINT ( 'NONE',  ( 26.11269837220809364, 15.55634918610396866, 0.000000000000000000 ) ) ;
#27587 =( LENGTH_UNIT ( ) NAMED_UNIT ( * ) SI_UNIT ( .MILLI., .METRE. ) );
#27588 = CARTESIAN_POINT ( 'NONE',  ( 424.8372781065089043, 400.0000000000067075, -123.9497041420121235 ) ) ;
#27589 = CARTESIAN_POINT ( 'NONE',  ( 102.7425154123292259, 25.56407025871218863, 10.02495677748274616 ) ) ;
#27590 = LINE ( 'NONE', #10716, #37611 ) ;
#27591 = CARTESIAN_POINT ( 'NONE',  ( 8.000000000000007105, 249.8719672152120381, 94.99999999999866418 ) ) ;
#27592 = CARTESIAN_POINT ( 'NONE',  ( 19.74724861314306423, 6.659670522263896331, 57.98450509540965214 ) ) ;
#27593 = DIRECTION ( 'NONE',  ( 0.000000000000000000, 0.000000000000000000, 1.000000000000000000 ) ) ;
#27594 = CARTESIAN_POINT ( 'NONE',  ( 8.336031647119270360, 6.376437040857335425, -68.88487339447647173 ) ) ;
#27595 = EDGE_LOOP ( 'NONE', ( #18691, #27574, #36554, #44970 ) ) ;
#27596 = DIRECTION ( 'NONE',  ( 1.000000000000000000, 0.000000000000000000, 4.943961906533900219E-16 ) ) ;
#27597 = CONTEXT_DEPENDENT_SHAPE_REPRESENTATION ( #10291, #3027 ) ;
#27598 = CARTESIAN_POINT ( 'NONE',  ( -131.6133495896317243, 50.37677745548732133, -64.40045989538849369 ) ) ;
#27599 = CARTESIAN_POINT ( 'NONE',  ( -131.7724154034330581, 50.48821165954358037, -37.74950181090596857 ) ) ;
#27600 = CARTESIAN_POINT ( 'NONE',  ( 42.49453823366106064, 8.831814337191470798, -63.12732282323006672 ) ) ;
#27601 = CARTESIAN_POINT ( 'NONE',  ( -39.55079474733624068, -51.59997227571039957, 170.0000000000000000 ) ) ;
#27602 = ORIENTED_EDGE ( 'NONE', *, *, #63589, .F. ) ;
#27603 = ORIENTED_EDGE ( 'NONE', *, *, #8920, .T. ) ;
#27604 = CARTESIAN_POINT ( 'NONE',  ( 15.55634918610409656, 31.11269837220803325, 0.000000000000000000 ) ) ;
#27605 = EDGE_CURVE ( 'NONE', #51770, #36565, #1744, .T. ) ;
#27606 = CARTESIAN_POINT ( 'NONE',  ( 177.5697161277706755, 75.12518909700808933, 83.86496702357472088 ) ) ;
#27607 = VERTEX_POINT ( 'NONE', #14858 ) ;
#27608 = VECTOR ( 'NONE', #916, 1000.000000000000000 ) ;
#27609 = EDGE_LOOP ( 'NONE', ( #4507, #5731, #9091, #31097, #3319 ) ) ;
#27610 = ADVANCED_FACE ( 'NONE', ( #36323 ), #20477, .F. ) ;
#27611 = DIRECTION ( 'NONE',  ( -0.000000000000000000, 0.000000000000000000, -1.000000000000000000 ) ) ;
#27612 = FACE_OUTER_BOUND ( 'NONE', #9528, .T. ) ;
#27613 = ORIENTED_EDGE ( 'NONE', *, *, #12104, .F. ) ;
#27614 = CARTESIAN_POINT ( 'NONE',  ( 113.8724110608469147, 31.71510301790680941, 57.37498895187409431 ) ) ;
#27615 = AXIS2_PLACEMENT_3D ( 'NONE', #12980, #39355, #18943 ) ;
#27616 = CARTESIAN_POINT ( 'NONE',  ( 141.3400002717723112, 47.33399859146518907, 64.42256861941518764 ) ) ;
#27617 = LINE ( 'NONE', #23413, #54429 ) ;
#27618 = CARTESIAN_POINT ( 'NONE',  ( -101.8145602049405767, 32.54453702486149780, 45.51907450641512298 ) ) ;
#27619 = VECTOR ( 'NONE', #55019, 1000.000000000000000 ) ;
#27621 = CARTESIAN_POINT ( 'NONE',  ( 17.45749844226121539, 6.558648963513285857, -89.34746460272506852 ) ) ;
#27620 = VECTOR ( 'NONE', #14485, 1000.000000000000000 ) ;
#27622 = CARTESIAN_POINT ( 'NONE',  ( -47.94960849910472689, 13.92522873833625141, -13.41420726261837437 ) ) ;
#27623 = AXIS2_PLACEMENT_3D ( 'NONE', #10816, #44201, #37547 ) ;
#27624 = VECTOR ( 'NONE', #44334, 1000.000000000000000 ) ;
#27625 = ORIENTED_EDGE ( 'NONE', *, *, #13092, .T. ) ;
#27626 = CARTESIAN_POINT ( 'NONE',  ( -20.55634918610400419, 15.55634918610405748, 2.000000000000000000 ) ) ;
#27627 = CIRCLE ( 'NONE', #6289, 5.000000000000000888 ) ;
#27628 = DIRECTION ( 'NONE',  ( 1.000000000000000000, 0.000000000000000000, -0.000000000000000000 ) ) ;
#27629 = EDGE_CURVE ( 'NONE', #54090, #68705, #55261, .T. ) ;
#27630 = CARTESIAN_POINT ( 'NONE',  ( -146.1140637052938587, 62.65471088530801325, -49.01697918332925497 ) ) ;
#27631 = EDGE_CURVE ( 'NONE', #8984, #26090, #6383, .T. ) ;
#27632 = CARTESIAN_POINT ( 'NONE',  ( -137.3060924980642596, 138.4631249211268482, 0.000000000000000000 ) ) ;
#27634 = VERTEX_POINT ( 'NONE', #60545 ) ;
#27633 = LINE ( 'NONE', #11796, #42199 ) ;
#27635 = CARTESIAN_POINT ( 'NONE',  ( 59.72647370436684611, 12.96353798836696214, 17.21311330783555604 ) ) ;
#27636 = VERTEX_POINT ( 'NONE', #17990 ) ;
#27637 = CARTESIAN_POINT ( 'NONE',  ( -148.6426981422629012, 63.44891673852537650, 57.60271724892876222 ) ) ;
#27638 = CARTESIAN_POINT ( 'NONE',  ( -74.81012118577218928, -5.477980300263997293, 170.0000000000000000 ) ) ;
#27639 = DIRECTION ( 'NONE',  ( 1.000000000000000000, 0.000000000000000000, 0.000000000000000000 ) ) ;
#27640 = CARTESIAN_POINT ( 'NONE',  ( 87.59078297315394934, 20.81577753000344444, 29.75859342957748410 ) ) ;
#27641 = CARTESIAN_POINT ( 'NONE',  ( 79.82127737190243977, 17.20935440217364487, -19.63345140900991481 ) ) ;
#27642 = DIRECTION ( 'NONE',  ( 0.000000000000000000, 0.000000000000000000, 1.000000000000000000 ) ) ;
#27643 = CARTESIAN_POINT ( 'NONE',  ( -96.02415295709704424, 29.71480036090584775, 7.030227792584213375 ) ) ;
#27644 = DIRECTION ( 'NONE',  ( 0.000000000000000000, 1.000000000000000000, 0.000000000000000000 ) ) ;
#27645 = ORIENTED_EDGE ( 'NONE', *, *, #51233, .F. ) ;
#27646 = VERTEX_POINT ( 'NONE', #44003 ) ;
#27647 = CARTESIAN_POINT ( 'NONE',  ( 46.13856685535755986, 9.381502944822525336, 40.74731373655765054 ) ) ;
#27648 = CARTESIAN_POINT ( 'NONE',  ( 21.38432669262978436, 61.76910524360982180, 41.38025477438755928 ) ) ;
#27649 = CARTESIAN_POINT ( 'NONE',  ( -51.66904755831210139, 6.635317295611287136E-14, 0.000000000000000000 ) ) ;
#27650 = CARTESIAN_POINT ( 'NONE',  ( 0.000000000000000000, 190.0000000000000000, 0.000000000000000000 ) ) ;
#27651 = CARTESIAN_POINT ( 'NONE',  ( -1.683356153843273750, 65.34430428700410687, 43.58025477438756212 ) ) ;
#27652 = CARTESIAN_POINT ( 'NONE',  ( 0.000000000000000000, 0.000000000000000000, 0.000000000000000000 ) ) ;
#27653 = CARTESIAN_POINT ( 'NONE',  ( 20.00000000000000000, 0.000000000000000000, -20.00000000000000000 ) ) ;
#27654 = CARTESIAN_POINT ( 'NONE',  ( 43.14565945994676355, 9.942782559600567893, -49.62327275826700657 ) ) ;
#27655 = CARTESIAN_POINT ( 'NONE',  ( 211.5175447467296124, 116.1901475271414199, 66.68740704858620916 ) ) ;
#27656 = ORIENTED_EDGE ( 'NONE', *, *, #36703, .F. ) ;
#27657 = CARTESIAN_POINT ( 'NONE',  ( -26.88234027341226096, 9.904106450608200163, 4.894934174378152925 ) ) ;
#27658 = ORIENTED_EDGE ( 'NONE', *, *, #35893, .F. ) ;
#27659 = AXIS2_PLACEMENT_3D ( 'NONE', #41926, #52481, #14843 ) ;
#27660 = PLANE ( 'NONE',  #15036 ) ;
#27661 = CARTESIAN_POINT ( 'NONE',  ( 0.000000000000000000, 0.000000000000000000, 40.00000000000003553 ) ) ;
#27662 = CARTESIAN_POINT ( 'NONE',  ( 89.88147981065577596, 21.62466191578947416, 70.83207453719057867 ) ) ;
#27663 = CARTESIAN_POINT ( 'NONE',  ( 150.5550643769628323, 52.46819381604269239, -19.69512367869445058 ) ) ;
#27664 = CARTESIAN_POINT ( 'NONE',  ( 2.905661822261151883E-14, 20.55634918610402906, 2.000000000000001776 ) ) ;
#27665 = AXIS2_PLACEMENT_3D ( 'NONE', #14789, #15826, #31658 ) ;
#27666 = CARTESIAN_POINT ( 'NONE',  ( 50.71116774460843857, -28.84239744659915416, 27.58472369397436452 ) ) ;
#27667 = CARTESIAN_POINT ( 'NONE',  ( 111.0244322366040564, 30.35584396427519849, -89.64231344153266434 ) ) ;
#27668 = AXIS2_PLACEMENT_3D ( 'NONE', #41804, #9450, #4513 ) ;
#27669 = DIRECTION ( 'NONE',  ( -0.000000000000000000, 1.000000000000000000, -0.000000000000000000 ) ) ;
#27670 = CYLINDRICAL_SURFACE ( 'NONE', #69039, 5.000000000000004441 ) ;
#27671 = VERTEX_POINT ( 'NONE', #43303 ) ;
#27672 = CARTESIAN_POINT ( 'NONE',  ( 197.9812431552294072, 97.56504682326740863, 87.03682254010664110 ) ) ;
#27673 = DIRECTION ( 'NONE',  ( 1.387778780781445429E-16, -1.000000000000000000, -3.081487911019577365E-33 ) ) ;
#27674 = CARTESIAN_POINT ( 'NONE',  ( -30.94753041835916108, 9.510749728915506296, 18.37190381572551701 ) ) ;
#27675 = DIRECTION ( 'NONE',  ( 0.000000000000000000, -0.000000000000000000, 1.000000000000000000 ) ) ;
#27676 = CARTESIAN_POINT ( 'NONE',  ( -62.33640798863619636, 16.75617156245991168, -94.56231254894214544 ) ) ;
#27677 = CARTESIAN_POINT ( 'NONE',  ( -108.5289085648060734, 36.07014995015116199, -65.20415147196632688 ) ) ;
#27678 = CARTESIAN_POINT ( 'NONE',  ( 93.96365369154807468, 23.13106400759562575, 92.50572082305301080 ) ) ;
#27679 = CIRCLE ( 'NONE', #67032, 243.4957430088094839 ) ;
#27680 = EDGE_LOOP ( 'NONE', ( #62715, #39407, #69125, #13287 ) ) ;
#27681 = DIRECTION ( 'NONE',  ( 0.4127082516087853259, -0.9108456776650110109, 0.005661319014690080476 ) ) ;
#27682 = DIRECTION ( 'NONE',  ( 0.000000000000000000, 0.000000000000000000, -1.000000000000000000 ) ) ;
#27683 = CARTESIAN_POINT ( 'NONE',  ( -128.1219934350341703, 47.97781708504715681, 18.45142153448720279 ) ) ;
#27684 = LINE ( 'NONE', #64989, #36818 ) ;
#27685 = EDGE_CURVE ( 'NONE', #37383, #21254, #65481, .T. ) ;
#27686 = CONTEXT_DEPENDENT_SHAPE_REPRESENTATION ( #17491, #65303 ) ;
#27687 = CARTESIAN_POINT ( 'NONE',  ( -179.7029633946883393, 94.76610802182018745, 88.39967368985821849 ) ) ;
#27688 = ORIENTED_EDGE ( 'NONE', *, *, #35155, .F. ) ;
#27689 = CARTESIAN_POINT ( 'NONE',  ( -125.0023254877051500, 45.90912477771773581, -49.87432082388755816 ) ) ;
#27690 = DIRECTION ( 'NONE',  ( 0.000000000000000000, 0.000000000000000000, 1.000000000000000000 ) ) ;
#27691 = CARTESIAN_POINT ( 'NONE',  ( -422.6627218934913799, 394.9999999999998295, -116.4497041420117824 ) ) ;
#27692 = EDGE_CURVE ( 'NONE', #34735, #31501, #68029, .T. ) ;
#27693 = CARTESIAN_POINT ( 'NONE',  ( -5.879983509979052059, 7.779504553499493547, -77.02244074307444066 ) ) ;
#27694 = EDGE_CURVE ( 'NONE', #67865, #27081, #54197, .T. ) ;
#27695 = PLANE ( 'NONE',  #48130 ) ;
#27696 = EDGE_LOOP ( 'NONE', ( #2927, #11086, #60441, #28815 ) ) ;
#27697 = CARTESIAN_POINT ( 'NONE',  ( 0.01688885742777274449, -6.535341423375596648, 4.680456609903981935 ) ) ;
#27698 = CARTESIAN_POINT ( 'NONE',  ( 86.62931800182293784, 20.48449268398422518, 2.867536982015617575 ) ) ;
#27699 = ADVANCED_FACE ( 'NONE', ( #760 ), #65131, .T. ) ;
#27700 = LINE ( 'NONE', #60758, #8329 ) ;
#27701 = CARTESIAN_POINT ( 'NONE',  ( 3.000000000000004441, 3.000000000000030198, -50.00000000000000000 ) ) ;
#27703 = ORIENTED_EDGE ( 'NONE', *, *, #60071, .T. ) ;
#27702 = CARTESIAN_POINT ( 'NONE',  ( 112.5612011511789916, 31.08353758940340583, 3.118228259027523652 ) ) ;
#27704 = LINE ( 'NONE', #1328, #20458 ) ;
#27705 = ORIENTED_EDGE ( 'NONE', *, *, #11890, .F. ) ;
#27706 = VERTEX_POINT ( 'NONE', #40473 ) ;
#27707 = VECTOR ( 'NONE', #12263, 1000.000000000000000 ) ;
#27708 = CARTESIAN_POINT ( 'NONE',  ( -124.2579583355759212, 45.42576894968487267, -88.77160920751813933 ) ) ;
#27709 = ADVANCED_FACE ( 'NONE', ( #18683 ), #61918, .F. ) ;
#27710 = CARTESIAN_POINT ( 'NONE',  ( -37.62144393131467268, 11.71252597733099421, -92.23831152112933296 ) ) ;
#27712 = ORIENTED_EDGE ( 'NONE', *, *, #55999, .T. ) ;
#27711 = CARTESIAN_POINT ( 'NONE',  ( 149.9714610887121751, 53.28792066194168342, 9.757508091027073505 ) ) ;
#27713 = DIRECTION ( 'NONE',  ( 0.000000000000000000, 0.000000000000000000, 1.000000000000000000 ) ) ;
#27714 = CARTESIAN_POINT ( 'NONE',  ( 57.30278335769541087, 48.40406511297401693, 170.0000000000000000 ) ) ;
#27715 = CARTESIAN_POINT ( 'NONE',  ( -78.66644367742109978, 23.39876645725290061, -35.11545063171788428 ) ) ;
#27716 = VECTOR ( 'NONE', #57131, 1000.000000000000000 ) ;
#27717 = EDGE_LOOP ( 'NONE', ( #22835, #177, #59982, #27070 ) ) ;
#27718 = CARTESIAN_POINT ( 'NONE',  ( 313.9975424824652350, 179.2896996249788799, 369.5505932007772003 ) ) ;
#27719 = CIRCLE ( 'NONE', #53569, 60.00000000000000000 ) ;
#27720 = FACE_OUTER_BOUND ( 'NONE', #30096, .T. ) ;
#27721 = AXIS2_PLACEMENT_3D ( 'NONE', #26350, #41835, #25325 ) ;
#27722 = CARTESIAN_POINT ( 'NONE',  ( -35.99019277275120032, 10.38248800679341777, -9.991386557961455139 ) ) ;
#27723 = LINE ( 'NONE', #6972, #11157 ) ;
#27724 = CARTESIAN_POINT ( 'NONE',  ( 128.4157044224114372, 39.39296260757095780, 58.67006427216110609 ) ) ;
#27725 = CARTESIAN_POINT ( 'NONE',  ( 15.78827728214693771, 7.507518794609574719, 71.85925826316895382 ) ) ;
#27726 = ORIENTED_EDGE ( 'NONE', *, *, #34770, .F. ) ;
#27727 = B_SPLINE_CURVE_WITH_KNOTS ( 'NONE', 3,
 ( #55736, #44114, #38505, #33940, #1224, #64899, #7563, #49738, #7199, #12132, #39214, #50111, #16697, #27598, #60312, #33595, #65962, #12477, #6844, #28659, #880, #28299, #59950, #44482, #55375, #33245, #1940, #23397, #18103, #66315, #38152, #11412, #32883, #54317, #40588, #30047, #67343, #19834, #19134, #34978, #45872, #35319, #41291, #8242, #46206, #2281 ),
 .UNSPECIFIED., .F., .F.,
 ( 4, 2, 2, 2, 2, 2, 2, 2, 2, 2, 2, 2, 2, 2, 2, 2, 2, 2, 2, 2, 2, 2, 4 ),
 ( 6.938893903907228378E-18, 0.001615199098318979148, 0.003230398196637951358, 0.004037997745797443534, 0.004845597294956941782, 0.006460796393275941747, 0.007268395942435461679, 0.008075995491594980744, 0.009691194589913980709, 0.01049879413907351539, 0.01130639368823305180, 0.01211399323739258647, 0.01292159278655212115, 0.01453679188487114887, 0.01615199098319018006, 0.01695959053234967484, 0.01776719008150916962, 0.01938238917982816265, 0.02099758827814715567, 0.02180518782730661922, 0.02261278737646608278, 0.02422798647478500988, 0.02584318557310393699 ),
 .UNSPECIFIED. ) ;
#27728 = ORIENTED_EDGE ( 'NONE', *, *, #10618, .F. ) ;
#27729 = ORIENTED_EDGE ( 'NONE', *, *, #44037, .T. ) ;
#27730 = CARTESIAN_POINT ( 'NONE',  ( 109.9975424824652777, 172.0000000000000284, 418.0000000000000000 ) ) ;
#27731 = FACE_OUTER_BOUND ( 'NONE', #30142, .T. ) ;
#27732 = CARTESIAN_POINT ( 'NONE',  ( -38.89042640463650002, 10.93374343663409753, -41.82923595654042259 ) ) ;
#27733 = CARTESIAN_POINT ( 'NONE',  ( -106.2787154433887764, 34.85886827088950213, 85.35571367539338894 ) ) ;
#27734 = CARTESIAN_POINT ( 'NONE',  ( -6.802008071587034799, -24.18409554641273473, 0.000000000000000000 ) ) ;
#27735 = DIRECTION ( 'NONE',  ( -1.000000000000000000, -0.000000000000000000, -0.000000000000000000 ) ) ;
#27736 = CARTESIAN_POINT ( 'NONE',  ( -48.35591483259475609, 14.02198755119445117, 88.11419938166893928 ) ) ;
#27737 = CARTESIAN_POINT ( 'NONE',  ( 79.22946426532583075, 17.02750615740070472, 62.80933842788154209 ) ) ;
#27738 = ORIENTED_EDGE ( 'NONE', *, *, #37321, .F. ) ;
#27739 = DIRECTION ( 'NONE',  ( -0.7071067811865474617, -9.058225723175622340E-16, 0.7071067811865474617 ) ) ;
#27740 = ORIENTED_EDGE ( 'NONE', *, *, #28997, .T. ) ;
#27741 = PRESENTATION_STYLE_ASSIGNMENT (( #16499 ) ) ;
#27742 = CARTESIAN_POINT ( 'NONE',  ( 188.4359598230020651, 86.36951380984523041, 35.29673132375548050 ) ) ;
#27743 = B_SPLINE_CURVE_WITH_KNOTS ( 'NONE', 3,
 ( #64956, #58967, #5166, #69518 ),
 .UNSPECIFIED., .F., .F.,
 ( 4, 4 ),
 ( 0.1259919275528358085, 0.1829744153748746882 ),
 .UNSPECIFIED. ) ;
#27744 = CARTESIAN_POINT ( 'NONE',  ( -3.000000000000003997, 23.97499999999999787, 0.000000000000000000 ) ) ;
#27745 = CARTESIAN_POINT ( 'NONE',  ( -75.64857587248467041, 21.19501514561448019, 17.94384578064662250 ) ) ;
#27746 = CARTESIAN_POINT ( 'NONE',  ( -34.34971582436550364, 10.08696685283320704, -89.58086001246577723 ) ) ;
#27747 = CARTESIAN_POINT ( 'NONE',  ( 20.36233635256088448, 7.697399815318437533, 31.55093273888049410 ) ) ;
#27748 = DIRECTION ( 'NONE',  ( 1.000000000000000000, -0.000000000000000000, 0.000000000000000000 ) ) ;
#27749 = CARTESIAN_POINT ( 'NONE',  ( -1.313474075707243838, -8.479269695850868871, -9.183279549040152645 ) ) ;
#27750 = EDGE_LOOP ( 'NONE', ( #45033, #62976, #44867, #5639 ) ) ;
#27751 = EDGE_CURVE ( 'NONE', #49232, #9677, #48879, .T. ) ;
#27752 = AXIS2_PLACEMENT_3D ( 'NONE', #29958, #7111, #51420 ) ;
#27753 = CARTESIAN_POINT ( 'NONE',  ( 64.52696037203369883, -10.43950074664762440, 43.58025477438756212 ) ) ;
#27754 = CARTESIAN_POINT ( 'NONE',  ( -62.31345272479883590, -18.49415068377726357, 40.00000000000003553 ) ) ;
#27755 = ORIENTED_EDGE ( 'NONE', *, *, #61464, .F. ) ;
#27756 = FACE_OUTER_BOUND ( 'NONE', #61842, .T. ) ;
#27757 = FILL_AREA_STYLE_COLOUR ( '', #35317 ) ;
#27758 = ORIENTED_EDGE ( 'NONE', *, *, #64498, .T. ) ;
#27759 = CARTESIAN_POINT ( 'NONE',  ( -78.66644367742109978, 22.32174330031319442, 30.41820113967310490 ) ) ;
#27760 = CARTESIAN_POINT ( 'NONE',  ( 155.2992895652387517, 57.24699634758577815, -77.66147854539327966 ) ) ;
#27761 = CARTESIAN_POINT ( 'NONE',  ( 45.35146934743634262, 10.27620685439442205, 42.00691914349181388 ) ) ;
#27762 = VECTOR ( 'NONE', #31921, 1000.000000000000000 ) ;
#27763 = DIRECTION ( 'NONE',  ( -0.000000000000000000, -0.000000000000000000, -1.000000000000000000 ) ) ;
#27764 = B_SPLINE_CURVE_WITH_KNOTS ( 'NONE', 3,
 ( #14776, #58369, #42545, #20394, #15812, #5258, #10183, #47463, #48148, #57351, #46789, #31644, #64000, #15129, #58037, #68261, #30622, #20064, #20747, #29998, #64340, #63668, #9858, #41517, #31316, #53082, #52417, #21429, #4912, #36241, #9162, #52742, #57698, #9508, #4568, #26378, #26032, #68922, #42207, #30971, #47816, #4234, #69276, #58707 ),
 .UNSPECIFIED., .F., .F.,
 ( 4, 2, 2, 2, 2, 2, 2, 2, 2, 2, 2, 2, 2, 2, 2, 2, 2, 2, 2, 2, 2, 4 ),
 ( 0.000000000000000000, 0.001482469635030009411, 0.002223704452545014875, 0.002964939270060020123, 0.004447408905090030617, 0.005929878540120041112, 0.007412348175150052475, 0.008153582992665062493, 0.008894817810180075113, 0.01037728744521010382, 0.01185975708024013600, 0.01260099189775512954, 0.01334222671527012308, 0.01482469635030015179, 0.01556593116781516094, 0.01630716598533017009, 0.01778963562036014676, 0.01927210525539012342, 0.02001334007290511002, 0.02075457489042010009, 0.02223704452545009758, 0.02371951416048009159 ),
 .UNSPECIFIED. ) ;
#27765 = CARTESIAN_POINT ( 'NONE',  ( -149.5074843970971017, 64.17983161892347255, 18.87627064943540134 ) ) ;
#27766 = VECTOR ( 'NONE', #3633, 1000.000000000000000 ) ;
#27767 = ORIENTED_EDGE ( 'NONE', *, *, #19229, .F. ) ;
#27768 = VERTEX_POINT ( 'NONE', #23616 ) ;
#27769 = DIRECTION ( 'NONE',  ( 0.000000000000000000, 0.000000000000000000, 1.000000000000000000 ) ) ;
#27770 = AXIS2_PLACEMENT_3D ( 'NONE', #15607, #62763, #63452 ) ;
#27771 = ORIENTED_EDGE ( 'NONE', *, *, #63600, .T. ) ;
#27772 = DIRECTION ( 'NONE',  ( 0.000000000000000000, -0.000000000000000000, 1.000000000000000000 ) ) ;
#27773 = CARTESIAN_POINT ( 'NONE',  ( 0.000000000000000000, 0.000000000000000000, 0.000000000000000000 ) ) ;
#27774 = CARTESIAN_POINT ( 'NONE',  ( 57.07734607129820148, 11.37318329671159844, 59.55008699787213544 ) ) ;
#27775 = CARTESIAN_POINT ( 'NONE',  ( 140.5011603602752359, 46.78412964631613136, 87.20346307703584898 ) ) ;
#27776 = VECTOR ( 'NONE', #37961, 1000.000000000000000 ) ;
#27777 = B_SPLINE_CURVE_WITH_KNOTS ( 'NONE', 3,
 ( #29064, #44167, #38921, #55075, #2329, #56835, #13912, #14602, #67055, #13569, #29744, #46607, #50852, #14266, #18848, #35027, #8648, #30101, #56474, #46960, #45924, #8297 ),
 .UNSPECIFIED., .F., .F.,
 ( 4, 2, 2, 2, 2, 2, 2, 2, 2, 2, 4 ),
 ( 8.002322828458971877E-17, 0.001318139496345188981, 0.001977209244517727418, 0.002636278992690265204, 0.003954418489035351619, 0.005272557985380436733, 0.005931627733553000541, 0.006590697481725565215, 0.007908836978070717116, 0.009226976474415867283, 0.01054511597076101918 ),
 .UNSPECIFIED. ) ;
#27778 = CARTESIAN_POINT ( 'NONE',  ( 50.98853755884136518, 400.0000000000071054, 96.05029585798814651 ) ) ;
#27779 = EDGE_CURVE ( 'NONE', #15703, #60845, #19715, .T. ) ;
#27780 = CARTESIAN_POINT ( 'NONE',  ( 109.9975424824652634, 18.00000000000002842, 256.8908838121927261 ) ) ;
#27781 = CIRCLE ( 'NONE', #17654, 243.4957430088094839 ) ;
#27782 = ORIENTED_EDGE ( 'NONE', *, *, #58215, .T. ) ;
#27783 = CARTESIAN_POINT ( 'NONE',  ( -31.11269837220804035, 15.55634918610408945, 2.000000000000001776 ) ) ;
#27784 = EDGE_LOOP ( 'NONE', ( #2323, #3768, #27832, #17997 ) ) ;
#27785 = ORIENTED_EDGE ( 'NONE', *, *, #23355, .F. ) ;
#27786 = LINE ( 'NONE', #5293, #61513 ) ;
#27787 = CARTESIAN_POINT ( 'NONE',  ( -64.97888516016270444, -7.103257987406331964, 43.58025477438756212 ) ) ;
#27788 = CARTESIAN_POINT ( 'NONE',  ( -172.3018509397888067, 86.22053936367346694, -7.900706070936963421 ) ) ;
#27789 = CARTESIAN_POINT ( 'NONE',  ( 134.3182571105338923, 42.88121222759019702, 17.66579024853170665 ) ) ;
#27790 = EDGE_CURVE ( 'NONE', #11928, #65701, #25005, .T. ) ;
#27791 = CARTESIAN_POINT ( 'NONE',  ( -16.35146342289083776, -18.91109843266265500, 0.000000000000000000 ) ) ;
#27792 = ORIENTED_EDGE ( 'NONE', *, *, #32326, .F. ) ;
#27793 = CARTESIAN_POINT ( 'NONE',  ( 85.67138972405899722, 19.09593469918313957, 2.913603581539713883 ) ) ;
#27794 = EDGE_LOOP ( 'NONE', ( #2452, #57041, #27012, #4862 ) ) ;
#27795 = CARTESIAN_POINT ( 'NONE',  ( -71.37402418445425667, 19.67651958824262337, 36.14765569274855039 ) ) ;
#27796 = ORIENTED_EDGE ( 'NONE', *, *, #58489, .T. ) ;
#27797 = DIRECTION ( 'NONE',  ( 1.000000000000000000, 0.000000000000000000, 0.000000000000000000 ) ) ;
#27798 = EDGE_CURVE ( 'NONE', #22360, #34775, #29236, .T. ) ;
#27799 = ORIENTED_EDGE ( 'NONE', *, *, #54559, .T. ) ;
#27800 = DIRECTION ( 'NONE',  ( -0.000000000000000000, -0.000000000000000000, -1.000000000000000000 ) ) ;
#27801 = EDGE_CURVE ( 'NONE', #26090, #52456, #34320, .T. ) ;
#27802 = CARTESIAN_POINT ( 'NONE',  ( 91.49345572560149265, 21.13836538408682841, 4.653589174503819592 ) ) ;
#27803 = PLANE ( 'NONE',  #28332 ) ;
#27804 = ORIENTED_EDGE ( 'NONE', *, *, #9056, .F. ) ;
#27805 = VECTOR ( 'NONE', #14229, 1000.000000000000000 ) ;
#27806 = LINE ( 'NONE', #49245, #64888 ) ;
#27807 =( NAMED_UNIT ( * ) PLANE_ANGLE_UNIT ( ) SI_UNIT ( $, .RADIAN. ) );
#27808 = CIRCLE ( 'NONE', #6481, 25.12245591505646303 ) ;
#27809 = DIRECTION ( 'NONE',  ( -0.000000000000000000, -0.000000000000000000, -1.000000000000000000 ) ) ;
#27810 = DIRECTION ( 'NONE',  ( 1.156482317317871232E-16, -3.126709176169244633E-16, 1.000000000000000000 ) ) ;
#27811 = CARTESIAN_POINT ( 'NONE',  ( -132.8123438040339863, 51.22132183644643533, -12.66178842039164643 ) ) ;
#27812 = DIRECTION ( 'NONE',  ( 0.000000000000000000, 0.000000000000000000, 1.000000000000000000 ) ) ;
#27813 = LINE ( 'NONE', #17251, #6907 ) ;
#27814 = ORIENTED_EDGE ( 'NONE', *, *, #37497, .F. ) ;
#27815 = CARTESIAN_POINT ( 'NONE',  ( 138.2136629441929188, 45.30947856186676148, -76.49082427909780790 ) ) ;
#27816 = VECTOR ( 'NONE', #59261, 1000.000000000000000 ) ;
#27817 = CARTESIAN_POINT ( 'NONE',  ( 0.000000000000000000, 0.000000000000000000, 2.499999999999999556 ) ) ;
#27818 = ORIENTED_EDGE ( 'NONE', *, *, #20727, .T. ) ;
#27819 = FACE_BOUND ( 'NONE', #59372, .T. ) ;
#27820 = CONICAL_SURFACE ( 'NONE', #50284, 74.95140232871122521, 0.8777644062502172329 ) ;
#27821 = CARTESIAN_POINT ( 'NONE',  ( -1.857619870843140397, 6.575690665396234813, -65.19364777147656298 ) ) ;
#27822 = CARTESIAN_POINT ( 'NONE',  ( -180.4651598106648294, 97.28730001475651079, 66.71784663132508797 ) ) ;
#27823 = CARTESIAN_POINT ( 'NONE',  ( -146.5309471467636797, 62.99917515507674892, -8.580487756379419295 ) ) ;
#27824 = LINE ( 'NONE', #21495, #14338 ) ;
#27825 = DIRECTION ( 'NONE',  ( -0.000000000000000000, 1.000000000000000000, -0.000000000000000000 ) ) ;
#27826 = DIRECTION ( 'NONE',  ( 1.000000000000000000, 0.000000000000000000, 0.000000000000000000 ) ) ;
#27827 = CARTESIAN_POINT ( 'NONE',  ( 113.7642062731436141, 21.75126402171896345, -3.307110067226746608 ) ) ;
#27828 = CARTESIAN_POINT ( 'NONE',  ( -119.9771613955297198, 43.90337778233483590, -73.87421532651727318 ) ) ;
#27829 = CARTESIAN_POINT ( 'NONE',  ( -13.29455179262033226, 8.319166883236665200, 32.47767114274684985 ) ) ;
#27830 = CARTESIAN_POINT ( 'NONE',  ( 157.4703587214989113, 57.65129005721576050, 17.56491688178971700 ) ) ;
#27831 = CARTESIAN_POINT ( 'NONE',  ( 44.17331380303619426, 10.09560889695571895, -91.01863521069090268 ) ) ;
#27832 = ORIENTED_EDGE ( 'NONE', *, *, #9282, .T. ) ;
#27833 = AXIS2_PLACEMENT_3D ( 'NONE', #38732, #28525, #1444 ) ;
#27834 = DIRECTION ( 'NONE',  ( -0.8532989592251507549, 0.000000000000000000, 0.5214219847544545594 ) ) ;
#27835 = VERTEX_POINT ( 'NONE', #61593 ) ;
#27836 = CARTESIAN_POINT ( 'NONE',  ( 60.58000000000000540, -36.09918303830819752, 20.41169613715280207 ) ) ;
#27837 = CARTESIAN_POINT ( 'NONE',  ( 84.05289558242220949, 19.61733656419351135, -77.21376866862176769 ) ) ;
#27838 = CARTESIAN_POINT ( 'NONE',  ( 115.0394167068075149, 32.28558853680154783, 85.02507986354113712 ) ) ;
#27839 = DIRECTION ( 'NONE',  ( -0.000000000000000000, -0.000000000000000000, 1.000000000000000000 ) ) ;
#27840 = CARTESIAN_POINT ( 'NONE',  ( 141.9165763529819344, 192.0000000000000000, 108.9999999999999858 ) ) ;
#27841 = CARTESIAN_POINT ( 'NONE',  ( -59.89379335984725117, 45.06047301136835870, 41.38025477438755928 ) ) ;
#27842 = CARTESIAN_POINT ( 'NONE',  ( -54.08488990389050599, 15.46443908526321920, -77.01379507922334255 ) ) ;
#27843 = EDGE_CURVE ( 'NONE', #7110, #25478, #51389, .T. ) ;
#27844 = CARTESIAN_POINT ( 'NONE',  ( -72.84536430560291365, 21.25605944016604809, -91.57030382287797465 ) ) ;
#27845 = CARTESIAN_POINT ( 'NONE',  ( -119.6801029354224966, 43.71909921132878196, -19.77672661693413403 ) ) ;
#27846 = ORIENTED_EDGE ( 'NONE', *, *, #18911, .T. ) ;
#27847 = EDGE_LOOP ( 'NONE', ( #58208, #22037, #5806, #17721 ) ) ;
#27848 = CARTESIAN_POINT ( 'NONE',  ( 39.40195752203891999, 9.424259417798145577, 71.75838489642698903 ) ) ;
#27849 = CARTESIAN_POINT ( 'NONE',  ( 0.000000000000000000, 0.000000000000000000, 3.469446951953614189E-15 ) ) ;
#27850 = EDGE_CURVE ( 'NONE', #11578, #27916, #3354, .T. ) ;
#27851 = DIRECTION ( 'NONE',  ( -0.000000000000000000, -0.000000000000000000, -1.000000000000000000 ) ) ;
#27852 = CARTESIAN_POINT ( 'NONE',  ( -95.54114085644955878, -170.0000000000000000, 94.99999999999866418 ) ) ;
#27853 = ORIENTED_EDGE ( 'NONE', *, *, #29123, .F. ) ;
#27854 = CARTESIAN_POINT ( 'NONE',  ( 107.9342863085848450, 28.93180871323605885, -50.57385741719785699 ) ) ;
#27855 = CARTESIAN_POINT ( 'NONE',  ( -11.14880195267006435, 7.129907723790824825, 71.20152023141297093 ) ) ;
#27856 = CARTESIAN_POINT ( 'NONE',  ( -78.66644367742111399, 22.32174330031316956, -8.270900041254197532 ) ) ;
#27857 = DIRECTION ( 'NONE',  ( -0.000000000000000000, -0.000000000000000000, -1.000000000000000000 ) ) ;
#27858 = CARTESIAN_POINT ( 'NONE',  ( 40.38414441725701209, 8.538832720399536669, -8.823556192051034586 ) ) ;
#27859 = CARTESIAN_POINT ( 'NONE',  ( 1.005827167100601827, 0.000000000000000000, -9.949286995052577964 ) ) ;
#27860 = FACE_BOUND ( 'NONE', #42008, .T. ) ;
#27861 = EDGE_CURVE ( 'NONE', #58622, #66845, #43263, .T. ) ;
#27862 = CARTESIAN_POINT ( 'NONE',  ( -60.13226458141420494, 16.10241298991027392, -37.19286980334710790 ) ) ;
#27863 = ADVANCED_FACE ( 'NONE', ( #63321 ), #25357, .T. ) ;
#27864 = VECTOR ( 'NONE', #18091, 1000.000000000000000 ) ;
#27865 = EDGE_CURVE ( 'NONE', #47842, #45708, #27764, .T. ) ;
#27866 = VERTEX_POINT ( 'NONE', #25699 ) ;
#27867 = AXIS2_PLACEMENT_3D ( 'NONE', #2283, #45876, #67690 ) ;
#27868 = FACE_OUTER_BOUND ( 'NONE', #49295, .T. ) ;
#27869 = CARTESIAN_POINT ( 'NONE',  ( 93.32228019177711076, 22.88890999585039765, -46.71524922504401900 ) ) ;
#27870 = DIRECTION ( 'NONE',  ( -0.000000000000000000, -0.000000000000000000, -1.000000000000000000 ) ) ;
#27871 = CARTESIAN_POINT ( 'NONE',  ( -180.5200658187032161, 97.35517482626558206, 10.21020346323557604 ) ) ;
#27872 = ADVANCED_FACE ( 'NONE', ( #10524 ), #42871, .T. ) ;
#27873 = CARTESIAN_POINT ( 'NONE',  ( 212.1488570093001442, 119.0116247937291689, 62.68074259173258866 ) ) ;
#27874 = CARTESIAN_POINT ( 'NONE',  ( -31.11269837220801193, 31.11269837220812207, 0.000000000000000000 ) ) ;
#27875 = AXIS2_PLACEMENT_3D ( 'NONE', #43026, #43379, #59897 ) ;
#27876 = EDGE_LOOP ( 'NONE', ( #37829, #10159 ) ) ;
#27877 = PLANE ( 'NONE',  #1115 ) ;
#27878 = CARTESIAN_POINT ( 'NONE',  ( -62.49130718206700408, 16.80297926264070085, 63.67143424412796548 ) ) ;
#27879 = ORIENTED_EDGE ( 'NONE', *, *, #57085, .F. ) ;
#27880 = CIRCLE ( 'NONE', #42496, 243.4957430088094839 ) ;
#27881 = ORIENTED_EDGE ( 'NONE', *, *, #18646, .F. ) ;
#27882 = CARTESIAN_POINT ( 'NONE',  ( -20.63749999999999929, 0.000000000000000000, -21.50000000000000000 ) ) ;
#27883 = CARTESIAN_POINT ( 'NONE',  ( 47.73902449249074920, -57.85799893277823713, 170.0000000000000000 ) ) ;
#27884 = CARTESIAN_POINT ( 'NONE',  ( 103.5839822277949764, 25.92130892112108143, 40.57116130282916799 ) ) ;
#27886 = ORIENTED_EDGE ( 'NONE', *, *, #28862, .T. ) ;
#27885 = EDGE_CURVE ( 'NONE', #50879, #45198, #42186, .T. ) ;
#27887 = ORIENTED_EDGE ( 'NONE', *, *, #51784, .F. ) ;
#27888 = DIRECTION ( 'NONE',  ( -0.000000000000000000, 1.000000000000000000, -0.000000000000000000 ) ) ;
#27889 = EDGE_CURVE ( 'NONE', #34656, #12108, #49896, .T. ) ;
#27891 = EDGE_CURVE ( 'NONE', #51413, #37758, #11554, .T. ) ;
#27890 = DIRECTION ( 'NONE',  ( -0.000000000000000000, -0.000000000000000000, -1.000000000000000000 ) ) ;
#27892 = EDGE_CURVE ( 'NONE', #44947, #2893, #66917, .T. ) ;
#27893 = CARTESIAN_POINT ( 'NONE',  ( 105.8229724512851391, 27.98935528750254065, 4.202583732138563732 ) ) ;
#27894 = DIRECTION ( 'NONE',  ( -7.596454196607838998E-65, 3.469446951953615421E-17, -1.000000000000000000 ) ) ;
#27895 = CARTESIAN_POINT ( 'NONE',  ( 92.21267147730743829, 21.40196534721315302, 42.24347036755128926 ) ) ;
#27896 = CARTESIAN_POINT ( 'NONE',  ( 103.5589117581614573, 27.00490790413960696, -13.13767299798190713 ) ) ;
#27897 = CARTESIAN_POINT ( 'NONE',  ( -47.94960849910471978, 13.92522873833624963, 13.43034332784529994 ) ) ;
#27898 = CARTESIAN_POINT ( 'NONE',  ( -8.679044977515172121, 7.955195573549007193, -89.10717191287118055 ) ) ;
#27899 = CARTESIAN_POINT ( 'NONE',  ( -156.8684223695132971, 72.05296926946580527, -94.46708670589811163 ) ) ;
#27900 = CARTESIAN_POINT ( 'NONE',  ( 63.01563776193091826, 12.67277567978495512, -89.40979201309708913 ) ) ;
#27901 = CARTESIAN_POINT ( 'NONE',  ( 92.99453320039974358, 21.69191284572291778, 86.92040988721714712 ) ) ;
#27903 = ORIENTED_EDGE ( 'NONE', *, *, #69525, .T. ) ;
#27902 = PLANE ( 'NONE',  #32109 ) ;
#27904 = EDGE_LOOP ( 'NONE', ( #13589, #45281, #6791, #68277, #16195, #10976 ) ) ;
#27905 = ORIENTED_EDGE ( 'NONE', *, *, #4740, .T. ) ;
#27906 = CARTESIAN_POINT ( 'NONE',  ( -11.57931195747592668, 7.164335452024273465, -9.562147327756052917 ) ) ;
#27907 = CARTESIAN_POINT ( 'NONE',  ( -51.13073217147958616, 13.66490163179656925, 44.21480333522377748 ) ) ;
#27908 = LINE ( 'NONE', #53235, #59198 ) ;
#27909 = PLANE ( 'NONE',  #47841 ) ;
#27910 = CARTESIAN_POINT ( 'NONE',  ( -37.93983213483218719, 11.77368372188051282, 68.33345614380237976 ) ) ;
#27911 = DIRECTION ( 'NONE',  ( -0.3754025596372949636, 0.9268618657695261165, 0.000000000000000000 ) ) ;
#27912 = CARTESIAN_POINT ( 'NONE',  ( -76.32962633615588288, 21.44528079176261670, -76.59068498040936390 ) ) ;
#27913 = CARTESIAN_POINT ( 'NONE',  ( 22.53041628628729853, 6.810083298012986397, -12.85235912044543127 ) ) ;
#27914 = ORIENTED_EDGE ( 'NONE', *, *, #27850, .T. ) ;
#27915 = PLANE ( 'NONE',  #42989 ) ;
#27916 = VERTEX_POINT ( 'NONE', #6994 ) ;
#27917 = ORIENTED_EDGE ( 'NONE', *, *, #20307, .F. ) ;
#27918 = AXIS2_PLACEMENT_3D ( 'NONE', #54773, #1318, #38604 ) ;
#27919 = LINE ( 'NONE', #49007, #24231 ) ;
#27920 = CARTESIAN_POINT ( 'NONE',  ( -27.20808966803983608, 9.951893639754503695, 85.20453094359582735 ) ) ;
#27921 = CARTESIAN_POINT ( 'NONE',  ( -97.49219489034500441, 30.41416107059310647, -48.30800170384669912 ) ) ;
#27922 = CIRCLE ( 'NONE', #49242, 5.000000000000004441 ) ;
#27923 = DIRECTION ( 'NONE',  ( -0.2225209339563184452, 0.9749279121818226201, 0.000000000000000000 ) ) ;
#27924 = DIRECTION ( 'NONE',  ( -0.000000000000000000, -0.000000000000000000, -1.000000000000000000 ) ) ;
#27925 = CARTESIAN_POINT ( 'NONE',  ( -49.42000000000000171, -36.09918303830819752, 20.41169613715280207 ) ) ;
#27926 = VERTEX_POINT ( 'NONE', #677 ) ;
#27927 = ORIENTED_EDGE ( 'NONE', *, *, #42638, .T. ) ;
#27928 = EDGE_LOOP ( 'NONE', ( #68295, #57501, #39849, #49530 ) ) ;
#27929 = EDGE_CURVE ( 'NONE', #62528, #44589, #65395, .T. ) ;
#27930 = CARTESIAN_POINT ( 'NONE',  ( 412.3372781065085633, 179.4906275429376024, 111.5502958579881749 ) ) ;
#27931 = CARTESIAN_POINT ( 'NONE',  ( -153.6994314938755792, 69.16570456337670691, -9.232507601247755602 ) ) ;
#27932 = CARTESIAN_POINT ( 'NONE',  ( 37.46254810722765427, 8.164772623042710009, -77.22570432960662856 ) ) ;
#27933 = CARTESIAN_POINT ( 'NONE',  ( 62.52742438962777527, 12.55954017561948000, -8.876140241706055534 ) ) ;
#27934 = CARTESIAN_POINT ( 'NONE',  ( -33.37566357177431087, 9.916833145467595756, 57.29897744571702844 ) ) ;
#27935 = FACE_OUTER_BOUND ( 'NONE', #45959, .T. ) ;
#27936 = ORIENTED_EDGE ( 'NONE', *, *, #63523, .T. ) ;
#27937 = CARTESIAN_POINT ( 'NONE',  ( 188.2086267457324880, 87.61890531228281986, 61.29282024878416735 ) ) ;
#27938 = CARTESIAN_POINT ( 'NONE',  ( 410.0000000000000000, 190.0000000000000000, 0.000000000000000000 ) ) ;
#27939 = DIRECTION ( 'NONE',  ( -0.9933367378126704006, -0.1152481032888702378, 1.361317959652291287E-16 ) ) ;
#27940 = CARTESIAN_POINT ( 'NONE',  ( -0.3740447803642804048, 7.527031846085010081, -43.90199697603654272 ) ) ;
#27941 = CARTESIAN_POINT ( 'NONE',  ( -165.7699288023689235, 79.30174988963858596, 9.961564374601575622 ) ) ;
#27942 = CARTESIAN_POINT ( 'NONE',  ( 0.000000000000000000, 0.000000000000000000, 43.58025477438756212 ) ) ;
#27943 = FACE_BOUND ( 'NONE', #66060, .T. ) ;
#27944 = ADVANCED_FACE ( 'NONE', ( #23185 ), #16840, .F. ) ;
#27945 = CARTESIAN_POINT ( 'NONE',  ( 204.6977192012829505, 108.0580384837234931, 56.05227132923312183 ) ) ;
#27946 = CARTESIAN_POINT ( 'NONE',  ( 9.416603677636260272, 6.380307115728824030, -73.82726956336668422 ) ) ;
#27947 = EDGE_CURVE ( 'NONE', #11659, #5640, #38656, .T. ) ;
#27948 = EDGE_CURVE ( 'NONE', #58197, #59365, #66967, .T. ) ;
#27949 = EDGE_CURVE ( 'NONE', #17425, #21145, #19800, .T. ) ;
#27950 = EDGE_LOOP ( 'NONE', ( #42788, #58196 ) ) ;
#27951 = CYLINDRICAL_SURFACE ( 'NONE', #20353, 23.97499999999999787 ) ;
#27952 = CARTESIAN_POINT ( 'NONE',  ( 177.2011275744679324, 74.76848439756737719, 30.38803117832052791 ) ) ;
#27953 = PLANE ( 'NONE',  #46660 ) ;
#27954 = CARTESIAN_POINT ( 'NONE',  ( 40.38414441725700499, 8.538832720399511800, -62.51265737297843827 ) ) ;
#27955 = DIRECTION ( 'NONE',  ( -0.000000000000000000, -1.000000000000000000, -0.000000000000000000 ) ) ;
#27956 = ORIENTED_EDGE ( 'NONE', *, *, #32858, .T. ) ;
#27957 = VERTEX_POINT ( 'NONE', #16152 ) ;
#27958 = DIRECTION ( 'NONE',  ( -1.000000000000000000, -3.697785493223491743E-32, 0.000000000000000000 ) ) ;
#27959 = FACE_OUTER_BOUND ( 'NONE', #939, .T. ) ;
#27960 = ORIENTED_EDGE ( 'NONE', *, *, #34648, .F. ) ;
#27961 = EDGE_LOOP ( 'NONE', ( #60820, #46356, #10608, #40178 ) ) ;
#27962 = CARTESIAN_POINT ( 'NONE',  ( 173.7227242028391174, 71.47307702680404873, -45.18960647539945796 ) ) ;
#27963 = CARTESIAN_POINT ( 'NONE',  ( 0.000000000000000000, 2.999999999999969358, 0.000000000000000000 ) ) ;
#27964 = ORIENTED_EDGE ( 'NONE', *, *, #44143, .T. ) ;
#27966 = CARTESIAN_POINT ( 'NONE',  ( 63.01563776193090405, 12.67277567978497643, -8.876140241706053757 ) ) ;
#27965 = AXIS2_PLACEMENT_3D ( 'NONE', #43099, #52958, #53298 ) ;
#27967 = AXIS2_PLACEMENT_3D ( 'NONE', #7577, #15259, #9984 ) ;
#27968 = CARTESIAN_POINT ( 'NONE',  ( -7.825402957745085430, 6.891034867348157178, -8.573520141480125645 ) ) ;
#27969 = CARTESIAN_POINT ( 'NONE',  ( -78.18913509716432486, 22.13995206110505976, -35.11545063171788428 ) ) ;
#27970 = ADVANCED_FACE ( 'NONE', ( #53771 ), #39984, .T. ) ;
#27971 = CYLINDRICAL_SURFACE ( 'NONE', #34, 5.000000000000004441 ) ;
#27972 = CARTESIAN_POINT ( 'NONE',  ( -30.46358361599563480, 10.45190018822943578, -8.520521904715787187 ) ) ;
#27973 = CARTESIAN_POINT ( 'NONE',  ( -48.34500911884040875, 14.01939034823941377, -12.50755381913665687 ) ) ;
#27974 = EDGE_CURVE ( 'NONE', #20959, #62198, #31001, .T. ) ;
#27975 = ORIENTED_EDGE ( 'NONE', *, *, #36448, .T. ) ;
#27976 = CARTESIAN_POINT ( 'NONE',  ( 114.4640969196985907, 30.88424258798504596, -49.62645197922152107 ) ) ;
#27977 = FACE_BOUND ( 'NONE', #36095, .T. ) ;
#27978 = CARTESIAN_POINT ( 'NONE',  ( 43.96465529479667111, 9.046527005589345194, -49.09265818586762720 ) ) ;
#27979 = CARTESIAN_POINT ( 'NONE',  ( -167.0073208999198471, 82.02183861952782706, -73.40875188435131804 ) ) ;
#27981 = ORIENTED_EDGE ( 'NONE', *, *, #43344, .T. ) ;
#27980 = LINE ( 'NONE', #18480, #622 ) ;
#27982 = CARTESIAN_POINT ( 'NONE',  ( 57.57684776206770749, 12.50442334002048561, 5.298377812166513934 ) ) ;
#27983 = ORIENTED_EDGE ( 'NONE', *, *, #32393, .F. ) ;
#27984 = DIRECTION ( 'NONE',  ( 0.000000000000000000, 0.000000000000000000, 1.000000000000000000 ) ) ;
#27985 = DIRECTION ( 'NONE',  ( -4.573512162503992243E-19, 5.081588203714606302E-18, -1.000000000000000000 ) ) ;
#27986 = DIRECTION ( 'NONE',  ( 0.000000000000000000, 0.000000000000000000, 1.000000000000000000 ) ) ;
#27987 = CARTESIAN_POINT ( 'NONE',  ( 149.4165763529819344, 225.8585178651493663, 108.9999999999999858 ) ) ;
#27988 = CARTESIAN_POINT ( 'NONE',  ( 83.38067517854670996, 18.33799117207142260, -23.24128901785653412 ) ) ;
#27989 = CARTESIAN_POINT ( 'NONE',  ( 42.48820792780866640, 9.847387255477761059, 3.729320912837806201 ) ) ;
#27990 = CYLINDRICAL_SURFACE ( 'NONE', #10635, 7.500000000000020428 ) ;
#27991 = DIRECTION ( 'NONE',  ( 0.000000000000000000, 0.000000000000000000, 1.000000000000000000 ) ) ;
#27992 = CARTESIAN_POINT ( 'NONE',  ( -156.3850008295872556, 70.23964984807268763, -92.99996502729436543 ) ) ;
#27993 = ORIENTED_EDGE ( 'NONE', *, *, #60529, .F. ) ;
#27994 = ORIENTED_EDGE ( 'NONE', *, *, #2977, .F. ) ;
#27995 = CARTESIAN_POINT ( 'NONE',  ( 41.80536115778105710, 8.734184316430670947, 30.30514126477402570 ) ) ;
#27996 = DIRECTION ( 'NONE',  ( 0.000000000000000000, 1.000000000000000000, 0.000000000000000000 ) ) ;
#27997 = DIRECTION ( 'NONE',  ( 1.000000000000000000, 0.000000000000000000, 0.000000000000000000 ) ) ;
#27998 = AXIS2_PLACEMENT_3D ( 'NONE', #29468, #28070, #40371 ) ;
#27999 = CARTESIAN_POINT ( 'NONE',  ( -30.00000000000000355, -30.00000000000000355, 12.00000000000000000 ) ) ;
#28000 = CARTESIAN_POINT ( 'NONE',  ( 208.9585401441655961, 114.1617785893844257, -37.63730762774075345 ) ) ;
#28001 = CARTESIAN_POINT ( 'NONE',  ( -71.23176719684943237, 20.69188312694500098, -68.44020852477699179 ) ) ;
#28002 = CARTESIAN_POINT ( 'NONE',  ( -104.5730787903383145, 33.96058035148152499, 72.02022507236867455 ) ) ;
#28003 = CARTESIAN_POINT ( 'NONE',  ( -24.93568128341084034, 8.613819379861698877, -39.04933227581432220 ) ) ;
#28004 = PLANE ( 'NONE',  #64388 ) ;
#28006 = ORIENTED_EDGE ( 'NONE', *, *, #6584, .F. ) ;
#28005 = EDGE_CURVE ( 'NONE', #65415, #2294, #655, .T. ) ;
#28007 = CARTESIAN_POINT ( 'NONE',  ( -56.44201257846630426, 32.26641783793562723, 170.0000000000000000 ) ) ;
#28008 = VERTEX_POINT ( 'NONE', #28092 ) ;
#28009 = CARTESIAN_POINT ( 'NONE',  ( -22.50000000000000355, -17.50000000000000000, 20.00000000000000000 ) ) ;
#28010 = EDGE_CURVE ( 'NONE', #45699, #38702, #59403, .T. ) ;
#28011 = PLANE ( 'NONE',  #15081 ) ;
#28012 = DIRECTION ( 'NONE',  ( -1.000000000000000000, 0.000000000000000000, -0.000000000000000000 ) ) ;
#28013 = CARTESIAN_POINT ( 'NONE',  ( 132.0249343950657135, 41.49728247212332377, 44.34218584777070049 ) ) ;
#28014 = CARTESIAN_POINT ( 'NONE',  ( 10.55634918610403084, -3.079134169858832593E-14, 85.00100000000000477 ) ) ;
#28015 = AXIS2_PLACEMENT_3D ( 'NONE', #51531, #62426, #14243 ) ;
#28016 = DIRECTION ( 'NONE',  ( -1.954612056407539268E-16, -1.558751100573764160E-16, 1.000000000000000000 ) ) ;
#28017 = DIRECTION ( 'NONE',  ( -0.000000000000000000, 1.000000000000000000, -0.000000000000000000 ) ) ;
#28018 = CARTESIAN_POINT ( 'NONE',  ( -75.31295361348104223, 0.000000000000000000, -2.499999999999970246 ) ) ;
#28019 = CARTESIAN_POINT ( 'NONE',  ( 209.7190351965047057, 113.4909703304756903, 84.81773753047731645 ) ) ;
#28020 = DIRECTION ( 'NONE',  ( 0.000000000000000000, 0.000000000000000000, 1.000000000000000000 ) ) ;
#28021 = ORIENTED_EDGE ( 'NONE', *, *, #1668, .T. ) ;
#28022 = CARTESIAN_POINT ( 'NONE',  ( 57.39233401791017997, 12.46575990788836030, 69.14437610160888426 ) ) ;
#28023 = CARTESIAN_POINT ( 'NONE',  ( 10.13563904803031512, 7.391572367417534650, -64.90997110317320562 ) ) ;
#28024 = FACE_OUTER_BOUND ( 'NONE', #64026, .T. ) ;
#28025 = ADVANCED_FACE ( 'NONE', ( #54462, #6294 ), #17547, .T. ) ;
#28026 = LINE ( 'NONE', #13257, #17483 ) ;
#28027 = CARTESIAN_POINT ( 'NONE',  ( 10.55634918610396511, -46.66904755831214402, 0.000000000000000000 ) ) ;
#28028 = B_SPLINE_CURVE_WITH_KNOTS ( 'NONE', 3,
 ( #17673, #12394, #50022, #60922, #13438, #28570, #23646, #28929, #1856, #34206, #7815, #50380, #66230, #39819, #13098, #45438, #45086, #23992, #27871, #40166, #61623, #49310, #1142, #6762, #17313, #38784, #60231, #12044, #28211, #47159, #52104, #35587, #62310, #63004, #45791, #61954, #8510, #25391, #29604, #62667, #67268, #51423, #19054, #46824 ),
 .UNSPECIFIED., .F., .F.,
 ( 4, 2, 2, 2, 2, 2, 2, 2, 2, 2, 2, 2, 2, 2, 2, 2, 2, 2, 2, 2, 2, 4 ),
 ( 0.02908143158676660539, 0.03095422299093868179, 0.03282701439511075819, 0.03469980579928283460, 0.03657259720345491100, 0.03844538860762698740, 0.04031818001179907074, 0.04125457571388507771, 0.04219097141597108469, 0.04312736711805709861, 0.04359556496910010209, 0.04406376282014311252, 0.04500015852222912643, 0.04593655422431514035, 0.04687294992640115426, 0.04780934562848716818, 0.04968213703265923764, 0.05155492843683130710, 0.05342771984100337657, 0.05530051124517543909, 0.05717330264934750855, 0.05904609405351957108 ),
 .UNSPECIFIED. ) ;
#28029 = EDGE_CURVE ( 'NONE', #1594, #60452, #22474, .T. ) ;
#28030 = EDGE_CURVE ( 'NONE', #4856, #30419, #54821, .T. ) ;
#28031 = EDGE_LOOP ( 'NONE', ( #50504, #21134, #35510, #3528 ) ) ;
#28032 = DIRECTION ( 'NONE',  ( 1.000000000000000000, 0.000000000000000000, 0.000000000000000000 ) ) ;
#28033 = VECTOR ( 'NONE', #9404, 1000.000000000000000 ) ;
#28034 = CARTESIAN_POINT ( 'NONE',  ( 49.42891899764522634, -30.98851909993380360, 27.58472315868181113 ) ) ;
#28035 = DIRECTION ( 'NONE',  ( -0.000000000000000000, -1.000000000000000000, 0.000000000000000000 ) ) ;
#28036 = DIRECTION ( 'NONE',  ( 0.7071067811865475727, 0.000000000000000000, 0.7071067811865474617 ) ) ;
#28037 = ADVANCED_FACE ( 'NONE', ( #60460 ), #12274, .F. ) ;
#28038 = CONTEXT_DEPENDENT_SHAPE_REPRESENTATION ( #49840, #11302 ) ;
#28039 = CARTESIAN_POINT ( 'NONE',  ( -132.0738857626834601, 51.93126104279146205, -46.67044353618173602 ) ) ;
#28040 = EDGE_LOOP ( 'NONE', ( #27625, #68471, #58209, #19289 ) ) ;
#28041 = CARTESIAN_POINT ( 'NONE',  ( -118.9468627709229480, 42.08677365399180559, -39.57500987869580911 ) ) ;
#28042 = CARTESIAN_POINT ( 'NONE',  ( -442.6627218934912662, 394.9999999999998295, 113.5502958579882034 ) ) ;
#28043 = CARTESIAN_POINT ( 'NONE',  ( -142.6264002846224059, 58.55577336362198082, -18.46366008300287120 ) ) ;
#28044 = CARTESIAN_POINT ( 'NONE',  ( -142.5336480376679162, 58.48275793139958267, 94.69040015390055487 ) ) ;
#28045 = CARTESIAN_POINT ( 'NONE',  ( 0.000000000000000000, 0.000000000000000000, 40.00000000000003553 ) ) ;
#28046 = ORIENTED_EDGE ( 'NONE', *, *, #42848, .T. ) ;
#28047 = DIRECTION ( 'NONE',  ( -1.000000000000000000, 0.000000000000000000, 0.000000000000000000 ) ) ;
#28048 = CARTESIAN_POINT ( 'NONE',  ( 198.7029050523552485, 98.46895521196212542, -39.29008233195586541 ) ) ;
#28049 = PLANE ( 'NONE',  #59962 ) ;
#28050 = VECTOR ( 'NONE', #69179, 1000.000000000000000 ) ;
#28051 = DIRECTION ( 'NONE',  ( 0.8805955318567322276, 0.4738686624730095165, 2.500042656554810340E-16 ) ) ;
#28053 = ORIENTED_EDGE ( 'NONE', *, *, #44367, .T. ) ;
#28052 = CARTESIAN_POINT ( 'NONE',  ( -56.02358673658417132, 14.94347049174937503, 3.520221774332097375 ) ) ;
#28054 = EDGE_CURVE ( 'NONE', #40156, #20810, #66110, .T. ) ;
#28055 = CARTESIAN_POINT ( 'NONE',  ( 15.55634918610411610, 46.66904755831205875, 85.00100000000000477 ) ) ;
#28056 = ORIENTED_EDGE ( 'NONE', *, *, #65706, .F. ) ;
#28057 = ORIENTED_EDGE ( 'NONE', *, *, #27605, .F. ) ;
#28058 = CARTESIAN_POINT ( 'NONE',  ( -72.76696720809547969, 20.16136115364207981, -11.11340259104759554 ) ) ;
#28059 = LINE ( 'NONE', #17504, #15840 ) ;
#28061 = ORIENTED_EDGE ( 'NONE', *, *, #14636, .F. ) ;
#28060 = CARTESIAN_POINT ( 'NONE',  ( -15.13211202216340467, 8.488266782358831364, -71.47197618211744441 ) ) ;
#28062 = DIRECTION ( 'NONE',  ( -0.000000000000000000, -1.000000000000000000, -0.000000000000000000 ) ) ;
#28063 = CARTESIAN_POINT ( 'NONE',  ( 181.0840389613909451, 80.03940679743416808, -36.22505766587961062 ) ) ;
#28064 = VECTOR ( 'NONE', #42248, 1000.000000000000114 ) ;
#28065 = CARTESIAN_POINT ( 'NONE',  ( -430.1627218934918346, 399.9999999999952820, 91.05029585799256608 ) ) ;
#28066 = EDGE_LOOP ( 'NONE', ( #33861, #41036, #24091, #23812 ) ) ;
#28067 = DIRECTION ( 'NONE',  ( -0.000000000000000000, -0.000000000000000000, 1.000000000000000000 ) ) ;
#28068 = CARTESIAN_POINT ( 'NONE',  ( -38.84150381976579780, 10.92416363971238980, -17.20362598305740320 ) ) ;
#28069 = CARTESIAN_POINT ( 'NONE',  ( 151.7977579753110433, 53.37137838551321778, -92.38936414380266626 ) ) ;
#28070 = DIRECTION ( 'NONE',  ( -0.000000000000000000, 1.000000000000000000, -0.000000000000000000 ) ) ;
#28071 = CARTESIAN_POINT ( 'NONE',  ( 18.43272992546528499, 7.606837839440253823, 71.38188367849733140 ) ) ;
#28072 = VERTEX_POINT ( 'NONE', #34447 ) ;
#28073 = ORIENTED_EDGE ( 'NONE', *, *, #14607, .F. ) ;
#28074 = ORIENTED_EDGE ( 'NONE', *, *, #37219, .F. ) ;
#28075 = AXIS2_PLACEMENT_3D ( 'NONE', #23606, #45395, #66527 ) ;
#28076 = DIRECTION ( 'NONE',  ( 0.000000000000000000, -0.5000000000000007772, 0.8660254037844381525 ) ) ;
#28077 = CARTESIAN_POINT ( 'NONE',  ( -105.4487797565983840, 35.55724615608637862, 4.360698117697985765 ) ) ;
#28078 = EDGE_CURVE ( 'NONE', #16701, #34756, #7702, .T. ) ;
#28079 = CYLINDRICAL_SURFACE ( 'NONE', #3237, 5.000000000000004441 ) ;
#28080 = CARTESIAN_POINT ( 'NONE',  ( -38.93922791710217268, 10.94334660650242341, -43.05910848483384967 ) ) ;
#28081 = CARTESIAN_POINT ( 'NONE',  ( -42.02161712141799654, -16.09918303830819397, 30.00000000000000000 ) ) ;
#28082 = DIRECTION ( 'NONE',  ( -0.000000000000000000, 1.000000000000000000, -0.000000000000000000 ) ) ;
#28083 = DIRECTION ( 'NONE',  ( -1.000000000000000000, 0.000000000000000000, 0.000000000000000000 ) ) ;
#28084 = CARTESIAN_POINT ( 'NONE',  ( -78.18897186942403721, 23.21604822208489338, -8.270900041254201085 ) ) ;
#28085 = EDGE_CURVE ( 'NONE', #43922, #53047, #7353, .T. ) ;
#28086 = CARTESIAN_POINT ( 'NONE',  ( 80.30232379693109124, 17.35837133860834314, 60.02175339020114819 ) ) ;
#28087 = ORIENTED_EDGE ( 'NONE', *, *, #36274, .F. ) ;
#28088 = CARTESIAN_POINT ( 'NONE',  ( -71.96466849523049802, -21.15771699337099321, 170.0000000000000000 ) ) ;
#28089 = ADVANCED_FACE ( 'NONE', ( #14009 ), #50257, .F. ) ;
#28090 = ORIENTED_EDGE ( 'NONE', *, *, #5952, .T. ) ;
#28091 = CARTESIAN_POINT ( 'NONE',  ( 181.9295719569814196, 79.46350097013163349, 29.34415077797327953 ) ) ;
#28092 = CARTESIAN_POINT ( 'NONE',  ( 17.98081503251174240, -17.36923402935755689, 0.000000000000000000 ) ) ;
#28093 = CARTESIAN_POINT ( 'NONE',  ( -73.63346300764936814, 20.46798018699518806, 5.507808174618403996 ) ) ;
#28094 = CARTESIAN_POINT ( 'NONE',  ( -118.6302575928420424, 43.07263081214306055, 66.85160587967178003 ) ) ;
#28095 = ADVANCED_FACE ( 'NONE', ( #51310 ), #40733, .F. ) ;
#28096 = CARTESIAN_POINT ( 'NONE',  ( 26.99999999999999289, 29.99999999999999645, 15.00000000000000000 ) ) ;
#28097 = CIRCLE ( 'NONE', #24755, 20.00000000000000000 ) ;
#28098 = CARTESIAN_POINT ( 'NONE',  ( 154.6667526376337207, 55.50347409140649546, -36.66424293194626216 ) ) ;
#28099 = CARTESIAN_POINT ( 'NONE',  ( 0.000000000000000000, 50.00000000000000000, -5.000000000000000000 ) ) ;
#28100 = VERTEX_POINT ( 'NONE', #34087 ) ;
#28101 = DIRECTION ( 'NONE',  ( 1.000000000000000000, 0.000000000000000000, 0.000000000000000000 ) ) ;
#28102 = DIRECTION ( 'NONE',  ( 0.000000000000000000, -1.000000000000000000, -0.000000000000000000 ) ) ;
#28103 = ORIENTED_EDGE ( 'NONE', *, *, #22795, .F. ) ;
#28104 = CARTESIAN_POINT ( 'NONE',  ( -91.00000000000001421, 0.000000000000000000, 54.99999999999999289 ) ) ;
#28105 = DIRECTION ( 'NONE',  ( 1.000000000000000000, 0.000000000000000000, 0.000000000000000000 ) ) ;
#28106 = VERTEX_POINT ( 'NONE', #17901 ) ;
#28107 = CARTESIAN_POINT ( 'NONE',  ( -79.14678386417816114, 22.50468917936073154, 45.41820113967313688 ) ) ;
#28108 = CARTESIAN_POINT ( 'NONE',  ( -30.46002654261638298, 10.45132580906815356, -77.11350681613473057 ) ) ;
#28109 = CARTESIAN_POINT ( 'NONE',  ( 44.34689728705970424, 10.12166135033765357, 43.07394473429382487 ) ) ;
#28110 = CARTESIAN_POINT ( 'NONE',  ( -28.81317668042940383, 9.175023678939295380, 57.53151503497319652 ) ) ;
#28111 = ADVANCED_FACE ( 'NONE', ( #55523 ), #61835, .F. ) ;
#28112 = EDGE_CURVE ( 'NONE', #13050, #36317, #13326, .T. ) ;
#28113 = ORIENTED_EDGE ( 'NONE', *, *, #28676, .F. ) ;
#28114 = ORIENTED_EDGE ( 'NONE', *, *, #22313, .T. ) ;
#28115 = VECTOR ( 'NONE', #45195, 1000.000000000000000 ) ;
#28116 = DIRECTION ( 'NONE',  ( -0.000000000000000000, 0.000000000000000000, -1.000000000000000000 ) ) ;
#28117 = ORIENTED_EDGE ( 'NONE', *, *, #44658, .T. ) ;
#28118 = CARTESIAN_POINT ( 'NONE',  ( 36.30999198706538067, 9.040534725358945423, -9.437934728592482614 ) ) ;
#28119 = FACE_OUTER_BOUND ( 'NONE', #29051, .T. ) ;
#28120 = SURFACE_SIDE_STYLE ('',( #12300 ) ) ;
#28121 = CARTESIAN_POINT ( 'NONE',  ( -0.5783162822156577842, 7.534184941292926041, 66.40692524127545937 ) ) ;
#28122 = CARTESIAN_POINT ( 'NONE',  ( -24.26658464276621885, 9.538695081344586768, -94.14796338366534201 ) ) ;
#28123 = CARTESIAN_POINT ( 'NONE',  ( -71.96466849523049802, -21.15771699337099321, 170.0000000000000000 ) ) ;
#28124 = ORIENTED_EDGE ( 'NONE', *, *, #297, .F. ) ;
#28125 = CARTESIAN_POINT ( 'NONE',  ( 15.78827728214693416, 6.500811158483329244, 45.01470767270524931 ) ) ;
#28126 = ORIENTED_EDGE ( 'NONE', *, *, #23911, .T. ) ;
#28127 = ORIENTED_EDGE ( 'NONE', *, *, #51326, .T. ) ;
#28128 = CARTESIAN_POINT ( 'NONE',  ( 164.8942204024297951, 63.66138186734712434, -15.67721590130059717 ) ) ;
#28129 = CARTESIAN_POINT ( 'NONE',  ( -65.13282190615095146, -1.847197903505587038E-12, -5.000000000000000000 ) ) ;
#28130 = FACE_OUTER_BOUND ( 'NONE', #28244, .T. ) ;
#28131 = CARTESIAN_POINT ( 'NONE',  ( 138.1901928158493718, 45.29454828899443442, 16.30506375331225755 ) ) ;
#28132 = CARTESIAN_POINT ( 'NONE',  ( 447.3372781065085633, 399.9999999999998863, 78.55029585798817493 ) ) ;
#28133 = CIRCLE ( 'NONE', #49460, 25.12245591505646303 ) ;
#28134 = ORIENTED_EDGE ( 'NONE', *, *, #38264, .T. ) ;
#28135 = CARTESIAN_POINT ( 'NONE',  ( 81.74909803672913711, 17.81295302817861881, 4.650954357442839360 ) ) ;
#28136 = ORIENTED_EDGE ( 'NONE', *, *, #39362, .T. ) ;
#28137 = LINE ( 'NONE', #42593, #32847 ) ;
#28138 = EDGE_LOOP ( 'NONE', ( #33338, #801, #1106, #29452 ) ) ;
#28139 = DIRECTION ( 'NONE',  ( -0.9959742939952382912, -0.08963930890344087854, 0.000000000000000000 ) ) ;
#28140 = ORIENTED_EDGE ( 'NONE', *, *, #30818, .F. ) ;
#28141 = LINE ( 'NONE', #16550, #9504 ) ;
#28142 = AXIS2_PLACEMENT_3D ( 'NONE', #14013, #28813, #29492 ) ;
#28143 = CARTESIAN_POINT ( 'NONE',  ( 94.06703982324147262, 22.09435144471462920, 11.36492375468983340 ) ) ;
#28144 = LINE ( 'NONE', #44686, #46258 ) ;
#28145 = ORIENTED_EDGE ( 'NONE', *, *, #24565, .F. ) ;
#28146 = CARTESIAN_POINT ( 'NONE',  ( 44.99999999999995737, -22.99999999999998579, 4.000000000000000000 ) ) ;
#28147 = CARTESIAN_POINT ( 'NONE',  ( 58.97837225874348377, 12.80135346511094774, 84.67264224153834107 ) ) ;
#28148 = CARTESIAN_POINT ( 'NONE',  ( 34.45158752686798209, 8.829194381142002612, 43.06926157878825023 ) ) ;
#28149 = CARTESIAN_POINT ( 'NONE',  ( -178.2328124332056234, 94.56955476227571467, -47.72005399664082859 ) ) ;
#28150 = CARTESIAN_POINT ( 'NONE',  ( -180.3582430093886728, 97.15509181467152189, -93.85725392925826327 ) ) ;
#28151 = LINE ( 'NONE', #16213, #51399 ) ;
#28152 = CARTESIAN_POINT ( 'NONE',  ( 60.58000000000000540, -36.09918303830819752, 10.41169613715280740 ) ) ;
#28153 = EDGE_LOOP ( 'NONE', ( #3501, #51537, #30698, #52279 ) ) ;
#28154 = LINE ( 'NONE', #65820, #25353 ) ;
#28155 = CARTESIAN_POINT ( 'NONE',  ( -147.3669217311067712, 63.69361261596463919, -76.34879821478752149 ) ) ;
#28156 = ORIENTED_EDGE ( 'NONE', *, *, #22422, .T. ) ;
#28157 = DIRECTION ( 'NONE',  ( -0.000000000000000000, 1.000000000000000000, -0.000000000000000000 ) ) ;
#28158 = LINE ( 'NONE', #38026, #43216 ) ;
#28159 = DIRECTION ( 'NONE',  ( -1.000000000000000000, 0.000000000000000000, 0.000000000000000000 ) ) ;
#28160 = LINE ( 'NONE', #54542, #38282 ) ;
#28161 = DIRECTION ( 'NONE',  ( 1.000000000000000000, 0.000000000000000000, 0.000000000000000000 ) ) ;
#28162 = CARTESIAN_POINT ( 'NONE',  ( 51.85299110299499148, -39.21848821248373440, 170.0000000000000000 ) ) ;
#28163 = CARTESIAN_POINT ( 'NONE',  ( 17.05487707116232343, 34.33113399044100333, 13.32819299319724671 ) ) ;
#28164 = CARTESIAN_POINT ( 'NONE',  ( 110.6583185015671944, 21.43197767180794244, 4.967364376802527737 ) ) ;
#28165 = CARTESIAN_POINT ( 'NONE',  ( -121.5680658099884397, 44.89994870382100345, -75.40337873448993378 ) ) ;
#28166 = ADVANCED_FACE ( 'NONE', ( #2764 ), #24230, .F. ) ;
#28167 = CARTESIAN_POINT ( 'NONE',  ( -12.40598104375063038, 8.242193636955557068, 43.57465072453484822 ) ) ;
#28168 = CARTESIAN_POINT ( 'NONE',  ( 157.9160637431159557, 57.99786926216935967, 17.56491688178972055 ) ) ;
#28169 = CARTESIAN_POINT ( 'NONE',  ( 46.19578020946207175, 10.40950134816946537, -93.62501912019730810 ) ) ;
#28170 = ORIENTED_EDGE ( 'NONE', *, *, #17306, .T. ) ;
#28171 = CARTESIAN_POINT ( 'NONE',  ( -32.40928421737413601, 10.77259363352673205, 3.418817049811458730 ) ) ;
#28173 = VERTEX_POINT ( 'NONE', #30195 ) ;
#28172 = EDGE_CURVE ( 'NONE', #54414, #46955, #19948, .T. ) ;
#28174 = PLANE ( 'NONE',  #3728 ) ;
#28175 = CARTESIAN_POINT ( 'NONE',  ( 84.97658021689289853, 19.92447159015899771, -77.48566349683447640 ) ) ;
#28176 = CARTESIAN_POINT ( 'NONE',  ( 109.9676357272098244, 29.86308433357949355, 83.29856572268397485 ) ) ;
#28177 = CARTESIAN_POINT ( 'NONE',  ( -173.1211646369891071, 87.12891641440859303, 3.977144016177345254 ) ) ;
#28178 = ADVANCED_FACE ( 'NONE', ( #51648 ), #45320, .T. ) ;
#28179 = CARTESIAN_POINT ( 'NONE',  ( -14.86660400085235345, 7.452266534569882417, 88.70135958064247461 ) ) ;
#28180 = VECTOR ( 'NONE', #50707, 1000.000000000000000 ) ;
#28181 = CARTESIAN_POINT ( 'NONE',  ( 311.8713128290285113, 190.0000000000000000, 346.5826552340383842 ) ) ;
#28182 = LINE ( 'NONE', #61251, #36689 ) ;
#28183 = CIRCLE ( 'NONE', #1277, 5.000000000000000888 ) ;
#28184 = DIRECTION ( 'NONE',  ( -0.000000000000000000, 1.000000000000000000, -0.000000000000000000 ) ) ;
#28185 = CARTESIAN_POINT ( 'NONE',  ( -27.00000000000000355, 0.000000000000000000, -0.000000000000000000 ) ) ;
#28186 = ORIENTED_EDGE ( 'NONE', *, *, #27544, .T. ) ;
#28187 = EDGE_LOOP ( 'NONE', ( #29440, #61531 ) ) ;
#28188 = CARTESIAN_POINT ( 'NONE',  ( 31.96192885395476324, 8.569232728322420556, 65.23638710323480439 ) ) ;
#28189 = CARTESIAN_POINT ( 'NONE',  ( 175.5406524085944966, 73.17873692326774915, 58.57573781641595190 ) ) ;
#28191 = DIRECTION ( 'NONE',  ( -1.000000000000000000, 0.000000000000000000, 0.000000000000000000 ) ) ;
#28190 = VECTOR ( 'NONE', #2046, 1000.000000000000000 ) ;
#28192 = CARTESIAN_POINT ( 'NONE',  ( -165.7690020878297901, 80.74028011998679233, 63.65475612973403940 ) ) ;
#28193 = CARTESIAN_POINT ( 'NONE',  ( -165.6397095829521504, 80.60756690931940227, -15.97658641783072930 ) ) ;
#28194 = EDGE_CURVE ( 'NONE', #42819, #28516, #60798, .T. ) ;
#28195 = AXIS2_PLACEMENT_3D ( 'NONE', #35448, #49970, #8727 ) ;
#28196 = DIRECTION ( 'NONE',  ( -1.000000000000000000, 0.000000000000000000, 0.000000000000000000 ) ) ;
#28197 = ORIENTED_EDGE ( 'NONE', *, *, #23702, .T. ) ;
#28198 = B_SPLINE_CURVE_WITH_KNOTS ( 'NONE', 3,
 ( #42550, #68927, #53434, #63671, #64699, #26382, #20751, #16508, #37966, #54113, #59064, #59409, #11221, #58376, #65048, #10186, #16157, #42879, #16846, #31649, #5263, #683, #47820, #38305, #31322, #52747, #4572, #69281, #15819, #22481, #23190, #49901, #1374, #33743, #12631, #2087, #44272, #49193, #7360, #54471, #18249, #55178, #39360, #43918 ),
 .UNSPECIFIED., .F., .F.,
 ( 4, 2, 2, 2, 2, 2, 2, 2, 2, 2, 2, 2, 2, 2, 2, 2, 2, 2, 2, 2, 2, 4 ),
 ( 0.000000000000000000, 0.003360573201437605691, 0.004200716501796969600, 0.005040859802156333509, 0.006721146402875015358, 0.007561289703234363654, 0.008401433003593711951, 0.009241576303953058513, 0.01008171960431240508, 0.01176200620503115198, 0.01260214950539053497, 0.01344229280574991969, 0.01428243610610930268, 0.01512257940646868741, 0.01680286600718746901, 0.01764300930754684679, 0.01848315260790622805, 0.02016343920862500791, 0.02184372580934379124, 0.02352401241006257110, 0.02520429901078135443, 0.02688458561150013429 ),
 .UNSPECIFIED. ) ;
#28199 = CARTESIAN_POINT ( 'NONE',  ( 93.32228019177713918, 22.88890999585040831, 6.973851955883334064 ) ) ;
#28200 = CARTESIAN_POINT ( 'NONE',  ( -68.06184294702747195, 31.38946074233368222, 41.38025477438755928 ) ) ;
#28201 = CARTESIAN_POINT ( 'NONE',  ( -71.96466849523048381, -21.15771699337101808, 43.58025477438756923 ) ) ;
#28202 = CARTESIAN_POINT ( 'NONE',  ( -83.74134668872638088, 25.40628965235943681, -90.76525586021888614 ) ) ;
#28203 = CARTESIAN_POINT ( 'NONE',  ( -36.11269837220801548, 36.11269837220812207, 85.00100000000000477 ) ) ;
#28204 = CARTESIAN_POINT ( 'NONE',  ( 8.000000000000007105, 249.8719672152120381, 94.99999999999866418 ) ) ;
#28205 = FACE_BOUND ( 'NONE', #46801, .T. ) ;
#28206 = PLANE ( 'NONE',  #34430 ) ;
#28207 = ORIENTED_EDGE ( 'NONE', *, *, #4846, .F. ) ;
#28208 = DIRECTION ( 'NONE',  ( 0.000000000000000000, 0.000000000000000000, -1.000000000000000000 ) ) ;
#28209 = CARTESIAN_POINT ( 'NONE',  ( 0.000000000000000000, -0.1068809833119260672, -91.05865558859387932 ) ) ;
#28210 = CARTESIAN_POINT ( 'NONE',  ( -48.58279704072702287, 14.07632445131079812, 68.46338809851388874 ) ) ;
#28211 = CARTESIAN_POINT ( 'NONE',  ( -180.2243452982808947, 96.99029284948629481, 13.90186183527965547 ) ) ;
#28212 = CARTESIAN_POINT ( 'NONE',  ( 208.5884523568771556, 113.6152425727544824, 69.97810575574392544 ) ) ;
#28213 = CARTESIAN_POINT ( 'NONE',  ( 24.79066879238614263, -3.228426989449305839, 0.000000000000000000 ) ) ;
#28214 = VERTEX_POINT ( 'NONE', #2419 ) ;
#28215 = CARTESIAN_POINT ( 'NONE',  ( 56.30171512200999473, 11.21502580416398764, 13.82023505722669476 ) ) ;
#28216 = CARTESIAN_POINT ( 'NONE',  ( -61.52143283897135717, 16.51181063611434752, 60.85814816128657156 ) ) ;
#28217 = ORIENTED_EDGE ( 'NONE', *, *, #64221, .F. ) ;
#28218 = ORIENTED_EDGE ( 'NONE', *, *, #40051, .F. ) ;
#28219 = CARTESIAN_POINT ( 'NONE',  ( 133.8566784816069344, -170.0000000000000000, 2.665790248531674678 ) ) ;
#28220 = CARTESIAN_POINT ( 'NONE',  ( -61.10880364359507411, 17.43879918625640002, -20.30299724292251184 ) ) ;
#28221 = CARTESIAN_POINT ( 'NONE',  ( 87.58754341703161117, 20.81465688423120142, -62.71234923768123792 ) ) ;
#28222 = ORIENTED_EDGE ( 'NONE', *, *, #31301, .T. ) ;
#28223 = AXIS2_PLACEMENT_3D ( 'NONE', #54492, #47485, #64360 ) ;
#28224 = ORIENTED_EDGE ( 'NONE', *, *, #21433, .F. ) ;
#28225 = CARTESIAN_POINT ( 'NONE',  ( 36.09137906183517686, 8.001963043161762101, -23.00953966251914906 ) ) ;
#28226 = CARTESIAN_POINT ( 'NONE',  ( 164.8914542114683570, 64.97670918603525081, 35.78822635281908759 ) ) ;
#28227 = CARTESIAN_POINT ( 'NONE',  ( 0.000000000000000000, 0.000000000000000000, -20.00000000000000000 ) ) ;
#28228 = CARTESIAN_POINT ( 'NONE',  ( 68.94948716683070700, 15.16699441119058100, 5.855287509081221309 ) ) ;
#28229 = CARTESIAN_POINT ( 'NONE',  ( -190.6985136298601731, 109.1272424661242582, 94.99999999999866418 ) ) ;
#28230 = AXIS2_PLACEMENT_3D ( 'NONE', #65523, #48963, #803 ) ;
#28231 = EDGE_CURVE ( 'NONE', #61740, #18178, #12624, .T. ) ;
#28232 = PRODUCT ( 'lock', 'lock', '', ( #69469 ) ) ;
#28233 = AXIS2_PLACEMENT_3D ( 'NONE', #52472, #9222, #4296 ) ;
#28234 = VECTOR ( 'NONE', #50775, 1000.000000000000000 ) ;
#28236 = EDGE_CURVE ( 'NONE', #34426, #63967, #24581, .T. ) ;
#28235 = DIRECTION ( 'NONE',  ( -1.000000000000000000, 0.000000000000000000, 0.000000000000000000 ) ) ;
#28237 = CARTESIAN_POINT ( 'NONE',  ( -50.14440374537738876, 14.45628984983895293, 16.66475555544458587 ) ) ;
#28238 = LINE ( 'NONE', #49333, #62873 ) ;
#28239 = CYLINDRICAL_SURFACE ( 'NONE', #37415, 65.36598343705435354 ) ;
#28240 = DIRECTION ( 'NONE',  ( 0.000000000000000000, 0.000000000000000000, -1.000000000000000000 ) ) ;
#28241 = DIRECTION ( 'NONE',  ( -0.000000000000000000, -0.000000000000000000, -1.000000000000000000 ) ) ;
#28243 = VERTEX_POINT ( 'NONE', #56220 ) ;
#28242 = CARTESIAN_POINT ( 'NONE',  ( 50.03867889673311709, 42.05760816978183669, 6.377659838150144402E-18 ) ) ;
#28244 = EDGE_LOOP ( 'NONE', ( #29276, #33899, #54073, #61181 ) ) ;
#28245 = ORIENTED_EDGE ( 'NONE', *, *, #60338, .F. ) ;
#28246 = DIRECTION ( 'NONE',  ( 0.000000000000000000, 0.000000000000000000, 1.000000000000000000 ) ) ;
#28247 = CARTESIAN_POINT ( 'NONE',  ( -166.5879373373658154, 81.58564870376412159, 88.31158596434660524 ) ) ;
#28248 = CARTESIAN_POINT ( 'NONE',  ( -51.77439426130689526, 13.82695438436703839, -9.121836570883877116 ) ) ;
#28249 = LINE ( 'NONE', #44432, #9706 ) ;
#28250 = EDGE_CURVE ( 'NONE', #15856, #35508, #8037, .T. ) ;
#28251 = CARTESIAN_POINT ( 'NONE',  ( -62.15063206372443716, 17.75106610013996189, -45.18927541931358149 ) ) ;
#28252 = EDGE_CURVE ( 'NONE', #46731, #34711, #45606, .T. ) ;
#28253 = DIRECTION ( 'NONE',  ( 0.000000000000000000, 0.000000000000000000, 1.000000000000000000 ) ) ;
#28254 = CARTESIAN_POINT ( 'NONE',  ( -71.22878586122430988, 19.62649588091169406, -68.46191443494774376 ) ) ;
#28255 = CARTESIAN_POINT ( 'NONE',  ( 19.11168290073779730, 6.629794975642855803, -9.446444181573534493 ) ) ;
#28256 = ORIENTED_EDGE ( 'NONE', *, *, #28514, .F. ) ;
#28257 = FACE_BOUND ( 'NONE', #45978, .T. ) ;
#28258 = VERTEX_POINT ( 'NONE', #20317 ) ;
#28259 = ORIENTED_EDGE ( 'NONE', *, *, #53488, .F. ) ;
#28260 = CARTESIAN_POINT ( 'NONE',  ( 66.73431804020508196, 14.60294556126670429, -22.89389229214575394 ) ) ;
#28261 = CARTESIAN_POINT ( 'NONE',  ( -60.43316470166142551, 17.23897012780379612, -91.17587151978018767 ) ) ;
#28262 = CARTESIAN_POINT ( 'NONE',  ( -24.07246351276930696, 9.512772164140772091, 89.95986364399971080 ) ) ;
#28263 = EDGE_CURVE ( 'NONE', #43897, #58070, #31919, .T. ) ;
#28264 = CARTESIAN_POINT ( 'NONE',  ( 113.8724110608469431, 31.71510301790681652, -23.15866281951693750 ) ) ;
#28265 = CARTESIAN_POINT ( 'NONE',  ( 15.68296563925497900, 63.09411298019765013, 43.58025477438756923 ) ) ;
#28266 = CARTESIAN_POINT ( 'NONE',  ( 0.000000000000000000, 35.00000000000000000, -27.00000000000000000 ) ) ;
#28267 = CARTESIAN_POINT ( 'NONE',  ( 138.1901928158493433, 45.29454828899443442, -10.53948683715141854 ) ) ;
#28268 = VERTEX_POINT ( 'NONE', #4827 ) ;
#28269 = ORIENTED_EDGE ( 'NONE', *, *, #45759, .F. ) ;
#28270 = ORIENTED_EDGE ( 'NONE', *, *, #3986, .T. ) ;
#28271 = CARTESIAN_POINT ( 'NONE',  ( 29.86806733335506436, 0.000000000000000000, 2.810436579993893957 ) ) ;
#28272 = DIRECTION ( 'NONE',  ( -0.000000000000000000, -0.000000000000000000, -1.000000000000000000 ) ) ;
#28273 = CYLINDRICAL_SURFACE ( 'NONE', #31164, 5.000000000000004441 ) ;
#28274 = CARTESIAN_POINT ( 'NONE',  ( 57.07734607129817306, 11.37318329671159134, -20.98356477351893901 ) ) ;
#28275 =( REPRESENTATION_RELATIONSHIP ('NONE','NONE', #40274, #50551 ) REPRESENTATION_RELATIONSHIP_WITH_TRANSFORMATION ( #53369 )SHAPE_REPRESENTATION_RELATIONSHIP( ) );
#28276 = EDGE_CURVE ( 'NONE', #25372, #40455, #57953, .T. ) ;
#28277 = UNCERTAINTY_MEASURE_WITH_UNIT (LENGTH_MEASURE( 1.000000000000000082E-05 ), #5782, 'distance_accuracy_value', 'NONE');
#28278 = AXIS2_PLACEMENT_3D ( 'NONE', #30735, #63083, #4677 ) ;
#28279 = CARTESIAN_POINT ( 'NONE',  ( -447.6627218934915504, 392.9289321881299770, 108.5502958579924950 ) ) ;
#28280 = ADVANCED_FACE ( 'NONE', ( #21018 ), #41437, .T. ) ;
#28281 = CARTESIAN_POINT ( 'NONE',  ( -35.00000000000000000, 225.0000000000000000, 2.000000000000000000 ) ) ;
#28282 = ADVANCED_FACE ( 'NONE', ( #20662 ), #42121, .T. ) ;
#28283 = ORIENTED_EDGE ( 'NONE', *, *, #36950, .F. ) ;
#28284 = ADVANCED_FACE ( 'NONE', ( #30535 ), #51984, .T. ) ;
#28285 = CARTESIAN_POINT ( 'NONE',  ( 185.1660960081724170, 84.30194217633010112, 57.35720483677989989 ) ) ;
#28286 = CARTESIAN_POINT ( 'NONE',  ( 176.6214367443247966, 74.20967084876663478, -64.52294413732886369 ) ) ;
#28287 = AXIS2_PLACEMENT_3D ( 'NONE', #25910, #43100, #42755 ) ;
#28288 = SHAPE_REPRESENTATION_RELATIONSHIP ( 'NONE' , 'NONE' ,  #31639, #32386 ) ;
#28289 = CARTESIAN_POINT ( 'NONE',  ( -1.327237339234996982, 7.561837009978233048, -39.16517982428524647 ) ) ;
#28290 = DIRECTION ( 'NONE',  ( 0.000000000000000000, 0.000000000000000000, 1.000000000000000000 ) ) ;
#28291 = CARTESIAN_POINT ( 'NONE',  ( -166.7049310409072120, 80.25944422923579680, 15.36979968814921627 ) ) ;
#28292 = DIRECTION ( 'NONE',  ( -0.7071067811865483499, 0.000000000000000000, 0.7071067811865467956 ) ) ;
#28293 = FACE_BOUND ( 'NONE', #64077, .T. ) ;
#28294 = CARTESIAN_POINT ( 'NONE',  ( -17.50000000000002842, -18.06806526123148160, 378.0000000000000000 ) ) ;
#28295 = AXIS2_PLACEMENT_3D ( 'NONE', #53054, #26006, #31285 ) ;
#28296 = VERTEX_POINT ( 'NONE', #35819 ) ;
#28297 = DIRECTION ( 'NONE',  ( 0.7071067811865405783, 7.105427357601001070E-15, -0.7071067811865545671 ) ) ;
#28298 = CLOSED_SHELL ( 'NONE', ( #29139, #35185, #44463, #1494, #48003, #66986, #34800, #51237, #2527, #4594, #60335, #34825, #37773, #28588, #9391, #3821, #49058, #47702, #33911, #6095, #21569, #66800 ) ) ;
#28299 = CARTESIAN_POINT ( 'NONE',  ( -133.2698123908828336, 51.54642138335022139, -67.87415851310558423 ) ) ;
#28300 = FACE_OUTER_BOUND ( 'NONE', #29854, .T. ) ;
#28301 = CARTESIAN_POINT ( 'NONE',  ( 46.64694836521739063, 9.462741877720628025, -71.91924328827956003 ) ) ;
#28302 = LINE ( 'NONE', #33598, #68122 ) ;
#28303 = ORIENTED_EDGE ( 'NONE', *, *, #21995, .T. ) ;
#28304 = ORIENTED_EDGE ( 'NONE', *, *, #10065, .T. ) ;
#28305 = CARTESIAN_POINT ( 'NONE',  ( -127.5425607999732307, 47.58841438093516274, -88.77439082497835443 ) ) ;
#28306 = CARTESIAN_POINT ( 'NONE',  ( 187.1633130089971644, 84.97574503406409008, 86.09156961515144246 ) ) ;
#28307 = VERTEX_POINT ( 'NONE', #15393 ) ;
#28308 = ORIENTED_EDGE ( 'NONE', *, *, #5489, .T. ) ;
#28309 = CARTESIAN_POINT ( 'NONE',  ( 173.6710158776850506, 71.42507420636738402, -44.90187336702329191 ) ) ;
#28310 = CARTESIAN_POINT ( 'NONE',  ( 162.8034185388970627, 63.22443559329410334, 4.769821300519481611 ) ) ;
#28311 = DIRECTION ( 'NONE',  ( -5.551115123125781716E-16, 0.000000000000000000, -1.000000000000000000 ) ) ;
#28312 = VERTEX_POINT ( 'NONE', #63920 ) ;
#28313 = DIRECTION ( 'NONE',  ( 0.000000000000000000, 0.000000000000000000, 1.000000000000000000 ) ) ;
#28314 = CARTESIAN_POINT ( 'NONE',  ( 141.0792860804900499, 47.16255757051797559, 61.76377827337359605 ) ) ;
#28315 = CARTESIAN_POINT ( 'NONE',  ( -71.97434903038468690, 19.88430675376531909, -46.03817687804183123 ) ) ;
#28316 = CARTESIAN_POINT ( 'NONE',  ( -109.0191069781766657, 37.48620563201052391, 94.99999999999866418 ) ) ;
#28317 = CARTESIAN_POINT ( 'NONE',  ( 61.94551956023253325, 24.58367740818825098, 34.48241823985146937 ) ) ;
#28318 = CARTESIAN_POINT ( 'NONE',  ( -49.13048465129991627, 14.20828170588045758, -11.24350225477614629 ) ) ;
#28319 = ADVANCED_FACE ( 'NONE', ( #41781 ), #62893, .T. ) ;
#28320 = ORIENTED_EDGE ( 'NONE', *, *, #39557, .F. ) ;
#28322 = ADVANCED_FACE ( 'NONE', ( #47383 ), #15734, .F. ) ;
#28321 = CARTESIAN_POINT ( 'NONE',  ( 115.7561705820729259, 31.51689401996058493, -48.53024572195440101 ) ) ;
#28323 = B_SPLINE_CURVE_WITH_KNOTS ( 'NONE', 3,
 ( #1513, #27899, #50404, #33881, #54620, #12423, #55673, #1167, #7506, #59890, #28959, #6448, #2221, #49334, #43709, #22621, #60257, #45114, #66597, #55319, #65542, #65187, #17338, #38453 ),
 .UNSPECIFIED., .F., .F.,
 ( 4, 2, 2, 2, 2, 2, 2, 2, 2, 2, 2, 4 ),
 ( 0.000000000000000000, 0.001596609432691784665, 0.002394914149037695103, 0.003193218865383606192, 0.003991523581729517281, 0.004789828298075427503, 0.006386437730767201108, 0.007184742447113077503, 0.007983047163458954765, 0.009579656596150731840, 0.01117626602884251238, 0.01277287546153429119 ),
 .UNSPECIFIED. ) ;
#28324 = CARTESIAN_POINT ( 'NONE',  ( -72.35078170365746075, 21.08176362823952843, 7.021010477035512842 ) ) ;
#28325 = CARTESIAN_POINT ( 'NONE',  ( -144.7530445311634253, 61.54314312182906832, -48.11838420148568218 ) ) ;
#28326 = FACE_OUTER_BOUND ( 'NONE', #20530, .T. ) ;
#28328 = VERTEX_POINT ( 'NONE', #25269 ) ;
#28327 = CARTESIAN_POINT ( 'NONE',  ( -122.3638092602184457, 44.21314101515333306, 85.18516341637682387 ) ) ;
#28329 = CARTESIAN_POINT ( 'NONE',  ( 59.29474530993689285, 12.86968658439548285, 16.98489541084898491 ) ) ;
#28330 = AXIS2_PLACEMENT_3D ( 'NONE', #58322, #15767, #16460 ) ;
#28331 = ORIENTED_EDGE ( 'NONE', *, *, #46763, .T. ) ;
#28332 = AXIS2_PLACEMENT_3D ( 'NONE', #49243, #29894, #24630 ) ;
#28333 = CARTESIAN_POINT ( 'NONE',  ( -149.0782809666403352, 63.81577337591401289, 57.56537183036275707 ) ) ;
#28334 = DIRECTION ( 'NONE',  ( 1.387778780781445922E-16, -1.000000000000000000, -1.232595164407830946E-32 ) ) ;
#28335 = FACE_OUTER_BOUND ( 'NONE', #45849, .T. ) ;
#28336 = EDGE_CURVE ( 'NONE', #59849, #68407, #25389, .T. ) ;
#28337 = CARTESIAN_POINT ( 'NONE',  ( 183.9986899696430669, 81.60141257362812439, -23.80433703628514763 ) ) ;
#28338 = CIRCLE ( 'NONE', #54168, 5.000000000000000000 ) ;
#28339 = EDGE_CURVE ( 'NONE', #4867, #33777, #13033, .T. ) ;
#28340 = CARTESIAN_POINT ( 'NONE',  ( 138.6020257460769187, 44.36414356192206299, -10.85064934410134008 ) ) ;
#28341 = CARTESIAN_POINT ( 'NONE',  ( 0.000000000000000000, 190.0000000000000000, 159.3522585083728700 ) ) ;
#28342 = CARTESIAN_POINT ( 'NONE',  ( 91.11342358617751813, 21.00000175105272149, -76.18291065189346511 ) ) ;
#28343 = CARTESIAN_POINT ( 'NONE',  ( -65.36598343705435354, 0.000000000000000000, 41.38025477438755928 ) ) ;
#28344 = DIRECTION ( 'NONE',  ( 1.000000000000000000, 0.000000000000000000, 0.000000000000000000 ) ) ;
#28345 = VERTEX_POINT ( 'NONE', #46351 ) ;
#28346 = ORIENTED_EDGE ( 'NONE', *, *, #25680, .F. ) ;
#28347 = EDGE_CURVE ( 'NONE', #61401, #59876, #13448, .T. ) ;
#28348 = CARTESIAN_POINT ( 'NONE',  ( 41.33692564073607656, 8.668977654195481719, 30.16360919430110599 ) ) ;
#28349 = CIRCLE ( 'NONE', #29461, 20.30000000000000071 ) ;
#28350 = CARTESIAN_POINT ( 'NONE',  ( 0.000000000000000000, 6.928203230275506108, 4.000000000000007105 ) ) ;
#28351 = CARTESIAN_POINT ( 'NONE',  ( 0.000000000000000000, 190.0000000000000000, -2.000000000000000000 ) ) ;
#28352 = DIRECTION ( 'NONE',  ( -0.000000000000000000, 1.000000000000000000, -0.000000000000000000 ) ) ;
#28353 = CARTESIAN_POINT ( 'NONE',  ( 212.1976655298228707, 119.0878071902807847, -44.00379268766470631 ) ) ;
#28354 = CARTESIAN_POINT ( 'NONE',  ( 204.6977192012829789, -170.0000000000000000, -36.32593103262158252 ) ) ;
#28355 = LINE ( 'NONE', #61747, #47176 ) ;
#28356 = FACE_OUTER_BOUND ( 'NONE', #57031, .T. ) ;
#28357 = PLANE ( 'NONE',  #10468 ) ;
#28358 = VERTEX_POINT ( 'NONE', #43833 ) ;
#28359 = CARTESIAN_POINT ( 'NONE',  ( -25.80443741485377984, 9.749985135376002532, 15.84590824961209066 ) ) ;
#28360 = VERTEX_POINT ( 'NONE', #10794 ) ;
#28361 = LINE ( 'NONE', #39277, #26283 ) ;
#28362 = CARTESIAN_POINT ( 'NONE',  ( -86.11780422997766493, 25.30122877727817254, 92.52076852176431032 ) ) ;
#28363 = CARTESIAN_POINT ( 'NONE',  ( -5.000000000000058620, -26.11269837220806522, 85.00100000000000477 ) ) ;
#28364 = CARTESIAN_POINT ( 'NONE',  ( 127.4992165631961569, 38.87141012667724027, 32.99998151848554073 ) ) ;
#28365 = CARTESIAN_POINT ( 'NONE',  ( -25.10237775011640338, 1.004202417053489116, 3.061616997868437868E-16 ) ) ;
#28366 = FACE_OUTER_BOUND ( 'NONE', #1285, .T. ) ;
#28367 = DIRECTION ( 'NONE',  ( -0.000000000000000000, -0.000000000000000000, 1.000000000000000000 ) ) ;
#28368 = EDGE_CURVE ( 'NONE', #29554, #347, #2933, .T. ) ;
#28369 = EDGE_CURVE ( 'NONE', #63634, #21301, #11139, .T. ) ;
#28370 = DIRECTION ( 'NONE',  ( 1.343643437439745986E-14, 1.000000000000000000, 1.110223024625156171E-16 ) ) ;
#28371 = CARTESIAN_POINT ( 'NONE',  ( 212.1962697089473693, 117.2293607936260429, 90.12784865809409496 ) ) ;
#28372 = ORIENTED_EDGE ( 'NONE', *, *, #25806, .F. ) ;
#28373 = CARTESIAN_POINT ( 'NONE',  ( 55.51637278631174155, 12.08345311280959500, 63.64786402826049994 ) ) ;
#28374 = LINE ( 'NONE', #1301, #56498 ) ;
#28376 = EDGE_CURVE ( 'NONE', #19070, #12059, #38937, .T. ) ;
#28375 = CARTESIAN_POINT ( 'NONE',  ( -12.40598104375063215, 8.242193636955555291, 16.73010013407117214 ) ) ;
#28377 = FACE_OUTER_BOUND ( 'NONE', #67049, .T. ) ;
#28378 = DIRECTION ( 'NONE',  ( -6.405132834375901070E-16, 1.000000000000000000, 6.405132834375902056E-16 ) ) ;
#28379 = CARTESIAN_POINT ( 'NONE',  ( -95.39402268064687007, 29.41819732823228861, -93.22295461411728468 ) ) ;
#28380 = ORIENTED_EDGE ( 'NONE', *, *, #34961, .T. ) ;
#28381 = AXIS2_PLACEMENT_3D ( 'NONE', #67435, #19580, #3071 ) ;
#28382 = PRODUCT_CONTEXT ( 'NONE', #61055, 'mechanical' ) ;
#28383 = DIRECTION ( 'NONE',  ( 0.000000000000000000, -1.000000000000000000, 0.000000000000000000 ) ) ;
#28384 = CARTESIAN_POINT ( 'NONE',  ( -37.05762690088739930, 11.60527003175541161, -47.79140132144340214 ) ) ;
#28385 = CARTESIAN_POINT ( 'NONE',  ( -167.6566265204789943, 82.70140535081090150, -37.06906935447201334 ) ) ;
#28386 = CARTESIAN_POINT ( 'NONE',  ( -179.0096683247334681, 93.93079036873261600, 87.35646014482341570 ) ) ;
#28387 = ORIENTED_EDGE ( 'NONE', *, *, #16655, .F. ) ;
#28388 = CARTESIAN_POINT ( 'NONE',  ( 25.00000000000763478, -65.13282190615278466, 5.000000000000000000 ) ) ;
#28389 = VECTOR ( 'NONE', #55956, 1000.000000000000000 ) ;
#28390 = CARTESIAN_POINT ( 'NONE',  ( 39.40195752203892710, 9.424259417798134919, 29.91383430596324899 ) ) ;
#28391 = CARTESIAN_POINT ( 'NONE',  ( -148.6426981422629012, 63.44891673852540492, -22.93093452246228026 ) ) ;
#28392 = CONICAL_SURFACE ( 'NONE', #20548, 74.95140232871122521, 0.8777644062502172329 ) ;
#28393 = CARTESIAN_POINT ( 'NONE',  ( -4.506365319453816909, 7.705038994660851515, -76.49273962913744640 ) ) ;
#28394 = CIRCLE ( 'NONE', #37369, 65.00000000000000000 ) ;
#28395 = CARTESIAN_POINT ( 'NONE',  ( -37.04655464516844177, 53.85410457537859230, 41.38025477438755928 ) ) ;
#28396 = VERTEX_POINT ( 'NONE', #5857 ) ;
#28397 = CARTESIAN_POINT ( 'NONE',  ( 159.2802156694726534, 60.35763705070695551, -90.02572906011900500 ) ) ;
#28398 = CARTESIAN_POINT ( 'NONE',  ( 201.6034029841262338, 102.1956603101140644, -36.98047612985361354 ) ) ;
#28399 = CARTESIAN_POINT ( 'NONE',  ( -96.45303203827903360, 31.03218867996498531, 42.76688867157084672 ) ) ;
#28400 = AXIS2_PLACEMENT_3D ( 'NONE', #50153, #61053, #38549 ) ;
#28401 = CARTESIAN_POINT ( 'NONE',  ( 15.78827728214693416, 6.500811158483284835, -50.51894409868581448 ) ) ;
#28403 = VERTEX_POINT ( 'NONE', #64968 ) ;
#28402 = CARTESIAN_POINT ( 'NONE',  ( 114.6659427952414489, 32.10199811723106222, 16.34235119158301330 ) ) ;
#28404 = CARTESIAN_POINT ( 'NONE',  ( 175.5429257635131250, 74.57009623370761631, 68.73334881941738672 ) ) ;
#28405 = ORIENTED_EDGE ( 'NONE', *, *, #43655, .F. ) ;
#28406 = ORIENTED_EDGE ( 'NONE', *, *, #10921, .F. ) ;
#28408 = EDGE_CURVE ( 'NONE', #47168, #48718, #12198, .T. ) ;
#28407 = CARTESIAN_POINT ( 'NONE',  ( -72.20490592113145567, 19.96451062593609649, -11.93102570283482855 ) ) ;
#28409 = CARTESIAN_POINT ( 'NONE',  ( 26.11269837220800127, -31.11269837220812562, 2.000000000000000000 ) ) ;
#28411 = ORIENTED_EDGE ( 'NONE', *, *, #43876, .T. ) ;
#28410 = FACE_OUTER_BOUND ( 'NONE', #6776, .T. ) ;
#28412 = CARTESIAN_POINT ( 'NONE',  ( 164.9697211531230039, 63.72502658717167634, 36.61266077936287644 ) ) ;
#28413 = DIRECTION ( 'NONE',  ( 0.000000000000000000, 0.000000000000000000, 1.000000000000000000 ) ) ;
#28414 = CARTESIAN_POINT ( 'NONE',  ( 11.05669727962760085, 70.00000000000000000, -27.88815958909220782 ) ) ;
#28415 = ORIENTED_EDGE ( 'NONE', *, *, #58194, .F. ) ;
#28416 = CARTESIAN_POINT ( 'NONE',  ( -146.3632089724601144, 62.86016173369542059, -89.17980501507723545 ) ) ;
#28417 = EDGE_CURVE ( 'NONE', #67247, #51018, #69191, .T. ) ;
#28418 = CARTESIAN_POINT ( 'NONE',  ( -38.26497993382595553, 10.81185389040525635, -12.85537468134073080 ) ) ;
#28419 = CARTESIAN_POINT ( 'NONE',  ( -180.2243452982808947, 96.99029284948633745, 40.74641242574331557 ) ) ;
#28420 = CARTESIAN_POINT ( 'NONE',  ( 130.3035708464390439, 40.48418876551455270, 70.47724502307815442 ) ) ;
#28421 = EDGE_CURVE ( 'NONE', #46743, #51410, #59663, .T. ) ;
#28422 = LINE ( 'NONE', #29129, #49721 ) ;
#28423 = VERTEX_POINT ( 'NONE', #55090 ) ;
#28424 = EDGE_CURVE ( 'NONE', #55566, #56923, #33661, .T. ) ;
#28425 = EDGE_LOOP ( 'NONE', ( #35121, #67993, #48370, #21355 ) ) ;
#28426 = ORIENTED_EDGE ( 'NONE', *, *, #66678, .T. ) ;
#28427 =( GEOMETRIC_REPRESENTATION_CONTEXT ( 3 ) GLOBAL_UNCERTAINTY_ASSIGNED_CONTEXT ( ( #33920 ) ) GLOBAL_UNIT_ASSIGNED_CONTEXT ( ( #53424, #30620, #41516 ) ) REPRESENTATION_CONTEXT ( 'NONE', 'WORKASPACE' ) );
#28428 = LINE ( 'NONE', #2063, #35122 ) ;
#28429 = ADVANCED_FACE ( 'NONE', ( #21693 ), #32945, .F. ) ;
#28430 = CARTESIAN_POINT ( 'NONE',  ( 0.000000000000000000, 0.000000000000000000, 85.00000000000000000 ) ) ;
#28431 = CARTESIAN_POINT ( 'NONE',  ( -31.43908319763709969, 10.61114334766716105, 30.21645440618916112 ) ) ;
#28432 = VECTOR ( 'NONE', #59312, 1000.000000000000000 ) ;
#28433 = LINE ( 'NONE', #1358, #20942 ) ;
#28434 = DIRECTION ( 'NONE',  ( 0.000000000000000000, 0.000000000000000000, 1.000000000000000000 ) ) ;
#28435 = LINE ( 'NONE', #34073, #15702 ) ;
#28436 = AXIS2_PLACEMENT_3D ( 'NONE', #33542, #6787, #54970 ) ;
#28437 = CARTESIAN_POINT ( 'NONE',  ( -133.2698123908828336, 51.54642138335022139, 66.34859443921281752 ) ) ;
#28438 = CARTESIAN_POINT ( 'NONE',  ( -74.18622060908361959, 21.73430079572373330, -21.80510037720168270 ) ) ;
#28439 = ORIENTED_EDGE ( 'NONE', *, *, #36220, .F. ) ;
#28441 = CARTESIAN_POINT ( 'NONE',  ( 81.74909803672915132, 17.81295302817863302, 58.34005553837022262 ) ) ;
#28440 = VECTOR ( 'NONE', #26911, 1000.000000000000000 ) ;
#28442 = EDGE_LOOP ( 'NONE', ( #54313, #53668 ) ) ;
#28443 = CARTESIAN_POINT ( 'NONE',  ( -96.05874693101999640, 30.84461336787882502, -92.00895264577386001 ) ) ;
#28444 = AXIS2_PLACEMENT_3D ( 'NONE', #47839, #4592, #25722 ) ;
#28445 = CARTESIAN_POINT ( 'NONE',  ( 63.01563776193091826, -170.0000000000000000, -96.90979201309711755 ) ) ;
#28446 = ORIENTED_EDGE ( 'NONE', *, *, #30493, .F. ) ;
#28447 = LINE ( 'NONE', #49895, #37461 ) ;
#28448 = DIRECTION ( 'NONE',  ( 0.000000000000000000, 0.000000000000000000, -1.000000000000000000 ) ) ;
#28449 = CARTESIAN_POINT ( 'NONE',  ( 204.6977192012829789, 108.0580384837235073, -63.17048162308526571 ) ) ;
#28450 = CARTESIAN_POINT ( 'NONE',  ( -422.6627218934914936, 399.9999999999998863, -141.4497041420118535 ) ) ;
#28451 = CARTESIAN_POINT ( 'NONE',  ( -54.08504625707234226, 14.42374043447187404, 18.42598598950144861 ) ) ;
#28452 = CONICAL_SURFACE ( 'NONE', #1485, 8.000000000000000000, 1.047197551196600296 ) ;
#28453 = DIRECTION ( 'NONE',  ( 0.000000000000000000, 0.000000000000000000, 1.000000000000000000 ) ) ;
#28454 = CARTESIAN_POINT ( 'NONE',  ( -84.49322488516129681, 0.000000000000000000, 43.58025477438756212 ) ) ;
#28455 = VERTEX_POINT ( 'NONE', #6211 ) ;
#28456 = CARTESIAN_POINT ( 'NONE',  ( 410.0000000000000000, 0.000000000000000000, -2.000000000000000000 ) ) ;
#28457 = B_SPLINE_CURVE_WITH_KNOTS ( 'NONE', 3,
 ( #21705, #27324, #954, #602, #22058, #64978, #66636, #54397, #16774, #18434, #2605, #43154, #5531, #43847, #13165, #38233, #18780, #34633, #64625, #10809, #32278, #53708, #16438, #37894, #6219, #59674, #14539, #52513, #47227, #57795, #68685, #67331, #19823, #25458, #3297, #20161, #36342, #41275, #51823, #9614, #40239, #62383, #19119, #51140 ),
 .UNSPECIFIED., .F., .F.,
 ( 4, 2, 2, 2, 2, 2, 2, 2, 2, 2, 2, 2, 2, 2, 2, 2, 2, 2, 2, 2, 2, 4 ),
 ( 6.938893903907228378E-18, 0.001472974678681662894, 0.002209462018022494666, 0.002945949357363326655, 0.004418924036045004944, 0.005891898714726683667, 0.007364873393408363257, 0.008101360732749184404, 0.008837848072090008153, 0.01031082275077161575, 0.01178379742945322335, 0.01252028476879400720, 0.01325677210813478932, 0.01472974678681635181, 0.01546623412615715995, 0.01620272146549796982, 0.01767569614417961385, 0.01914867082286125788, 0.01988515816220207469, 0.02062164550154288803, 0.02209462018022450430, 0.02356759485890611364 ),
 .UNSPECIFIED. ) ;
#28458 = DIRECTION ( 'NONE',  ( -0.000000000000000000, 1.000000000000000000, -0.000000000000000000 ) ) ;
#28459 = ORIENTED_EDGE ( 'NONE', *, *, #29225, .T. ) ;
#28460 = CARTESIAN_POINT ( 'NONE',  ( 49.76301652092167416, 41.81676920493115546, 170.0000000000000000 ) ) ;
#28461 = CARTESIAN_POINT ( 'NONE',  ( 61.28323125814100081, 21.66484633135460669, 40.00000000000003553 ) ) ;
#28463 = EDGE_CURVE ( 'NONE', #67388, #2651, #48073, .T. ) ;
#28462 = DIRECTION ( 'NONE',  ( 1.000000000000000000, 1.850550996349095901E-16, 1.228197773518735191E-20 ) ) ;
#28464 = ORIENTED_EDGE ( 'NONE', *, *, #43359, .F. ) ;
#28465 = CARTESIAN_POINT ( 'NONE',  ( -86.09999398724993114, 25.29376521564873670, 38.94662278282052625 ) ) ;
#28466 = CARTESIAN_POINT ( 'NONE',  ( 150.0980941434704619, 53.37942190380066165, -71.87366452615613355 ) ) ;
#28467 = CARTESIAN_POINT ( 'NONE',  ( 59.95259601283825646, 11.98300577492408259, -50.07103179405425664 ) ) ;
#28468 = CARTESIAN_POINT ( 'NONE',  ( 137.3958226571046737, 43.60243650158412265, -50.15227799746330106 ) ) ;
#28469 = ORIENTED_EDGE ( 'NONE', *, *, #7309, .F. ) ;
#28470 = ORIENTED_EDGE ( 'NONE', *, *, #47792, .T. ) ;
#28471 = DIRECTION ( 'NONE',  ( 0.000000000000000000, -0.000000000000000000, -1.000000000000000000 ) ) ;
#28472 = ORIENTED_EDGE ( 'NONE', *, *, #6741, .F. ) ;
#28473 = CARTESIAN_POINT ( 'NONE',  ( 35.65622260226241025, 8.964590916200318560, -9.772986381556050262 ) ) ;
#28474 = LINE ( 'NONE', #17575, #5725 ) ;
#28475 =( NAMED_UNIT ( * ) PLANE_ANGLE_UNIT ( ) SI_UNIT ( $, .RADIAN. ) );
#28476 = CARTESIAN_POINT ( 'NONE',  ( 136.9486907385599750, 44.50999891875532910, 83.85916308499764682 ) ) ;
#28477 = CARTESIAN_POINT ( 'NONE',  ( -24.09190246691234805, 9.515371887976103338, -95.00000000000133582 ) ) ;
#28478 = VERTEX_POINT ( 'NONE', #17100 ) ;
#28479 = TOROIDAL_SURFACE ( 'NONE', #397, 24.69999999999999929, 0.3000000000000035971 ) ;
#28480 = CARTESIAN_POINT ( 'NONE',  ( -36.11269837220809364, -15.55634918610397754, 85.00100000000000477 ) ) ;
#28481 = ORIENTED_EDGE ( 'NONE', *, *, #47513, .T. ) ;
#28482 = EDGE_LOOP ( 'NONE', ( #6478, #66068, #6480, #57491, #36541, #8945, #38878, #60954 ) ) ;
#28483 = DIRECTION ( 'NONE',  ( -0.000000000000000000, 1.000000000000000000, -0.000000000000000000 ) ) ;
#28484 = CARTESIAN_POINT ( 'NONE',  ( 0.000000000000000000, 0.000000000000000000, 43.58025477438756212 ) ) ;
#28485 = AXIS2_PLACEMENT_3D ( 'NONE', #30883, #37180, #58626 ) ;
#28486 = CARTESIAN_POINT ( 'NONE',  ( 5.799999999999999822, 4.618802153517001408, -8.000000000000000000 ) ) ;
#28488 = CARTESIAN_POINT ( 'NONE',  ( -133.2386331335365242, 52.76072997738348391, -94.50456680151590660 ) ) ;
#28487 = B_SPLINE_CURVE_WITH_KNOTS ( 'NONE', 3,
 ( #8784, #14401, #24958, #67517, #35851, #57305, #52368, #31270, #62928, #18976, #68211, #14728, #61870, #40427, #20021, #20349, #52023, #9463, #41818, #9810, #9115, #25308, #30573, #13698, #3837, #46739, #36194, #19316, #30924, #35150, #40771, #14044, #35503, #25653, #63272, #56964, #15080, #36543, #54064, #11172 ),
 .UNSPECIFIED., .F., .F.,
 ( 4, 2, 2, 2, 2, 2, 2, 2, 2, 2, 2, 2, 2, 2, 2, 2, 2, 2, 2, 4 ),
 ( 0.02454308262169000235, 0.02608670964102868459, 0.02685852315069804305, 0.02763033666036740499, 0.02917396367970614274, 0.02994577718937551161, 0.03071759069904488049, 0.03226121771838367375, 0.03303303122805310160, 0.03380484473772252946, 0.03534847175706141986, 0.03689209877640031721, 0.03843572579573920067, 0.03997935281507809802, 0.04152297983441698148, 0.04306660685375587189, 0.04461023387309476229, 0.04615386089243365270, 0.04769748791177254310, 0.04924111493111143351 ),
 .UNSPECIFIED. ) ;
#28489 = CARTESIAN_POINT ( 'NONE',  ( -190.6985136298601731, 109.1272424661242582, 94.99999999999866418 ) ) ;
#28490 = PRODUCT_RELATED_PRODUCT_CATEGORY ( 'part', '', ( #52880 ) ) ;
#28491 = EDGE_LOOP ( 'NONE', ( #50458, #6771, #5824, #15219, #43264, #15398, #10187, #31283 ) ) ;
#28493 = EDGE_CURVE ( 'NONE', #42670, #62968, #38570, .T. ) ;
#28492 = AXIS2_PLACEMENT_3D ( 'NONE', #7267, #55435, #50518 ) ;
#28494 = EDGE_CURVE ( 'NONE', #51562, #27030, #32141, .T. ) ;
#28495 = ORIENTED_EDGE ( 'NONE', *, *, #44221, .T. ) ;
#28496 = AXIS2_PLACEMENT_3D ( 'NONE', #52854, #58154, #52184 ) ;
#28497 = CARTESIAN_POINT ( 'NONE',  ( 15.78827728214693416, 6.500811158483329244, 45.01470767270524931 ) ) ;
#28498 = VERTEX_POINT ( 'NONE', #18864 ) ;
#28499 = EDGE_CURVE ( 'NONE', #5653, #44052, #50128, .T. ) ;
#28500 = CARTESIAN_POINT ( 'NONE',  ( 31.89651141207616192, -56.63578868294582946, 40.00000000000003553 ) ) ;
#28501 = AXIS2_PLACEMENT_3D ( 'NONE', #36626, #42242, #21466 ) ;
#28502 = AXIS2_PLACEMENT_3D ( 'NONE', #42883, #10532, #52750 ) ;
#28503 = VERTEX_POINT ( 'NONE', #56142 ) ;
#28504 = CARTESIAN_POINT ( 'NONE',  ( -148.6426981422628728, 63.44891673852540492, -76.62003570338966085 ) ) ;
#28505 = CARTESIAN_POINT ( 'NONE',  ( 89.22118407503263882, 20.32164250407901207, 17.40952166681993063 ) ) ;
#28506 = CARTESIAN_POINT ( 'NONE',  ( -442.6627218934912662, 394.9999999999998295, 103.5502958579880612 ) ) ;
#28507 = ORIENTED_EDGE ( 'NONE', *, *, #67432, .T. ) ;
#28508 = DIRECTION ( 'NONE',  ( -0.000000000000000000, -0.000000000000000000, -1.000000000000000000 ) ) ;
#28509 = DIRECTION ( 'NONE',  ( -1.000000000000000000, -3.697785493223490648E-32, 0.000000000000000000 ) ) ;
#28510 = CARTESIAN_POINT ( 'NONE',  ( 38.42095780754793566, 9.297684251045559733, 44.86571034329109153 ) ) ;
#28511 = CARTESIAN_POINT ( 'NONE',  ( -179.5109681715918555, 96.11572638569522553, -46.17695725115778771 ) ) ;
#28512 = DIRECTION ( 'NONE',  ( 0.000000000000000000, -0.000000000000000000, 1.000000000000000000 ) ) ;
#28513 = CARTESIAN_POINT ( 'NONE',  ( -149.1099326198686583, 63.84262089027424736, -88.50193171241930656 ) ) ;
#28514 = EDGE_CURVE ( 'NONE', #10774, #12136, #39622, .T. ) ;
#28515 = CARTESIAN_POINT ( 'NONE',  ( 127.4953815656694758, 37.71366486045442912, -66.36346676285383239 ) ) ;
#28516 = VERTEX_POINT ( 'NONE', #19192 ) ;
#28517 = CARTESIAN_POINT ( 'NONE',  ( 138.5943620234098717, 45.55242290395135285, -76.20239256362549440 ) ) ;
#28519 = EDGE_CURVE ( 'NONE', #8171, #32531, #39966, .T. ) ;
#28518 = DIRECTION ( 'NONE',  ( -0.000000000000000000, -0.000000000000000000, 1.000000000000000000 ) ) ;
#28520 = VERTEX_POINT ( 'NONE', #2343 ) ;
#28521 = CARTESIAN_POINT ( 'NONE',  ( -149.5074843970971017, 65.50121172469319220, -49.81283053149199702 ) ) ;
#28522 = CARTESIAN_POINT ( 'NONE',  ( -4.081377963939778475, 6.676029627840592617, -76.26587694573117915 ) ) ;
#28523 = CARTESIAN_POINT ( 'NONE',  ( -38.93847286785604211, 11.96870349976818204, 37.20973207589809562 ) ) ;
#28524 = CARTESIAN_POINT ( 'NONE',  ( 0.000000000000000000, 0.000000000000000000, 0.000000000000000000 ) ) ;
#28525 = DIRECTION ( 'NONE',  ( -0.000000000000000000, -0.000000000000000000, -1.000000000000000000 ) ) ;
#28526 = LINE ( 'NONE', #44343, #58001 ) ;
#28527 = CARTESIAN_POINT ( 'NONE',  ( -11.10395507987084329, 7.126520090179309541, -89.84858484025937742 ) ) ;
#28528 = CARTESIAN_POINT ( 'NONE',  ( -17.50000000000002842, 207.5000000000000284, 0.000000000000000000 ) ) ;
#28529 = CARTESIAN_POINT ( 'NONE',  ( 429.8372781065085633, 400.0000000000000568, -128.9497041420118251 ) ) ;
#28530 = CARTESIAN_POINT ( 'NONE',  ( -11.57950265606958418, 8.174070387114797498, 44.11303985588816090 ) ) ;
#28531 = CARTESIAN_POINT ( 'NONE',  ( 117.7411475730015269, 32.50808475802731579, 9.724032258917603144 ) ) ;
#28532 = CARTESIAN_POINT ( 'NONE',  ( 0.000000000000000000, -26.09918303830819397, 30.00000000000000000 ) ) ;
#28533 = ORIENTED_EDGE ( 'NONE', *, *, #29174, .T. ) ;
#28534 = MECHANICAL_DESIGN_GEOMETRIC_PRESENTATION_REPRESENTATION (  '', ( #36365 ), #57712 ) ;
#28535 = CARTESIAN_POINT ( 'NONE',  ( -95.60805465865863084, 30.63099276904602775, -45.97777768882416893 ) ) ;
#28536 = VERTEX_POINT ( 'NONE', #13923 ) ;
#28537 = LINE ( 'NONE', #44719, #16075 ) ;
#28538 = DIRECTION ( 'NONE',  ( -0.3090169943749582759, 0.9510565162951499785, 0.000000000000000000 ) ) ;
#28539 = CARTESIAN_POINT ( 'NONE',  ( 39.89571693415784637, 8.473773298340393723, 71.75838489642697482 ) ) ;
#28540 = DIRECTION ( 'NONE',  ( 0.000000000000000000, 0.000000000000000000, 1.000000000000000000 ) ) ;
#28541 = LINE ( 'NONE', #66542, #28890 ) ;
#28542 = CARTESIAN_POINT ( 'NONE',  ( -63.73419499958981049, -12.83646726144931449, 0.000000000000000000 ) ) ;
#28543 = CIRCLE ( 'NONE', #20645, 19.99999999999998934 ) ;
#28544 = CARTESIAN_POINT ( 'NONE',  ( 62.20483532083785860, 13.51802415804941937, -89.44279409927861479 ) ) ;
#28545 = CARTESIAN_POINT ( 'NONE',  ( -124.7710763417278201, 46.96042092553521030, -22.98812073115930232 ) ) ;
#28546 = VERTEX_POINT ( 'NONE', #34706 ) ;
#28547 = CONICAL_SURFACE ( 'NONE', #58805, 65.00000000000000000, 0.7853981633974497223 ) ;
#28548 = ORIENTED_EDGE ( 'NONE', *, *, #33614, .F. ) ;
#28549 = CIRCLE ( 'NONE', #8371, 74.95140232871122521 ) ;
#28550 = DIRECTION ( 'NONE',  ( 0.000000000000000000, -1.000000000000000000, 0.000000000000000000 ) ) ;
#28551 = CARTESIAN_POINT ( 'NONE',  ( 174.1251613516844259, 71.84747073139214990, 66.50424727365492572 ) ) ;
#28552 = DIRECTION ( 'NONE',  ( 0.000000000000000000, 0.000000000000000000, 1.000000000000000000 ) ) ;
#28553 = CARTESIAN_POINT ( 'NONE',  ( -166.0031475600389115, 80.98114714564771077, 67.54672357681444339 ) ) ;
#28554 = CIRCLE ( 'NONE', #67879, 5.000000000000000000 ) ;
#28555 = CARTESIAN_POINT ( 'NONE',  ( -166.2065256787326177, 81.19093426984588291, -12.44839775261722181 ) ) ;
#28556 = VECTOR ( 'NONE', #7458, 1000.000000000000000 ) ;
#28557 = LINE ( 'NONE', #6402, #13944 ) ;
#28558 = EDGE_LOOP ( 'NONE', ( #52748, #23368 ) ) ;
#28559 = CARTESIAN_POINT ( 'NONE',  ( 109.3154830994003532, 29.56170298203815605, -50.87960775427016813 ) ) ;
#28560 = CARTESIAN_POINT ( 'NONE',  ( 157.4703587214989113, 57.65129005721576050, -62.96873488960130771 ) ) ;
#28561 = CARTESIAN_POINT ( 'NONE',  ( 15.29912143387263690, 7.491799981865499447, 56.85925826316893250 ) ) ;
#28562 = CARTESIAN_POINT ( 'NONE',  ( 3.000000000000006217, 0.000000000000000000, 0.000000000000000000 ) ) ;
#28563 = DIRECTION ( 'NONE',  ( -0.000000000000000000, 1.000000000000000000, -0.000000000000000000 ) ) ;
#28564 = FACE_BOUND ( 'NONE', #68626, .T. ) ;
#28565 = CARTESIAN_POINT ( 'NONE',  ( -62.30100056228381789, 16.74548393487071252, -40.72482722506486397 ) ) ;
#28566 = VERTEX_POINT ( 'NONE', #35387 ) ;
#28567 = FACE_OUTER_BOUND ( 'NONE', #17069, .T. ) ;
#28568 = CARTESIAN_POINT ( 'NONE',  ( 87.10672734544985474, 20.64813880796636170, -50.82156419891173016 ) ) ;
#28569 = CARTESIAN_POINT ( 'NONE',  ( 61.28323125814129213, -21.66484633135379667, 170.0000000000000000 ) ) ;
#28570 = CARTESIAN_POINT ( 'NONE',  ( -175.9864315813574080, 91.91454246454364352, 4.533208682208026197 ) ) ;
#28571 = CARTESIAN_POINT ( 'NONE',  ( 205.5130322755755401, 109.1888880665735542, 71.05227132923313604 ) ) ;
#28572 = CARTESIAN_POINT ( 'NONE',  ( 84.05098130332766004, 18.55728792516086401, -63.11908039286798555 ) ) ;
#28573 = EDGE_CURVE ( 'NONE', #58185, #41538, #2681, .T. ) ;
#28574 = ORIENTED_EDGE ( 'NONE', *, *, #34734, .T. ) ;
#28575 = CARTESIAN_POINT ( 'NONE',  ( 59.95259601283823514, 11.98300577492410390, 3.618069386873109305 ) ) ;
#28576 = CARTESIAN_POINT ( 'NONE',  ( -58.76006735892197241, 15.70681061434692261, 58.13766844807554435 ) ) ;
#28577 = EDGE_CURVE ( 'NONE', #34081, #58070, #45936, .T. ) ;
#28578 = ORIENTED_EDGE ( 'NONE', *, *, #50654, .F. ) ;
#28579 = CARTESIAN_POINT ( 'NONE',  ( -65.36598343705435354, 0.000000000000000000, 41.38025477438755928 ) ) ;
#28580 = EDGE_LOOP ( 'NONE', ( #3433, #47277, #1995, #8119 ) ) ;
#28581 = AXIS2_PLACEMENT_3D ( 'NONE', #66162, #11264, #64746 ) ;
#28582 = PLANE ( 'NONE',  #4941 ) ;
#28583 = CARTESIAN_POINT ( 'NONE',  ( -62.14837099232443762, 17.75045801599140205, -13.42952458767598856 ) ) ;
#28584 = EDGE_CURVE ( 'NONE', #45708, #33533, #62107, .T. ) ;
#28585 = CARTESIAN_POINT ( 'NONE',  ( 157.4703587214989398, -170.0000000000000000, 29.40946747225336466 ) ) ;
#28586 = ORIENTED_EDGE ( 'NONE', *, *, #67836, .T. ) ;
#28587 = VECTOR ( 'NONE', #41450, 1000.000000000000000 ) ;
#28588 = ADVANCED_FACE ( 'NONE', ( #7960 ), #40651, .T. ) ;
#28589 = ORIENTED_EDGE ( 'NONE', *, *, #19182, .F. ) ;
#28590 = CARTESIAN_POINT ( 'NONE',  ( 43.14669449386823885, 9.942681284149136545, 70.77495916275495347 ) ) ;
#28591 = CARTESIAN_POINT ( 'NONE',  ( 164.4760519199596160, 64.62478832434435105, 39.63968248660635396 ) ) ;
#28592 = CARTESIAN_POINT ( 'NONE',  ( -155.7455325080991599, 71.01834415181984639, -64.98546709743690997 ) ) ;
#28593 = CARTESIAN_POINT ( 'NONE',  ( 66.73431804020508196, 14.60294556126668475, 3.950658298317914596 ) ) ;
#28594 = VECTOR ( 'NONE', #35053, 1000.000000000000000 ) ;
#28595 = CARTESIAN_POINT ( 'NONE',  ( 86.62931800182292363, 19.42108912189597092, 44.71208757247933363 ) ) ;
#28596 = ORIENTED_EDGE ( 'NONE', *, *, #17755, .T. ) ;
#28597 = AXIS2_PLACEMENT_3D ( 'NONE', #11305, #38754, #17645 ) ;
#28598 = AXIS2_PLACEMENT_3D ( 'NONE', #5813, #37139, #26932 ) ;
#28599 = FACE_OUTER_BOUND ( 'NONE', #16171, .T. ) ;
#28600 = CYLINDRICAL_SURFACE ( 'NONE', #5067, 7.500000000000013323 ) ;
#28601 = AXIS2_PLACEMENT_3D ( 'NONE', #34493, #1775, #1071 ) ;
#28602 = CARTESIAN_POINT ( 'NONE',  ( -133.3923804760465543, 52.87100816290224969, -16.13643682761781761 ) ) ;
#28604 = EDGE_CURVE ( 'NONE', #15890, #10200, #45588, .T. ) ;
#28603 = FACE_OUTER_BOUND ( 'NONE', #36485, .T. ) ;
#28605 = PLANE ( 'NONE',  #166 ) ;
#28606 = DIRECTION ( 'NONE',  ( -0.000000000000000000, 1.000000000000000000, -0.000000000000000000 ) ) ;
#28608 = VERTEX_POINT ( 'NONE', #23796 ) ;
#28607 = DIRECTION ( 'NONE',  ( 1.000000000000000000, 0.000000000000000000, 0.000000000000000000 ) ) ;
#28609 = ORIENTED_EDGE ( 'NONE', *, *, #18265, .F. ) ;
#28610 = ORIENTED_EDGE ( 'NONE', *, *, #5690, .F. ) ;
#28611 = DIRECTION ( 'NONE',  ( 1.000000000000000000, 0.000000000000000000, 0.000000000000000000 ) ) ;
#28612 = CARTESIAN_POINT ( 'NONE',  ( 175.5498284945444709, 74.57669191966279243, 4.876327785689846372 ) ) ;
#28613 = DIRECTION ( 'NONE',  ( -1.850371928290090422E-16, 1.000000000000000000, 1.110223024625156171E-16 ) ) ;
#28614 = CARTESIAN_POINT ( 'NONE',  ( 107.9301116202191793, 27.82606182274595241, -23.72815433879570790 ) ) ;
#28615 = CARTESIAN_POINT ( 'NONE',  ( 141.0229350107040887, 45.92325889728665800, -95.00000000000133582 ) ) ;
#28616 = CARTESIAN_POINT ( 'NONE',  ( -58.32502757340553501, 16.62877055630752920, -49.48199589557358280 ) ) ;
#28617 = DIRECTION ( 'NONE',  ( 4.852411958229186445E-18, -1.576644219464734062E-18, -1.000000000000000000 ) ) ;
#28618 = DIRECTION ( 'NONE',  ( -1.020422603260505347E-14, 1.000000000000000000, 5.551115123125782702E-17 ) ) ;
#28619 = CARTESIAN_POINT ( 'NONE',  ( -14.19447842053094178, 7.389800932646232390, 41.58366191049604055 ) ) ;
#28620 = ORIENTED_EDGE ( 'NONE', *, *, #37114, .T. ) ;
#28621 = LINE ( 'NONE', #44798, #66632 ) ;
#28622 = EDGE_LOOP ( 'NONE', ( #32143, #17002, #52097, #52078 ) ) ;
#28623 = EDGE_LOOP ( 'NONE', ( #33068, #12410 ) ) ;
#28624 = CARTESIAN_POINT ( 'NONE',  ( -836.0476379851789943, -568.5227338237882577, 10.00000000000000000 ) ) ;
#28625 = CARTESIAN_POINT ( 'NONE',  ( -171.4943428135323131, 86.82484920477510570, 45.69172056196202192 ) ) ;
#28626 = CARTESIAN_POINT ( 'NONE',  ( 117.6924004117966689, 33.61107268965020012, -17.59174222879768834 ) ) ;
#28627 = CARTESIAN_POINT ( 'NONE',  ( -105.4556185321791304, 34.42302275449793569, 17.98560306758872329 ) ) ;
#28628 = DIRECTION ( 'NONE',  ( -0.000000000000000000, 1.000000000000000000, -0.000000000000000000 ) ) ;
#28629 = CARTESIAN_POINT ( 'NONE',  ( 136.9822423813093337, 44.53121110416873307, -23.50049531503082889 ) ) ;
#28630 = ORIENTED_EDGE ( 'NONE', *, *, #39488, .T. ) ;
#28631 = ORIENTED_EDGE ( 'NONE', *, *, #45480, .F. ) ;
#28632 = ORIENTED_EDGE ( 'NONE', *, *, #29785, .T. ) ;
#28633 = CIRCLE ( 'NONE', #3930, 74.95140232871122521 ) ;
#28634 = LINE ( 'NONE', #55353, #14737 ) ;
#28635 = CYLINDRICAL_SURFACE ( 'NONE', #3838, 7.500000000000013323 ) ;
#28636 = LINE ( 'NONE', #8225, #19910 ) ;
#28637 = CARTESIAN_POINT ( 'NONE',  ( 47.73902449249082025, -57.85799893277825845, 43.58025477438756923 ) ) ;
#28638 = AXIS2_PLACEMENT_3D ( 'NONE', #12756, #44766, #66932 ) ;
#28639 = LINE ( 'NONE', #23013, #49474 ) ;
#28640 = CARTESIAN_POINT ( 'NONE',  ( -102.2801239173131052, 32.78103895658057354, -23.17002667451225406 ) ) ;
#28641 = ORIENTED_EDGE ( 'NONE', *, *, #44714, .F. ) ;
#28642 = VECTOR ( 'NONE', #33288, 1000.000000000000114 ) ;
#28643 = AXIS2_PLACEMENT_3D ( 'NONE', #49468, #37893, #26648 ) ;
#28644 = CARTESIAN_POINT ( 'NONE',  ( 39.54205320694412507, -51.58901073076707888, 170.0000000000000000 ) ) ;
#28645 = CARTESIAN_POINT ( 'NONE',  ( 197.5344630110112121, 98.61758706718741507, -72.91483488310812788 ) ) ;
#28646 = EDGE_CURVE ( 'NONE', #38367, #69371, #66379, .T. ) ;
#28647 = CARTESIAN_POINT ( 'NONE',  ( 280.0000000000000000, -21.42428528562853529, -4.999999999999990230 ) ) ;
#28648 = SURFACE_SIDE_STYLE ('',( #45162 ) ) ;
#28649 = CARTESIAN_POINT ( 'NONE',  ( 396.6937511374966334, 500.0000000000000000, -51.64566090791306863 ) ) ;
#28650 = LINE ( 'NONE', #39894, #22822 ) ;
#28651 = VECTOR ( 'NONE', #58634, 1000.000000000000114 ) ;
#28652 = FACE_BOUND ( 'NONE', #30350, .T. ) ;
#28653 = CARTESIAN_POINT ( 'NONE',  ( 100.0000000000000284, 0.000000000000000000, 20.00000000000001421 ) ) ;
#28654 = VECTOR ( 'NONE', #20714, 1000.000000000000114 ) ;
#28655 = B_SPLINE_CURVE_WITH_KNOTS ( 'NONE', 3,
 ( #43393, #64163, #32165, #57857, #36405, #15975, #64514, #69439, #53595, #16322, #42022, #5072, #63481, #36752, #5426, #52906, #4728, #26193, #58529, #47628, #69081, #20915, #42366, #15638, #37089, #31813, #53246, #26879, #42705, #137, #26540, #11041, #48303, #59221, #32503, #18073, #28260, #2247, #844, #12096, #50427, #54283, #66281, #12797 ),
 .UNSPECIFIED., .F., .F.,
 ( 4, 2, 2, 2, 2, 2, 2, 2, 2, 2, 2, 2, 2, 2, 2, 2, 2, 2, 2, 2, 2, 4 ),
 ( 0.000000000000000000, 0.001487235713946821964, 0.002230853570920213538, 0.002974471427893605763, 0.004461707141840350749, 0.005948942855787096168, 0.007436178569733841587, 0.008179796426707214296, 0.008923414283680587006, 0.01041064999762734804, 0.01189788571157410907, 0.01264150356854749566, 0.01338512142552088224, 0.01487235713946764674, 0.01561597499644103507, 0.01635959285341442512, 0.01784682856736120524, 0.01933406428130798535, 0.02007768213828137541, 0.02082129999525476199, 0.02230853570920153170, 0.02379577142314830140 ),
 .UNSPECIFIED. ) ;
#28656 = AXIS2_PLACEMENT_3D ( 'NONE', #40282, #65989, #61725 ) ;
#28657 = VERTEX_POINT ( 'NONE', #17824 ) ;
#28658 = CARTESIAN_POINT ( 'NONE',  ( 276.6972452105824800, 21.67615690170940468, -3.768214559138908015 ) ) ;
#28659 = CARTESIAN_POINT ( 'NONE',  ( -133.0808647576834005, 51.41195281028755915, -67.09815806457598342 ) ) ;
#28660 = CARTESIAN_POINT ( 'NONE',  ( 26.99999999999999645, -27.00000000000000355, 12.00000000000000000 ) ) ;
#28661 = CARTESIAN_POINT ( 'NONE',  ( -125.8938041572051105, 46.49392987655495091, 72.46449846362081360 ) ) ;
#28662 = DIRECTION ( 'NONE',  ( 0.000000000000000000, 0.000000000000000000, -1.000000000000000000 ) ) ;
#28663 = ORIENTED_EDGE ( 'NONE', *, *, #632, .F. ) ;
#28664 = DIRECTION ( 'NONE',  ( 0.000000000000000000, 0.000000000000000000, 1.000000000000000000 ) ) ;
#28665 = CARTESIAN_POINT ( 'NONE',  ( 188.5164425382173192, 86.45836816134917058, 91.57835675204685799 ) ) ;
#28666 = EDGE_CURVE ( 'NONE', #51932, #5346, #60723, .T. ) ;
#28667 = ORIENTED_EDGE ( 'NONE', *, *, #38257, .T. ) ;
#28668 = VERTEX_POINT ( 'NONE', #35043 ) ;
#28669 = CARTESIAN_POINT ( 'NONE',  ( 173.5837434292113812, 71.34409607026158540, -44.01311006594448827 ) ) ;
#28670 = CARTESIAN_POINT ( 'NONE',  ( -178.0633751203917825, 92.80295726428047942, -63.41043722487919609 ) ) ;
#28671 = CARTESIAN_POINT ( 'NONE',  ( 26.99999999999999289, 29.99999999999999645, 12.00000000000000000 ) ) ;
#28672 = ORIENTED_EDGE ( 'NONE', *, *, #57352, .F. ) ;
#28673 = CARTESIAN_POINT ( 'NONE',  ( 50.97490815085634352, 6.000000000000000000, -46.68900338898716029 ) ) ;
#28674 = CARTESIAN_POINT ( 'NONE',  ( -180.3158531669106424, 95.51092859788509770, 9.337317216626621175 ) ) ;
#28675 = CARTESIAN_POINT ( 'NONE',  ( -76.10397364431021572, 21.36211154336728768, -49.66815503544774657 ) ) ;
#28676 = EDGE_CURVE ( 'NONE', #2074, #44289, #11680, .T. ) ;
#28677 = CARTESIAN_POINT ( 'NONE',  ( 79.66256042745894206, 17.16036700714778718, -94.20191509326981816 ) ) ;
#28678 = CARTESIAN_POINT ( 'NONE',  ( -29.87147652227456263, -74.98256102853682137, 73.58025477438756923 ) ) ;
#28679 = CARTESIAN_POINT ( 'NONE',  ( -50.53243683205842984, 14.55237037207940887, -9.867349686703617451 ) ) ;
#28680 = B_SPLINE_CURVE_WITH_KNOTS ( 'NONE', 3,
 ( #55429, #28715, #1278, #34350, #55790, #7614 ),
 .UNSPECIFIED., .F., .F.,
 ( 4, 2, 4 ),
 ( 0.03218939915585355971, 0.06469836417558699759, 0.09720732919532043548 ),
 .UNSPECIFIED. ) ;
#28681 = ORIENTED_EDGE ( 'NONE', *, *, #66338, .T. ) ;
#28682 = CARTESIAN_POINT ( 'NONE',  ( -149.5074843970971017, 65.50121172469319220, 72.56537183036277838 ) ) ;
#28683 = AXIS2_PLACEMENT_3D ( 'NONE', #42280, #41587, #20822 ) ;
#28684 = CARTESIAN_POINT ( 'NONE',  ( -71.15374617000810531, 20.66492714610677339, 11.08381322999615293 ) ) ;
#28685 = EDGE_CURVE ( 'NONE', #64974, #27768, #24289, .T. ) ;
#28686 = DIRECTION ( 'NONE',  ( -0.6910626489868580968, -0.7227948638273978821, 0.000000000000000000 ) ) ;
#28687 = CARTESIAN_POINT ( 'NONE',  ( -166.7136514167008841, 81.71618216218797670, -72.96353840939907798 ) ) ;
#28688 = VECTOR ( 'NONE', #26443, 1000.000000000000000 ) ;
#28690 = ORIENTED_EDGE ( 'NONE', *, *, #58213, .T. ) ;
#28689 = CARTESIAN_POINT ( 'NONE',  ( -133.2683599795575446, 51.54537714913664814, 90.40267370649584677 ) ) ;
#28691 = CARTESIAN_POINT ( 'NONE',  ( 83.38067517854670996, 18.33799117207140483, -50.08583960832021376 ) ) ;
#28692 = EDGE_CURVE ( 'NONE', #44289, #11417, #46271, .T. ) ;
#28693 = ADVANCED_FACE ( 'NONE', ( #41358 ), #10031, .F. ) ;
#28694 = AXIS2_PLACEMENT_3D ( 'NONE', #22044, #68837, #20661 ) ;
#28695 = CIRCLE ( 'NONE', #20798, 25.00000000000000000 ) ;
#28696 = ORIENTED_EDGE ( 'NONE', *, *, #40501, .F. ) ;
#28697 = CARTESIAN_POINT ( 'NONE',  ( -129.6165111262477865, 48.99406349865703447, 31.60480352819717353 ) ) ;
#28698 = CARTESIAN_POINT ( 'NONE',  ( 412.3372781065085633, 179.4906275429376024, 111.5502958579881749 ) ) ;
#28699 = CARTESIAN_POINT ( 'NONE',  ( -74.69807204964287450, -6.722948167758066695, 43.58025477438756212 ) ) ;
#28701 = CARTESIAN_POINT ( 'NONE',  ( 89.65730223173024172, 21.54473673261223610, 30.34629236393602625 ) ) ;
#28700 = TOROIDAL_SURFACE ( 'NONE', #4000, 24.69999999999999929, 0.3000000000000035971 ) ;
#28702 = CARTESIAN_POINT ( 'NONE',  ( -121.5921196778231490, 43.72569502503144179, 58.80275198742250353 ) ) ;
#28703 = CARTESIAN_POINT ( 'NONE',  ( -442.6627218934913230, 399.9999999999997726, 108.5502958579881891 ) ) ;
#28704 = CARTESIAN_POINT ( 'NONE',  ( -180.5200658187031877, 97.35517482626552521, -16.63434712722808229 ) ) ;
#28705 = CIRCLE ( 'NONE', #5086, 8.000000000000000000 ) ;
#28706 = CARTESIAN_POINT ( 'NONE',  ( -53.14657859411973817, 15.21831473227210552, 45.07509434600507348 ) ) ;
#28707 = EDGE_LOOP ( 'NONE', ( #61129, #56088 ) ) ;
#28708 = APPLICATION_CONTEXT ( 'automotive_design' ) ;
#28709 = EDGE_LOOP ( 'NONE', ( #1351, #21069, #7850, #22419 ) ) ;
#28710 = LINE ( 'NONE', #65649, #18125 ) ;
#28711 = CARTESIAN_POINT ( 'NONE',  ( 198.7029050523552201, 98.46895521196213963, -12.44553174149221064 ) ) ;
#28712 = DIRECTION ( 'NONE',  ( -0.000000000000000000, -1.000000000000000000, -0.000000000000000000 ) ) ;
#28713 = FACE_OUTER_BOUND ( 'NONE', #53561, .T. ) ;
#28714 = CARTESIAN_POINT ( 'NONE',  ( 212.0803491126037272, 118.9047894217573571, -42.46139465240390365 ) ) ;
#28715 = CARTESIAN_POINT ( 'NONE',  ( 14.72760812434781208, 30.00634360379971000, 6.893342934305382030 ) ) ;
#28716 = LINE ( 'NONE', #1626, #3410 ) ;
#28717 = DIRECTION ( 'NONE',  ( -0.000000000000000000, 1.000000000000000000, -0.000000000000000000 ) ) ;
#28718 = CARTESIAN_POINT ( 'NONE',  ( -31.11269837220804035, 15.55634918610408945, 2.000000000000001776 ) ) ;
#28719 = ORIENTED_EDGE ( 'NONE', *, *, #48640, .T. ) ;
#28720 = ORIENTED_EDGE ( 'NONE', *, *, #54042, .F. ) ;
#28721 = CARTESIAN_POINT ( 'NONE',  ( -19.46539569203812903, -15.68752276659308365, 0.000000000000000000 ) ) ;
#28722 = CARTESIAN_POINT ( 'NONE',  ( -74.87059534020256990, 20.91186903862810098, 85.13133443590446348 ) ) ;
#28723 = DIRECTION ( 'NONE',  ( 0.8584487936018728726, -0.5128992774058949156, 0.000000000000000000 ) ) ;
#28724 = CARTESIAN_POINT ( 'NONE',  ( 129.1310456962234809, 39.80382822048402147, 31.16611068083063074 ) ) ;
#28725 = CARTESIAN_POINT ( 'NONE',  ( 107.7808008216759390, -21.53681828009572286, -4.492424461587423146 ) ) ;
#28726 = DIRECTION ( 'NONE',  ( -1.000000000000000000, -0.000000000000000000, -0.000000000000000000 ) ) ;
#28727 = CARTESIAN_POINT ( 'NONE',  ( -95.60805465865863084, 30.63099276904604906, -19.13322709836046442 ) ) ;
#28728 = CARTESIAN_POINT ( 'NONE',  ( 60.61895554631703931, 13.15982272268127851, 44.43620800597218334 ) ) ;
#28729 = DIRECTION ( 'NONE',  ( -0.9510565162951544194, 0.3090169943749446757, 0.000000000000000000 ) ) ;
#28731 = ORIENTED_EDGE ( 'NONE', *, *, #63763, .T. ) ;
#28730 = ADVANCED_FACE ( 'NONE', ( #35739 ), #47299, .F. ) ;
#28732 = CARTESIAN_POINT ( 'NONE',  ( 55.57634120535664124, 12.09544293553730476, 65.14168292286281314 ) ) ;
#28733 = PLANE ( 'NONE',  #66663 ) ;
#28734 = CARTESIAN_POINT ( 'NONE',  ( -14.93280618462406473, 8.469244267267914239, 13.17839159822831441 ) ) ;
#28735 = DIRECTION ( 'NONE',  ( -1.000000000000000000, 0.000000000000000000, 0.000000000000000000 ) ) ;
#28736 = DIRECTION ( 'NONE',  ( 0.000000000000000000, 0.000000000000000000, -1.000000000000000000 ) ) ;
#28737 = CARTESIAN_POINT ( 'NONE',  ( 132.2818448028687612, 41.65267246304674842, -24.01511195972667778 ) ) ;
#28738 = EDGE_CURVE ( 'NONE', #47361, #14330, #31018, .T. ) ;
#28739 = AXIS2_PLACEMENT_3D ( 'NONE', #567, #17073, #22019 ) ;
#28740 = EDGE_LOOP ( 'NONE', ( #62684, #63912, #33441, #13187 ) ) ;
#28741 = CONICAL_SURFACE ( 'NONE', #14123, 65.00000000000000000, 0.7853981633974497223 ) ;
#28742 = DIRECTION ( 'NONE',  ( -0.000000000000000000, -1.000000000000000000, -0.000000000000000000 ) ) ;
#28743 = CARTESIAN_POINT ( 'NONE',  ( -34.52542994698664813, 11.14027065218092005, -35.97735163564012595 ) ) ;
#28744 = CARTESIAN_POINT ( 'NONE',  ( -165.9121868482146454, 80.88751546905565704, -44.30229986177329238 ) ) ;
#28745 = CONTEXT_DEPENDENT_SHAPE_REPRESENTATION ( #22425, #43308 ) ;
#28746 = CYLINDRICAL_SURFACE ( 'NONE', #10799, 7.500000000000013323 ) ;
#28747 = VERTEX_POINT ( 'NONE', #3710 ) ;
#28749 = CARTESIAN_POINT ( 'NONE',  ( 0.000000000000000000, 0.000000000000000000, 41.38025477438755928 ) ) ;
#28748 = VECTOR ( 'NONE', #5104, 1000.000000000000000 ) ;
#28750 = AXIS2_PLACEMENT_3D ( 'NONE', #31766, #53197, #5025 ) ;
#28751 = DIRECTION ( 'NONE',  ( 0.7530714660036195163, -0.6579387259397027066, 0.000000000000000000 ) ) ;
#28752 =( GEOMETRIC_REPRESENTATION_CONTEXT ( 3 ) GLOBAL_UNCERTAINTY_ASSIGNED_CONTEXT ( ( #20493 ) ) GLOBAL_UNIT_ASSIGNED_CONTEXT ( ( #46034, #34465, #35488 ) ) REPRESENTATION_CONTEXT ( 'NONE', 'WORKASPACE' ) );
#28753 = ADVANCED_FACE ( 'NONE', ( #52589 ), #4070, .F. ) ;
#28754 = CARTESIAN_POINT ( 'NONE',  ( -142.9728934044262019, 58.82891228489263113, -19.18790406048661268 ) ) ;
#28755 = VECTOR ( 'NONE', #13802, 1000.000000000000227 ) ;
#28756 = DIRECTION ( 'NONE',  ( 0.000000000000000000, 0.000000000000000000, 1.000000000000000000 ) ) ;
#28757 = EDGE_CURVE ( 'NONE', #8520, #2392, #4408, .T. ) ;
#28758 = DIRECTION ( 'NONE',  ( -0.000000000000000000, 1.000000000000000000, -0.000000000000000000 ) ) ;
#28759 = EDGE_CURVE ( 'NONE', #3025, #65848, #39119, .T. ) ;
#28760 = ORIENTED_EDGE ( 'NONE', *, *, #28646, .F. ) ;
#28761 = CARTESIAN_POINT ( 'NONE',  ( -61.41100614348690101, 43.07262267896644659, 43.58025477438756923 ) ) ;
#28762 = CARTESIAN_POINT ( 'NONE',  ( 85.67165909753201447, 20.15791549876374944, 17.82174123723708448 ) ) ;
#28763 = CARTESIAN_POINT ( 'NONE',  ( -96.43817545481741149, 31.02509717589736127, 33.28916959688606880 ) ) ;
#28764 = EDGE_CURVE ( 'NONE', #40747, #67789, #38401, .T. ) ;
#28765 = CARTESIAN_POINT ( 'NONE',  ( -7.825402957745085430, 7.899365992529253866, -89.10717191287116634 ) ) ;
#28767 = ORIENTED_EDGE ( 'NONE', *, *, #1016, .T. ) ;
#28766 = DIRECTION ( 'NONE',  ( 0.000000000000000000, 0.000000000000000000, 1.000000000000000000 ) ) ;
#28768 = CARTESIAN_POINT ( 'NONE',  ( 55.90910788310613810, 11.13585330978400911, 39.76043137525509508 ) ) ;
#28769 = VERTEX_POINT ( 'NONE', #54917 ) ;
#28770 = ORIENTED_EDGE ( 'NONE', *, *, #54297, .T. ) ;
#28771 = CARTESIAN_POINT ( 'NONE',  ( -78.66644367742111399, 22.32174330031316956, -8.270900041254197532 ) ) ;
#28772 = EDGE_CURVE ( 'NONE', #6708, #13790, #16660, .T. ) ;
#28773 = LINE ( 'NONE', #11522, #24847 ) ;
#28775 = ORIENTED_EDGE ( 'NONE', *, *, #42928, .F. ) ;
#28774 = CARTESIAN_POINT ( 'NONE',  ( -9.524904342798460988, 8.016391612076533946, -77.07167657488317047 ) ) ;
#28776 = FACE_OUTER_BOUND ( 'NONE', #36380, .T. ) ;
#28777 = CARTESIAN_POINT ( 'NONE',  ( -26.49928411671542960, 9.848831533840668229, 43.38111134601233942 ) ) ;
#28778 = EDGE_CURVE ( 'NONE', #52011, #7422, #56170, .T. ) ;
#28779 = EDGE_CURVE ( 'NONE', #66775, #36668, #32197, .T. ) ;
#28780 = FACE_BOUND ( 'NONE', #49994, .T. ) ;
#28781 = ORIENTED_EDGE ( 'NONE', *, *, #23049, .T. ) ;
#28782 = CARTESIAN_POINT ( 'NONE',  ( 181.0840389613909736, 80.03940679743415387, -89.91415884680696990 ) ) ;
#28783 = CARTESIAN_POINT ( 'NONE',  ( -33.84080342750782933, 9.997552308299118451, -23.09450778006452509 ) ) ;
#28784 = CARTESIAN_POINT ( 'NONE',  ( 155.6786224008560851, 56.27084630678375277, -90.02132744223033001 ) ) ;
#28785 = CARTESIAN_POINT ( 'NONE',  ( -125.8938041572051389, 47.69968343338778283, 3.775397282693376155 ) ) ;
#28786 = CARTESIAN_POINT ( 'NONE',  ( 157.4703587214989113, 57.65129005721575339, 56.25401806271706562 ) ) ;
#28787 = ORIENTED_EDGE ( 'NONE', *, *, #48676, .F. ) ;
#28788 = ORIENTED_EDGE ( 'NONE', *, *, #8680, .T. ) ;
#28789 = AXIS2_PLACEMENT_3D ( 'NONE', #33737, #56572, #13661 ) ;
#28790 = EDGE_LOOP ( 'NONE', ( #22080, #35868, #16201, #61662, #52881, #43580, #50573, #46480, #2665 ) ) ;
#28791 = CARTESIAN_POINT ( 'NONE',  ( -442.6627218934912662, 394.9999999999998295, 113.5502958579881465 ) ) ;
#28792 = VECTOR ( 'NONE', #14029, 1000.000000000000000 ) ;
#28793 = AXIS2_PLACEMENT_3D ( 'NONE', #50392, #45803, #34216 ) ;
#28794 =( LENGTH_UNIT ( ) NAMED_UNIT ( * ) SI_UNIT ( .MILLI., .METRE. ) );
#28795 = CARTESIAN_POINT ( 'NONE',  ( -38.93878980550034186, 10.94326053663842302, -42.32003742428015869 ) ) ;
#28796 = CARTESIAN_POINT ( 'NONE',  ( -95.00979396555173651, 29.23841379431415888, 89.83681514907920018 ) ) ;
#28797 = AXIS2_PLACEMENT_3D ( 'NONE', #46373, #41461, #57637 ) ;
#28798 = CARTESIAN_POINT ( 'NONE',  ( -48.12872802574198516, -43.70867239603780519, 170.0000000000000000 ) ) ;
#28799 = CARTESIAN_POINT ( 'NONE',  ( -133.3149301983942223, 51.57857650535018479, 66.08309739370045577 ) ) ;
#28800 = CARTESIAN_POINT ( 'NONE',  ( -76.78104518372332166, 22.68568622761704034, -23.04560864541017295 ) ) ;
#28801 = AXIS2_PLACEMENT_3D ( 'NONE', #35717, #25166, #46595 ) ;
#28802 = EDGE_LOOP ( 'NONE', ( #60168, #31437, #17320, #48393 ) ) ;
#28803 = CARTESIAN_POINT ( 'NONE',  ( 81.03898448521317732, 17.58847173596442559, 59.03229392868342984 ) ) ;
#28804 = ORIENTED_EDGE ( 'NONE', *, *, #31739, .T. ) ;
#28805 = CARTESIAN_POINT ( 'NONE',  ( 32.67604596315971577, 7.629767358313821468, 34.08620588322428091 ) ) ;
#28806 = DIRECTION ( 'NONE',  ( -0.000000000000000000, -0.000000000000000000, -1.000000000000000000 ) ) ;
#28807 = EDGE_LOOP ( 'NONE', ( #2770, #46170, #65547, #33079, #47276, #20741, #56907, #30009, #67163, #11498, #26537, #35582, #11119, #31924, #45049, #52777, #8900, #16675, #4001, #27162, #5958, #24627, #39378 ) ) ;
#28808 = CARTESIAN_POINT ( 'NONE',  ( 188.0141161196704900, 85.90515114331880397, 39.69055676661305654 ) ) ;
#28809 = CARTESIAN_POINT ( 'NONE',  ( 154.4165763529819628, 225.8585178651493663, 138.9999999999999716 ) ) ;
#28810 = CARTESIAN_POINT ( 'NONE',  ( 412.3372781065085633, 219.4906275429376308, 111.5502958579881749 ) ) ;
#28811 = CARTESIAN_POINT ( 'NONE',  ( -124.9970785861867739, 47.10847819093960709, 57.51488436916137914 ) ) ;
#28812 = CARTESIAN_POINT ( 'NONE',  ( -9.524904342798462764, 8.016391612076533946, -50.22712598441950149 ) ) ;
#28813 = DIRECTION ( 'NONE',  ( -0.000000000000000000, 0.000000000000000000, -1.000000000000000000 ) ) ;
#28814 = CARTESIAN_POINT ( 'NONE',  ( 254.4165763529819344, 225.8585178651493948, 108.9999999999999858 ) ) ;
#28815 = ORIENTED_EDGE ( 'NONE', *, *, #38024, .T. ) ;
#28816 = DIRECTION ( 'NONE',  ( 0.000000000000000000, 0.000000000000000000, -1.000000000000000000 ) ) ;
#28817 = PLANE ( 'NONE',  #3805 ) ;
#28818 = ORIENTED_EDGE ( 'NONE', *, *, #94, .F. ) ;
#28819 = DIRECTION ( 'NONE',  ( 0.9839295885986295565, 0.1785568947986370392, -0.000000000000000000 ) ) ;
#28820 = CARTESIAN_POINT ( 'NONE',  ( -94.87734348028330089, 29.17663635873013561, -95.00000000000133582 ) ) ;
#28821 = DIRECTION ( 'NONE',  ( -0.000000000000000000, 1.000000000000000000, -0.000000000000000000 ) ) ;
#28822 = ORIENTED_EDGE ( 'NONE', *, *, #4611, .T. ) ;
#28823 = CARTESIAN_POINT ( 'NONE',  ( 450.2085304802404266, 190.0000000000000000, -250.0000000000000000 ) ) ;
#28824 = CARTESIAN_POINT ( 'NONE',  ( -11.14880195267006435, 7.129907723790826601, -63.02123272090544503 ) ) ;
#28825 = CARTESIAN_POINT ( 'NONE',  ( -33.36721086971961370, 9.915747831546605440, 44.96849820624647265 ) ) ;
#28826 = CARTESIAN_POINT ( 'NONE',  ( 141.3707934840545022, 46.15056991286791543, -43.55297844023782261 ) ) ;
#28827 = EDGE_CURVE ( 'NONE', #42019, #26008, #1123, .T. ) ;
#28828 = VERTEX_POINT ( 'NONE', #14104 ) ;
#28829 = DIRECTION ( 'NONE',  ( -1.000000000000000000, 0.000000000000000000, 0.000000000000000000 ) ) ;
#28830 = EDGE_LOOP ( 'NONE', ( #39796, #46515, #12708, #17147 ) ) ;
#28831 = CARTESIAN_POINT ( 'NONE',  ( 32.66364305947234925, 8.639871491745255483, -12.94525474216406735 ) ) ;
#28832 = CARTESIAN_POINT ( 'NONE',  ( -38.12206941991763642, -16.97122571883291897, 13.79046340968177731 ) ) ;
#28833 = LINE ( 'NONE', #7728, #20633 ) ;
#28834 = CARTESIAN_POINT ( 'NONE',  ( -4.731197926646205865, 7.716745361328041675, 57.62373423735959221 ) ) ;
#28835 = ADVANCED_FACE ( 'NONE', ( #67249 ), #46449, .T. ) ;
#28836 = PRODUCT_DEFINITION_SHAPE ( 'NONE', 'NONE',  #69574 ) ;
#28837 = CARTESIAN_POINT ( 'NONE',  ( 197.8055825329258823, 98.95774805991030121, -94.51229222371586047 ) ) ;
#28838 = SURFACE_STYLE_FILL_AREA ( #7384 ) ;
#28839 = VECTOR ( 'NONE', #21416, 1000.000000000000000 ) ;
#28840 = DIRECTION ( 'NONE',  ( 1.000000000000000000, 0.000000000000000000, 0.000000000000000000 ) ) ;
#28841 = ADVANCED_FACE ( 'NONE', ( #8840 ), #30290, .T. ) ;
#28842 = ORIENTED_EDGE ( 'NONE', *, *, #41632, .T. ) ;
#28843 = CARTESIAN_POINT ( 'NONE',  ( 162.1014732644455307, 61.34312237409764634, -10.86097702891884076 ) ) ;
#28844 = LINE ( 'NONE', #8072, #51936 ) ;
#28845 = AXIS2_PLACEMENT_3D ( 'NONE', #64015, #42559, #30983 ) ;
#28846 = CARTESIAN_POINT ( 'NONE',  ( -452.6627218934913799, 0.000000000000000000, -146.4497041420118251 ) ) ;
#28847 = CARTESIAN_POINT ( 'NONE',  ( 140.9169160367233360, 45.85398962664667977, -67.78391568571109360 ) ) ;
#28848 = CARTESIAN_POINT ( 'NONE',  ( 196.9999999999999716, 2.999999999999969802, 0.000000000000000000 ) ) ;
#28849 = EDGE_CURVE ( 'NONE', #8603, #27646, #51739, .T. ) ;
#28850 = VECTOR ( 'NONE', #17315, 1000.000000000000000 ) ;
#28851 = ORIENTED_EDGE ( 'NONE', *, *, #62023, .T. ) ;
#28852 = CARTESIAN_POINT ( 'NONE',  ( -118.9668643994983483, 43.27909474462862960, 67.85177516854167834 ) ) ;
#28853 = CARTESIAN_POINT ( 'NONE',  ( 164.8444104055694481, 64.93678790243654930, -18.17606153825600757 ) ) ;
#28854 = CARTESIAN_POINT ( 'NONE',  ( 8.528421445032394743, 6.376778749352037146, 35.56919029742448402 ) ) ;
#28855 = ORIENTED_EDGE ( 'NONE', *, *, #5474, .T. ) ;
#28856 = VECTOR ( 'NONE', #29541, 999.9999999999998863 ) ;
#28857 = CARTESIAN_POINT ( 'NONE',  ( 65.39792658623288446, 14.27332852928127949, 71.27325231829686913 ) ) ;
#28858 = CARTESIAN_POINT ( 'NONE',  ( -49.42000000000000171, -36.09918303830819752, 15.41169613715280562 ) ) ;
#28859 = VERTEX_POINT ( 'NONE', #34542 ) ;
#28860 = CARTESIAN_POINT ( 'NONE',  ( 163.5944442552009548, 63.88381951184481267, -39.28731366255506430 ) ) ;
#28861 = CARTESIAN_POINT ( 'NONE',  ( 88.53517449242357884, 20.08005703101045469, 17.62531166502685309 ) ) ;
#28862 = EDGE_CURVE ( 'NONE', #19609, #13387, #62292, .T. ) ;
#28863 = CARTESIAN_POINT ( 'NONE',  ( 163.7464701930789772, 62.69993100427429056, -47.76119388460286075 ) ) ;
#28864 = VERTEX_POINT ( 'NONE', #19376 ) ;
#28865 = EDGE_CURVE ( 'NONE', #9949, #40156, #61931, .T. ) ;
#28866 = CARTESIAN_POINT ( 'NONE',  ( -95.04371414958063724, 30.36527049547256851, 9.135576169247952905 ) ) ;
#28867 = CARTESIAN_POINT ( 'NONE',  ( -442.6627218934913230, 1.665334536937734811E-13, 108.5502958579881749 ) ) ;
#28868 = CARTESIAN_POINT ( 'NONE',  ( 33.77444274891860942, 8.756048688386680823, 32.44976720788645252 ) ) ;
#28869 = CARTESIAN_POINT ( 'NONE',  ( -180.6021503146988607, 97.45669259943413465, -41.59167162592825662 ) ) ;
#28870 = CARTESIAN_POINT ( 'NONE',  ( -132.6161619568759988, 51.08240647571221871, -18.90511423407786040 ) ) ;
#28871 = CARTESIAN_POINT ( 'NONE',  ( -146.7427626416307476, 61.86902255109500004, -89.01813897100886663 ) ) ;
#28872 = CARTESIAN_POINT ( 'NONE',  ( 126.8237978310704221, 37.33705012421152247, -67.74913777150965188 ) ) ;
#28873 = B_SPLINE_CURVE_WITH_KNOTS ( 'NONE', 3,
 ( #31789, #4709, #51863, #36733, #25150, #62773 ),
 .UNSPECIFIED., .F., .F.,
 ( 4, 2, 4 ),
 ( 0.008690415895085790154, 0.01102883710845593661, 0.01336725832182608306 ),
 .UNSPECIFIED. ) ;
#28874 = ORIENTED_EDGE ( 'NONE', *, *, #54778, .T. ) ;
#28875 = CARTESIAN_POINT ( 'NONE',  ( 134.3135005523731706, 42.87884033955813123, -77.85745800642466463 ) ) ;
#28876 = CARTESIAN_POINT ( 'NONE',  ( -10.69547592951790982, 8.103864096836389308, 57.51816172537316163 ) ) ;
#28877 = VERTEX_POINT ( 'NONE', #56670 ) ;
#28878 = CARTESIAN_POINT ( 'NONE',  ( -156.1477286774994582, 71.38742644140637594, -38.81583713021509396 ) ) ;
#28879 = CARTESIAN_POINT ( 'NONE',  ( -1.740765642171157257, 66.62262586640527218, 34.48241795236666718 ) ) ;
#28880 = CARTESIAN_POINT ( 'NONE',  ( -36.37229078872272936, 11.47648211215765990, 32.04620998045675151 ) ) ;
#28881 = CARTESIAN_POINT ( 'NONE',  ( -27.00000000000000355, 26.99999999999999645, 12.00000000000000000 ) ) ;
#28882 = CARTESIAN_POINT ( 'NONE',  ( -3.255961059272217906, 7.643453059677443484, 43.58302407791597943 ) ) ;
#28883 = CARTESIAN_POINT ( 'NONE',  ( 0.000000000000000000, 0.000000000000000000, -0.002000000000002000178 ) ) ;
#28884 = CARTESIAN_POINT ( 'NONE',  ( 0.000000000000000000, -27.00000000000000355, 12.00000000000000000 ) ) ;
#28885 = CARTESIAN_POINT ( 'NONE',  ( 207.8484262634767674, 110.7633525054914401, -50.64494125179354711 ) ) ;
#28886 = CARTESIAN_POINT ( 'NONE',  ( -15.07235766390729026, 8.482541916553470784, 35.66812363169304945 ) ) ;
#28887 = CARTESIAN_POINT ( 'NONE',  ( 164.9697211531229470, 63.72502658717164792, 9.768110188899187918 ) ) ;
#28888 = LINE ( 'NONE', #50340, #29788 ) ;
#28889 = VERTEX_POINT ( 'NONE', #29938 ) ;
#28890 = VECTOR ( 'NONE', #45409, 1000.000000000000000 ) ;
#28891 = CARTESIAN_POINT ( 'NONE',  ( -96.43817545481742570, 31.02509717589737193, -47.24448217450499499 ) ) ;
#28892 = ORIENTED_EDGE ( 'NONE', *, *, #31125, .F. ) ;
#28893 = CARTESIAN_POINT ( 'NONE',  ( -31.11269837220804035, 15.55634918610408945, 85.00100000000000477 ) ) ;
#28894 = CARTESIAN_POINT ( 'NONE',  ( 45.76553115525425142, 10.34124506813254740, -20.25205682851913025 ) ) ;
#28895 = VECTOR ( 'NONE', #31930, 1000.000000000000000 ) ;
#28896 = CARTESIAN_POINT ( 'NONE',  ( -15.55634918610403439, 5.000000000000028422, 85.00100000000000477 ) ) ;
#28897 = CARTESIAN_POINT ( 'NONE',  ( -4.180838820196593808, 65.23214221112780820, 41.38025477438755928 ) ) ;
#28898 = CARTESIAN_POINT ( 'NONE',  ( 0.000000000000000000, 0.000000000000000000, 0.000000000000000000 ) ) ;
#28899 = AXIS2_PLACEMENT_3D ( 'NONE', #57313, #56616, #40436 ) ;
#28900 = PRODUCT_DEFINITION ( 'UNKNOWN', '', #62490, #11313 ) ;
#28901 = CARTESIAN_POINT ( 'NONE',  ( 0.4969600502617471105, 4.995646404165273502, -7.347286611336972584 ) ) ;
#28903 = VECTOR ( 'NONE', #15480, 1000.000000000000000 ) ;
#28902 = LINE ( 'NONE', #40143, #63392 ) ;
#28904 = CARTESIAN_POINT ( 'NONE',  ( -118.4470345550925998, 42.96051736048244862, -16.61147982237926968 ) ) ;
#28905 = EDGE_LOOP ( 'NONE', ( #181, #21295, #36449, #32047 ) ) ;
#28906 = VERTEX_POINT ( 'NONE', #51404 ) ;
#28907 = EDGE_CURVE ( 'NONE', #55398, #41122, #50696, .T. ) ;
#28908 = CYLINDRICAL_SURFACE ( 'NONE', #54518, 7.500000000000013323 ) ;
#28909 = CARTESIAN_POINT ( 'NONE',  ( -14.19745703647395274, -56.58567453852795381, 27.58472315868180402 ) ) ;
#28910 = DIRECTION ( 'NONE',  ( 0.6427876096865403621, -0.7660444431189770143, 1.393823445737823288E-16 ) ) ;
#28911 = CARTESIAN_POINT ( 'NONE',  ( 107.9213359589208636, 28.92595015506873679, 71.10305713611002432 ) ) ;
#28912 = EDGE_CURVE ( 'NONE', #58260, #16366, #25016, .T. ) ;
#28913 = DIRECTION ( 'NONE',  ( 0.000000000000000000, 0.000000000000000000, 1.000000000000000000 ) ) ;
#28914 = DIRECTION ( 'NONE',  ( 1.000000000000000000, 0.000000000000000000, 0.000000000000000000 ) ) ;
#28915 = ORIENTED_EDGE ( 'NONE', *, *, #19860, .F. ) ;
#28916 = DIRECTION ( 'NONE',  ( -1.000000000000000000, 0.000000000000000000, 0.000000000000000000 ) ) ;
#28917 = DIRECTION ( 'NONE',  ( -0.000000000000000000, 1.000000000000000000, -0.000000000000000000 ) ) ;
#28918 = CARTESIAN_POINT ( 'NONE',  ( -82.53770812813171176, 23.83403279300013722, -22.19906966960727246 ) ) ;
#28919 = CARTESIAN_POINT ( 'NONE',  ( 0.000000000000000000, 0.000000000000000000, 8.000000000000000000 ) ) ;
#28920 = LINE ( 'NONE', #45078, #12938 ) ;
#28921 = FACE_BOUND ( 'NONE', #44189, .T. ) ;
#28922 = ADVANCED_FACE ( 'NONE', ( #57363 ), #67931, .F. ) ;
#28923 = EDGE_CURVE ( 'NONE', #37187, #45254, #12572, .T. ) ;
#28924 = ORIENTED_EDGE ( 'NONE', *, *, #67594, .F. ) ;
#28925 = EDGE_CURVE ( 'NONE', #62951, #20416, #14192, .T. ) ;
#28926 = CARTESIAN_POINT ( 'NONE',  ( -53.31111153860302210, 37.18770477615724701, 170.0000000000000000 ) ) ;
#28927 = LINE ( 'NONE', #45084, #55238 ) ;
#28928 = CARTESIAN_POINT ( 'NONE',  ( 32.15284246740100116, 8.588257691344875155, -68.02502300723051576 ) ) ;
#28929 = CARTESIAN_POINT ( 'NONE',  ( -177.1381400275771796, 93.26609858452820845, 5.128634852069275496 ) ) ;
#28930 = CARTESIAN_POINT ( 'NONE',  ( 152.2940756559019064, 53.73566983921583073, 4.632148972456340275 ) ) ;
#28931 = LINE ( 'NONE', #6420, #69245 ) ;
#28932 = VECTOR ( 'NONE', #14803, 1000.000000000000000 ) ;
#28933 = VERTEX_POINT ( 'NONE', #18694 ) ;
#28934 = CARTESIAN_POINT ( 'NONE',  ( 26.11269837220806167, 4.999999999999936939, 0.000000000000000000 ) ) ;
#28935 = CARTESIAN_POINT ( 'NONE',  ( 197.3119541548905715, 98.33923235143190311, -45.14000074610142832 ) ) ;
#28936 = EDGE_LOOP ( 'NONE', ( #18605, #18545 ) ) ;
#28938 = CARTESIAN_POINT ( 'NONE',  ( 0.000000000000000000, -26.09918303830819397, 30.00000000000000000 ) ) ;
#28937 = AXIS2_PLACEMENT_3D ( 'NONE', #33495, #1124, #13078 ) ;
#28939 = ORIENTED_EDGE ( 'NONE', *, *, #31868, .T. ) ;
#28940 = CARTESIAN_POINT ( 'NONE',  ( 290.0000000000000568, 0.000000000000000000, 0.000000000000000000 ) ) ;
#28941 = LINE ( 'NONE', #29616, #10640 ) ;
#28942 = CARTESIAN_POINT ( 'NONE',  ( 91.12448333640237763, 22.07449368110502164, -76.18914264227882427 ) ) ;
#28943 = ORIENTED_EDGE ( 'NONE', *, *, #5158, .F. ) ;
#28944 = CIRCLE ( 'NONE', #40137, 243.4957430088094839 ) ;
#28945 = VERTEX_POINT ( 'NONE', #9175 ) ;
#28946 = CARTESIAN_POINT ( 'NONE',  ( -447.6627218934913799, 0.000000000000000000, -136.4497041420118251 ) ) ;
#28947 = CARTESIAN_POINT ( 'NONE',  ( 163.7379901688713346, 64.00402364591249693, 41.03665140154781454 ) ) ;
#28948 = VECTOR ( 'NONE', #35257, 1000.000000000000000 ) ;
#28949 = CARTESIAN_POINT ( 'NONE',  ( -156.3734885497382265, 71.59531449004289527, -72.18732252565617102 ) ) ;
#28950 = CARTESIAN_POINT ( 'NONE',  ( 70.51522979775971578, 15.57935281015687146, 10.97061778370436436 ) ) ;
#28951 = DIRECTION ( 'NONE',  ( -0.000000000000000000, -1.000000000000000000, -0.000000000000000000 ) ) ;
#28952 = EDGE_LOOP ( 'NONE', ( #6768, #56569, #18272, #57058, #38742, #40564, #5527, #39195, #23343 ) ) ;
#28953 = VECTOR ( 'NONE', #38714, 1000.000000000000000 ) ;
#28954 = ADVANCED_FACE ( 'NONE', ( #46803 ), #19851, .T. ) ;
#28955 = CARTESIAN_POINT ( 'NONE',  ( 0.000000000000000000, 0.000000000000000000, 0.000000000000000000 ) ) ;
#28956 = AXIS2_PLACEMENT_3D ( 'NONE', #25602, #9757, #63221 ) ;
#28957 = CARTESIAN_POINT ( 'NONE',  ( -53.38065169970960966, 15.27943072477081721, 18.28795179123243742 ) ) ;
#28958 = CARTESIAN_POINT ( 'NONE',  ( -11.85813018568104305, 8.195977661838494299, -90.22625169180082594 ) ) ;
#28959 = CARTESIAN_POINT ( 'NONE',  ( -155.2449610530290158, 70.56131896221211264, -91.16623920745314535 ) ) ;
#28960 = DIRECTION ( 'NONE',  ( 0.000000000000000000, -0.000000000000000000, -1.000000000000000000 ) ) ;
#28961 = CARTESIAN_POINT ( 'NONE',  ( 79.79041068698137451, 17.19981260293680236, 87.80323115344171470 ) ) ;
#28963 = ORIENTED_EDGE ( 'NONE', *, *, #12905, .T. ) ;
#28962 = CARTESIAN_POINT ( 'NONE',  ( 2.700000000000004619, 0.000000000000000000, 0.000000000000000000 ) ) ;
#28964 = ORIENTED_EDGE ( 'NONE', *, *, #9200, .F. ) ;
#28965 = EDGE_LOOP ( 'NONE', ( #38705, #1653, #22607, #30150 ) ) ;
#28966 = CARTESIAN_POINT ( 'NONE',  ( 40.37438610703016906, 8.537526699166109623, 3.116409814543585455 ) ) ;
#28967 = CARTESIAN_POINT ( 'NONE',  ( -179.6930825076241831, 96.33844031696564514, 88.38185184032300867 ) ) ;
#28968 = DIRECTION ( 'NONE',  ( -0.8090169943749506709, 0.5877852522924686962, 0.000000000000000000 ) ) ;
#28969 = CARTESIAN_POINT ( 'NONE',  ( 103.4696172145935122, 25.87254488218943749, -13.34745220050455750 ) ) ;
#28970 = CARTESIAN_POINT ( 'NONE',  ( 200.8298320869469933, 101.1869877914233484, 3.423144167023327356 ) ) ;
#28971 = CARTESIAN_POINT ( 'NONE',  ( 208.2960261509592215, 113.1866506096883143, 83.81060036596683460 ) ) ;
#28972 = DIRECTION ( 'NONE',  ( -0.000000000000000000, -1.000000000000000000, -0.000000000000000000 ) ) ;
#28973 = CARTESIAN_POINT ( 'NONE',  ( -71.97434903038468690, 19.88430675376532974, -72.88272746850553574 ) ) ;
#28974 = CARTESIAN_POINT ( 'NONE',  ( -11.57931195747592312, 7.164335452024272577, 44.12695385317129393 ) ) ;
#28975 = VERTEX_POINT ( 'NONE', #13077 ) ;
#28976 = CARTESIAN_POINT ( 'NONE',  ( 13.83281508467571363, 7.452090093180184560, -8.916925143331820180 ) ) ;
#28977 = ORIENTED_EDGE ( 'NONE', *, *, #30021, .T. ) ;
#28978 = ORIENTED_EDGE ( 'NONE', *, *, #55726, .T. ) ;
#28979 = CARTESIAN_POINT ( 'NONE',  ( -145.9181947914994737, 62.49417193455356312, 17.96563906742083461 ) ) ;
#28980 = B_SPLINE_CURVE_WITH_KNOTS ( 'NONE', 3,
 ( #53478, #31360, #20, #68967, #25746, #5309, #37305, #47175, #41563, #52462, #47866, #4284, #63715, #68635, #26768, #4614, #69328, #20441, #48194, #15527, #26079, #47509, #10919, #36641, #36980, #58416, #21475, #16202, #10232, #31695, #21151, #42596, #64048, #15859, #64390, #37654, #32396, #53820, #27442, #11974, #60508, #43966, #22178, #48881, #7041, #12673 ),
 .UNSPECIFIED., .F., .F.,
 ( 4, 2, 2, 2, 2, 2, 2, 2, 2, 2, 2, 2, 2, 2, 2, 2, 2, 2, 2, 2, 2, 2, 4 ),
 ( 6.938893903907228378E-18, 0.003192770216278345216, 0.003990962770347930219, 0.004789155324417515222, 0.006385540432556695636, 0.007183732986626276303, 0.007981925540695855234, 0.009578310648835018301, 0.01037650320290461024, 0.01117469575697420045, 0.01197288831104379239, 0.01277108086511338433, 0.01436746597325256822, 0.01596385108139174863, 0.01676204363546133017, 0.01756023618953090823, 0.01835842874360048629, 0.01915662129767006783, 0.02075300640580923089, 0.02234939151394839396, 0.02394577662208755703, 0.02474396917615713856, 0.02554216173022672356 ),
 .UNSPECIFIED. ) ;
#28981 = LINE ( 'NONE', #45138, #42843 ) ;
#28982 = CARTESIAN_POINT ( 'NONE',  ( -166.2065256787326746, 81.19093426984592554, 41.24070342831011260 ) ) ;
#28983 = CARTESIAN_POINT ( 'NONE',  ( 117.4806398654733641, 33.50379325299402922, -18.61210399727144704 ) ) ;
#28984 = ADVANCED_FACE ( 'NONE', ( #55983 ), #23966, .T. ) ;
#28986 = CARTESIAN_POINT ( 'NONE',  ( -108.9452487746634404, 36.29752968355631992, 7.697822667569220734 ) ) ;
#28985 = CIRCLE ( 'NONE', #46946, 20.00000000000001066 ) ;
#28987 = CARTESIAN_POINT ( 'NONE',  ( 39.40195752203892710, -170.0000000000000000, 10.56928371549958889 ) ) ;
#28988 = CARTESIAN_POINT ( 'NONE',  ( 141.0517870458593279, 47.14452711594498169, -14.54592510178403586 ) ) ;
#28989 = EDGE_LOOP ( 'NONE', ( #12310, #35249, #21110, #9210, #60931, #43366 ) ) ;
#28990 = ORIENTED_EDGE ( 'NONE', *, *, #67534, .T. ) ;
#28991 = ADVANCED_FACE ( 'NONE', ( #40149 ), #61603, .F. ) ;
#28992 =( BOUNDED_CURVE ( )  B_SPLINE_CURVE ( 3, ( #21137, #59090, #53460, #43950 ),
 .UNSPECIFIED., .F., .F. ) 
 B_SPLINE_CURVE_WITH_KNOTS ( ( 4, 4 ),
 ( 4.791312937756477625E-14, 1.570796326794909437 ),
 .UNSPECIFIED. ) 
 CURVE ( )  GEOMETRIC_REPRESENTATION_ITEM ( )  RATIONAL_B_SPLINE_CURVE ( ( 1.000000000000000000, 0.8047378541243732641, 0.8047378541243732641, 1.000000000000000000 ) ) 
 REPRESENTATION_ITEM ( '' )  );
#28993 = AXIS2_PLACEMENT_3D ( 'NONE', #42309, #41617, #67671 ) ;
#28994 = LINE ( 'NONE', #46534, #33877 ) ;
#28995 = CARTESIAN_POINT ( 'NONE',  ( -2.873135757086586750E-15, 6.534749472788147884, 4.681481898397000130 ) ) ;
#28996 = CARTESIAN_POINT ( 'NONE',  ( -24.07306065005153783, 53.14126621947204399, 27.58472369383525802 ) ) ;
#28997 = EDGE_CURVE ( 'NONE', #27057, #52056, #8138, .T. ) ;
#28998 = CARTESIAN_POINT ( 'NONE',  ( -156.3413281584584809, 70.19975255048969132, 94.99999999999866418 ) ) ;
#28999 = VECTOR ( 'NONE', #28036, 1000.000000000000000 ) ;
#29001 = ADVANCED_FACE ( 'NONE', ( #20760 ), #64352, .T. ) ;
#29000 = UNCERTAINTY_MEASURE_WITH_UNIT (LENGTH_MEASURE( 1.000000000000000082E-05 ), #46628, 'distance_accuracy_value', 'NONE');
#29002 = CARTESIAN_POINT ( 'NONE',  ( 198.2581645178919132, 99.52881771501675701, 67.40755752364371745 ) ) ;
#29003 = ORIENTED_EDGE ( 'NONE', *, *, #7236, .F. ) ;
#29004 = AXIS2_PLACEMENT_3D ( 'NONE', #48371, #58948, #8448 ) ;
#29005 = LINE ( 'NONE', #43500, #49087 ) ;
#29006 = CARTESIAN_POINT ( 'NONE',  ( -58.32502757340554922, 16.62877055630752920, -76.32654648603724468 ) ) ;
#29007 = CARTESIAN_POINT ( 'NONE',  ( 177.0024338932394130, 74.57605685449962607, -64.26120218828934583 ) ) ;
#29008 = CARTESIAN_POINT ( 'NONE',  ( 275.0002060648038196, -21.99995316709852133, 0.3345430166890087653 ) ) ;
#29009 = CARTESIAN_POINT ( 'NONE',  ( 196.9999999999999716, 0.000000000000000000, -3.000000000000030198 ) ) ;
#29010 = CARTESIAN_POINT ( 'NONE',  ( -172.3057147739576749, 86.22480007276992353, 4.010060984321524913 ) ) ;
#29011 = CARTESIAN_POINT ( 'NONE',  ( 437.3372781065085633, 395.0000000000001137, -146.4497041420118535 ) ) ;
#29012 = FACE_BOUND ( 'NONE', #34054, .T. ) ;
#29013 = CARTESIAN_POINT ( 'NONE',  ( -189.6935402730020428, 107.7189398452714926, 94.71296932948054348 ) ) ;
#29014 = VECTOR ( 'NONE', #26462, 1000.000000000000000 ) ;
#29015 = EDGE_CURVE ( 'NONE', #49177, #29619, #56909, .T. ) ;
#29016 = CARTESIAN_POINT ( 'NONE',  ( -2.866724795119716340, 6.618578306599220973, 70.10825721528765087 ) ) ;
#29017 = ORIENTED_EDGE ( 'NONE', *, *, #48965, .F. ) ;
#29018 = EDGE_CURVE ( 'NONE', #66152, #59483, #10841, .T. ) ;
#29019 = CARTESIAN_POINT ( 'NONE',  ( 275.5071502593006585, 21.88997039781574472, 2.218170224452117978 ) ) ;
#29020 = CARTESIAN_POINT ( 'NONE',  ( 149.9683128897949871, 53.28564708287390772, 64.28427443997613011 ) ) ;
#29021 = PLANE ( 'NONE',  #46712 ) ;
#29022 = DIRECTION ( 'NONE',  ( -0.000000000000000000, -0.000000000000000000, -1.000000000000000000 ) ) ;
#29023 = FACE_OUTER_BOUND ( 'NONE', #64242, .T. ) ;
#29024 = ORIENTED_EDGE ( 'NONE', *, *, #49589, .F. ) ;
#29025 = CARTESIAN_POINT ( 'NONE',  ( 50.97490815085634352, 6.000000000000000000, -14.43565316649549679 ) ) ;
#29026 = CARTESIAN_POINT ( 'NONE',  ( 187.2889560709053853, 85.11232376512226949, 94.72469196122591484 ) ) ;
#29027 = ORIENTED_EDGE ( 'NONE', *, *, #42643, .F. ) ;
#29028 = EDGE_LOOP ( 'NONE', ( #36390, #56034 ) ) ;
#29029 = LINE ( 'NONE', #44126, #18460 ) ;
#29030 = CARTESIAN_POINT ( 'NONE',  ( 152.8373718734504507, 55.38925997611396923, 42.82746393499770932 ) ) ;
#29031 = DIRECTION ( 'NONE',  ( -1.048079516971690241E-11, 0.000000000000000000, -1.000000000000000000 ) ) ;
#29032 = ORIENTED_EDGE ( 'NONE', *, *, #37471, .F. ) ;
#29033 = CARTESIAN_POINT ( 'NONE',  ( -452.6627218934914367, 399.9999999999998863, -116.4497041420118393 ) ) ;
#29034 = B_SPLINE_CURVE_WITH_KNOTS ( 'NONE', 3,
 ( #41321, #63809, #26516, #63117, #25153, #41659, #36736, #36040, #46581, #62776, #58180, #31793, #21238, #53227, #68062, #4712, #52554, #14916, #9655, #20535, #5053, #52212, #31118, #15958, #10328, #47956, #31452, #14580, #4377, #69422, #15617, #25840, #36387, #20894, #19865, #68724, #57839, #47272, #57496, #42685, #42350, #9999, #9302, #42004, #64144, #63464, #68398, #15274, #20203, #52886 ),
 .UNSPECIFIED., .F., .F.,
 ( 4, 2, 2, 2, 2, 2, 2, 2, 2, 2, 2, 2, 2, 2, 2, 2, 2, 2, 2, 2, 2, 2, 2, 2, 4 ),
 ( 0.03296461860586802350, 0.03492857779726595696, 0.03689253698866389042, 0.03885649618006182388, 0.04082045537145975733, 0.04278441456285769079, 0.04376639415855662629, 0.04474837375425555486, 0.04573035334995449036, 0.04671233294565341893, 0.04720332274350288321, 0.04769431254135235443, 0.04867629213705128299, 0.04965827173275021156, 0.05064025132844914706, 0.05162223092414808256, 0.05260421051984701113, 0.05358619011554593969, 0.05456816971124487520, 0.05555014930694381070, 0.05653212890264273927, 0.05849608809404058252, 0.06046004728543843271, 0.06242400647683628290, 0.06438796566823412615 ),
 .UNSPECIFIED. ) ;
#29035 = CARTESIAN_POINT ( 'NONE',  ( -18.89790202299119315, -62.20684691518632548, 43.58025477438756923 ) ) ;
#29036 = FACE_OUTER_BOUND ( 'NONE', #46458, .T. ) ;
#29037 = CARTESIAN_POINT ( 'NONE',  ( 209.3223706822284100, 18.00000000000002842, 276.7520087653757628 ) ) ;
#29038 = CARTESIAN_POINT ( 'NONE',  ( -26.49928411671542960, 9.848831533840670005, -10.30798983491501808 ) ) ;
#29039 = CARTESIAN_POINT ( 'NONE',  ( -54.08816720029309977, 15.46531105893041769, -8.418552427708386077 ) ) ;
#29040 = ORIENTED_EDGE ( 'NONE', *, *, #44447, .F. ) ;
#29041 = VECTOR ( 'NONE', #21719, 1000.000000000000114 ) ;
#29042 = CARTESIAN_POINT ( 'NONE',  ( 117.4696399285658543, 32.37118663718647582, -45.49517373264203002 ) ) ;
#29043 = CARTESIAN_POINT ( 'NONE',  ( 307.2575771313985342, 172.0000000000000284, 256.6193948016162381 ) ) ;
#29044 = CARTESIAN_POINT ( 'NONE',  ( 45.36109889487609337, 9.259412558041161034, -38.53950509509405720 ) ) ;
#29045 = AXIS2_PLACEMENT_3D ( 'NONE', #45000, #34476, #44670 ) ;
#29046 = LINE ( 'NONE', #18134, #18558 ) ;
#29048 = ORIENTED_EDGE ( 'NONE', *, *, #45762, .T. ) ;
#29047 = LINE ( 'NONE', #17791, #33221 ) ;
#29049 = CARTESIAN_POINT ( 'NONE',  ( -34.75846525698938194, -54.92585086258257121, 40.00000000000003553 ) ) ;
#29050 = AXIS2_PLACEMENT_3D ( 'NONE', #38287, #37244, #37942 ) ;
#29051 = EDGE_LOOP ( 'NONE', ( #2604, #31053, #1247, #24935 ) ) ;
#29052 = CARTESIAN_POINT ( 'NONE',  ( -142.3178993725749137, 58.31327888234797996, 67.27388540028242403 ) ) ;
#29053 = CARTESIAN_POINT ( 'NONE',  ( 81.05403189674299824, 18.64820877954959499, 32.17181610260639246 ) ) ;
#29054 = CARTESIAN_POINT ( 'NONE',  ( -18.89790202299119315, -62.20684691518632548, 0.000000000000000000 ) ) ;
#29055 = DIRECTION ( 'NONE',  ( -0.000000000000000000, -0.000000000000000000, -1.000000000000000000 ) ) ;
#29056 = FACE_OUTER_BOUND ( 'NONE', #55556, .T. ) ;
#29057 = CARTESIAN_POINT ( 'NONE',  ( 43.96421756700842565, 10.06386361114660311, 4.596548279175047824 ) ) ;
#29058 = CARTESIAN_POINT ( 'NONE',  ( -179.5109681715917986, 96.11572638569518290, -19.33240666069409031 ) ) ;
#29059 = FACE_OUTER_BOUND ( 'NONE', #52208, .T. ) ;
#29060 = VERTEX_POINT ( 'NONE', #48160 ) ;
#29061 = ORIENTED_EDGE ( 'NONE', *, *, #18344, .F. ) ;
#29062 = CARTESIAN_POINT ( 'NONE',  ( 109.7774723066848850, 28.66666416591279898, 56.45576479620101651 ) ) ;
#29063 = CARTESIAN_POINT ( 'NONE',  ( 159.6593397521789370, 59.37286298965125297, 56.56669563789166233 ) ) ;
#29064 = CARTESIAN_POINT ( 'NONE',  ( -190.6985136298601731, 109.1272424661242582, 60.81597207375692449 ) ) ;
#29065 = CARTESIAN_POINT ( 'NONE',  ( 30.28348399776037070, 22.91216519805201202, -19.22558936715840261 ) ) ;
#29066 = FACE_OUTER_BOUND ( 'NONE', #34808, .T. ) ;
#29067 = CARTESIAN_POINT ( 'NONE',  ( -108.6634958860518338, 36.14357436892402831, 68.80899113430457703 ) ) ;
#29068 = CARTESIAN_POINT ( 'NONE',  ( -26.88245755577923646, 8.887394979218518287, -48.79474396477220210 ) ) ;
#29069 = CARTESIAN_POINT ( 'NONE',  ( 433.3728120124416137, 388.0000000000066507, -132.4852380479447902 ) ) ;
#29070 = VERTEX_POINT ( 'NONE', #26046 ) ;
#29071 = ORIENTED_EDGE ( 'NONE', *, *, #37207, .F. ) ;
#29072 = ADVANCED_FACE ( 'NONE', ( #53441 ), #52754, .F. ) ;
#29073 = ORIENTED_EDGE ( 'NONE', *, *, #3314, .T. ) ;
#29074 = DIRECTION ( 'NONE',  ( -0.000000000000000000, -0.9989683093773507050, -0.04541273895899305274 ) ) ;
#29075 = CARTESIAN_POINT ( 'NONE',  ( -76.27009788956611658, 21.42253842560091570, 84.47334644398770820 ) ) ;
#29076 = CARTESIAN_POINT ( 'NONE',  ( 15.78827728214693416, -170.0000000000000000, 45.01470767270524931 ) ) ;
#29077 = CARTESIAN_POINT ( 'NONE',  ( 132.0563630623056781, 41.51825634609595994, 29.72595898648637203 ) ) ;
#29078 = CARTESIAN_POINT ( 'NONE',  ( -422.6627218934912662, 394.9999999999998295, 113.5502958579882034 ) ) ;
#29079 = LINE ( 'NONE', #61758, #22185 ) ;
#29080 = ADVANCED_FACE ( 'NONE', ( #36253 ), #2989, .T. ) ;
#29081 = PLANE ( 'NONE',  #65213 ) ;
#29082 = CARTESIAN_POINT ( 'NONE',  ( 56.29445224195348629, 12.24017809212661945, 33.94850966223434341 ) ) ;
#29083 = CARTESIAN_POINT ( 'NONE',  ( 32.71243998906020778, 7.633449976421425198, 87.69550224701529828 ) ) ;
#29084 = VERTEX_POINT ( 'NONE', #37268 ) ;
#29085 = CARTESIAN_POINT ( 'NONE',  ( -3.252497086158845363, 6.636017118947991733, -48.88317998446056833 ) ) ;
#29086 = PLANE ( 'NONE',  #39675 ) ;
#29087 = CARTESIAN_POINT ( 'NONE',  ( -189.2739965869454295, 107.1373753350176230, -42.99051981391919242 ) ) ;
#29088 = CARTESIAN_POINT ( 'NONE',  ( -142.9730935922300148, 58.82921737386683247, 15.06684688205722544 ) ) ;
#29089 = LINE ( 'NONE', #44564, #15280 ) ;
#29090 = CARTESIAN_POINT ( 'NONE',  ( -104.1342612728951167, 33.73231160250194449, -76.64130442548571409 ) ) ;
#29091 = CARTESIAN_POINT ( 'NONE',  ( 130.7260570116704059, 40.73146260246710426, -9.847617054034046191 ) ) ;
#29092 = EDGE_CURVE ( 'NONE', #46344, #32718, #57709, .T. ) ;
#29093 = CIRCLE ( 'NONE', #9954, 65.00000000000000000 ) ;
#29094 = ORIENTED_EDGE ( 'NONE', *, *, #42402, .F. ) ;
#29095 =( NAMED_UNIT ( * ) PLANE_ANGLE_UNIT ( ) SI_UNIT ( $, .RADIAN. ) );
#29096 = CARTESIAN_POINT ( 'NONE',  ( 28.03312966668345041, -18.20513007408997197, 6.893343212288941757 ) ) ;
#29097 = CARTESIAN_POINT ( 'NONE',  ( -36.89224332184166855, 11.57404295377975778, -47.97205884790524522 ) ) ;
#29098 = DIRECTION ( 'NONE',  ( -0.000000000000000000, -1.000000000000000000, -0.000000000000000000 ) ) ;
#29099 = CARTESIAN_POINT ( 'NONE',  ( -165.7184136928310920, 79.24930266387268318, 93.27236818605236124 ) ) ;
#29100 = EDGE_LOOP ( 'NONE', ( #36549, #35891 ) ) ;
#29101 = CARTESIAN_POINT ( 'NONE',  ( -118.3927673406137302, 41.74929850983304647, -42.17578386237221366 ) ) ;
#29102 = CARTESIAN_POINT ( 'NONE',  ( -417.6627218934913799, 399.9999999999998295, -111.4497041420118251 ) ) ;
#29103 = DIRECTION ( 'NONE',  ( -1.000000000000000000, -0.000000000000000000, -0.000000000000000000 ) ) ;
#29104 = CARTESIAN_POINT ( 'NONE',  ( 154.3232427916091751, 56.50492108618855980, 83.78354423499102666 ) ) ;
#29105 = ORIENTED_EDGE ( 'NONE', *, *, #62771, .F. ) ;
#29106 = DIRECTION ( 'NONE',  ( -0.000000000000000000, 1.000000000000000000, -0.000000000000000000 ) ) ;
#29107 = CARTESIAN_POINT ( 'NONE',  ( -2.700000000000004619, 0.000000000000000000, 0.000000000000000000 ) ) ;
#29108 = CARTESIAN_POINT ( 'NONE',  ( 141.9165763529819344, -52.00000000000000711, 129.0000000000000000 ) ) ;
#29109 = CARTESIAN_POINT ( 'NONE',  ( 19.74724861314307134, 6.659670522263898107, -49.39369726644508063 ) ) ;
#29111 = ORIENTED_EDGE ( 'NONE', *, *, #35186, .F. ) ;
#29110 = DIRECTION ( 'NONE',  ( 0.000000000000000000, -1.000000000000000000, 0.000000000000000000 ) ) ;
#29112 = CARTESIAN_POINT ( 'NONE',  ( 59.72897338775216980, 11.93428797217974591, 30.56701851669645009 ) ) ;
#29113 = ORIENTED_EDGE ( 'NONE', *, *, #60991, .T. ) ;
#29114 = EDGE_LOOP ( 'NONE', ( #24605, #20671, #33954, #64458 ) ) ;
#29115 = CARTESIAN_POINT ( 'NONE',  ( 174.9099402067542428, 73.96774984027642574, 41.07482263567545999 ) ) ;
#29116 = CARTESIAN_POINT ( 'NONE',  ( 15.78827728214693416, 6.500811158483284835, -77.36349468914950478 ) ) ;
#29118 = EDGE_LOOP ( 'NONE', ( #64620, #31725 ) ) ;
#29117 = DIRECTION ( 'NONE',  ( -0.000000000000000000, 1.000000000000000000, -0.000000000000000000 ) ) ;
#29119 = DIRECTION ( 'NONE',  ( -1.000000000000000000, 0.000000000000000000, 0.000000000000000000 ) ) ;
#29120 = CARTESIAN_POINT ( 'NONE',  ( -25.49247221749738301, 9.706368398275719400, 42.31336193027286185 ) ) ;
#29121 = CARTESIAN_POINT ( 'NONE',  ( -71.27103490383372275, 20.70545763375144688, -41.34176840752093796 ) ) ;
#29122 = ORIENTED_EDGE ( 'NONE', *, *, #42561, .F. ) ;
#29123 = EDGE_CURVE ( 'NONE', #14016, #61067, #37721, .T. ) ;
#29124 = CARTESIAN_POINT ( 'NONE',  ( 212.1669304543882220, 119.0398299474538959, -71.37118650051857571 ) ) ;
#29125 = EDGE_CURVE ( 'NONE', #34523, #17392, #38314, .T. ) ;
#29126 = DIRECTION ( 'NONE',  ( -0.8160245890732938934, -0.5780171883497599028, 0.000000000000000000 ) ) ;
#29127 = CARTESIAN_POINT ( 'NONE',  ( 115.0485321076020284, 32.28990710985444679, 42.89032573288258732 ) ) ;
#29128 = CARTESIAN_POINT ( 'NONE',  ( -128.3448054685827913, 49.34430406923178225, 4.183529080979890402 ) ) ;
#29129 = CARTESIAN_POINT ( 'NONE',  ( -53.60725281709859757, -37.40286400928327026, 6.377659838150123602E-18 ) ) ;
#29130 = ORIENTED_EDGE ( 'NONE', *, *, #42961, .T. ) ;
#29131 = AXIS2_PLACEMENT_3D ( 'NONE', #35336, #39572, #50472 ) ;
#29132 = EDGE_LOOP ( 'NONE', ( #60808, #35010, #19871, #49410 ) ) ;
#29133 = EDGE_LOOP ( 'NONE', ( #11988, #4288 ) ) ;
#29134 = LINE ( 'NONE', #28791, #13778 ) ;
#29135 = VECTOR ( 'NONE', #64554, 1000.000000000000000 ) ;
#29136 = CARTESIAN_POINT ( 'NONE',  ( -38.84150381976580491, 10.92416363971239157, -44.04817657352107574 ) ) ;
#29137 = LINE ( 'NONE', #50588, #10156 ) ;
#29138 = FACE_OUTER_BOUND ( 'NONE', #64749, .T. ) ;
#29139 = ADVANCED_FACE ( 'NONE', ( #22841 ), #44282, .T. ) ;
#29140 = CARTESIAN_POINT ( 'NONE',  ( 30.58844092318264529, -28.38418505339829778, 13.79046340968177908 ) ) ;
#29141 = CARTESIAN_POINT ( 'NONE',  ( 259.2042601260359334, 188.0000000000000000, -23.09547038499562888 ) ) ;
#29142 = ORIENTED_EDGE ( 'NONE', *, *, #65773, .T. ) ;
#29143 = CARTESIAN_POINT ( 'NONE',  ( 433.3728120124415568, 395.0000000000042633, 99.58582976391699049 ) ) ;
#29144 = EDGE_CURVE ( 'NONE', #55150, #3858, #6331, .T. ) ;
#29145 = ORIENTED_EDGE ( 'NONE', *, *, #7319, .F. ) ;
#29146 = CARTESIAN_POINT ( 'NONE',  ( 33.75639351246965703, 7.742023566824295600, 32.45167201372024124 ) ) ;
#29147 = SURFACE_SIDE_STYLE ('',( #40047 ) ) ;
#29148 = DIRECTION ( 'NONE',  ( 4.492911005741668837E-18, -2.417738509769519932E-18, -1.000000000000000000 ) ) ;
#29149 = DIRECTION ( 'NONE',  ( 0.2225209339563184452, -0.9749279121818226201, -5.146830507070804164E-17 ) ) ;
#29150 = CARTESIAN_POINT ( 'NONE',  ( 410.0000000000000000, 190.0000000000000000, 2.000000000000000000 ) ) ;
#29151 = CARTESIAN_POINT ( 'NONE',  ( -121.5680658099884255, 44.89994870382102476, 58.81937421782851771 ) ) ;
#29152 = CARTESIAN_POINT ( 'NONE',  ( -48.33725449172840172, 12.98311179783360103, 7.596865058600053899 ) ) ;
#29153 = EDGE_CURVE ( 'NONE', #45146, #58415, #17563, .T. ) ;
#29154 = AXIS2_PLACEMENT_3D ( 'NONE', #32742, #59461, #42932 ) ;
#29155 = DIRECTION ( 'NONE',  ( 0.000000000000000000, 1.000000000000000000, 0.000000000000000000 ) ) ;
#29156 = ORIENTED_EDGE ( 'NONE', *, *, #41530, .F. ) ;
#29157 = CARTESIAN_POINT ( 'NONE',  ( -106.2973690786608501, 34.86887399500433560, -89.86655251325186100 ) ) ;
#29158 = CARTESIAN_POINT ( 'NONE',  ( -156.6819053601226130, 70.51177710383655040, -13.20956540371496324 ) ) ;
#29159 = ORIENTED_EDGE ( 'NONE', *, *, #35498, .F. ) ;
#29160 = CARTESIAN_POINT ( 'NONE',  ( -31.11269837220804035, 20.55634918610408945, 85.00100000000000477 ) ) ;
#29161 = CARTESIAN_POINT ( 'NONE',  ( -56.96436614829621448, 16.24647150911282623, 57.40554593459077637 ) ) ;
#29162 = DIRECTION ( 'NONE',  ( 0.000000000000000000, 0.000000000000000000, 1.000000000000000000 ) ) ;
#29163 = ORIENTED_EDGE ( 'NONE', *, *, #45999, .T. ) ;
#29164 = B_SPLINE_CURVE_WITH_KNOTS ( 'NONE', 3,
 ( #16592, #59836, #12018, #16932, #769, #6391, #37696, #16245, #38048, #59148, #22221, #33131, #7086, #27844, #48574, #33489, #54564, #17282, #43659, #32434, #53862, #49634 ),
 .UNSPECIFIED., .F., .F.,
 ( 4, 2, 2, 2, 2, 2, 2, 2, 2, 2, 4 ),
 ( 0.01086728410803540143, 0.01221890224361778243, 0.01357052037920016344, 0.01492213851478254444, 0.01559794758257374188, 0.01627375665036493932, 0.01762537478594729951, 0.01830118385373846399, 0.01897699292152962847, 0.02032861105711193661, 0.02168022919269424129 ),
 .UNSPECIFIED. ) ;
#29165 = DIRECTION ( 'NONE',  ( -0.000000000000000000, -0.000000000000000000, -1.000000000000000000 ) ) ;
#29166 = CARTESIAN_POINT ( 'NONE',  ( 150.9013375937531123, 53.96275732797609237, -66.84018692432205455 ) ) ;
#29167 = CARTESIAN_POINT ( 'NONE',  ( -32.41627406084104734, 9.753381371531508748, 45.16836582512236475 ) ) ;
#29168 = CARTESIAN_POINT ( 'NONE',  ( 133.8566784816069060, 41.42467568809810530, -51.02331093239568816 ) ) ;
#29169 = EDGE_CURVE ( 'NONE', #44045, #4538, #9204, .T. ) ;
#29170 = ORIENTED_EDGE ( 'NONE', *, *, #44240, .F. ) ;
#29171 = CIRCLE ( 'NONE', #43750, 65.00000000000000000 ) ;
#29172 = EDGE_CURVE ( 'NONE', #9895, #55030, #45658, .T. ) ;
#29173 = EDGE_CURVE ( 'NONE', #33414, #31540, #47897, .T. ) ;
#29174 = EDGE_CURVE ( 'NONE', #25573, #16185, #25168, .T. ) ;
#29175 = CARTESIAN_POINT ( 'NONE',  ( -125.8938041572051389, 46.49392987655492249, 30.61994787315706290 ) ) ;
#29176 = ORIENTED_EDGE ( 'NONE', *, *, #23911, .F. ) ;
#29177 = CARTESIAN_POINT ( 'NONE',  ( 36.08914434112043779, 9.014684630517859176, -9.542106359090377410 ) ) ;
#29178 = FACE_OUTER_BOUND ( 'NONE', #19176, .T. ) ;
#29179 = SURFACE_STYLE_USAGE ( .BOTH. , #28120 ) ;
#29180 = CARTESIAN_POINT ( 'NONE',  ( 127.2459819677542754, 38.72844404003734553, 87.15258772988752867 ) ) ;
#29181 = DIRECTION ( 'NONE',  ( -1.000000000000000000, 0.000000000000000000, 0.000000000000000000 ) ) ;
#29182 = B_SPLINE_CURVE_WITH_KNOTS ( 'NONE', 3,
 ( #54057, #43168, #50201, #64994, #17126, #65337 ),
 .UNSPECIFIED., .F., .F.,
 ( 4, 2, 4 ),
 ( 1.095770181113686320E-06, 0.03239442681617711595, 0.06478775786217312593 ),
 .UNSPECIFIED. ) ;
#29183 = PRESENTATION_STYLE_ASSIGNMENT (( #38688 ) ) ;
#29184 = DIRECTION ( 'NONE',  ( -0.9009688679024218105, 0.4338837391175525693, 0.000000000000000000 ) ) ;
#29185 = AXIS2_PLACEMENT_3D ( 'NONE', #15955, #69420, #58857 ) ;
#29186 = ORIENTED_EDGE ( 'NONE', *, *, #23199, .T. ) ;
#29187 = DIRECTION ( 'NONE',  ( 0.000000000000000000, 0.000000000000000000, 1.000000000000000000 ) ) ;
#29188 = CARTESIAN_POINT ( 'NONE',  ( 266.9165763529819628, 192.0000000000000000, 128.9999999999999716 ) ) ;
#29189 = CARTESIAN_POINT ( 'NONE',  ( 69.50572373348801136, 14.27208627753791603, 67.94843943493852123 ) ) ;
#29190 = CARTESIAN_POINT ( 'NONE',  ( 133.8566784816069628, 41.42467568809806977, -62.86786152285933582 ) ) ;
#29191 = CARTESIAN_POINT ( 'NONE',  ( 4.606779575614314837, -24.69646479044436305, 3.061616997868437868E-16 ) ) ;
#29192 = VECTOR ( 'NONE', #17138, 999.9999999999998863 ) ;
#29193 = ORIENTED_EDGE ( 'NONE', *, *, #22283, .F. ) ;
#29194 = CARTESIAN_POINT ( 'NONE',  ( 163.5944155533006210, 63.88379440759436534, -21.11661691084674075 ) ) ;
#29195 = CARTESIAN_POINT ( 'NONE',  ( 8.848532525911927848, 6.377649276597440853, 40.39023764036181063 ) ) ;
#29196 = EDGE_LOOP ( 'NONE', ( #60422, #32561 ) ) ;
#29197 = CARTESIAN_POINT ( 'NONE',  ( 69.48877314113910586, 15.30784187978995092, 67.95358286125032521 ) ) ;
#29198 = CARTESIAN_POINT ( 'NONE',  ( -17.90772993695011905, -72.84144224619156205, 43.58025477438756212 ) ) ;
#29199 = ORIENTED_EDGE ( 'NONE', *, *, #61382, .F. ) ;
#29200 = CARTESIAN_POINT ( 'NONE',  ( -145.3109762780891003, 60.69959559383372749, -62.92412485375768938 ) ) ;
#29202 = DIRECTION ( 'NONE',  ( 0.7071067811865474617, 4.906538933386759377E-15, 0.7071067811865474617 ) ) ;
#29201 = AXIS2_PLACEMENT_3D ( 'NONE', #10864, #31306, #4901 ) ;
#29203 = CARTESIAN_POINT ( 'NONE',  ( 417.3372781065086201, 0.000000000000000000, -141.4497041420118251 ) ) ;
#29204 = CARTESIAN_POINT ( 'NONE',  ( 164.4615316623335275, 63.29763980349835606, -46.35316271778197006 ) ) ;
#29205 = ORIENTED_EDGE ( 'NONE', *, *, #41286, .T. ) ;
#29206 = DIRECTION ( 'NONE',  ( -0.000000000000000000, 1.000000000000000000, 1.224646799147353207E-16 ) ) ;
#29207 = LINE ( 'NONE', #13716, #49192 ) ;
#29208 = EDGE_CURVE ( 'NONE', #3067, #41030, #66294, .T. ) ;
#29209 = CARTESIAN_POINT ( 'NONE',  ( 33.44035656425388225, 8.720466003183672044, 41.99093887284341520 ) ) ;
#29210 = CARTESIAN_POINT ( 'NONE',  ( 79.37778929114109872, 18.12554302172299714, -14.49807325564501603 ) ) ;
#29211 = CARTESIAN_POINT ( 'NONE',  ( -133.3765738414514601, 51.62252165471731047, -14.99249644436331685 ) ) ;
#29212 = LINE ( 'NONE', #39413, #30056 ) ;
#29213 = CARTESIAN_POINT ( 'NONE',  ( 132.0440382699655117, 40.34028297386452522, -77.65984809815648759 ) ) ;
#29214 = ORIENTED_EDGE ( 'NONE', *, *, #41374, .T. ) ;
#29215 = CARTESIAN_POINT ( 'NONE',  ( 427.4999999999999432, -17.50000000000000000, 1.999999999999998224 ) ) ;
#29216 = CARTESIAN_POINT ( 'NONE',  ( -13.29455179262032871, 8.319166883236675858, 59.32222173321054726 ) ) ;
#29217 = ORIENTED_EDGE ( 'NONE', *, *, #15426, .T. ) ;
#29218 = AXIS2_PLACEMENT_3D ( 'NONE', #12804, #27924, #23002 ) ;
#29219 = CARTESIAN_POINT ( 'NONE',  ( -151.6648563624119390, 67.36546864992760675, -49.50942221783397201 ) ) ;
#29220 = CARTESIAN_POINT ( 'NONE',  ( -1.368053059006204331, 58.32353538761584133, 27.58472315868180402 ) ) ;
#29221 = CARTESIAN_POINT ( 'NONE',  ( -38.92718193365330848, 11.96647478777219753, 38.20581357431434810 ) ) ;
#29222 = CARTESIAN_POINT ( 'NONE',  ( -0.7211439451572428938, 7.539282923622931065, 40.03214358363065628 ) ) ;
#29223 = CARTESIAN_POINT ( 'NONE',  ( 23.37466857204352522, 46.07527450587193130, 26.66469066592269499 ) ) ;
#29224 = DIRECTION ( 'NONE',  ( 0.000000000000000000, 0.000000000000000000, -1.000000000000000000 ) ) ;
#29225 = EDGE_CURVE ( 'NONE', #10970, #19049, #15062, .T. ) ;
#29226 = CARTESIAN_POINT ( 'NONE',  ( -1.862553927312057267, 7.582910205528083480, -20.64884027158456803 ) ) ;
#29227 = EDGE_CURVE ( 'NONE', #16, #58236, #50318, .T. ) ;
#29228 = CARTESIAN_POINT ( 'NONE',  ( -14.33576511807125620, 8.413127487936188587, 41.37126689364819043 ) ) ;
#29230 = EDGE_CURVE ( 'NONE', #52338, #10473, #63936, .T. ) ;
#29229 = CARTESIAN_POINT ( 'NONE',  ( -60.65612136648953623, 16.25551606627059087, 15.98195799223179492 ) ) ;
#29231 = VERTEX_POINT ( 'NONE', #57632 ) ;
#29232 = CARTESIAN_POINT ( 'NONE',  ( -31.08850265415324188, 49.36609516667732578, 27.58472315868180402 ) ) ;
#29233 = ORIENTED_EDGE ( 'NONE', *, *, #22243, .T. ) ;
#29234 = CARTESIAN_POINT ( 'NONE',  ( 103.5588133492865239, 25.91050225236393345, -73.70627781999075978 ) ) ;
#29235 = ADVANCED_FACE ( 'NONE', ( #42134, #68527, #52348, #52680, #4166, #4843 ), #37542, .T. ) ;
#29236 = LINE ( 'NONE', #8124, #64633 ) ;
#29237 = CARTESIAN_POINT ( 'NONE',  ( 46.65037935242576594, 9.463293687292228640, 66.20036211219351685 ) ) ;
#29238 = CARTESIAN_POINT ( 'NONE',  ( 8.000000000000007105, 249.8719672152120381, 94.99999999999866418 ) ) ;
#29239 = CYLINDRICAL_SURFACE ( 'NONE', #59179, 7.500000000000027534 ) ;
#29240 = VECTOR ( 'NONE', #67364, 999.9999999999998863 ) ;
#29241 = CARTESIAN_POINT ( 'NONE',  ( -42.32797523529131922, 61.85511477251419166, 41.38025477438755928 ) ) ;
#29242 = CARTESIAN_POINT ( 'NONE',  ( 39.40195752203892710, 8.409560354027384221, 44.91383430596327742 ) ) ;
#29243 = CARTESIAN_POINT ( 'NONE',  ( 60.00000000000000000, 0.000000000000000000, 10.00000000000000000 ) ) ;
#29244 = EDGE_LOOP ( 'NONE', ( #61381, #40740, #50249, #29170 ) ) ;
#29245 = ORIENTED_EDGE ( 'NONE', *, *, #68894, .F. ) ;
#29246 = CARTESIAN_POINT ( 'NONE',  ( -74.91942932610496086, 19.16407787157945108, 38.91942932610496086 ) ) ;
#29247 = DIRECTION ( 'NONE',  ( -0.000000000000000000, -0.000000000000000000, 1.000000000000000000 ) ) ;
#29248 = DIRECTION ( 'NONE',  ( 0.000000000000000000, 1.000000000000000000, -0.000000000000000000 ) ) ;
#29249 = CARTESIAN_POINT ( 'NONE',  ( 109.7782172510783170, 29.77507867835874933, 56.45576479620099519 ) ) ;
#29250 = CARTESIAN_POINT ( 'NONE',  ( 442.3372781065089612, 370.0000000000064801, -141.4497041420121661 ) ) ;
#29251 = AXIS2_PLACEMENT_3D ( 'NONE', #14946, #26884, #31476 ) ;
#29252 = CARTESIAN_POINT ( 'NONE',  ( 60.61895554631703220, 13.15982272268128206, -9.252893174955183042 ) ) ;
#29253 = ORIENTED_EDGE ( 'NONE', *, *, #25685, .T. ) ;
#29254 = EDGE_CURVE ( 'NONE', #62436, #23495, #64779, .T. ) ;
#29255 = EDGE_CURVE ( 'NONE', #39331, #33627, #15407, .T. ) ;
#29256 = CARTESIAN_POINT ( 'NONE',  ( 103.5849290181278803, 27.01613348792541913, -46.88419179696489891 ) ) ;
#29257 = DIRECTION ( 'NONE',  ( -1.000000000000000000, 0.000000000000000000, 0.000000000000000000 ) ) ;
#29258 = CARTESIAN_POINT ( 'NONE',  ( -81.01337222286375095, 23.22902179892321683, -22.91030771783860587 ) ) ;
#29259 = CARTESIAN_POINT ( 'NONE',  ( -2.000000000000000000, 192.0000000000000000, 380.0000000000000000 ) ) ;
#29260 = CARTESIAN_POINT ( 'NONE',  ( 212.1931396682533375, 117.2245435827729239, -16.66766266149112496 ) ) ;
#29261 = FACE_BOUND ( 'NONE', #21411, .T. ) ;
#29262 = EDGE_CURVE ( 'NONE', #23762, #67138, #26313, .T. ) ;
#29263 = ORIENTED_EDGE ( 'NONE', *, *, #25723, .T. ) ;
#29264 = DIRECTION ( 'NONE',  ( 1.000000000000000000, 0.000000000000000000, 0.000000000000000000 ) ) ;
#29265 = CARTESIAN_POINT ( 'NONE',  ( 89.65730223173021329, 21.54473673261222899, -50.18735940745502688 ) ) ;
#29266 = CARTESIAN_POINT ( 'NONE',  ( 31.95163392065795449, 8.568192436298444292, -70.95598465355915607 ) ) ;
#29267 = DIRECTION ( 'NONE',  ( -1.000000000000000000, 0.000000000000000000, 0.000000000000000000 ) ) ;
#29268 = CARTESIAN_POINT ( 'NONE',  ( 212.1978255065450867, 119.0880569674902603, 63.90116129329218353 ) ) ;
#29269 = VECTOR ( 'NONE', #59576, 1000.000000000000000 ) ;
#29270 = DIRECTION ( 'NONE',  ( -0.000000000000000000, 1.000000000000000000, -0.000000000000000000 ) ) ;
#29271 = ORIENTED_EDGE ( 'NONE', *, *, #45883, .F. ) ;
#29272 = FACE_OUTER_BOUND ( 'NONE', #7088, .T. ) ;
#29273 = CARTESIAN_POINT ( 'NONE',  ( 199.2049631873262001, 100.7347227143599753, -38.71285982394856262 ) ) ;
#29274 = VERTEX_POINT ( 'NONE', #21031 ) ;
#29275 = DIRECTION ( 'NONE',  ( 1.000000000000000000, 0.000000000000000000, 0.000000000000000000 ) ) ;
#29276 = ORIENTED_EDGE ( 'NONE', *, *, #48469, .T. ) ;
#29277 = DIRECTION ( 'NONE',  ( -0.000000000000000000, -0.000000000000000000, -1.000000000000000000 ) ) ;
#29278 = CARTESIAN_POINT ( 'NONE',  ( -58.32502757340554211, 16.62877055630752210, -22.63744530510987119 ) ) ;
#29279 = LINE ( 'NONE', #35247, #49292 ) ;
#29280 = VERTEX_POINT ( 'NONE', #37196 ) ;
#29281 = ORIENTED_EDGE ( 'NONE', *, *, #49778, .F. ) ;
#29282 = CARTESIAN_POINT ( 'NONE',  ( 41.34269507549200995, 9.685203600174697058, 56.99739923425319432 ) ) ;
#29283 = CARTESIAN_POINT ( 'NONE',  ( -104.3632071119006923, 34.98619430863521984, -88.98640296607699440 ) ) ;
#29284 = CARTESIAN_POINT ( 'NONE',  ( 103.0124792097646491, 26.77148435100179569, 8.208214002704151468 ) ) ;
#29285 = ORIENTED_EDGE ( 'NONE', *, *, #35255, .F. ) ;
#29286 = CARTESIAN_POINT ( 'NONE',  ( 209.9999999999999716, -57.00000000000007816, 72.99999999999998579 ) ) ;
#29287 = EDGE_CURVE ( 'NONE', #29750, #8207, #58058, .T. ) ;
#29288 = CARTESIAN_POINT ( 'NONE',  ( -53.14657859411974528, 15.21831473227210552, 18.23054375554142581 ) ) ;
#29289 = CARTESIAN_POINT ( 'NONE',  ( -127.6881387055492354, 48.89937523111243678, -22.85493024525475647 ) ) ;
#29290 = CARTESIAN_POINT ( 'NONE',  ( 149.4165763529819344, 225.8585178651493663, 129.0000000000000000 ) ) ;
#29291 = FACE_OUTER_BOUND ( 'NONE', #53078, .T. ) ;
#29293 = ORIENTED_EDGE ( 'NONE', *, *, #10854, .F. ) ;
#29292 = CARTESIAN_POINT ( 'NONE',  ( 313.9975424824652350, 171.8183490441642789, 533.9018882243741473 ) ) ;
#29294 = ORIENTED_EDGE ( 'NONE', *, *, #12997, .T. ) ;
#29295 = AXIS2_PLACEMENT_3D ( 'NONE', #7871, #29321, #51477 ) ;
#29296 = EDGE_LOOP ( 'NONE', ( #44941, #10674, #64325, #36392 ) ) ;
#29297 = CARTESIAN_POINT ( 'NONE',  ( 41.09671232177014844, 8.635892912882344064, 3.259150826632041476 ) ) ;
#29299 = CARTESIAN_POINT ( 'NONE',  ( -179.9997297618090784, 96.71425526203211120, 94.99999999999866418 ) ) ;
#29298 = AXIS2_PLACEMENT_3D ( 'NONE', #15074, #57300, #46735 ) ;
#29300 = CARTESIAN_POINT ( 'NONE',  ( -48.33725449172838751, 12.98311179783359037, -19.24768553186362041 ) ) ;
#29301 = CARTESIAN_POINT ( 'NONE',  ( 102.8518012651273921, 25.61025413220826863, -15.27953052830500091 ) ) ;
#29302 = CARTESIAN_POINT ( 'NONE',  ( 200.4559562755962077, 100.7034888016685557, 3.660617377573986087 ) ) ;
#29303 = EDGE_CURVE ( 'NONE', #35812, #61203, #11488, .T. ) ;
#29304 = CARTESIAN_POINT ( 'NONE',  ( 212.1648021685800245, 119.0365075864307300, 89.65931539195061362 ) ) ;
#29306 = LINE ( 'NONE', #55333, #55712 ) ;
#29305 = AXIS2_PLACEMENT_3D ( 'NONE', #39586, #14244, #67034 ) ;
#29307 = CARTESIAN_POINT ( 'NONE',  ( -85.35172689181706573, 26.07142112926219113, 61.32667841685976384 ) ) ;
#29308 = CARTESIAN_POINT ( 'NONE',  ( -15.31363169557738502, 7.494880774891997888, 37.12813078065121175 ) ) ;
#29309 = VERTEX_POINT ( 'NONE', #11848 ) ;
#29310 = CARTESIAN_POINT ( 'NONE',  ( 11.81843724556921416, 7.412394300769733491, -9.806428785726447828 ) ) ;
#29311 = ORIENTED_EDGE ( 'NONE', *, *, #56681, .F. ) ;
#29312 = ADVANCED_FACE ( 'NONE', ( #17470 ), #14279, .F. ) ;
#29313 = EDGE_LOOP ( 'NONE', ( #16822, #13604, #10072, #7684 ) ) ;
#29314 = EDGE_CURVE ( 'NONE', #59875, #62269, #16442, .T. ) ;
#29315 = FACE_OUTER_BOUND ( 'NONE', #54783, .T. ) ;
#29316 = DIRECTION ( 'NONE',  ( -1.000000000000000000, -0.000000000000000000, -0.000000000000000000 ) ) ;
#29317 = CARTESIAN_POINT ( 'NONE',  ( -173.1211646369891355, 88.63826465341152527, 45.82169460664104577 ) ) ;
#29318 = CIRCLE ( 'NONE', #16940, 65.36598343705435354 ) ;
#29319 = CARTESIAN_POINT ( 'NONE',  ( -99.97541017369790950, 31.62502926470688180, -35.36197685046671779 ) ) ;
#29320 = ADVANCED_FACE ( 'NONE', ( #957 ), #37896, .T. ) ;
#29321 = DIRECTION ( 'NONE',  ( -0.000000000000000000, 1.000000000000000000, -0.000000000000000000 ) ) ;
#29322 = CARTESIAN_POINT ( 'NONE',  ( 111.9975424824652634, 172.0000000000000284, 418.0000000000000568 ) ) ;
#29323 = CARTESIAN_POINT ( 'NONE',  ( 129.1381264900934696, 38.64720302602604107, -37.67339026062629870 ) ) ;
#29324 = VERTEX_POINT ( 'NONE', #6581 ) ;
#29325 = ORIENTED_EDGE ( 'NONE', *, *, #27692, .F. ) ;
#29326 = CARTESIAN_POINT ( 'NONE',  ( 188.0287290159266433, 87.41935856271966543, 87.65909336768878291 ) ) ;
#29327 = CARTESIAN_POINT ( 'NONE',  ( -66.25334423260856909, -7.217961380022510198, 34.48241823979542886 ) ) ;
#29328 = DIRECTION ( 'NONE',  ( 0.000000000000000000, 0.000000000000000000, 1.000000000000000000 ) ) ;
#29329 = CARTESIAN_POINT ( 'NONE',  ( 63.01563776193091826, 12.67277567978500308, -23.87614024170608218 ) ) ;
#29330 = CARTESIAN_POINT ( 'NONE',  ( -51.78153763344963778, 13.82841714689604196, 31.05108900895189805 ) ) ;
#29331 = CARTESIAN_POINT ( 'NONE',  ( 197.8588046850313731, 99.02485934465610740, 66.64561215349371537 ) ) ;
#29332 = VERTEX_POINT ( 'NONE', #27326 ) ;
#29333 = FACE_OUTER_BOUND ( 'NONE', #23693, .T. ) ;
#29334 = CARTESIAN_POINT ( 'NONE',  ( -56.97556689808916985, 16.24958672959845885, -62.30750940606130683 ) ) ;
#29335 = CARTESIAN_POINT ( 'NONE',  ( 197.1975259970231491, 98.19639476549652102, -70.34394312000644334 ) ) ;
#29336 = SHAPE_REPRESENTATION_RELATIONSHIP ( 'NONE' , 'NONE' ,  #38847, #62542 ) ;
#29337 = CARTESIAN_POINT ( 'NONE',  ( 276.9490892766210663, -21.63874093657135589, -3.974828052515721577 ) ) ;
#29338 = CARTESIAN_POINT ( 'NONE',  ( 106.6192711434718206, 27.24117154335861812, 3.695783610869706415 ) ) ;
#29339 = CARTESIAN_POINT ( 'NONE',  ( -165.6210506643948577, 79.15024150453834295, 11.77841337596324500 ) ) ;
#29340 = DIRECTION ( 'NONE',  ( 6.405132834375901070E-16, -1.000000000000000000, -6.405132834375902056E-16 ) ) ;
#29341 = EDGE_CURVE ( 'NONE', #11433, #34620, #26986, .T. ) ;
#29342 = CARTESIAN_POINT ( 'NONE',  ( -189.7238975269522712, 107.7611624801371022, 89.42997806037180908 ) ) ;
#29343 = CARTESIAN_POINT ( 'NONE',  ( -7.330690860789852437, 6.858814156830895570, 71.96013162991093282 ) ) ;
#29344 = ORIENTED_EDGE ( 'NONE', *, *, #69178, .T. ) ;
#29345 = CARTESIAN_POINT ( 'NONE',  ( 278.3839814017205185, 21.48303375171747120, 4.742972355882017155 ) ) ;
#29346 = VECTOR ( 'NONE', #33594, 1000.000000000000000 ) ;
#29347 = CARTESIAN_POINT ( 'NONE',  ( 0.000000000000000000, 0.000000000000000000, 0.000000000000000000 ) ) ;
#29348 = CARTESIAN_POINT ( 'NONE',  ( 99.99999999999997158, 6.000000000000000000, -46.99999999999998579 ) ) ;
#29349 = LINE ( 'NONE', #61013, #40185 ) ;
#29350 = CARTESIAN_POINT ( 'NONE',  ( 60.82895951008426749, -30.68107831874539926, 41.38025477438755928 ) ) ;
#29351 = VECTOR ( 'NONE', #59177, 1000.000000000000000 ) ;
#29352 = ORIENTED_EDGE ( 'NONE', *, *, #51156, .T. ) ;
#29353 = SURFACE_SIDE_STYLE ('',( #19484 ) ) ;
#29354 = CARTESIAN_POINT ( 'NONE',  ( -442.6627218934913230, 399.9999999999997726, 103.5502958579881891 ) ) ;
#29355 = VERTEX_POINT ( 'NONE', #54399 ) ;
#29356 = CIRCLE ( 'NONE', #58558, 25.12245591505646303 ) ;
#29357 = VECTOR ( 'NONE', #22309, 1000.000000000000114 ) ;
#29358 = ORIENTED_EDGE ( 'NONE', *, *, #52712, .T. ) ;
#29359 = CARTESIAN_POINT ( 'NONE',  ( 0.000000000000000000, 0.000000000000000000, 0.000000000000000000 ) ) ;
#29360 = CARTESIAN_POINT ( 'NONE',  ( -178.2381786520593323, 93.01028335822120141, -63.56798082661889282 ) ) ;
#29361 = FACE_OUTER_BOUND ( 'NONE', #23913, .T. ) ;
#29362 = VERTEX_POINT ( 'NONE', #48416 ) ;
#29363 = LINE ( 'NONE', #19150, #49510 ) ;
#29364 = CARTESIAN_POINT ( 'NONE',  ( -179.8996803435688889, 95.00451760716450167, 14.69856830855032470 ) ) ;
#29365 = CARTESIAN_POINT ( 'NONE',  ( -1.857619870843147725, 6.575690665396233037, 15.34000399991449015 ) ) ;
#29366 = MECHANICAL_DESIGN_GEOMETRIC_PRESENTATION_REPRESENTATION (  '', ( #2405 ), #48365 ) ;
#29367 = CARTESIAN_POINT ( 'NONE',  ( -452.6627218934913230, 399.9999999999997726, 83.55029585798818914 ) ) ;
#29368 = PLANE ( 'NONE',  #64063 ) ;
#29369 = CARTESIAN_POINT ( 'NONE',  ( -24.32471770265758337, 9.546495606312143778, -18.39735782029327993 ) ) ;
#29370 = CARTESIAN_POINT ( 'NONE',  ( 138.5721691894143817, 44.34516164557651052, 4.313163325010641813 ) ) ;
#29371 = EDGE_CURVE ( 'NONE', #10959, #13791, #37860, .T. ) ;
#29372 = EDGE_CURVE ( 'NONE', #61844, #22131, #53603, .T. ) ;
#29373 = ORIENTED_EDGE ( 'NONE', *, *, #314, .T. ) ;
#29374 = CARTESIAN_POINT ( 'NONE',  ( 209.9999999999999716, -2.000000000000001776, 93.99999999999998579 ) ) ;
#29375 = EDGE_CURVE ( 'NONE', #28328, #52426, #604, .T. ) ;
#29376 = CARTESIAN_POINT ( 'NONE',  ( -73.09214866197366689, 21.34321757515763096, 6.031536298108171046 ) ) ;
#29377 = FACE_BOUND ( 'NONE', #12409, .T. ) ;
#29378 = DIRECTION ( 'NONE',  ( -1.000000000000000000, 0.000000000000000000, 0.000000000000000000 ) ) ;
#29380 = ORIENTED_EDGE ( 'NONE', *, *, #47710, .T. ) ;
#29379 = PLANE ( 'NONE',  #15239 ) ;
#29381 = CARTESIAN_POINT ( 'NONE',  ( 84.27368848767930842, 18.63026910897604083, -50.45834538360720956 ) ) ;
#29382 = ORIENTED_EDGE ( 'NONE', *, *, #4984, .F. ) ;
#29383 = DIRECTION ( 'NONE',  ( 0.000000000000000000, -1.000000000000000000, 0.000000000000000000 ) ) ;
#29384 = CYLINDRICAL_SURFACE ( 'NONE', #5289, 160.5210298272983778 ) ;
#29385 = FACE_OUTER_BOUND ( 'NONE', #39592, .T. ) ;
#29386 = CARTESIAN_POINT ( 'NONE',  ( 186.6118452967672283, 84.37814701615442914, -11.78640348934926152 ) ) ;
#29387 = CARTESIAN_POINT ( 'NONE',  ( 0.000000000000000000, 35.00000000000000000, 0.000000000000000000 ) ) ;
#29388 = CARTESIAN_POINT ( 'NONE',  ( 8.828807734113995664, 74.48902371486721563, 73.58025477438756923 ) ) ;
#29389 = CARTESIAN_POINT ( 'NONE',  ( 20.77767936488358558, 7.719073965783881164, -91.09253317339127420 ) ) ;
#29390 = CARTESIAN_POINT ( 'NONE',  ( -50.14440374537738876, 14.45628984983895116, 43.50930614590824774 ) ) ;
#29391 = EDGE_LOOP ( 'NONE', ( #34411, #37876 ) ) ;
#29392 = EDGE_CURVE ( 'NONE', #66476, #33038, #10812, .T. ) ;
#29393 = VERTEX_POINT ( 'NONE', #44195 ) ;
#29394 = EDGE_CURVE ( 'NONE', #4959, #65795, #65682, .T. ) ;
#29395 = VECTOR ( 'NONE', #46468, 1000.000000000000000 ) ;
#29396 = CARTESIAN_POINT ( 'NONE',  ( 107.9362503323352627, 27.82881837607798303, 71.10819457095023211 ) ) ;
#29397 = PLANE ( 'NONE',  #7669 ) ;
#29398 = DIRECTION ( 'NONE',  ( -0.000000000000000000, -0.000000000000000000, 1.000000000000000000 ) ) ;
#29399 = AXIS2_PLACEMENT_3D ( 'NONE', #13202, #22352, #11787 ) ;
#29400 = CARTESIAN_POINT ( 'NONE',  ( -2.368959188627552503, -24.88750755625419941, 0.000000000000000000 ) ) ;
#29401 = CARTESIAN_POINT ( 'NONE',  ( -109.7816385129979153, 36.75776661907242726, 64.36293740281786313 ) ) ;
#29402 = CARTESIAN_POINT ( 'NONE',  ( 15.55634918610400241, -15.55634918610406103, 0.000000000000000000 ) ) ;
#29404 = CARTESIAN_POINT ( 'NONE',  ( 162.1014732644455307, 61.34312237409764634, -64.55007820984620537 ) ) ;
#29403 = B_SPLINE_CURVE_WITH_KNOTS ( 'NONE', 3,
 ( #15224, #37352, #53868, #31742, #25795, #21197, #10279, #21872, #52510, #48243, #26125, #43319, #63767, #16597, #5691, #38053 ),
 .UNSPECIFIED., .F., .F.,
 ( 4, 2, 2, 2, 2, 2, 2, 4 ),
 ( 0.000000000000000000, 0.001302991001000006156, 0.002605982002000012312, 0.003908973003000018251, 0.005211964004000024624, 0.006514955005000030996, 0.007817946006000036502, 0.01042392800800004925 ),
 .UNSPECIFIED. ) ;
#29405 = ORIENTED_EDGE ( 'NONE', *, *, #53154, .T. ) ;
#29406 = PRODUCT_DEFINITION_SHAPE ( 'NONE', 'NONE',  #39219 ) ;
#29407 = ORIENTED_EDGE ( 'NONE', *, *, #43268, .F. ) ;
#29408 = EDGE_LOOP ( 'NONE', ( #39029, #29405, #13495, #9102 ) ) ;
#29409 = CIRCLE ( 'NONE', #68708, 5.000000000000000888 ) ;
#29410 = CARTESIAN_POINT ( 'NONE',  ( 56.74421265833603201, -32.44697398030824331, 3.125053320693577513E-16 ) ) ;
#29411 = CARTESIAN_POINT ( 'NONE',  ( -71.39537134557981801, 19.68387687359727778, 93.47482192707475690 ) ) ;
#29412 = CARTESIAN_POINT ( 'NONE',  ( -8.000000000000000000, 0.7809653281576073303, -9.500000000000001776 ) ) ;
#29413 = CARTESIAN_POINT ( 'NONE',  ( 67.56108154898468854, 13.77276756375645128, -37.23494202805936482 ) ) ;
#29414 = DIRECTION ( 'NONE',  ( -0.8118923937861950435, -0.5838071093367415143, 0.000000000000000000 ) ) ;
#29415 = CARTESIAN_POINT ( 'NONE',  ( -62.55184817504200367, 17.87278652436697968, 37.30171783089942039 ) ) ;
#29416 = CLOSED_SHELL ( 'NONE', ( #65442, #21674, #15577, #9048, #43735, #30186, #51291, #21931, #39105, #41389, #18142, #33465, #67887, #59542, #25438, #44372, #39551, #60362, #50185, #49449, #50491, #30197, #5221, #54619, #56902, #43553, #19046, #25817, #32780, #42317, #4321, #44384, #40582, #31534, #10074, #49605, #27093, #16267, #38973, #63611, #19806, #408, #51487, #59629, #32468, #13761, #22771, #31371, #62190, #59313, #21402, #64214, #26045, #19212, #31446, #41588, #50497, #48088, #43592, #63055, #48875, #51949, #66823, #39071, #68322, #21480, #20881, #25966, #57606, #289, #57978, #42480, #5090, #11126, #12707, #12472, #2105, #51064, #68297, #51711, #42999, #23672, #9938, #27489, #67823, #36617, #58134, #6598, #49849, #49454, #32320, #51762, #41543, #29623, #65471, #41687, #38701, #63551, #48314, #5634, #16882, #13739, #11319, #68778, #57864, #66091, #51071 ) ) ;
#29417 = DIRECTION ( 'NONE',  ( 0.000000000000000000, 0.000000000000000000, -1.000000000000000000 ) ) ;
#29418 = B_SPLINE_CURVE_WITH_KNOTS ( 'NONE', 3,
 ( #33841, #28561, #66222, #39459, #65501, #55992, #34198, #12732, #29590, #55631, #7807, #60216, #12033, #30993, #46460, #57372, #61946, #52090, #46814, #29950, #19735, #8498, #13765, #14465, #3910, #41196, #30301, #45782, #40495, #14113, #51415, #57035, #52440, #3225, #25719, #14799, #31336, #67941, #9532, #62657, #41540, #25379, #3555, #35223, #9185 ),
 .UNSPECIFIED., .F., .F.,
 ( 4, 2, 2, 1, 2, 2, 2, 2, 2, 2, 2, 2, 2, 2, 2, 2, 2, 2, 2, 2, 2, 2, 4 ),
 ( 0.02346057189573571775, 0.02492590417315498907, 0.02565857031186461953, 0.02639123645057425346, 0.02712390258928388739, 0.02785656872799351785, 0.02932190100541277183, 0.03005456714412239189, 0.03078723328283201194, 0.03225256556025124510, 0.03298523169896087903, 0.03371789783767051296, 0.03518323011508977388, 0.03664856239250902786, 0.03738122853121866179, 0.03811389466992828878, 0.03957922694734754970, 0.04104455922476681062, 0.04250989150218607154, 0.04324255764089569160, 0.04397522377960530471, 0.04544055605702456563, 0.04690588833444381961 ),
 .UNSPECIFIED. ) ;
#29419 = CARTESIAN_POINT ( 'NONE',  ( 60.40531521312255592, 13.11276739283241710, 30.27770789689484943 ) ) ;
#29420 = CARTESIAN_POINT ( 'NONE',  ( 33.60094621367903756, 7.725337012799395886, 86.30269869955574791 ) ) ;
#29421 = ORIENTED_EDGE ( 'NONE', *, *, #67680, .F. ) ;
#29422 = CARTESIAN_POINT ( 'NONE',  ( -2.866724795119727887, 6.618578306599220085, -37.26994514656705348 ) ) ;
#29423 = CARTESIAN_POINT ( 'NONE',  ( 33.40240406473286328, 1.250000000000020206, 6.893342931450256117 ) ) ;
#29424 = CARTESIAN_POINT ( 'NONE',  ( -189.2442476610617916, 107.0963225822736433, -41.67591933138472626 ) ) ;
#29425 = CARTESIAN_POINT ( 'NONE',  ( 30.12852347772541961, 58.62603998952764783, 73.58025477438755502 ) ) ;
#29426 = CARTESIAN_POINT ( 'NONE',  ( 284.4930355657062364, -21.89000795769331731, -2.217852339353765245 ) ) ;
#29427 = CARTESIAN_POINT ( 'NONE',  ( -109.0297561673456244, 36.34391931706013423, -66.07908170626511435 ) ) ;
#29428 = CARTESIAN_POINT ( 'NONE',  ( 126.3554864210861837, 38.22801630372153170, -16.45079121831199487 ) ) ;
#29429 = ORIENTED_EDGE ( 'NONE', *, *, #51568, .T. ) ;
#29430 = CARTESIAN_POINT ( 'NONE',  ( 130.7260570116704343, 40.73146260246712558, -36.69216764449773649 ) ) ;
#29431 = FACE_OUTER_BOUND ( 'NONE', #62979, .T. ) ;
#29432 = CARTESIAN_POINT ( 'NONE',  ( 0.3173508448886565581, -8.480771745766405800, -1.310872448937993928 ) ) ;
#29433 = CONTEXT_DEPENDENT_SHAPE_REPRESENTATION ( #36816, #46842 ) ;
#29434 = CARTESIAN_POINT ( 'NONE',  ( -169.3169969001603761, 82.99181976410343964, 85.54137684301231559 ) ) ;
#29435 = ORIENTED_EDGE ( 'NONE', *, *, #45883, .T. ) ;
#29436 = CARTESIAN_POINT ( 'NONE',  ( 127.4992165631961569, 38.87141012667727580, 6.155430928021909942 ) ) ;
#29437 = CARTESIAN_POINT ( 'NONE',  ( -143.8566410313463564, 59.53044870492036011, -10.51068613821876774 ) ) ;
#29438 = FACE_OUTER_BOUND ( 'NONE', #36588, .T. ) ;
#29439 = CARTESIAN_POINT ( 'NONE',  ( 158.1693234658825133, 59.47518947913521714, 83.10736755387232222 ) ) ;
#29440 = ORIENTED_EDGE ( 'NONE', *, *, #27865, .F. ) ;
#29441 = CARTESIAN_POINT ( 'NONE',  ( 29.86806733335506792, 70.00000000000000000, 2.810436579993894401 ) ) ;
#29442 = CARTESIAN_POINT ( 'NONE',  ( -156.0209085498131856, 71.27066046086515883, 34.46375622281639295 ) ) ;
#29443 = CIRCLE ( 'NONE', #3630, 25.00000000000296296 ) ;
#29444 = DIRECTION ( 'NONE',  ( -0.000000000000000000, 1.000000000000000000, -0.000000000000000000 ) ) ;
#29445 = CARTESIAN_POINT ( 'NONE',  ( 81.76092782665034520, 17.81692437267514606, 16.07796231263216313 ) ) ;
#29447 = VERTEX_POINT ( 'NONE', #22061 ) ;
#29446 = CARTESIAN_POINT ( 'NONE',  ( -20.55634918610408945, -31.11269837220804035, 2.000000000000001776 ) ) ;
#29448 = CARTESIAN_POINT ( 'NONE',  ( 57.08336938683660833, 11.37442068895389014, 41.92839751438462059 ) ) ;
#29449 = EDGE_CURVE ( 'NONE', #69450, #48350, #64628, .T. ) ;
#29450 = EDGE_LOOP ( 'NONE', ( #5057, #8885, #51592, #23627, #35369, #40162, #67236, #43858, #23065 ) ) ;
#29451 = VECTOR ( 'NONE', #62201, 1000.000000000000114 ) ;
#29452 = ORIENTED_EDGE ( 'NONE', *, *, #16682, .F. ) ;
#29453 = CARTESIAN_POINT ( 'NONE',  ( 174.6242782760049863, 73.69713439533578025, 40.62850159014154627 ) ) ;
#29454 = EDGE_CURVE ( 'NONE', #20799, #61203, #55852, .T. ) ;
#29456 = CARTESIAN_POINT ( 'NONE',  ( -30.00000000000000355, -30.00000000000000355, 0.000000000000000000 ) ) ;
#29455 = AXIS2_PLACEMENT_3D ( 'NONE', #32651, #16474, #65722 ) ;
#29458 = VERTEX_POINT ( 'NONE', #43503 ) ;
#29457 = CARTESIAN_POINT ( 'NONE',  ( -190.6985136298601731, 109.1272424661242582, 94.99999999999866418 ) ) ;
#29459 = DIRECTION ( 'NONE',  ( 0.000000000000000000, 0.000000000000000000, 1.000000000000000000 ) ) ;
#29460 = EDGE_CURVE ( 'NONE', #10653, #41171, #59456, .T. ) ;
#29461 = AXIS2_PLACEMENT_3D ( 'NONE', #63197, #63540, #52627 ) ;
#29462 = CARTESIAN_POINT ( 'NONE',  ( -24.39249304643357519, -60.24953346690487166, 170.0000000000000000 ) ) ;
#29463 = CARTESIAN_POINT ( 'NONE',  ( -72.77296415263759854, 21.23032531836536307, -47.28051332976320253 ) ) ;
#29464 = ORIENTED_EDGE ( 'NONE', *, *, #12, .F. ) ;
#29465 = CARTESIAN_POINT ( 'NONE',  ( 210.6592759200687794, 116.7161312026394029, -66.11224254623208196 ) ) ;
#29466 = CARTESIAN_POINT ( 'NONE',  ( 137.3861614007145135, 44.78548268714477132, 43.63210590249699550 ) ) ;
#29467 = DIRECTION ( 'NONE',  ( -0.000000000000000000, -0.000000000000000000, -1.000000000000000000 ) ) ;
#29468 = CARTESIAN_POINT ( 'NONE',  ( -31.43908319763710679, -170.0000000000000000, 10.87190381572550280 ) ) ;
#29469 = CARTESIAN_POINT ( 'NONE',  ( 67.93317348534927191, 14.90531593353391671, -64.38129521441156555 ) ) ;
#29470 = B_SPLINE_CURVE_WITH_KNOTS ( 'NONE', 3,
 ( #22545, #55599, #7428, #8109, #29560, #67552, #39090, #60531, #19010, #66873, #28880, #51024, #60870, #33801, #49969, #55241, #7771, #56642, #1803, #45041, #28523, #12345, #29221, #12695, #23258, #50332, #8463, #67226, #29914, #51374, #7065, #40462, #66184, #3191, #23603, #44704, #34855, #17976, #34161, #2148, #39421, #18315, #39771 ),
 .UNSPECIFIED., .F., .F.,
 ( 4, 2, 2, 2, 2, 2, 2, 2, 2, 2, 2, 2, 1, 2, 2, 2, 2, 2, 2, 2, 2, 4 ),
 ( 0.02358007599568756954, 0.02505677178601662877, 0.02579511968118114798, 0.02653346757634567066, 0.02801016336667472989, 0.02948685915700378912, 0.03022520705216830833, 0.03096355494733283448, 0.03244025073766187983, 0.03391694652799092519, 0.03539364231831997054, 0.03613199021348449669, 0.03687033810864901590, 0.03760868600381354204, 0.03834703389897806125, 0.03982372968930709967, 0.04130042547963613808, 0.04277712126996517650, 0.04351546916512970264, 0.04425381706029422879, 0.04573051285062328802, 0.04720720864095235419 ),
 .UNSPECIFIED. ) ;
#29471 = EDGE_CURVE ( 'NONE', #8304, #64355, #45948, .T. ) ;
#29472 = ORIENTED_EDGE ( 'NONE', *, *, #33602, .F. ) ;
#29473 = EDGE_LOOP ( 'NONE', ( #18289, #2159, #32314, #46701 ) ) ;
#29474 = ORIENTED_EDGE ( 'NONE', *, *, #17943, .T. ) ;
#29475 = PLANE ( 'NONE',  #27220 ) ;
#29476 = SURFACE_SIDE_STYLE ('',( #8023 ) ) ;
#29477 = DIRECTION ( 'NONE',  ( -0.000000000000000000, -0.000000000000000000, -1.000000000000000000 ) ) ;
#29478 = DIRECTION ( 'NONE',  ( -0.000000000000000000, 1.000000000000000000, -0.000000000000000000 ) ) ;
#29479 = PLANE ( 'NONE',  #31426 ) ;
#29480 = DIRECTION ( 'NONE',  ( -0.000000000000000000, -0.000000000000000000, 1.000000000000000000 ) ) ;
#29481 = CARTESIAN_POINT ( 'NONE',  ( -71.57025115638936086, 20.80908992785612099, -18.25007248965231810 ) ) ;
#29482 = VERTEX_POINT ( 'NONE', #13938 ) ;
#29483 = CARTESIAN_POINT ( 'NONE',  ( -109.3585523124447576, 37.67345343047318806, 40.55142789949354665 ) ) ;
#29484 = ORIENTED_EDGE ( 'NONE', *, *, #16464, .F. ) ;
#29485 = CARTESIAN_POINT ( 'NONE',  ( -95.08295392099647358, 30.38371693924408135, -94.08104204696795136 ) ) ;
#29486 = CARTESIAN_POINT ( 'NONE',  ( 84.97658021689288432, 19.92447159015899061, 56.73708945548396798 ) ) ;
#29487 = ORIENTED_EDGE ( 'NONE', *, *, #7324, .T. ) ;
#29488 = CARTESIAN_POINT ( 'NONE',  ( 74.01791526339553684, 12.16185512414947034, 170.0000000000000000 ) ) ;
#29489 = CARTESIAN_POINT ( 'NONE',  ( -196.7348448768811409, -170.0000000000000000, -68.95563438847170801 ) ) ;
#29490 = CARTESIAN_POINT ( 'NONE',  ( 121.4242852856285140, 0.000000000000000000, -20.00000000000000000 ) ) ;
#29491 = CARTESIAN_POINT ( 'NONE',  ( -15.27733754929849397, 8.502213909106947298, -41.93932207287456748 ) ) ;
#29492 = DIRECTION ( 'NONE',  ( -1.000000000000000000, 0.000000000000000000, 0.000000000000000000 ) ) ;
#29493 = ORIENTED_EDGE ( 'NONE', *, *, #62408, .T. ) ;
#29494 = CIRCLE ( 'NONE', #8159, 243.4957430088094839 ) ;
#29495 = CARTESIAN_POINT ( 'NONE',  ( -105.5524494737681920, 34.47420209251092160, -89.44164320824525305 ) ) ;
#29496 = CARTESIAN_POINT ( 'NONE',  ( -155.1302201283145905, 69.09929365814129198, -10.49887033788333746 ) ) ;
#29497 = VERTEX_POINT ( 'NONE', #2357 ) ;
#29498 = LINE ( 'NONE', #8757, #29451 ) ;
#29499 = CARTESIAN_POINT ( 'NONE',  ( 9.737557066527559257, 192.0000000000000000, 2.275957463600584596 ) ) ;
#29500 = DIRECTION ( 'NONE',  ( 0.000000000000000000, 0.000000000000000000, 1.000000000000000000 ) ) ;
#29501 = EDGE_LOOP ( 'NONE', ( #11782, #24750, #27796, #24578 ) ) ;
#29502 = LINE ( 'NONE', #18259, #61425 ) ;
#29503 = CARTESIAN_POINT ( 'NONE',  ( 150.2941978382489197, 53.52137138947627903, -72.66572206626821639 ) ) ;
#29504 = CARTESIAN_POINT ( 'NONE',  ( -37.79823708645147917, 10.72197716414928692, 33.73258574390899156 ) ) ;
#29505 = AXIS2_PLACEMENT_3D ( 'NONE', #46631, #35050, #3383 ) ;
#29506 = CARTESIAN_POINT ( 'NONE',  ( 138.6020257460769471, 44.36414356192210562, -37.69519993456503926 ) ) ;
#29507 = ORIENTED_EDGE ( 'NONE', *, *, #13717, .T. ) ;
#29508 = CIRCLE ( 'NONE', #38488, 5.000000000000004441 ) ;
#29509 = CARTESIAN_POINT ( 'NONE',  ( -7.662721893488489755, 395.0000000000064801, 308.5502958579854180 ) ) ;
#29510 = LINE ( 'NONE', #50974, #25635 ) ;
#29511 = ORIENTED_EDGE ( 'NONE', *, *, #62373, .F. ) ;
#29512 = CARTESIAN_POINT ( 'NONE',  ( 26.11269837220809364, 15.55634918610396866, 85.00100000000000477 ) ) ;
#29513 = CARTESIAN_POINT ( 'NONE',  ( -452.6627218934861503, 365.0000000000064233, -146.4497041420121377 ) ) ;
#29514 = EDGE_CURVE ( 'NONE', #22434, #40256, #45601, .T. ) ;
#29515 = CARTESIAN_POINT ( 'NONE',  ( 50.97490815085634352, 6.000000000000000000, -36.68900338898716740 ) ) ;
#29516 = CARTESIAN_POINT ( 'NONE',  ( 204.6977192012829789, 108.0580384837234931, -90.01503221354883522 ) ) ;
#29517 = LINE ( 'NONE', #17213, #59598 ) ;
#29518 = CARTESIAN_POINT ( 'NONE',  ( -118.6157340058430236, 41.88485941274769431, -67.42784937615110152 ) ) ;
#29519 = ORIENTED_EDGE ( 'NONE', *, *, #9690, .T. ) ;
#29520 = LINE ( 'NONE', #2802, #7596 ) ;
#29521 = CARTESIAN_POINT ( 'NONE',  ( -31.43908319763709258, 9.591432048623765638, 18.37190381572551701 ) ) ;
#29522 = CARTESIAN_POINT ( 'NONE',  ( 63.01563776193090405, 12.67277567978497643, 71.65751152968501003 ) ) ;
#29523 = CARTESIAN_POINT ( 'NONE',  ( 137.6104751318276840, 44.92718313329106650, 3.668482549248312186 ) ) ;
#29524 = FACE_OUTER_BOUND ( 'NONE', #10619, .T. ) ;
#29525 = ORIENTED_EDGE ( 'NONE', *, *, #9690, .F. ) ;
#29526 = CARTESIAN_POINT ( 'NONE',  ( 8.000000000000000000, -4.618802153517021836, -9.500000000000000000 ) ) ;
#29527 = EDGE_CURVE ( 'NONE', #2227, #43392, #39292, .T. ) ;
#29528 = CARTESIAN_POINT ( 'NONE',  ( 40.81683905770021425, 8.677580323404230356, 13.79046412291064883 ) ) ;
#29529 = ORIENTED_EDGE ( 'NONE', *, *, #18278, .F. ) ;
#29530 = CARTESIAN_POINT ( 'NONE',  ( 69.72564955710444679, 15.37006465677309386, 67.51718129031921478 ) ) ;
#29531 = CARTESIAN_POINT ( 'NONE',  ( 132.3763947360081374, 40.53774838062970076, 83.34026022301281955 ) ) ;
#29532 = AXIS2_PLACEMENT_3D ( 'NONE', #31726, #10607, #4646 ) ;
#29533 = ORIENTED_EDGE ( 'NONE', *, *, #46920, .F. ) ;
#29534 = CARTESIAN_POINT ( 'NONE',  ( 164.8908506817024033, 64.97619709085125805, -42.49963807020401418 ) ) ;
#29535 = ADVANCED_FACE ( 'NONE', ( #62119 ), #67087, .F. ) ;
#29536 = DIRECTION ( 'NONE',  ( -0.9561276726666719794, 1.170918693907448050E-16, 0.2929502919626694180 ) ) ;
#29537 = FACE_OUTER_BOUND ( 'NONE', #34746, .T. ) ;
#29538 = DIRECTION ( 'NONE',  ( 0.000000000000000000, -1.000000000000000000, 0.000000000000000000 ) ) ;
#29539 = AXIS2_PLACEMENT_3D ( 'NONE', #66015, #11823, #38555 ) ;
#29540 = ORIENTED_EDGE ( 'NONE', *, *, #68607, .T. ) ;
#29541 = DIRECTION ( 'NONE',  ( -0.2660368455666826670, 0.9639628606958513535, 0.000000000000000000 ) ) ;
#29542 = VECTOR ( 'NONE', #20851, 1000.000000000000114 ) ;
#29543 = DIRECTION ( 'NONE',  ( 1.000000000000000000, 0.000000000000000000, 0.000000000000000000 ) ) ;
#29544 = DIRECTION ( 'NONE',  ( -1.000000000000000000, 0.000000000000000000, 7.703719777548943412E-34 ) ) ;
#29545 = CARTESIAN_POINT ( 'NONE',  ( 80.71682498289317209, 18.54204664833077487, -11.83616858174047515 ) ) ;
#29546 = CARTESIAN_POINT ( 'NONE',  ( -177.9671374276251754, 94.25162618736496256, -90.16083395623414276 ) ) ;
#29547 = VECTOR ( 'NONE', #20167, 1000.000000000000000 ) ;
#29548 = CARTESIAN_POINT ( 'NONE',  ( -142.2675133814582011, 58.27369719190851072, -93.98005135264823195 ) ) ;
#29549 = CARTESIAN_POINT ( 'NONE',  ( 130.3245512970360664, 39.33195360491889403, -63.73478426897061411 ) ) ;
#29550 = EDGE_CURVE ( 'NONE', #2387, #4848, #63720, .T. ) ;
#29551 = ORIENTED_EDGE ( 'NONE', *, *, #17779, .T. ) ;
#29552 = CARTESIAN_POINT ( 'NONE',  ( -98.68609963468202295, 32.11186931716883208, 71.46360670857458786 ) ) ;
#29553 = CARTESIAN_POINT ( 'NONE',  ( -10.92576759990585877, 8.121994053275063408, 71.29367127698461104 ) ) ;
#29554 = VERTEX_POINT ( 'NONE', #15667 ) ;
#29555 = AXIS2_PLACEMENT_3D ( 'NONE', #12972, #23867, #45310 ) ;
#29556 = ADVANCED_FACE ( 'NONE', ( #25549 ), #37116, .T. ) ;
#29557 = EDGE_CURVE ( 'NONE', #52636, #36166, #5276, .T. ) ;
#29558 = CARTESIAN_POINT ( 'NONE',  ( -149.9471644042846776, 65.87751327280741975, -49.80312880028602507 ) ) ;
#29559 = CARTESIAN_POINT ( 'NONE',  ( 0.6527133886630186455, -8.860760056385776906, -0.4969600502617733118 ) ) ;
#29560 = CARTESIAN_POINT ( 'NONE',  ( -33.36965723649377935, 10.93726715887721745, 30.46507517067076876 ) ) ;
#29561 = CARTESIAN_POINT ( 'NONE',  ( -149.5074843970971017, 64.17983161892348676, -61.65738112195564469 ) ) ;
#29562 = CYLINDRICAL_SURFACE ( 'NONE', #38172, 7.500000000000013323 ) ;
#29563 = CARTESIAN_POINT ( 'NONE',  ( -48.33725449172840882, 12.98311179783359748, -72.93678671279100456 ) ) ;
#29564 = CARTESIAN_POINT ( 'NONE',  ( -0.3740447803642790170, 7.527031846085009192, -17.05744638557283821 ) ) ;
#29565 = CARTESIAN_POINT ( 'NONE',  ( 175.5493994043409316, 73.18740965572600032, 15.03151793349688070 ) ) ;
#29566 = CARTESIAN_POINT ( 'NONE',  ( -55.05276343752909440, 14.68156374112637508, 18.47277718246750311 ) ) ;
#29567 = ORIENTED_EDGE ( 'NONE', *, *, #34348, .T. ) ;
#29568 = CARTESIAN_POINT ( 'NONE',  ( -21.93488196095011844, 35.49895255660060656, 13.79046340968177908 ) ) ;
#29569 = VERTEX_POINT ( 'NONE', #26221 ) ;
#29570 = FILL_AREA_STYLE_COLOUR ( '', #17166 ) ;
#29571 = DIRECTION ( 'NONE',  ( 0.000000000000000000, 0.000000000000000000, 1.000000000000000000 ) ) ;
#29572 = DIRECTION ( 'NONE',  ( 0.3962817440048567175, 0.9137562205704280460, -0.08950055160341974236 ) ) ;
#29573 = CARTESIAN_POINT ( 'NONE',  ( 64.52696037203357093, 10.43950074664854633, 41.38025477438755928 ) ) ;
#29574 = DIRECTION ( 'NONE',  ( -0.000000000000000000, -0.000000000000000000, -1.000000000000000000 ) ) ;
#29575 = CARTESIAN_POINT ( 'NONE',  ( -104.5916564445180086, 35.10571011602408475, -8.519735482012867678 ) ) ;
#29576 = CARTESIAN_POINT ( 'NONE',  ( 55.00000000000000000, 0.000000000000000000, 0.000000000000000000 ) ) ;
#29577 = CARTESIAN_POINT ( 'NONE',  ( -172.7154982671752066, 86.67743928531947972, 57.66624519710474317 ) ) ;
#29578 = ORIENTED_EDGE ( 'NONE', *, *, #64112, .F. ) ;
#29579 = ORIENTED_EDGE ( 'NONE', *, *, #63356, .F. ) ;
#29580 = FACE_BOUND ( 'NONE', #54135, .T. ) ;
#29581 = CARTESIAN_POINT ( 'NONE',  ( -65.00200000000002376, 1.250000000000021982, 3.061616997868437868E-16 ) ) ;
#29582 = CARTESIAN_POINT ( 'NONE',  ( 17.14961149657550976, 48.73599200008756327, 26.66469104408689716 ) ) ;
#29583 = CYLINDRICAL_SURFACE ( 'NONE', #31662, 5.000000000000004441 ) ;
#29584 = DIRECTION ( 'NONE',  ( -0.000000000000000000, -0.000000000000000000, -1.000000000000000000 ) ) ;
#29585 = AXIS2_PLACEMENT_3D ( 'NONE', #47725, #25265, #21015 ) ;
#29586 = CARTESIAN_POINT ( 'NONE',  ( 63.01563776193090405, 13.70579113808098093, -8.876140241706053757 ) ) ;
#29587 = VERTEX_POINT ( 'NONE', #52600 ) ;
#29588 = CARTESIAN_POINT ( 'NONE',  ( 123.4242852856285566, 6.000000000000000000, -30.00000000000000000 ) ) ;
#29589 = CARTESIAN_POINT ( 'NONE',  ( -10.91976120871578182, 7.112268444252506150, 57.62380858786094961 ) ) ;
#29590 = CARTESIAN_POINT ( 'NONE',  ( 12.04188192036244942, 7.416006018508748632, 57.85736376901041211 ) ) ;
#29591 = VECTOR ( 'NONE', #37881, 1000.000000000000000 ) ;
#29592 = LINE ( 'NONE', #2871, #17215 ) ;
#29593 = EDGE_CURVE ( 'NONE', #17986, #35602, #19235, .T. ) ;
#29594 = CARTESIAN_POINT ( 'NONE',  ( -452.6627218934913230, 399.9999999999998295, -146.4497041420117398 ) ) ;
#29595 = CIRCLE ( 'NONE', #64383, 21.99999999999998579 ) ;
#29596 = EDGE_CURVE ( 'NONE', #35021, #32880, #15789, .T. ) ;
#29597 = VECTOR ( 'NONE', #23569, 1000.000000000000000 ) ;
#29598 = ORIENTED_EDGE ( 'NONE', *, *, #15260, .F. ) ;
#29599 = VERTEX_POINT ( 'NONE', #11067 ) ;
#29600 = CYLINDRICAL_SURFACE ( 'NONE', #42371, 65.00000000000000000 ) ;
#29601 = DIRECTION ( 'NONE',  ( -0.000000000000000000, -0.000000000000000000, 1.000000000000000000 ) ) ;
#29602 = AXIS2_PLACEMENT_3D ( 'NONE', #26455, #15205, #42284 ) ;
#29603 = CARTESIAN_POINT ( 'NONE',  ( 2.699999999999990408, 0.000000000000000000, -19.99999999999998934 ) ) ;
#29604 = CARTESIAN_POINT ( 'NONE',  ( -175.9944734395086243, 91.92390745845762012, 18.41779132216174375 ) ) ;
#29605 = CARTESIAN_POINT ( 'NONE',  ( 8.984386073292506936, 6.377982749901330628, 94.42819228249486230 ) ) ;
#29606 = CARTESIAN_POINT ( 'NONE',  ( 79.38459371357853911, 17.07499996355401706, -68.16129631415398649 ) ) ;
#29607 = VERTEX_POINT ( 'NONE', #32530 ) ;
#29609 = EDGE_CURVE ( 'NONE', #52822, #60122, #65960, .T. ) ;
#29608 = PLANE ( 'NONE',  #64024 ) ;
#29610 = CARTESIAN_POINT ( 'NONE',  ( -4.000000000000009770, -6.928203230275505220, -9.500000000000000000 ) ) ;
#29611 = ORIENTED_EDGE ( 'NONE', *, *, #32716, .F. ) ;
#29612 = EDGE_CURVE ( 'NONE', #60419, #23236, #53528, .T. ) ;
#29613 = CARTESIAN_POINT ( 'NONE',  ( 417.3372781065085633, 400.0000000000000568, -146.4497041420118535 ) ) ;
#29614 = VERTEX_POINT ( 'NONE', #55898 ) ;
#29615 = CARTESIAN_POINT ( 'NONE',  ( -82.93267503967651066, 23.99263498936122474, -63.28692396105326168 ) ) ;
#29616 = CARTESIAN_POINT ( 'NONE',  ( 46.66904755831207297, -10.55634918610412853, 0.000000000000000000 ) ) ;
#29617 = CARTESIAN_POINT ( 'NONE',  ( 311.9975424824652350, 296.0000000000000000, 529.9060149868646477 ) ) ;
#29618 = APPLICATION_CONTEXT ( 'automotive_design' ) ;
#29619 = VERTEX_POINT ( 'NONE', #56235 ) ;
#29620 = ADVANCED_FACE ( 'NONE', ( #23549 ), #24930, .T. ) ;
#29621 = ORIENTED_EDGE ( 'NONE', *, *, #54069, .F. ) ;
#29622 = CARTESIAN_POINT ( 'NONE',  ( 46.51679720856117939, 10.46086439153924452, 61.83516232796673506 ) ) ;
#29623 = ADVANCED_FACE ( 'NONE', ( #57284 ), #46364, .F. ) ;
#29624 = DIRECTION ( 'NONE',  ( -0.000000000000000000, -0.000000000000000000, -1.000000000000000000 ) ) ;
#29625 = CARTESIAN_POINT ( 'NONE',  ( 19.74724861314306779, 6.659670522263898107, 4.295403914482277763 ) ) ;
#29626 = ORIENTED_EDGE ( 'NONE', *, *, #15378, .T. ) ;
#29627 = DIRECTION ( 'NONE',  ( 0.000000000000000000, 1.000000000000000000, 0.000000000000000000 ) ) ;
#29628 = CARTESIAN_POINT ( 'NONE',  ( 177.0110682437507705, 75.98481089748382544, -76.88340400380999995 ) ) ;
#29629 = AXIS2_PLACEMENT_3D ( 'NONE', #54138, #5961, #48857 ) ;
#29630 = FACE_OUTER_BOUND ( 'NONE', #60747, .T. ) ;
#29631 = CARTESIAN_POINT ( 'NONE',  ( 110.7114632166112216, 29.09878355652112347, -24.07788697519004373 ) ) ;
#29632 = CARTESIAN_POINT ( 'NONE',  ( 79.52639011421921111, 18.17129627604989395, -40.86144025082357700 ) ) ;
#29634 = ORIENTED_EDGE ( 'NONE', *, *, #23112, .T. ) ;
#29633 = DIRECTION ( 'NONE',  ( -0.000000000000000000, 1.000000000000000000, -0.000000000000000000 ) ) ;
#29635 = VERTEX_POINT ( 'NONE', #8762 ) ;
#29636 = AXIS2_PLACEMENT_3D ( 'NONE', #27661, #590, #58976 ) ;
#29637 = EDGE_CURVE ( 'NONE', #45426, #7527, #8051, .T. ) ;
#29638 = EDGE_CURVE ( 'NONE', #38509, #23556, #14021, .T. ) ;
#29639 = ORIENTED_EDGE ( 'NONE', *, *, #32710, .T. ) ;
#29640 = VECTOR ( 'NONE', #14459, 1000.000000000000000 ) ;
#29641 = CARTESIAN_POINT ( 'NONE',  ( 46.89006465517227440, 9.501960077668742954, 11.05812210281710328 ) ) ;
#29642 = CARTESIAN_POINT ( 'NONE',  ( -176.6647631907062816, 92.70765962153599560, 85.38109267834556704 ) ) ;
#29643 = CARTESIAN_POINT ( 'NONE',  ( -47.56463531432803649, 12.80077789972090230, -15.38160938467773775 ) ) ;
#29644 = CARTESIAN_POINT ( 'NONE',  ( 103.9652201950894721, 26.08439499369983494, -12.46680327629901619 ) ) ;
#29645 = EDGE_CURVE ( 'NONE', #46683, #16988, #29502, .T. ) ;
#29646 = CARTESIAN_POINT ( 'NONE',  ( 201.9777685760379597, 102.6876480786892927, 2.861658522975385921 ) ) ;
#29647 = AXIS2_PLACEMENT_3D ( 'NONE', #56138, #18511, #39962 ) ;
#29648 = CARTESIAN_POINT ( 'NONE',  ( 447.3372781065085064, 400.0000000000009663, -146.4497041420118535 ) ) ;
#29649 = CARTESIAN_POINT ( 'NONE',  ( 206.0312234087882644, 109.9233711042669484, 82.99752539405173479 ) ) ;
#29650 = VECTOR ( 'NONE', #13774, 1000.000000000000000 ) ;
#29651 = CARTESIAN_POINT ( 'NONE',  ( 207.4566510040494620, 111.9649643341356011, 29.73049175326031701 ) ) ;
#29652 = CARTESIAN_POINT ( 'NONE',  ( -85.89078989036973155, 26.29712602777652464, 62.73225277927918597 ) ) ;
#29653 = LINE ( 'NONE', #2925, #53362 ) ;
#29654 = VERTEX_POINT ( 'NONE', #34797 ) ;
#29655 = B_SPLINE_CURVE_WITH_KNOTS ( 'NONE', 3,
 ( #56094, #44494, #29707, #65976, #60673, #12490, #61368, #28670, #29360, #23407, #44843, #66328, #18117, #39571, #50813, #61022, #12849, #58491, #31435, #41985, #15258, #51517, #25135, #41305, #57479, #58167, #36021, #57140, #52867, #63449, #15604, #25482, #41643, #3321, #4362, #35688, #3661, #36719, #63099, #52539, #46922, #14901, #9983, #30397, #68384, #36367 ),
 .UNSPECIFIED., .F., .F.,
 ( 4, 2, 2, 2, 2, 2, 2, 2, 2, 2, 2, 2, 2, 2, 2, 2, 2, 2, 2, 2, 2, 2, 4 ),
 ( 1.387778780781445676E-17, 0.003736383952885294346, 0.005604575929327934580, 0.007472767905770574814, 0.008406863893991927891, 0.009340959882213282703, 0.01120915185865596284, 0.01214324784687731938, 0.01307734383509867593, 0.01401143982332003421, 0.01494553581154139076, 0.01587963179976274730, 0.01681372778798410211, 0.01774782377620546386, 0.01868191976442681868, 0.01961601575264817349, 0.02055011174086953177, 0.02148420772909088658, 0.02241830371731224139, 0.02428649569375490244, 0.02615468767019755655, 0.02802287964664021760, 0.02989107162308287519 ),
 .UNSPECIFIED. ) ;
#29656 = CARTESIAN_POINT ( 'NONE',  ( 10.55634918610397577, -26.11269837220809364, 0.000000000000000000 ) ) ;
#29657 = ORIENTED_EDGE ( 'NONE', *, *, #3064, .F. ) ;
#29658 = ORIENTED_EDGE ( 'NONE', *, *, #58975, .T. ) ;
#29659 = CYLINDRICAL_SURFACE ( 'NONE', #63530, 7.500000000000013323 ) ;
#29660 = CARTESIAN_POINT ( 'NONE',  ( 188.5651904823862139, 88.01586411309101265, -69.95864106785619185 ) ) ;
#29661 = VECTOR ( 'NONE', #22919, 1000.000000000000000 ) ;
#29662 = CARTESIAN_POINT ( 'NONE',  ( -165.9154624515710168, 80.89088623112735377, 40.42332398115727443 ) ) ;
#29663 = DIRECTION ( 'NONE',  ( 1.000000000000000000, 0.000000000000000000, 0.000000000000000000 ) ) ;
#29664 = CARTESIAN_POINT ( 'NONE',  ( -24.03640295269301319, 9.507963273819770578, 9.642600505910863262 ) ) ;
#29665 = CARTESIAN_POINT ( 'NONE',  ( 209.9999999999999716, 190.0000000000000000, 72.99999999999998579 ) ) ;
#29666 = CARTESIAN_POINT ( 'NONE',  ( -36.11269837220801548, 36.11269837220812207, 2.000000000000001776 ) ) ;
#29667 = CARTESIAN_POINT ( 'NONE',  ( 126.6395826915639731, 37.23416510613625974, -45.58068663486469063 ) ) ;
#29668 = ORIENTED_EDGE ( 'NONE', *, *, #61211, .F. ) ;
#29669 = B_SPLINE_CURVE_WITH_KNOTS ( 'NONE', 3,
 ( #57670, #4204, #47784, #15784, #62942, #10158, #9135, #20718, #69244, #9482, #26007, #63639, #48122, #47434, #26348, #68564, #21074, #26691, #37230, #30940, #3857, #20037, #42845, #52384, #41491, #25669, #52040, #46756, #41833, #31620, #68229, #47102, #63290, #36559, #58009, #9828 ),
 .UNSPECIFIED., .F., .F.,
 ( 4, 2, 2, 2, 2, 2, 2, 2, 2, 2, 2, 2, 2, 2, 2, 2, 2, 4 ),
 ( 3.469446951953614189E-18, 0.001545474820159074359, 0.003090949640318145248, 0.004636424460477216354, 0.006181899280636287027, 0.007727374100795358566, 0.008500111510874876555, 0.009272848920954396279, 0.01081832374111341144, 0.01236379856127242487, 0.01390927338143144003, 0.01545474820159045866, 0.01700022302174947209, 0.01854569784190848725, 0.02009117266206750588, 0.02163664748222652104, 0.02318212230238553967, 0.02472759712254455136 ),
 .UNSPECIFIED. ) ;
#29670 = ORIENTED_EDGE ( 'NONE', *, *, #11924, .T. ) ;
#29671 = CARTESIAN_POINT ( 'NONE',  ( 188.5076656590985635, 87.95171816312542035, 91.58452734307059018 ) ) ;
#29672 = CARTESIAN_POINT ( 'NONE',  ( -14.19493007850031852, 7.389842975086046373, 6.803802910258403891 ) ) ;
#29673 = LINE ( 'NONE', #13501, #5334 ) ;
#29674 = CARTESIAN_POINT ( 'NONE',  ( -26.49516976694649628, 8.831756547364854271, -64.00066573786835988 ) ) ;
#29675 = UNCERTAINTY_MEASURE_WITH_UNIT (LENGTH_MEASURE( 1.000000000000000082E-05 ), #49218, 'distance_accuracy_value', 'NONE');
#29676 = CARTESIAN_POINT ( 'NONE',  ( 14.80205238535216772, 6.470775952815778886, 3.219160964839414607 ) ) ;
#29677 = ORIENTED_EDGE ( 'NONE', *, *, #21428, .F. ) ;
#29678 = DIRECTION ( 'NONE',  ( -0.8160245890732938934, -0.5780171883497599028, 0.000000000000000000 ) ) ;
#29679 = DIRECTION ( 'NONE',  ( -1.000000000000000000, 0.000000000000000000, -1.337618101958020291E-16 ) ) ;
#29680 = CARTESIAN_POINT ( 'NONE',  ( 178.4027079424739100, 75.93756746109792743, -63.56196981810690971 ) ) ;
#29681 = DIRECTION ( 'NONE',  ( -1.205632815803654626E-16, 1.000000000000000000, 8.673486594973769070E-19 ) ) ;
#29682 = CARTESIAN_POINT ( 'NONE',  ( 275.6635180218175947, -21.85802590693743852, 2.510273771313272562 ) ) ;
#29683 = CARTESIAN_POINT ( 'NONE',  ( 107.2672065034543039, 27.52931006625852817, 3.378187332071801663 ) ) ;
#29684 = CARTESIAN_POINT ( 'NONE',  ( 417.3372781065086770, 0.000000000000000000, 108.5502958579881749 ) ) ;
#29685 = CARTESIAN_POINT ( 'NONE',  ( -19.44450032618849633, -27.18813209818722498, 6.893343212288935540 ) ) ;
#29686 = CARTESIAN_POINT ( 'NONE',  ( -48.33725449172840172, 12.98311179783358860, 61.28596623952740430 ) ) ;
#29687 = ADVANCED_FACE ( 'NONE', ( #7717 ), #61521, .F. ) ;
#29688 = CIRCLE ( 'NONE', #38673, 5.000000000000000888 ) ;
#29689 = CARTESIAN_POINT ( 'NONE',  ( -4.955782654901478068, 6.720825733572401539, 57.51796347446001789 ) ) ;
#29690 = EDGE_LOOP ( 'NONE', ( #7831, #20092, #27375, #25900 ) ) ;
#29692 = CARTESIAN_POINT ( 'NONE',  ( 70.21761529798025947, 26.35311180610075610, 43.58025477438756212 ) ) ;
#29691 = VECTOR ( 'NONE', #19287, 1000.000000000000000 ) ;
#29693 = LINE ( 'NONE', #35674, #53175 ) ;
#29694 = DIRECTION ( 'NONE',  ( 1.000000000000000000, 0.000000000000000000, 0.000000000000000000 ) ) ;
#29695 = FACE_OUTER_BOUND ( 'NONE', #51167, .T. ) ;
#29696 = PLANE ( 'NONE',  #45715 ) ;
#29697 = CIRCLE ( 'NONE', #61184, 5.000000000000004441 ) ;
#29698 = EDGE_LOOP ( 'NONE', ( #3133, #43919, #26498, #8269 ) ) ;
#29699 = AXIS2_PLACEMENT_3D ( 'NONE', #29932, #1822, #56312 ) ;
#29701 = EDGE_CURVE ( 'NONE', #28566, #3016, #39718, .T. ) ;
#29700 = DIRECTION ( 'NONE',  ( 0.000000000000000000, 0.000000000000000000, 1.000000000000000000 ) ) ;
#29702 = VECTOR ( 'NONE', #5038, 1000.000000000000000 ) ;
#29703 = DIRECTION ( 'NONE',  ( -0.000000000000000000, -0.000000000000000000, -1.000000000000000000 ) ) ;
#29704 = ORIENTED_EDGE ( 'NONE', *, *, #52039, .F. ) ;
#29705 = ORIENTED_EDGE ( 'NONE', *, *, #58762, .T. ) ;
#29706 = DIRECTION ( 'NONE',  ( 0.000000000000000000, 0.000000000000000000, 1.000000000000000000 ) ) ;
#29707 = CARTESIAN_POINT ( 'NONE',  ( -174.7869898116916261, 88.99756909636809610, -61.69509254903428541 ) ) ;
#29708 = ADVANCED_FACE ( 'NONE', ( #2432 ), #50614, .T. ) ;
#29709 = DIRECTION ( 'NONE',  ( -0.000000000000000000, -0.000000000000000000, 1.000000000000000000 ) ) ;
#29710 = ORIENTED_EDGE ( 'NONE', *, *, #48395, .F. ) ;
#29711 = DIRECTION ( 'NONE',  ( -1.000000000000000000, 0.000000000000000000, 0.000000000000000000 ) ) ;
#29712 = EDGE_CURVE ( 'NONE', #61832, #17233, #19642, .T. ) ;
#29713 = CARTESIAN_POINT ( 'NONE',  ( -180.3153482337535536, 95.51031295027648582, 13.61842630024514378 ) ) ;
#29714 = CARTESIAN_POINT ( 'NONE',  ( -1.876547441458563670, 6.576559737910136150, 6.196969845067472171 ) ) ;
#29715 = CARTESIAN_POINT ( 'NONE',  ( 58.08938767906773393, 12.61185010801510487, -37.54421099187102584 ) ) ;
#29716 = DIRECTION ( 'NONE',  ( 0.000000000000000000, 1.000000000000000000, 0.000000000000000000 ) ) ;
#29717 = CARTESIAN_POINT ( 'NONE',  ( 150.0047159235711831, 52.07197026280400820, 91.64991005666685453 ) ) ;
#29718 = CARTESIAN_POINT ( 'NONE',  ( 136.3292018078239778, 42.93753790426544015, 3.081257596490504458 ) ) ;
#29719 = ORIENTED_EDGE ( 'NONE', *, *, #43268, .T. ) ;
#29720 = CARTESIAN_POINT ( 'NONE',  ( -2.967675169455163520, 38.21895468312379052, 13.32819299319723783 ) ) ;
#29721 = CARTESIAN_POINT ( 'NONE',  ( -73.63128929564830116, 21.53548093502885052, 16.63761306745141866 ) ) ;
#29722 = CARTESIAN_POINT ( 'NONE',  ( 45.02738683369923223, 9.207938468499236251, -48.08623862790063441 ) ) ;
#29723 = DIRECTION ( 'NONE',  ( 1.000000000000000000, 0.000000000000000000, 0.000000000000000000 ) ) ;
#29725 = VERTEX_POINT ( 'NONE', #23889 ) ;
#29724 = FACE_OUTER_BOUND ( 'NONE', #15606, .T. ) ;
#29726 = CARTESIAN_POINT ( 'NONE',  ( 79.53408731553405175, 17.12082763744058767, -40.84044364051945308 ) ) ;
#29727 = EDGE_CURVE ( 'NONE', #35721, #37319, #41105, .T. ) ;
#29728 = ORIENTED_EDGE ( 'NONE', *, *, #46598, .T. ) ;
#29729 = CARTESIAN_POINT ( 'NONE',  ( 0.000000000000000000, 0.000000000000000000, -2.000000000000000000 ) ) ;
#29730 = CARTESIAN_POINT ( 'NONE',  ( -13.24252603915608617, 63.63674649211943546, 170.0000000000000000 ) ) ;
#29731 = DIRECTION ( 'NONE',  ( -0.08963930890344087854, 0.9959742939952382912, 0.000000000000000000 ) ) ;
#29732 = ADVANCED_FACE ( 'NONE', ( #14376 ), #8406, .T. ) ;
#29733 = CARTESIAN_POINT ( 'NONE',  ( 187.2465631085773907, 85.06582225041684353, -12.57587812946169770 ) ) ;
#29734 = CARTESIAN_POINT ( 'NONE',  ( 140.0614732283738704, 45.29930344725075742, -20.89927350591657529 ) ) ;
#29735 = CARTESIAN_POINT ( 'NONE',  ( -86.10360257264198935, 26.38663017581291115, -14.76872716454347767 ) ) ;
#29736 = CARTESIAN_POINT ( 'NONE',  ( -179.8926034784145713, 96.58272071140100934, -18.60358020078452768 ) ) ;
#29737 = AXIS2_PLACEMENT_3D ( 'NONE', #41151, #3177, #62612 ) ;
#29738 = CARTESIAN_POINT ( 'NONE',  ( -47.56466076048270963, 13.83435953640666938, 37.32649237162055300 ) ) ;
#29739 = VERTEX_POINT ( 'NONE', #35831 ) ;
#29740 = EDGE_LOOP ( 'NONE', ( #28574, #25275, #54654, #12740 ) ) ;
#29741 = DIRECTION ( 'NONE',  ( 0.000000000000000000, 0.000000000000000000, 1.000000000000000000 ) ) ;
#29742 = CARTESIAN_POINT ( 'NONE',  ( -31.43908319763709969, 9.591432048623765638, 30.21645440618916112 ) ) ;
#29743 = CARTESIAN_POINT ( 'NONE',  ( 163.2886151008987383, 62.32020850087168640, 59.01466171590617193 ) ) ;
#29744 = CARTESIAN_POINT ( 'NONE',  ( -189.2352924136013712, 107.0839554967701304, 64.82041842450834679 ) ) ;
#29745 = AXIS2_PLACEMENT_3D ( 'NONE', #69110, #43760, #42392 ) ;
#29746 = DIRECTION ( 'NONE',  ( 1.000000000000000000, 0.000000000000000000, 0.000000000000000000 ) ) ;
#29747 = DIRECTION ( 'NONE',  ( -0.5000000000000014433, 0.8660254037844378194, 0.000000000000000000 ) ) ;
#29748 = CIRCLE ( 'NONE', #17386, 243.4957430088094839 ) ;
#29749 = CARTESIAN_POINT ( 'NONE',  ( 163.7607557204680404, 62.71181783708026813, -66.35314833076057539 ) ) ;
#29750 = VERTEX_POINT ( 'NONE', #13674 ) ;
#29751 = VERTEX_POINT ( 'NONE', #67169 ) ;
#29752 = CIRCLE ( 'NONE', #8422, 66.50000000000000000 ) ;
#29753 = VERTEX_POINT ( 'NONE', #51322 ) ;
#29754 = LINE ( 'NONE', #69368, #64486 ) ;
#29755 = CIRCLE ( 'NONE', #8424, 125.0000000000000000 ) ;
#29756 = CARTESIAN_POINT ( 'NONE',  ( 6.400000000000000355, 0.000000000000000000, -5.400000000000001243 ) ) ;
#29757 = CARTESIAN_POINT ( 'NONE',  ( -85.46258339457290276, 25.02772366257408976, 61.58065315855991173 ) ) ;
#29758 = CARTESIAN_POINT ( 'NONE',  ( 66.72974708835174340, 13.56459745268606376, -49.75501017375558632 ) ) ;
#29759 = DIRECTION ( 'NONE',  ( -4.270088556250601699E-16, -0.000000000000000000, -1.000000000000000000 ) ) ;
#29760 = CARTESIAN_POINT ( 'NONE',  ( -55.05276343752909440, 15.72344139423348430, 45.31732777293115788 ) ) ;
#29761 = CARTESIAN_POINT ( 'NONE',  ( -98.68609963468200874, 32.11186931716881787, -9.070045062816474157 ) ) ;
#29762 = CARTESIAN_POINT ( 'NONE',  ( 57.41085175769453741, 12.46982565415947164, 32.32325660257177447 ) ) ;
#29763 = CARTESIAN_POINT ( 'NONE',  ( 39.74012880617502930, 8.453553184817396371, 83.60337793500843873 ) ) ;
#29764 = ORIENTED_EDGE ( 'NONE', *, *, #60020, .F. ) ;
#29765 = CARTESIAN_POINT ( 'NONE',  ( -0.5780275525703858497, 6.527356703336898214, -44.86394364185162686 ) ) ;
#29766 = PLANE ( 'NONE',  #44177 ) ;
#29767 = CARTESIAN_POINT ( 'NONE',  ( -868.3301948030079984, -622.0000000000060254, 10.00000000000000000 ) ) ;
#29768 = DIRECTION ( 'NONE',  ( 2.775557561562891844E-16, -0.000000000000000000, 1.000000000000000000 ) ) ;
#29769 = CARTESIAN_POINT ( 'NONE',  ( -16.68907004672388084, 73.11959341363670717, 0.000000000000000000 ) ) ;
#29771 = EDGE_CURVE ( 'NONE', #41500, #30587, #3135, .T. ) ;
#29770 = CARTESIAN_POINT ( 'NONE',  ( 17.48988570800758779, 7.568061572928498570, -8.865890789862755028 ) ) ;
#29772 = CARTESIAN_POINT ( 'NONE',  ( 199.3743599161303166, 99.31857334527875025, 68.86014906300715666 ) ) ;
#29773 = EDGE_CURVE ( 'NONE', #33133, #29802, #67495, .T. ) ;
#29774 = B_SPLINE_CURVE_WITH_KNOTS ( 'NONE', 3,
 ( #29317, #55342, #28625, #45139, #35290, #60974, #56391, #18766, #8211, #66283, #18415, #19102, #40556, #51473, #28982, #44445, #29662, #18075, #51122, #2935, #24399, #45841, #50429, #22999, #34615, #65934, #17729, #34257, #39186, #39525, #7170, #23361, #12800, #56050, #9941, #35643, #26112, #20479, #41944, #63408, #15211, #57435, #31394, #36674, #31056, #37015 ),
 .UNSPECIFIED., .F., .F.,
 ( 4, 2, 2, 2, 2, 2, 2, 2, 2, 2, 2, 2, 2, 2, 2, 2, 2, 2, 2, 2, 2, 2, 4 ),
 ( 1.387778780781445676E-17, 0.003635178948345801821, 0.005452768422518668688, 0.007270357896691534254, 0.008179152633777973108, 0.009087947370864411095, 0.01090553684503733217, 0.01181433158212380832, 0.01272312631921028447, 0.01363192105629676062, 0.01454071579338323504, 0.01544951053046971119, 0.01635830526755618908, 0.01726710000464266176, 0.01817589474172913791, 0.01908468947881561406, 0.01999348421590209021, 0.02090227895298856636, 0.02181107369007504251, 0.02362866316424793930, 0.02544625263842083263, 0.02726384211259372595, 0.02908143158676661927 ),
 .UNSPECIFIED. ) ;
#29775 = ORIENTED_EDGE ( 'NONE', *, *, #68602, .F. ) ;
#29776 = CARTESIAN_POINT ( 'NONE',  ( -125.8938041572051105, 46.49392987655492959, 57.46449846362076386 ) ) ;
#29777 = DIRECTION ( 'NONE',  ( 0.000000000000000000, 0.000000000000000000, -1.000000000000000000 ) ) ;
#29778 = DIRECTION ( 'NONE',  ( -1.000000000000000000, -1.001918046209079887E-14, 9.729495617646301779E-15 ) ) ;
#29779 = ITEM_DEFINED_TRANSFORMATION ( 'NONE', 'NONE', #59099,  #66832 ) ;
#29780 = CARTESIAN_POINT ( 'NONE',  ( -165.6837635325849760, 79.21404047536307758, 91.02581465340531963 ) ) ;
#29781 = ORIENTED_EDGE ( 'NONE', *, *, #66157, .T. ) ;
#29782 = CARTESIAN_POINT ( 'NONE',  ( 126.4219470349615904, 38.26519385429184439, 11.18839248169725131 ) ) ;
#29783 = VERTEX_POINT ( 'NONE', #26311 ) ;
#29785 = EDGE_CURVE ( 'NONE', #43079, #61401, #31578, .T. ) ;
#29784 = FACE_BOUND ( 'NONE', #3069, .T. ) ;
#29786 = CARTESIAN_POINT ( 'NONE',  ( 0.000000000000000000, 0.000000000000000000, 170.0000000000000000 ) ) ;
#29787 = ORIENTED_EDGE ( 'NONE', *, *, #64005, .F. ) ;
#29788 = VECTOR ( 'NONE', #34169, 1000.000000000000000 ) ;
#29789 = EDGE_CURVE ( 'NONE', #51247, #17838, #52345, .T. ) ;
#29790 = CARTESIAN_POINT ( 'NONE',  ( 163.0539896041220800, 63.43291176144029464, 85.57986349963141492 ) ) ;
#29791 = VERTEX_POINT ( 'NONE', #37194 ) ;
#29792 = CARTESIAN_POINT ( 'NONE',  ( -58.76099769480632062, 16.75353773354894571, 17.49641683403302039 ) ) ;
#29793 = FACE_OUTER_BOUND ( 'NONE', #6145, .T. ) ;
#29794 = EDGE_CURVE ( 'NONE', #62258, #3570, #20677, .T. ) ;
#29795 = AXIS2_PLACEMENT_3D ( 'NONE', #55510, #20221, #14599 ) ;
#29796 = CARTESIAN_POINT ( 'NONE',  ( -155.2836587093739524, 70.59655508952972980, 33.43029846410576766 ) ) ;
#29797 = DIRECTION ( 'NONE',  ( 0.000000000000000000, 0.000000000000000000, 1.000000000000000000 ) ) ;
#29798 = VECTOR ( 'NONE', #23458, 1000.000000000000000 ) ;
#29800 = CARTESIAN_POINT ( 'NONE',  ( -34.96012151086435438, -55.23134702900938464, 43.58025477438756212 ) ) ;
#29799 = CIRCLE ( 'NONE', #64643, 2.999999999999999112 ) ;
#29802 = VERTEX_POINT ( 'NONE', #26649 ) ;
#29801 = CARTESIAN_POINT ( 'NONE',  ( 72.99999999999998579, 8.939921633775675282E-15, 25.70156211871649887 ) ) ;
#29803 =( GEOMETRIC_REPRESENTATION_CONTEXT ( 3 ) GLOBAL_UNCERTAINTY_ASSIGNED_CONTEXT ( ( #35303 ) ) GLOBAL_UNIT_ASSIGNED_CONTEXT ( ( #55012, #39545, #50099 ) ) REPRESENTATION_CONTEXT ( 'NONE', 'WORKASPACE' ) );
#29804 = CARTESIAN_POINT ( 'NONE',  ( 58.48209831743719178, 11.66636741727081805, 43.30750159671042354 ) ) ;
#29805 = VECTOR ( 'NONE', #21649, 1000.000000000000000 ) ;
#29806 = ORIENTED_EDGE ( 'NONE', *, *, #40488, .T. ) ;
#29807 = ORIENTED_EDGE ( 'NONE', *, *, #59061, .F. ) ;
#29808 = CARTESIAN_POINT ( 'NONE',  ( 177.7886308167536527, 76.74396398590874924, 43.56092108689954046 ) ) ;
#29809 = CIRCLE ( 'NONE', #69098, 246.3582898394607241 ) ;
#29810 = CARTESIAN_POINT ( 'NONE',  ( 23.09541709302173018, 6.844586979481588784, -71.57097287790641360 ) ) ;
#29812 = ORIENTED_EDGE ( 'NONE', *, *, #64229, .T. ) ;
#29811 = CARTESIAN_POINT ( 'NONE',  ( -129.4036885357274116, 50.06837984316183565, 71.59659508659780158 ) ) ;
#29813 = CARTESIAN_POINT ( 'NONE',  ( -97.58423681613963652, 31.57579159344722086, 85.85188415635715842 ) ) ;
#29814 = CARTESIAN_POINT ( 'NONE',  ( -71.97658551692140350, 20.95070248419150971, -46.01531844971390228 ) ) ;
#29815 = ORIENTED_EDGE ( 'NONE', *, *, #29937, .F. ) ;
#29816 = CARTESIAN_POINT ( 'NONE',  ( 210.0055645826033413, 115.7254585628714381, -75.99226608288455509 ) ) ;
#29817 = CARTESIAN_POINT ( 'NONE',  ( 141.9165763529819344, -2.000000000000001776, 129.0000000000000000 ) ) ;
#29818 = CARTESIAN_POINT ( 'NONE',  ( 113.4418023215250457, 31.50656691678295473, 30.31107852835060612 ) ) ;
#29819 = DIRECTION ( 'NONE',  ( 1.000000000000000000, 0.000000000000000000, 0.000000000000000000 ) ) ;
#29820 = CARTESIAN_POINT ( 'NONE',  ( 39.40195752203892710, 8.409560354027400209, 56.75838489642694640 ) ) ;
#29821 = ORIENTED_EDGE ( 'NONE', *, *, #19628, .F. ) ;
#29822 = ORIENTED_EDGE ( 'NONE', *, *, #53901, .T. ) ;
#29823 = DIRECTION ( 'NONE',  ( -0.000000000000000000, -0.000000000000000000, -1.000000000000000000 ) ) ;
#29824 = DIRECTION ( 'NONE',  ( 1.000000000000000000, 0.000000000000000000, 0.000000000000000000 ) ) ;
#29825 = DIRECTION ( 'NONE',  ( 0.000000000000000000, 0.000000000000000000, -1.000000000000000000 ) ) ;
#29826 = DIRECTION ( 'NONE',  ( 0.000000000000000000, 1.000000000000000000, -0.000000000000000000 ) ) ;
#29827 = DIRECTION ( 'NONE',  ( 0.9959742939952382912, 0.08963930890344087854, 0.000000000000000000 ) ) ;
#29828 = CARTESIAN_POINT ( 'NONE',  ( -4.999999999999922728, 46.66904755831208718, 85.00100000000000477 ) ) ;
#29829 = CARTESIAN_POINT ( 'NONE',  ( -172.7116702014380110, 86.67317892691259829, -61.55650775521370122 ) ) ;
#29830 = EDGE_LOOP ( 'NONE', ( #7952, #39695, #5424, #67549 ) ) ;
#29831 = CARTESIAN_POINT ( 'NONE',  ( -109.7079446832838983, 37.86719386855315861, 36.94873819821719252 ) ) ;
#29832 = VERTEX_POINT ( 'NONE', #68524 ) ;
#29833 = VECTOR ( 'NONE', #55778, 1000.000000000000000 ) ;
#29834 = CARTESIAN_POINT ( 'NONE',  ( -38.93878980550034186, 10.94326053663841947, 11.36906375664720947 ) ) ;
#29835 = CARTESIAN_POINT ( 'NONE',  ( 82.34401416830216647, 19.05992892018825557, 57.89662370918314593 ) ) ;
#29836 = ORIENTED_EDGE ( 'NONE', *, *, #56025, .F. ) ;
#29837 = CARTESIAN_POINT ( 'NONE',  ( 56.56044447577782108, 35.24940721789563725, 34.48241823993598132 ) ) ;
#29838 = CARTESIAN_POINT ( 'NONE',  ( -189.2442476610617632, 107.0963225822736291, -68.52046992184840235 ) ) ;
#29839 = DIRECTION ( 'NONE',  ( -1.001915251000354105E-14, 1.000000000000000000, -5.551115123125782702E-17 ) ) ;
#29841 = FACE_OUTER_BOUND ( 'NONE', #1329, .T. ) ;
#29840 = AXIS2_PLACEMENT_3D ( 'NONE', #22124, #55172, #49536 ) ;
#29842 = CARTESIAN_POINT ( 'NONE',  ( 33.44983424733137412, 7.709709042132403489, 15.15903636718023328 ) ) ;
#29843 = CARTESIAN_POINT ( 'NONE',  ( -14.93280618462406828, 8.469244267267916015, -40.51070958269902889 ) ) ;
#29844 = CARTESIAN_POINT ( 'NONE',  ( 259.4165763529819060, -27.00000000000000355, 108.9999999999999858 ) ) ;
#29845 = EDGE_CURVE ( 'NONE', #55324, #14098, #42132, .T. ) ;
#29846 = VECTOR ( 'NONE', #12128, 1000.000000000000000 ) ;
#29847 = VECTOR ( 'NONE', #36271, 1000.000000000000000 ) ;
#29848 = ORIENTED_EDGE ( 'NONE', *, *, #68784, .T. ) ;
#29849 = PLANE ( 'NONE',  #54423 ) ;
#29850 = ORIENTED_EDGE ( 'NONE', *, *, #1415, .F. ) ;
#29851 = CARTESIAN_POINT ( 'NONE',  ( -20.93485882276935328, -13.66498028065569059, 0.000000000000000000 ) ) ;
#29852 = CARTESIAN_POINT ( 'NONE',  ( -61.76386578474848932, 17.63453064612501109, 61.27715783582140574 ) ) ;
#29853 = FACE_OUTER_BOUND ( 'NONE', #6252, .T. ) ;
#29854 = EDGE_LOOP ( 'NONE', ( #22758, #32519, #20518, #57717 ) ) ;
#29855 = DIRECTION ( 'NONE',  ( -1.000000000000000000, 0.000000000000000000, 0.000000000000000000 ) ) ;
#29856 = AXIS2_PLACEMENT_3D ( 'NONE', #43019, #42006, #11022 ) ;
#29858 = EDGE_CURVE ( 'NONE', #44762, #33459, #53014, .T. ) ;
#29857 = CARTESIAN_POINT ( 'NONE',  ( 153.2208437558771550, 55.67531116261156399, -64.27115891943437020 ) ) ;
#29859 = CARTESIAN_POINT ( 'NONE',  ( -38.69408084385329971, 10.89529537250243152, 39.68205672784471005 ) ) ;
#29860 = CARTESIAN_POINT ( 'NONE',  ( 133.8566784816069628, 41.42467568809806977, -36.02331093239566684 ) ) ;
#29861 = AXIS2_PLACEMENT_3D ( 'NONE', #49892, #55165, #16832 ) ;
#29862 = EDGE_CURVE ( 'NONE', #28258, #30681, #4185, .T. ) ;
#29863 = EDGE_LOOP ( 'NONE', ( #46653, #49005, #33163, #63362, #10415, #66809, #56620, #27144 ) ) ;
#29864 = EDGE_CURVE ( 'NONE', #32511, #39395, #7560, .T. ) ;
#29865 = DIRECTION ( 'NONE',  ( 0.1142836089109254549, -0.2522235278763978461, 0.9608967419654821374 ) ) ;
#29866 = CARTESIAN_POINT ( 'NONE',  ( -72.57286576968782299, -18.73210786364450442, 41.38025477438755928 ) ) ;
#29867 = CARTESIAN_POINT ( 'NONE',  ( -123.4416615615272832, 44.90042688650404301, 45.21152833363236567 ) ) ;
#29868 = CARTESIAN_POINT ( 'NONE',  ( -62.45176220516621868, 16.79101814080731714, -41.46409900258914405 ) ) ;
#29869 = ORIENTED_EDGE ( 'NONE', *, *, #9935, .T. ) ;
#29870 = LINE ( 'NONE', #2791, #50374 ) ;
#29871 = B_SPLINE_CURVE_WITH_KNOTS ( 'NONE', 3,
 ( #42016, #5751, #4722, #64856, #31807, #36747, #43034, #21934, #42361, #37082, #16658, #32158, #63475, #64508, #15290, #32840, #48297, #47282, #26873, #130, #58192, #64156, #58524, #21585, #15970, #58870, #16315, #26186, #69073, #37418, #69433, #5419, #10013, #31465, #10342, #52901, #21250, #486, #11034, #47622, #27208, #37771, #63821, #53240, #26533, #47968, #54275 ),
 .UNSPECIFIED., .F., .F.,
 ( 4, 2, 2, 2, 2, 2, 2, 2, 2, 2, 2, 1, 2, 2, 2, 2, 2, 2, 2, 2, 2, 2, 2, 4 ),
 ( 0.000000000000000000, 0.003297771944418878293, 0.004122214930523569569, 0.004946657916628260411, 0.006595543888837659442, 0.007419986874942373703, 0.008244429861047088831, 0.009068872847151803959, 0.009893315833256519087, 0.01154220180546601179, 0.01236664479157075641, 0.01319108777767550277, 0.01401553076378025085, 0.01483997374988499547, 0.01566441673598974182, 0.01648885972209448644, 0.01813774569430391323, 0.01896218868040866826, 0.01978663166651342328, 0.02061107465261817831, 0.02143551763872292987, 0.02308440361093241910, 0.02473328958314190834, 0.02638217555535140105 ),
 .UNSPECIFIED. ) ;
#29872 = CARTESIAN_POINT ( 'NONE',  ( 89.21005684773501798, 20.31770592753386850, 57.01058117278675041 ) ) ;
#29873 = DIRECTION ( 'NONE',  ( -1.387778780781446169E-16, 1.000000000000000000, 3.469446951953615421E-17 ) ) ;
#29874 = PRESENTATION_STYLE_ASSIGNMENT (( #14396 ) ) ;
#29875 = EDGE_CURVE ( 'NONE', #35686, #66579, #34480, .T. ) ;
#29876 = B_SPLINE_CURVE_WITH_KNOTS ( 'NONE', 3,
 ( #64211, #56436, #65980, #51173, #34994, #7914, #61715, #45193, #33956, #55389, #50476, #8259, #8614, #29364, #2990, #30068, #29713, #51521, #23746, #24449, #7218, #13872, #45890, #44499, #34663, #28674, #66332, #61373, #39575, #39917, #19151, #13539, #39233, #24099, #12494, #50129, #40266, #23052, #7581, #67360, #50818, #1956, #40605, #18469, #62057, #17775 ),
 .UNSPECIFIED., .F., .F.,
 ( 4, 2, 2, 2, 2, 2, 2, 2, 2, 2, 2, 2, 2, 2, 2, 2, 2, 2, 2, 2, 2, 2, 4 ),
 ( 0.000000000000000000, 0.003736383952885362434, 0.005604575929328028255, 0.007472767905770694510, 0.008406863893992026771, 0.009340959882213357296, 0.01120915185865602355, 0.01214324784687736622, 0.01307734383509870889, 0.01401143982332004982, 0.01494553581154139249, 0.01587963179976273342, 0.01681372778798407436, 0.01774782377620541529, 0.01868191976442675623, 0.01961601575264810063, 0.02055011174086944156, 0.02148420772909078943, 0.02241830371731213037, 0.02428649569375483999, 0.02615468767019754615, 0.02802287964664025230, 0.02989107162308296539 ),
 .UNSPECIFIED. ) ;
#29877 = LINE ( 'NONE', #67185, #51488 ) ;
#29878 = ORIENTED_EDGE ( 'NONE', *, *, #39464, .F. ) ;
#29879 = CARTESIAN_POINT ( 'NONE',  ( 203.9181091394787018, 105.2759068139670973, 44.20772073876945285 ) ) ;
#29880 = CARTESIAN_POINT ( 'NONE',  ( -6.123233995736762338E-16, 0.000000000000000000, -20.00000000000000000 ) ) ;
#29881 = CARTESIAN_POINT ( 'NONE',  ( 66.73594759725092729, 13.56641407806657540, 70.67429847145855604 ) ) ;
#29882 = CARTESIAN_POINT ( 'NONE',  ( 188.0300953578913266, 85.92260131067908446, -94.54474959917212118 ) ) ;
#29883 = PLANE ( 'NONE',  #19564 ) ;
#29884 = ORIENTED_EDGE ( 'NONE', *, *, #66713, .T. ) ;
#29885 = CARTESIAN_POINT ( 'NONE',  ( 164.8908506817023465, 64.97619709085121542, -15.65508747974032566 ) ) ;
#29886 = ORIENTED_EDGE ( 'NONE', *, *, #473, .T. ) ;
#29887 = CIRCLE ( 'NONE', #68112, 0.3000000000000051514 ) ;
#29888 = CARTESIAN_POINT ( 'NONE',  ( 70.46579300139245561, 15.56614468937219264, 65.15598333419700339 ) ) ;
#29889 = CARTESIAN_POINT ( 'NONE',  ( 126.5017642286235287, 37.15732438686229244, 89.18760059589644129 ) ) ;
#29890 = VECTOR ( 'NONE', #40050, 1000.000000000000000 ) ;
#29891 = VERTEX_POINT ( 'NONE', #36863 ) ;
#29892 = CARTESIAN_POINT ( 'NONE',  ( -143.3925773749112125, 59.16144459815139811, -64.80734044691615736 ) ) ;
#29893 = DIRECTION ( 'NONE',  ( 0.000000000000000000, 0.000000000000000000, 1.000000000000000000 ) ) ;
#29894 = DIRECTION ( 'NONE',  ( -0.5323601107705935309, 0.8465179929926602842, 0.000000000000000000 ) ) ;
#29895 = VECTOR ( 'NONE', #61702, 1000.000000000000000 ) ;
#29896 = VECTOR ( 'NONE', #6432, 1000.000000000000000 ) ;
#29897 = EDGE_LOOP ( 'NONE', ( #48694, #13318, #35426, #1171 ) ) ;
#29898 = AXIS2_PLACEMENT_3D ( 'NONE', #2360, #40669, #55109 ) ;
#29899 = DIRECTION ( 'NONE',  ( 1.000000000000000000, 0.000000000000000000, -0.000000000000000000 ) ) ;
#29900 = VECTOR ( 'NONE', #38366, 1000.000000000000000 ) ;
#29901 = CARTESIAN_POINT ( 'NONE',  ( -30.00000000000000355, 29.99999999999999645, 0.000000000000000000 ) ) ;
#29902 = CARTESIAN_POINT ( 'NONE',  ( 152.9696068220085863, 55.48791888908662884, -91.30131104750859095 ) ) ;
#29903 = VECTOR ( 'NONE', #34535, 1000.000000000000000 ) ;
#29904 = DIRECTION ( 'NONE',  ( -0.000000000000000000, -1.000000000000000000, -0.000000000000000000 ) ) ;
#29905 = CARTESIAN_POINT ( 'NONE',  ( 442.3372781065085633, 369.9999999999999432, -141.4497041420118251 ) ) ;
#29906 = CARTESIAN_POINT ( 'NONE',  ( 0.000000000000000000, 0.000000000000000000, 12.00000000000000000 ) ) ;
#29907 = CARTESIAN_POINT ( 'NONE',  ( 88.98064924903390249, 21.30386569031176336, 44.33800583418702246 ) ) ;
#29908 = ORIENTED_EDGE ( 'NONE', *, *, #25019, .T. ) ;
#29909 = CARTESIAN_POINT ( 'NONE',  ( -94.77890319529970498, 30.24118571794802435, 64.36354809645237651 ) ) ;
#29910 = CARTESIAN_POINT ( 'NONE',  ( -14.56631729561072852, 8.434645566888203660, 67.78470214004869376 ) ) ;
#29911 = ORIENTED_EDGE ( 'NONE', *, *, #47466, .F. ) ;
#29912 = CARTESIAN_POINT ( 'NONE',  ( 151.1700480242206197, 54.15904440870133385, -12.70232037378493573 ) ) ;
#29913 = CARTESIAN_POINT ( 'NONE',  ( -22.50000000000003197, -18.06806526123148160, 0.000000000000000000 ) ) ;
#29914 = CARTESIAN_POINT ( 'NONE',  ( -38.17232309348611352, 11.81874355808867882, 41.05688953177845235 ) ) ;
#29915 = ADVANCED_FACE ( 'NONE', ( #47741 ), #69204, .T. ) ;
#29916 = CARTESIAN_POINT ( 'NONE',  ( -154.0775378574013814, 68.15437918458555089, -63.19143630128887423 ) ) ;
#29917 = CARTESIAN_POINT ( 'NONE',  ( 56.67004931728209982, 11.28989923258780159, 94.99999999999866418 ) ) ;
#29918 = CARTESIAN_POINT ( 'NONE',  ( -51.99406906667275052, 13.88268392809765395, -62.70866649372558754 ) ) ;
#29919 = CARTESIAN_POINT ( 'NONE',  ( -4.072522659361689890, 7.683023425615370883, -22.57170394412693071 ) ) ;
#29920 = CARTESIAN_POINT ( 'NONE',  ( 174.6127059037623042, 72.30368563770915102, 6.133683309753402035 ) ) ;
#29921 = CYLINDRICAL_SURFACE ( 'NONE', #66922, 10.00000000000000000 ) ;
#29922 = ORIENTED_EDGE ( 'NONE', *, *, #48649, .F. ) ;
#29923 = FACE_OUTER_BOUND ( 'NONE', #11375, .T. ) ;
#29924 = EDGE_LOOP ( 'NONE', ( #22833, #19061, #9550, #56172 ) ) ;
#29925 = CARTESIAN_POINT ( 'NONE',  ( 105.8203563788590742, 26.88901185006199057, -64.20487891140942338 ) ) ;
#29926 = DIRECTION ( 'NONE',  ( -0.000000000000000000, -1.000000000000000000, -0.000000000000000000 ) ) ;
#29927 = CARTESIAN_POINT ( 'NONE',  ( -36.53690438256410289, 73.43472186181504924, 133.5802547743875550 ) ) ;
#29928 = DIRECTION ( 'NONE',  ( 1.000000000000000000, 0.000000000000000000, 0.000000000000000000 ) ) ;
#29929 = CARTESIAN_POINT ( 'NONE',  ( -11.84613025833866473, 7.186187877555967773, 84.96521102128788527 ) ) ;
#29930 = CARTESIAN_POINT ( 'NONE',  ( -107.7677210873466009, 36.80113675102408166, -20.80525371622632846 ) ) ;
#29931 = ORIENTED_EDGE ( 'NONE', *, *, #24301, .F. ) ;
#29932 = CARTESIAN_POINT ( 'NONE',  ( 149.4165763529819344, -26.99999999999998224, 138.9999999999999716 ) ) ;
#29933 = CARTESIAN_POINT ( 'NONE',  ( -167.1534554062404538, 80.72263015867915215, 69.71615865952209390 ) ) ;
#29934 = ORIENTED_EDGE ( 'NONE', *, *, #47858, .F. ) ;
#29935 = ORIENTED_EDGE ( 'NONE', *, *, #19128, .T. ) ;
#29937 = EDGE_CURVE ( 'NONE', #18071, #62698, #13128, .T. ) ;
#29936 = CARTESIAN_POINT ( 'NONE',  ( 123.4242852856285566, 0.000000000000000000, -30.00000000000000000 ) ) ;
#29938 = CARTESIAN_POINT ( 'NONE',  ( -180.5668408223793904, 95.81768001203278118, -95.00000000000133582 ) ) ;
#29939 = CARTESIAN_POINT ( 'NONE',  ( 173.6012773665503914, 71.36035397668605640, -17.46879726638741559 ) ) ;
#29940 = AXIS2_PLACEMENT_3D ( 'NONE', #8731, #13313, #3441 ) ;
#29941 = CARTESIAN_POINT ( 'NONE',  ( 103.8325688302027459, 27.12251147381400784, 60.05448002011801378 ) ) ;
#29942 = DIRECTION ( 'NONE',  ( 0.000000000000000000, 0.000000000000000000, 1.000000000000000000 ) ) ;
#29943 = AXIS2_PLACEMENT_3D ( 'NONE', #34003, #23101, #50865 ) ;
#29944 = ADVANCED_FACE ( 'NONE', ( #47394 ), #42808, .F. ) ;
#29945 = CARTESIAN_POINT ( 'NONE',  ( 56.52885800925549376, 12.28784885070978916, -20.17303737264423447 ) ) ;
#29946 = ORIENTED_EDGE ( 'NONE', *, *, #55997, .T. ) ;
#29947 = CARTESIAN_POINT ( 'NONE',  ( -72.62976060914719767, -18.74780984163136210, 43.58025477438756212 ) ) ;
#29948 = VERTEX_POINT ( 'NONE', #53358 ) ;
#29949 = CARTESIAN_POINT ( 'NONE',  ( 208.6132326550593916, 111.8685719053116543, 16.27391699821244231 ) ) ;
#29950 = CARTESIAN_POINT ( 'NONE',  ( 8.683910719548892487, 7.383368463746301735, 61.94290726329433028 ) ) ;
#29951 = CARTESIAN_POINT ( 'NONE',  ( 211.7419975634644800, 116.5322580952101390, 34.05327329600243758 ) ) ;
#29952 = CARTESIAN_POINT ( 'NONE',  ( 10.79880987033570783, 6.392085142689816202, -91.09258533748153752 ) ) ;
#29953 = CARTESIAN_POINT ( 'NONE',  ( -77.71448999903253707, 21.96089801565739208, 18.52841490789106160 ) ) ;
#29954 = VECTOR ( 'NONE', #14750, 1000.000000000000000 ) ;
#29955 = ADVANCED_FACE ( 'NONE', ( #63934 ), #41452, .F. ) ;
#29956 = ORIENTED_EDGE ( 'NONE', *, *, #4928, .T. ) ;
#29957 = ORIENTED_EDGE ( 'NONE', *, *, #68405, .F. ) ;
#29958 = CARTESIAN_POINT ( 'NONE',  ( 0.000000000000000000, 0.000000000000000000, 0.000000000000000000 ) ) ;
#29959 = DIRECTION ( 'NONE',  ( 0.000000000000000000, 0.000000000000000000, 1.000000000000000000 ) ) ;
#29960 = CARTESIAN_POINT ( 'NONE',  ( 34.45972925205163762, 8.830088223935240066, -75.62682501707777760 ) ) ;
#29961 = CYLINDRICAL_SURFACE ( 'NONE', #66923, 7.500000000000020428 ) ;
#29962 = CARTESIAN_POINT ( 'NONE',  ( 12.30794027880714303, 6.414170680043896233, 84.55216331891460868 ) ) ;
#29963 = ADVANCED_FACE ( 'NONE', ( #64276 ), #30546, .T. ) ;
#29964 = B_SPLINE_CURVE_WITH_KNOTS ( 'NONE', 3,
 ( #32070, #31383, #21173, #36661, #4638, #43294, #68994, #59478, #5664, #393, #69354, #64770, #54189, #42948, #15886, #21851, #26101, #47531, #27471, #10951, #10258, #64418, #63742, #20819, #32420, #48914, #42278, #44, #58783, #37001, #53151, #31719, #64074, #6011, #58112, #27125, #4985, #752, #42618, #22207, #59129, #52816, #43645 ),
 .UNSPECIFIED., .F., .F.,
 ( 4, 2, 2, 2, 2, 2, 2, 2, 2, 2, 2, 2, 1, 2, 2, 2, 2, 2, 2, 2, 2, 4 ),
 ( 0.02371951416048007424, 0.02520633211177540287, 0.02594974108742304636, 0.02669315006307068985, 0.02817996801436598031, 0.02966678596566126730, 0.03041019494130891426, 0.03115360391695655776, 0.03264042186825184821, 0.03412723981954713520, 0.03561405777084242219, 0.03635746674649006915, 0.03710087572213771612, 0.03784428469778536308, 0.03858769367343301004, 0.04007451162472831091, 0.04156132957602361178, 0.04304814752731891958, 0.04379155650296657348, 0.04453496547861422045, 0.04602178342990952825, 0.04750860138120482912 ),
 .UNSPECIFIED. ) ;
#29965 = CARTESIAN_POINT ( 'NONE',  ( 22.59201934342795681, 7.821623272182323561, 94.42844641394751193 ) ) ;
#29966 = EDGE_LOOP ( 'NONE', ( #19144, #16859, #38336, #51346 ) ) ;
#29967 = FACE_OUTER_BOUND ( 'NONE', #51817, .T. ) ;
#29968 = CARTESIAN_POINT ( 'NONE',  ( 203.1423857108907498, 105.9238244286949708, -51.17351567888142228 ) ) ;
#29969 = VERTEX_POINT ( 'NONE', #3814 ) ;
#29970 = PLANE ( 'NONE',  #8153 ) ;
#29971 = VERTEX_POINT ( 'NONE', #25281 ) ;
#29972 = CARTESIAN_POINT ( 'NONE',  ( -85.91089317961402116, 25.21459833389208782, -71.46727687246068683 ) ) ;
#29973 = CARTESIAN_POINT ( 'NONE',  ( -452.6627218934913230, 217.8591479523843475, 78.55029585798814651 ) ) ;
#29974 = ORIENTED_EDGE ( 'NONE', *, *, #48989, .T. ) ;
#29975 = ORIENTED_EDGE ( 'NONE', *, *, #1262, .T. ) ;
#29976 = CARTESIAN_POINT ( 'NONE',  ( 10.83046137699561484, 6.392429922561258415, -37.37009112564436464 ) ) ;
#29977 = CARTESIAN_POINT ( 'NONE',  ( -108.8556526337305996, 37.39618721751735819, -92.58918846270292136 ) ) ;
#29978 = CARTESIAN_POINT ( 'NONE',  ( 103.8055367708241050, 27.11070767929348335, 14.14709985013681148 ) ) ;
#29979 = VERTEX_POINT ( 'NONE', #46719 ) ;
#29980 = PRODUCT_DEFINITION_SHAPE ( 'NONE', 'NONE',  #69606 ) ;
#29981 = CARTESIAN_POINT ( 'NONE',  ( 0.000000000000000000, 0.000000000000000000, 41.38025477438755928 ) ) ;
#29982 = VECTOR ( 'NONE', #37962, 1000.000000000000000 ) ;
#29983 = CARTESIAN_POINT ( 'NONE',  ( 176.6238742729554474, 75.60943990211363541, -76.61804891973169163 ) ) ;
#29984 = CARTESIAN_POINT ( 'NONE',  ( -444.4229916354184979, 394.6798985497181889, -128.9497041420121093 ) ) ;
#29985 = B_SPLINE_CURVE_WITH_KNOTS ( 'NONE', 3,
 ( #69006, #762, #10962, #22216, #1111, #17640, #16239, #38390, #6730, #54198, #48229, #43653, #32769, #44357, #5348, #22561, #48569, #65841, #16586, #39107, #27838, #54, #12360, #37691, #54906, #6021, #21514, #26802, #404, #28176, #60546, #17275, #32429, #65132, #43304, #38749, #12011, #59831, #5673, #27481, #64780, #33817, #44004, #11649, #65482, #60193, #42957, #48922, #64428, #33484, #49628, #53856, #16926, #27136, #1457, #38043, #21861, #33126, #54556, #59487 ),
 .UNSPECIFIED., .F., .F.,
 ( 4, 2, 2, 2, 2, 2, 2, 2, 2, 2, 2, 2, 2, 2, 2, 2, 2, 2, 2, 2, 2, 2, 2, 2, 2, 2, 2, 2, 2, 4 ),
 ( 0.000000000000000000, 0.002104973360485384165, 0.003157460040728082319, 0.004209946720970781341, 0.005262433401213479495, 0.006314920081456177649, 0.007367406761698876670, 0.008419893441941574824, 0.009472380122184272111, 0.01052486680242696940, 0.01157735348266966668, 0.01262984016291236397, 0.01368232684315506473, 0.01473481352339776722, 0.01683978688388317740, 0.01789227356412587816, 0.01894476024436858239, 0.01999724692461128661, 0.02104973360485398737, 0.02315470696533938194, 0.02420719364558207923, 0.02525968032582477651, 0.02631216700606748074, 0.02736465368631018150, 0.02841714036655287878, 0.02946962704679557954, 0.03052211372703827683, 0.03157460040728097411, 0.03262708708752367487, 0.03367957376776637562 ),
 .UNSPECIFIED. ) ;
#29986 = CARTESIAN_POINT ( 'NONE',  ( 112.7784411285249178, 30.07270878825233851, -23.64024644625330751 ) ) ;
#29987 = CARTESIAN_POINT ( 'NONE',  ( 84.26390409839196138, 19.68678207880321196, -36.18818452320425649 ) ) ;
#29988 = AXIS2_PLACEMENT_3D ( 'NONE', #51997, #14709, #68851 ) ;
#29989 = DIRECTION ( 'NONE',  ( 0.000000000000000000, 0.000000000000000000, 1.000000000000000000 ) ) ;
#29990 = ORIENTED_EDGE ( 'NONE', *, *, #55999, .F. ) ;
#29991 = VECTOR ( 'NONE', #14216, 999.9999999999998863 ) ;
#29992 = ORIENTED_EDGE ( 'NONE', *, *, #31278, .T. ) ;
#29993 = CARTESIAN_POINT ( 'NONE',  ( 45.90693067088658097, 9.344800815249309167, 14.33438021413847530 ) ) ;
#29994 = CARTESIAN_POINT ( 'NONE',  ( -8.062763356759356626, -40.94272338264845956, 13.79046412294881208 ) ) ;
#29995 = DIRECTION ( 'NONE',  ( 0.9362348706397417564, -0.3513748240813305279, 0.000000000000000000 ) ) ;
#29996 = ADVANCED_FACE ( 'NONE', ( #9440 ), #57630, .F. ) ;
#29997 = LINE ( 'NONE', #63390, #25431 ) ;
#29998 = CARTESIAN_POINT ( 'NONE',  ( 55.56474667084417263, 11.06706367715628758, -69.07264011740940646 ) ) ;
#29999 = AXIS2_PLACEMENT_3D ( 'NONE', #34090, #8039, #34449 ) ;
#30000 = CARTESIAN_POINT ( 'NONE',  ( 126.4754729582247847, 37.14269484129876275, 11.52096225339949598 ) ) ;
#30001 = CARTESIAN_POINT ( 'NONE',  ( -31.01099134985120642, 9.521461689106248016, -89.01550512782000624 ) ) ;
#30002 = CARTESIAN_POINT ( 'NONE',  ( 211.9209160201162945, 118.6566773314361001, 88.36684836799790332 ) ) ;
#30003 = CARTESIAN_POINT ( 'NONE',  ( 208.9583973663597192, 114.1615900753670445, 30.51926161164170992 ) ) ;
#30004 = CARTESIAN_POINT ( 'NONE',  ( -83.13046924527392889, 25.15778674529014225, 58.73105344031623787 ) ) ;
#30005 = DIRECTION ( 'NONE',  ( -0.000000000000000000, 0.000000000000000000, 1.000000000000000000 ) ) ;
#30007 = ORIENTED_EDGE ( 'NONE', *, *, #53757, .F. ) ;
#30006 = ADVANCED_FACE ( 'NONE', ( #25630 ), #47064, .T. ) ;
#30008 = CARTESIAN_POINT ( 'NONE',  ( 8.537735592981562149, 7.383000420390739116, -14.24046554414789867 ) ) ;
#30009 = ORIENTED_EDGE ( 'NONE', *, *, #68461, .F. ) ;
#30010 = CARTESIAN_POINT ( 'NONE',  ( 197.8572563162090887, 97.41072138832261373, -13.89129495889377175 ) ) ;
#30011 = ORIENTED_EDGE ( 'NONE', *, *, #42666, .F. ) ;
#30012 = CARTESIAN_POINT ( 'NONE',  ( -148.6471085600699951, 64.76880961642446266, 3.913156007458206798 ) ) ;
#30013 = CARTESIAN_POINT ( 'NONE',  ( 187.8973304652193406, 87.27378997243175718, -73.71654343158144229 ) ) ;
#30014 = CARTESIAN_POINT ( 'NONE',  ( -38.20537251366653209, 11.82499390270895390, 88.10609205668197319 ) ) ;
#30015 = CARTESIAN_POINT ( 'NONE',  ( -94.78109144324895396, 29.13179392050636807, -42.79980480196593362 ) ) ;
#30016 = CARTESIAN_POINT ( 'NONE',  ( -29.50439180771548209, 10.29976981300626804, 3.609381438886668736 ) ) ;
#30017 = CYLINDRICAL_SURFACE ( 'NONE', #29295, 7.500000000000020428 ) ;
#30018 = CYLINDRICAL_SURFACE ( 'NONE', #21368, 7.500000000000013323 ) ;
#30019 = CARTESIAN_POINT ( 'NONE',  ( 129.4987365823222376, 38.85470922756776702, -49.63207471537052129 ) ) ;
#30020 = ORIENTED_EDGE ( 'NONE', *, *, #13419, .T. ) ;
#30021 = EDGE_CURVE ( 'NONE', #45190, #43728, #17111, .T. ) ;
#30022 = ORIENTED_EDGE ( 'NONE', *, *, #62986, .T. ) ;
#30023 = EDGE_CURVE ( 'NONE', #52460, #40175, #9811, .T. ) ;
#30024 = DIRECTION ( 'NONE',  ( 0.000000000000000000, 0.000000000000000000, 1.000000000000000000 ) ) ;
#30025 = CARTESIAN_POINT ( 'NONE',  ( -60.67627457812066183, -44.08389392193601708, 0.000000000000000000 ) ) ;
#30026 = CARTESIAN_POINT ( 'NONE',  ( -27.70562707895079768, 9.007984652865422603, -76.18518309368259622 ) ) ;
#30027 = EDGE_CURVE ( 'NONE', #41104, #19981, #48414, .T. ) ;
#30028 = EDGE_CURVE ( 'NONE', #30365, #21034, #34274, .T. ) ;
#30029 = CARTESIAN_POINT ( 'NONE',  ( 8.848532525911927848, 6.377649276597439965, 13.54568704989812034 ) ) ;
#30030 = ORIENTED_EDGE ( 'NONE', *, *, #56639, .T. ) ;
#30031 = PLANE ( 'NONE',  #15430 ) ;
#30032 = CARTESIAN_POINT ( 'NONE',  ( -59.57462349605617646, 16.98779896904799358, -75.56450611661117023 ) ) ;
#30033 = CARTESIAN_POINT ( 'NONE',  ( 174.9053416555737215, 72.57849647436445650, -74.85130122728419622 ) ) ;
#30034 =( NAMED_UNIT ( * ) PLANE_ANGLE_UNIT ( ) SI_UNIT ( $, .RADIAN. ) );
#30035 = CIRCLE ( 'NONE', #50264, 74.95140232871122521 ) ;
#30036 = CARTESIAN_POINT ( 'NONE',  ( 275.0322429538348956, -21.99260513325770106, -0.6553719608280085263 ) ) ;
#30037 = PRESENTATION_STYLE_ASSIGNMENT (( #18785 ) ) ;
#30038 = CARTESIAN_POINT ( 'NONE',  ( -24.95029760921699946, 9.631514785009935409, 60.79180759298469638 ) ) ;
#30039 = DIRECTION ( 'NONE',  ( -0.000000000000000000, -0.000000000000000000, -1.000000000000000000 ) ) ;
#30040 = CARTESIAN_POINT ( 'NONE',  ( -50.14771795543005339, 13.42081263859821050, 58.96722719906514953 ) ) ;
#30041 = AXIS2_PLACEMENT_3D ( 'NONE', #38762, #65853, #22927 ) ;
#30042 = EDGE_CURVE ( 'NONE', #14210, #31197, #29005, .T. ) ;
#30043 = CARTESIAN_POINT ( 'NONE',  ( -0.7174461528505765573, 6.532311451815528969, 66.86584012114198572 ) ) ;
#30044 = ORIENTED_EDGE ( 'NONE', *, *, #60421, .T. ) ;
#30045 = AXIS2_PLACEMENT_3D ( 'NONE', #51746, #51058, #19040 ) ;
#30046 = CARTESIAN_POINT ( 'NONE',  ( 275.0320943261245361, 21.99263847259265958, 0.6545153999150201685 ) ) ;
#30047 = CARTESIAN_POINT ( 'NONE',  ( -130.6002960060535827, 49.67125682092490990, -75.11777304400855826 ) ) ;
#30048 = CARTESIAN_POINT ( 'NONE',  ( -0.6225858807736643907, -41.72441896235496728, 13.79046412284827383 ) ) ;
#30049 = CARTESIAN_POINT ( 'NONE',  ( -47.60396279792517760, 12.80997843568595229, -43.72255466512232402 ) ) ;
#30050 = EDGE_CURVE ( 'NONE', #41880, #1454, #32616, .T. ) ;
#30051 = LINE ( 'NONE', #34980, #45806 ) ;
#30052 = EDGE_CURVE ( 'NONE', #17792, #3940, #67111, .T. ) ;
#30053 = FACE_OUTER_BOUND ( 'NONE', #65926, .T. ) ;
#30054 = EDGE_CURVE ( 'NONE', #3625, #58133, #59237, .T. ) ;
#30055 = AXIS2_PLACEMENT_3D ( 'NONE', #24786, #14904, #14232 ) ;
#30056 = VECTOR ( 'NONE', #51016, 1000.000000000000000 ) ;
#30057 = ORIENTED_EDGE ( 'NONE', *, *, #56724, .T. ) ;
#30058 =( LENGTH_UNIT ( ) NAMED_UNIT ( * ) SI_UNIT ( .MILLI., .METRE. ) );
#30059 = CARTESIAN_POINT ( 'NONE',  ( 427.4999999999999432, 207.5000000000000284, 0.000000000000000000 ) ) ;
#30060 = ORIENTED_EDGE ( 'NONE', *, *, #21024, .T. ) ;
#30061 = B_SPLINE_CURVE_WITH_KNOTS ( 'NONE', 3,
 ( #46752, #47097, #57666, #15098, #68224, #19675, #41136, #42170, #41486, #9824, #12764, #68559, #34224, #62937, #20362, #14741, #41829, #63286, #36553, #31282, #52709, #22094, #43188, #42840, #27711, #10842, #63633, #22440, #37225, #281, #64662, #53051, #4876, #21068, #16471, #48800, #26687, #65011, #64311, #42514, #54079, #53741, #642, #16806, #5898, #63966, #58335, #10494, #47780, #48116 ),
 .UNSPECIFIED., .F., .F.,
 ( 4, 2, 2, 2, 2, 2, 2, 2, 2, 2, 2, 2, 2, 2, 2, 2, 2, 2, 2, 2, 2, 2, 2, 2, 4 ),
 ( 0.02688458561150008919, 0.02770990876165288844, 0.02853523191180568769, 0.03018587821211130354, 0.03183652451241691245, 0.03266184766256971517, 0.03348717081272251789, 0.03513781711302807476, 0.03678846341333363162, 0.03761378656348642741, 0.03843910971363923013, 0.03926443286379202591, 0.04008975601394482863, 0.04174040231425042713, 0.04256572546440322291, 0.04339104861455601175, 0.04421637176470880753, 0.04504169491486159638, 0.04586701806501439216, 0.04669234121516718794, 0.04834298751547283501, 0.04916831066562561692, 0.04999363381577841270, 0.05164428011608405977, 0.05329492641638969297 ),
 .UNSPECIFIED. ) ;
#30062 = ORIENTED_EDGE ( 'NONE', *, *, #46604, .F. ) ;
#30063 = FACE_OUTER_BOUND ( 'NONE', #13164, .T. ) ;
#30064 = DIRECTION ( 'NONE',  ( 1.000000000000000000, 0.000000000000000000, 0.000000000000000000 ) ) ;
#30065 = DIRECTION ( 'NONE',  ( -1.000000000000000000, 0.000000000000000000, 0.000000000000000000 ) ) ;
#30066 = EDGE_LOOP ( 'NONE', ( #36412, #37689 ) ) ;
#30067 = CARTESIAN_POINT ( 'NONE',  ( -31.11269837220806878, 5.594483210025202879E-14, 85.00100000000000477 ) ) ;
#30068 = CARTESIAN_POINT ( 'NONE',  ( -180.2252811616041868, 95.40045830523435200, 13.89892224170345614 ) ) ;
#30069 = DIRECTION ( 'NONE',  ( 1.000000000000000000, 0.000000000000000000, 0.000000000000000000 ) ) ;
#30070 = CARTESIAN_POINT ( 'NONE',  ( -452.6627218934913230, 177.8591479523843475, 78.55029585798814651 ) ) ;
#30071 = DIRECTION ( 'NONE',  ( -0.000000000000000000, -0.000000000000000000, -1.000000000000000000 ) ) ;
#30072 = CARTESIAN_POINT ( 'NONE',  ( -30.95341298663139540, 10.53108683215057795, -23.47264677473819816 ) ) ;
#30073 = CARTESIAN_POINT ( 'NONE',  ( 135.4423125506059478, 42.39015362494586725, 2.831777643547055856 ) ) ;
#30074 = ORIENTED_EDGE ( 'NONE', *, *, #44302, .T. ) ;
#30075 = CARTESIAN_POINT ( 'NONE',  ( 31.11269837220800127, -31.11269837220812562, 0.000000000000000000 ) ) ;
#30076 = CARTESIAN_POINT ( 'NONE',  ( 0.000000000000000000, 0.000000000000000000, 85.00000000000000000 ) ) ;
#30077 = CARTESIAN_POINT ( 'NONE',  ( 46.13856685535758118, 9.381502944822518231, -39.78633803483338482 ) ) ;
#30078 = CARTESIAN_POINT ( 'NONE',  ( -71.63719014813169395, 20.83242381180886937, 88.97194804729541318 ) ) ;
#30080 = ORIENTED_EDGE ( 'NONE', *, *, #6132, .F. ) ;
#30079 = CARTESIAN_POINT ( 'NONE',  ( -189.2776534485022069, -170.0000000000000000, -95.00000000000133582 ) ) ;
#30081 = CARTESIAN_POINT ( 'NONE',  ( 13.24564585880038514, 63.65041531508843065, 170.0000000000000000 ) ) ;
#30082 = VERTEX_POINT ( 'NONE', #5868 ) ;
#30083 = ORIENTED_EDGE ( 'NONE', *, *, #5686, .F. ) ;
#30084 = CARTESIAN_POINT ( 'NONE',  ( -142.0251973982164770, 58.08401473564117623, 64.47829236375538642 ) ) ;
#30085 = VECTOR ( 'NONE', #35338, 1000.000000000000227 ) ;
#30086 = CARTESIAN_POINT ( 'NONE',  ( -84.49322488516129681, 0.000000000000000000, 43.58025477438756212 ) ) ;
#30087 = CARTESIAN_POINT ( 'NONE',  ( 0.000000000000000000, 0.000000000000000000, 41.38025477438755928 ) ) ;
#30088 = CARTESIAN_POINT ( 'NONE',  ( -20.55634918610411077, -46.66904755831208718, 85.00100000000000477 ) ) ;
#30089 = DIRECTION ( 'NONE',  ( -0.000000000000000000, 1.000000000000000000, -0.000000000000000000 ) ) ;
#30090 = VECTOR ( 'NONE', #16865, 1000.000000000000000 ) ;
#30091 = CARTESIAN_POINT ( 'NONE',  ( -81.01931326044685022, 24.31309346877660715, -8.645523102376230895 ) ) ;
#30092 = DIRECTION ( 'NONE',  ( -0.000000000000000000, 0.000000000000000000, -1.000000000000000000 ) ) ;
#30093 = ADVANCED_FACE ( 'NONE', ( #29333 ), #61346, .F. ) ;
#30094 = CARTESIAN_POINT ( 'NONE',  ( -151.2497169612549044, 65.66843968092747730, -34.96368695887081657 ) ) ;
#30095 = VERTEX_POINT ( 'NONE', #11151 ) ;
#30096 = EDGE_LOOP ( 'NONE', ( #25552, #1199, #38398, #15111 ) ) ;
#30097 = AXIS2_PLACEMENT_3D ( 'NONE', #33943, #24435, #34292 ) ;
#30098 = CARTESIAN_POINT ( 'NONE',  ( -109.7643866341847172, 37.89854104106755273, 10.62320483512874070 ) ) ;
#30099 = CARTESIAN_POINT ( 'NONE',  ( 109.3079614081140818, 28.45126415661779617, 71.41187614436252318 ) ) ;
#30100 = CARTESIAN_POINT ( 'NONE',  ( 0.000000000000000000, 190.0000000000000000, 380.0000000000000000 ) ) ;
#30101 = CARTESIAN_POINT ( 'NONE',  ( -189.7987719395348734, 107.8653664616570609, 68.14804509738834781 ) ) ;
#30102 = VECTOR ( 'NONE', #23754, 1000.000000000000114 ) ;
#30103 = CARTESIAN_POINT ( 'NONE',  ( 15.55634918610409656, 36.11269837220803680, 85.00100000000000477 ) ) ;
#30104 = LINE ( 'NONE', #46261, #7884 ) ;
#30105 = CARTESIAN_POINT ( 'NONE',  ( -142.9201923544618182, 60.07121543956493781, 88.30931796572481574 ) ) ;
#30106 = VERTEX_POINT ( 'NONE', #22407 ) ;
#30107 = EDGE_CURVE ( 'NONE', #23015, #48266, #50784, .T. ) ;
#30108 = ORIENTED_EDGE ( 'NONE', *, *, #58570, .T. ) ;
#30109 = EDGE_CURVE ( 'NONE', #2286, #32665, #28457, .T. ) ;
#30110 = ORIENTED_EDGE ( 'NONE', *, *, #50417, .T. ) ;
#30111 = ADVANCED_FACE ( 'NONE', ( #62735 ), #31077, .F. ) ;
#30112 = AXIS2_PLACEMENT_3D ( 'NONE', #46504, #41246, #62703 ) ;
#30113 = CYLINDRICAL_SURFACE ( 'NONE', #22912, 7.500000000000020428 ) ;
#30114 = CARTESIAN_POINT ( 'NONE',  ( 174.7690563370620112, 72.45075441521997561, -93.36227965153190667 ) ) ;
#30115 = CARTESIAN_POINT ( 'NONE',  ( 64.69649025047537805, 13.06878919510321602, -50.53396286999748099 ) ) ;
#30116 = CARTESIAN_POINT ( 'NONE',  ( 109.8560624239070336, 28.70302459854760713, -89.61153874658104712 ) ) ;
#30117 = EDGE_CURVE ( 'NONE', #56201, #48145, #28944, .T. ) ;
#30118 = CARTESIAN_POINT ( 'NONE',  ( -56.01329802674221980, 15.98369420723828860, 30.36332081584329856 ) ) ;
#30119 = B_SPLINE_CURVE_WITH_KNOTS ( 'NONE', 3,
 ( #55612, #7441, #21858, #43300, #64776, #9161, #46093, #13066, #29925, #66537, #18326, #40819, #62273, #35551, #45052, #2849, #46436, #56303, #19713, #14092, #34866, #51388, #67915, #41174, #50346, #13403, #67562, #45757, #23954, #29234, #8827, #14443, #45404, #24316, #57349, #35895, #67237, #19021, #39784, #66887, #40472, #55970, #18681, #8122 ),
 .UNSPECIFIED., .F., .F.,
 ( 4, 2, 2, 2, 2, 2, 2, 2, 2, 2, 2, 2, 2, 2, 2, 2, 2, 2, 2, 2, 2, 4 ),
 ( 0.000000000000000000, 0.001533942663855612787, 0.003067885327711225574, 0.004601827991566838361, 0.005368799323494643019, 0.006135770655422447678, 0.007669713319278084751, 0.008436684651205901553, 0.009203655983133720089, 0.01073759864698937451, 0.01150456997891720172, 0.01227154131084502893, 0.01303851264277285787, 0.01380548397470068335, 0.01533942663855629787, 0.01687336930241191066, 0.01840731196626752345, 0.01994125463012313623, 0.02070822596205094956, 0.02147519729397876637, 0.02300913995783438262, 0.02454308262169000235 ),
 .UNSPECIFIED. ) ;
#30120 = CARTESIAN_POINT ( 'NONE',  ( -37.93983213483220140, 11.77368372188049328, -65.88929680851603621 ) ) ;
#30121 = CARTESIAN_POINT ( 'NONE',  ( -40.99999999999997868, 0.000000000000000000, -6.071532165918823253E-15 ) ) ;
#30122 = CARTESIAN_POINT ( 'NONE',  ( 32.10490206750998965, 7.572278537213176008, 92.86731323645747693 ) ) ;
#30123 = SHAPE_REPRESENTATION_RELATIONSHIP ( 'NONE' , 'NONE' ,  #34334, #41606 ) ;
#30124 = ORIENTED_EDGE ( 'NONE', *, *, #13414, .F. ) ;
#30125 = CARTESIAN_POINT ( 'NONE',  ( -0.5158933718595617446, 6.525180340836105763, -41.22077923227989515 ) ) ;
#30126 = CARTESIAN_POINT ( 'NONE',  ( 2.700000000000004619, 0.000000000000000000, 0.000000000000000000 ) ) ;
#30127 = CARTESIAN_POINT ( 'NONE',  ( -118.6849742182705398, 41.92701402439733016, 13.36181871470159876 ) ) ;
#30128 = CARTESIAN_POINT ( 'NONE',  ( 65.41496713438826305, 13.24164235279043389, -62.94294025472531473 ) ) ;
#30129 = CARTESIAN_POINT ( 'NONE',  ( 126.8947007444828898, 37.37669340849691224, -19.48012531352281584 ) ) ;
#30130 = DIRECTION ( 'NONE',  ( 1.000000000000000000, 0.000000000000000000, 0.000000000000000000 ) ) ;
#30131 = CARTESIAN_POINT ( 'NONE',  ( -107.0751323097254470, 35.28386110859231906, -75.14699250370651384 ) ) ;
#30132 = ORIENTED_EDGE ( 'NONE', *, *, #61711, .F. ) ;
#30133 = SHAPE_DEFINITION_REPRESENTATION ( #29406, #55473 ) ;
#30134 = CARTESIAN_POINT ( 'NONE',  ( 63.01563776193091826, 12.67277567978495512, -89.40979201309708913 ) ) ;
#30135 = CARTESIAN_POINT ( 'NONE',  ( 6.400000000000000355, 0.000000000000000000, 0.000000000000000000 ) ) ;
#30136 = ADVANCED_FACE ( 'NONE', ( #67670 ), #63071, .F. ) ;
#30137 = LINE ( 'NONE', #51588, #5376 ) ;
#30138 = ADVANCED_FACE ( 'NONE', ( #30373 ), #30031, .T. ) ;
#30139 = CONTEXT_DEPENDENT_SHAPE_REPRESENTATION ( #54345, #32655 ) ;
#30140 = DIRECTION ( 'NONE',  ( -0.000000000000000000, -0.000000000000000000, 1.000000000000000000 ) ) ;
#30141 = ORIENTED_EDGE ( 'NONE', *, *, #19954, .F. ) ;
#30142 = EDGE_LOOP ( 'NONE', ( #65328, #18372, #26644, #25516 ) ) ;
#30143 = EDGE_CURVE ( 'NONE', #48419, #53230, #8230, .T. ) ;
#30144 = CARTESIAN_POINT ( 'NONE',  ( -145.9095871962850595, 61.18682730038540285, -8.883549365152694222 ) ) ;
#30145 = CARTESIAN_POINT ( 'NONE',  ( 199.3764173596862008, 100.9540560740992134, 4.553511661046183434 ) ) ;
#30146 = ORIENTED_EDGE ( 'NONE', *, *, #32245, .F. ) ;
#30147 = VECTOR ( 'NONE', #27510, 1000.000000000000000 ) ;
#30148 =( REPRESENTATION_RELATIONSHIP ('NONE','NONE', #40274, #64096 ) REPRESENTATION_RELATIONSHIP_WITH_TRANSFORMATION ( #17121 )SHAPE_REPRESENTATION_RELATIONSHIP( ) );
#30149 = CARTESIAN_POINT ( 'NONE',  ( 161.5974713863948011, 62.23003014314474513, 84.30540274493955621 ) ) ;
#30150 = ORIENTED_EDGE ( 'NONE', *, *, #26122, .F. ) ;
#30151 = CARTESIAN_POINT ( 'NONE',  ( -55.54036735998992924, 15.85474597822063281, 18.47277718246749956 ) ) ;
#30152 = CARTESIAN_POINT ( 'NONE',  ( -2.700000000000004619, 0.000000000000000000, 0.000000000000000000 ) ) ;
#30153 = CARTESIAN_POINT ( 'NONE',  ( -153.6994314938755224, 69.16570456337669270, 44.45659357967959124 ) ) ;
#30154 = DIRECTION ( 'NONE',  ( -0.000000000000000000, -0.000000000000000000, -1.000000000000000000 ) ) ;
#30155 = CIRCLE ( 'NONE', #27875, 27.00000000000000000 ) ;
#30156 = DIRECTION ( 'NONE',  ( -0.000000000000000000, 1.000000000000000000, -0.000000000000000000 ) ) ;
#30158 = ORIENTED_EDGE ( 'NONE', *, *, #30733, .T. ) ;
#30157 = DIRECTION ( 'NONE',  ( 1.000000000000000000, 0.000000000000000000, 0.000000000000000000 ) ) ;
#30159 = CARTESIAN_POINT ( 'NONE',  ( 57.07734607129818016, 11.37318329671159312, 32.70553640740841672 ) ) ;
#30160 = ORIENTED_EDGE ( 'NONE', *, *, #3058, .T. ) ;
#30161 = VERTEX_POINT ( 'NONE', #25108 ) ;
#30162 = CARTESIAN_POINT ( 'NONE',  ( -165.9121868482146454, 80.88751546905565704, 9.386801319154086443 ) ) ;
#30163 = CARTESIAN_POINT ( 'NONE',  ( 20.36314374176837916, 6.689939636827348934, -75.82707789680702604 ) ) ;
#30165 = ORIENTED_EDGE ( 'NONE', *, *, #28112, .F. ) ;
#30164 = CARTESIAN_POINT ( 'NONE',  ( 16.78635691501517613, 6.000000000000000000, -9.435653166495500344 ) ) ;
#30166 = CARTESIAN_POINT ( 'NONE',  ( -95.44494005344630239, 30.55403701725966670, 88.60368125266712980 ) ) ;
#30167 = CARTESIAN_POINT ( 'NONE',  ( -75.43495400358861502, 22.18831810339349886, -49.38790907511541661 ) ) ;
#30168 = ORIENTED_EDGE ( 'NONE', *, *, #32865, .F. ) ;
#30169 = CARTESIAN_POINT ( 'NONE',  ( 209.6698611676811481, 115.2210955123518517, -65.03741327442061504 ) ) ;
#30170 = CARTESIAN_POINT ( 'NONE',  ( 8.000000000000007105, 249.8719672152120381, -95.00000000000133582 ) ) ;
#30171 = EDGE_CURVE ( 'NONE', #42155, #7326, #68016, .T. ) ;
#30172 = CARTESIAN_POINT ( 'NONE',  ( 114.6797682035589219, 32.10876583290006892, 31.04538199320165148 ) ) ;
#30173 = CARTESIAN_POINT ( 'NONE',  ( -50.92620509423088038, 55.07344309828770434, 43.58025477438756212 ) ) ;
#30174 = CARTESIAN_POINT ( 'NONE',  ( 68.94948716683072121, 15.16699441119056146, -74.67836426230981317 ) ) ;
#30175 = ORIENTED_EDGE ( 'NONE', *, *, #8526, .F. ) ;
#30176 = ORIENTED_EDGE ( 'NONE', *, *, #17201, .F. ) ;
#30177 = CARTESIAN_POINT ( 'NONE',  ( 11.79090982778180141, 7.411142935774506668, -90.30599167494429480 ) ) ;
#30178 = LINE ( 'NONE', #7067, #25593 ) ;
#30179 = CARTESIAN_POINT ( 'NONE',  ( 99.71998884745383407, 188.0000000000000000, 7.478223336038896996 ) ) ;
#30180 = CARTESIAN_POINT ( 'NONE',  ( -47.88880928231646550, 12.87693921808227770, -94.14315601767113151 ) ) ;
#30181 = CARTESIAN_POINT ( 'NONE',  ( -54.62718114890975585, 15.60883832648648095, -88.90542517938722256 ) ) ;
#30182 = LINE ( 'NONE', #18930, #9024 ) ;
#30183 = CARTESIAN_POINT ( 'NONE',  ( 70.50376765786471367, 15.57629333413342998, -43.71097164717498629 ) ) ;
#30184 = CARTESIAN_POINT ( 'NONE',  ( -44.99999999999998579, -22.99999999999998579, 4.000000000000000000 ) ) ;
#30185 = CARTESIAN_POINT ( 'NONE',  ( 204.6977192012829789, 106.3443248447423599, 56.05227132923312183 ) ) ;
#30186 = ADVANCED_FACE ( 'NONE', ( #62028 ), #3989, .T. ) ;
#30187 = ORIENTED_EDGE ( 'NONE', *, *, #31366, .F. ) ;
#30188 = CARTESIAN_POINT ( 'NONE',  ( -108.5248383251030333, 37.21456094989613206, 33.85788099656151218 ) ) ;
#30189 = VERTEX_POINT ( 'NONE', #14875 ) ;
#30190 = CARTESIAN_POINT ( 'NONE',  ( -32.41627406084104734, 9.753381371531503419, 18.32381523465870288 ) ) ;
#30191 = CARTESIAN_POINT ( 'NONE',  ( 79.92842440418705507, 18.29578799637231512, 60.65141981179670694 ) ) ;
#30192 = EDGE_CURVE ( 'NONE', #1555, #44224, #38541, .T. ) ;
#30193 = ORIENTED_EDGE ( 'NONE', *, *, #43361, .F. ) ;
#30194 = CARTESIAN_POINT ( 'NONE',  ( -20.63749999999999929, 2.449293598294705724E-15, 19.99999999999999289 ) ) ;
#30195 = CARTESIAN_POINT ( 'NONE',  ( 26.12852347772543737, 70.00000000000000000, 77.58025477438755502 ) ) ;
#30196 = CONICAL_SURFACE ( 'NONE', #40281, 74.99999999999998579, 0.6747409422235518539 ) ;
#30197 = ADVANCED_FACE ( 'NONE', ( #37031 ), #38059, .F. ) ;
#30198 = CARTESIAN_POINT ( 'NONE',  ( 47.99999999999997158, -20.00000000000000355, 0.000000000000000000 ) ) ;
#30199 = CARTESIAN_POINT ( 'NONE',  ( -444.4229916354184411, 400.0000000000065370, -128.9497041420121093 ) ) ;
#30200 = CARTESIAN_POINT ( 'NONE',  ( -12.40598104375063571, 8.242193636955557068, -36.95900104685619425 ) ) ;
#30201 = DIRECTION ( 'NONE',  ( -0.7100673072878298520, -0.7041338076821836989, 0.000000000000000000 ) ) ;
#30202 = ADVANCED_FACE ( 'NONE', ( #20497 ), #59160, .T. ) ;
#30203 = AXIS2_PLACEMENT_3D ( 'NONE', #11905, #31982, #48137 ) ;
#30204 = ORIENTED_EDGE ( 'NONE', *, *, #41476, .F. ) ;
#30205 = DIRECTION ( 'NONE',  ( 1.000000000000000000, 0.000000000000000000, 0.000000000000000000 ) ) ;
#30206 = VERTEX_POINT ( 'NONE', #16256 ) ;
#30207 = CARTESIAN_POINT ( 'NONE',  ( -173.1211646369891355, -170.0000000000000000, -88.40105834567734178 ) ) ;
#30208 = CARTESIAN_POINT ( 'NONE',  ( -57.65574514524054450, 16.43983577669854768, 57.62394589512655330 ) ) ;
#30209 = CARTESIAN_POINT ( 'NONE',  ( -189.4248691432192118, 107.3461292335514230, 9.845412498708020266 ) ) ;
#30210 = VERTEX_POINT ( 'NONE', #53535 ) ;
#30211 = CARTESIAN_POINT ( 'NONE',  ( -61.29635759142585982, -21.66977272663580578, 41.38025477438755928 ) ) ;
#30212 = CARTESIAN_POINT ( 'NONE',  ( -58.35379405639710626, 15.59115156255354329, -89.65743652648848183 ) ) ;
#30213 = CARTESIAN_POINT ( 'NONE',  ( -38.55214349681829589, 10.86754840574842085, 35.28784456186913587 ) ) ;
#30214 = CARTESIAN_POINT ( 'NONE',  ( 154.4435090467313501, 56.59612921827833532, -36.75824220859233549 ) ) ;
#30215 = ORIENTED_EDGE ( 'NONE', *, *, #5535, .F. ) ;
#30216 = DIRECTION ( 'NONE',  ( 0.4127148655274874289, -0.9108602745606092510, -7.359365692622866563E-15 ) ) ;
#30217 = CARTESIAN_POINT ( 'NONE',  ( -155.1204242627070187, 70.44799358128194910, 60.08489091306021379 ) ) ;
#30218 = CARTESIAN_POINT ( 'NONE',  ( -188.6739852773921200, 108.2139733222100375, 66.97274234833881223 ) ) ;
#30219 = CARTESIAN_POINT ( 'NONE',  ( -15.55634918610400597, 15.55634918610405748, 2.000000000000001776 ) ) ;
#30220 = EDGE_LOOP ( 'NONE', ( #6930, #64984, #42364, #58263 ) ) ;
#30221 = CARTESIAN_POINT ( 'NONE',  ( -175.9864315813574933, 91.91454246454364352, -76.00044308918302249 ) ) ;
#30222 = B_SPLINE_CURVE_WITH_KNOTS ( 'NONE', 3,
 ( #1820, #61250, #56308, #61596, #13070, #65843 ),
 .UNSPECIFIED., .F., .F.,
 ( 4, 2, 4 ),
 ( 1.095770181105393655E-06, 0.03239442681617711595, 0.06478775786217312593 ),
 .UNSPECIFIED. ) ;
#30223 = CARTESIAN_POINT ( 'NONE',  ( -65.36598343705435354, 0.000000000000000000, 41.38025477438755928 ) ) ;
#30224 = EDGE_CURVE ( 'NONE', #19726, #54877, #64801, .T. ) ;
#30225 = CARTESIAN_POINT ( 'NONE',  ( 114.4640969196986191, 30.88424258798505306, 30.90719979216948943 ) ) ;
#30226 = LINE ( 'NONE', #35847, #41813 ) ;
#30227 = B_SPLINE_CURVE_WITH_KNOTS ( 'NONE', 3,
 ( #10302, #64466, #31095, #26152, #57818, #63441, #15599, #31771 ),
 .UNSPECIFIED., .F., .F.,
 ( 4, 2, 2, 4 ),
 ( 0.01336725832182608306, 0.01453745201803765055, 0.01570764571424921457, 0.01804803310667234956 ),
 .UNSPECIFIED. ) ;
#30228 = FACE_OUTER_BOUND ( 'NONE', #5579, .T. ) ;
#30229 = ORIENTED_EDGE ( 'NONE', *, *, #19669, .F. ) ;
#30230 = CARTESIAN_POINT ( 'NONE',  ( 203.1511228994173734, 104.2426341584999392, 29.32292381179308904 ) ) ;
#30231 = CARTESIAN_POINT ( 'NONE',  ( 8.000000000000000000, 4.618802153516997855, -9.500000000000000000 ) ) ;
#30232 = CARTESIAN_POINT ( 'NONE',  ( 187.8965227056807521, 87.27289477191496303, 39.95742566600716827 ) ) ;
#30233 = CARTESIAN_POINT ( 'NONE',  ( 140.9141742510256279, 47.05414327990545331, 7.575130398038848689 ) ) ;
#30234 = FACE_OUTER_BOUND ( 'NONE', #44877, .T. ) ;
#30235 = ORIENTED_EDGE ( 'NONE', *, *, #2569, .F. ) ;
#30236 = CARTESIAN_POINT ( 'NONE',  ( 164.6598737201887843, 64.78038692612514637, -18.98586800582112133 ) ) ;
#30237 = VERTEX_POINT ( 'NONE', #26130 ) ;
#30238 = CARTESIAN_POINT ( 'NONE',  ( 8.000000000000007105, 249.8719672152120381, 94.99999999999866418 ) ) ;
#30239 = CARTESIAN_POINT ( 'NONE',  ( 126.7968382499399809, 37.32194343744114207, 88.14309609214454611 ) ) ;
#30240 = CIRCLE ( 'NONE', #8903, 164.5210298272983778 ) ;
#30242 = EDGE_LOOP ( 'NONE', ( #14308, #1916, #43778, #40502 ) ) ;
#30241 = DIRECTION ( 'NONE',  ( 0.8345732537212999791, 0.5508969814521065267, -0.000000000000000000 ) ) ;
#30243 = CARTESIAN_POINT ( 'NONE',  ( -149.5074843970971017, 64.17983161892348676, -61.65738112195564469 ) ) ;
#30244 = DIRECTION ( 'NONE',  ( -0.000000000000000000, 1.000000000000000000, -0.000000000000000000 ) ) ;
#30245 = VECTOR ( 'NONE', #56168, 1000.000000000000000 ) ;
#30246 = CARTESIAN_POINT ( 'NONE',  ( 163.7607557204680404, 62.71181783708028235, -39.50859774029689930 ) ) ;
#30247 = ORIENTED_EDGE ( 'NONE', *, *, #57323, .F. ) ;
#30248 = CARTESIAN_POINT ( 'NONE',  ( -99.10904156412044586, 32.31949011661293270, 17.98775302372827056 ) ) ;
#30249 = EDGE_CURVE ( 'NONE', #12453, #66690, #67119, .T. ) ;
#30250 = EDGE_CURVE ( 'NONE', #63181, #40287, #24430, .T. ) ;
#30251 = CARTESIAN_POINT ( 'NONE',  ( 55.82249137702105202, 12.14481401622953527, 88.85236193575613584 ) ) ;
#30252 = PLANE ( 'NONE',  #12976 ) ;
#30253 = CARTESIAN_POINT ( 'NONE',  ( 50.03867889673372105, -42.05760816978111194, 41.38025477438755928 ) ) ;
#30254 = EDGE_CURVE ( 'NONE', #38471, #51430, #21055, .T. ) ;
#30255 = CARTESIAN_POINT ( 'NONE',  ( -171.0814041607219451, 84.88598211196838861, 31.09197369155747381 ) ) ;
#30256 = CARTESIAN_POINT ( 'NONE',  ( 150.2794558856211324, 52.26944788078752424, 65.95378106583270039 ) ) ;
#30257 = CARTESIAN_POINT ( 'NONE',  ( 44.99999999999999289, 20.00000000000000355, 0.000000000000000000 ) ) ;
#30258 = B_SPLINE_CURVE_WITH_KNOTS ( 'NONE', 3,
 ( #51211, #40998, #62454, #19184, #40638, #62098, #13914, #35376, #26199, #15981, #47979, #37784, #4734, #31820, #49012, #53940, #21602, #5763, #27222, #47635, #37431, #850, #27570, #63834, #53251, #26885, #22302, #58882, #43739, #10697, #65217, #37095, #59229, #15644, #32172, #53604, #64519, #11384, #58534, #6111, #36759, #48658, #31477, #64869, #10354 ),
 .UNSPECIFIED., .F., .F.,
 ( 4, 2, 2, 1, 2, 2, 2, 2, 2, 2, 2, 2, 2, 2, 2, 2, 2, 2, 2, 2, 2, 2, 4 ),
 ( 0.02345095402629350512, 0.02491692321306682514, 0.02564990780645348689, 0.02638289239984014517, 0.02711587699322680345, 0.02784886158661346520, 0.02931483077338677481, 0.03004781536677342962, 0.03078079996016008443, 0.03224676914693339058, 0.03297975374032004886, 0.03371273833370670020, 0.03517870752048000982, 0.03664467670725331944, 0.03737766130063997772, 0.03811064589402662905, 0.03957661508079991786, 0.04104258426757321360, 0.04250855345434650934, 0.04324153804773314680, 0.04397452264111979814, 0.04544049182789308694, 0.04690646101466637574 ),
 .UNSPECIFIED. ) ;
#30259 = VERTEX_POINT ( 'NONE', #26476 ) ;
#30260 = CARTESIAN_POINT ( 'NONE',  ( -96.45303203827901939, 31.03218867996498531, 69.61143926203455123 ) ) ;
#30261 = CARTESIAN_POINT ( 'NONE',  ( -8.800520192024523070, 7.964629484975256801, 57.00751323463713760 ) ) ;
#30262 = ORIENTED_EDGE ( 'NONE', *, *, #22943, .T. ) ;
#30263 = EDGE_CURVE ( 'NONE', #42164, #42704, #3227, .T. ) ;
#30264 = CARTESIAN_POINT ( 'NONE',  ( 149.9883446984744637, 53.30011109831374227, -17.36738191414244170 ) ) ;
#30265 = CARTESIAN_POINT ( 'NONE',  ( 39.40195752203892710, -170.0000000000000000, -96.80891864635512434 ) ) ;
#30266 = CARTESIAN_POINT ( 'NONE',  ( 104.7042813665017462, 27.49927371769997464, 42.19190249457584940 ) ) ;
#30267 = CARTESIAN_POINT ( 'NONE',  ( -0.9897066053608900571, 7.549089325901769065, 34.51982852159657256 ) ) ;
#30268 = CARTESIAN_POINT ( 'NONE',  ( 63.68918951593933997, 12.82977143588412972, 83.52517258632475716 ) ) ;
#30269 = CARTESIAN_POINT ( 'NONE',  ( 186.0827296088606602, 85.28826835108064586, 15.56026340398669916 ) ) ;
#30270 = LINE ( 'NONE', #37947, #36188 ) ;
#30271 = CARTESIAN_POINT ( 'NONE',  ( 177.0024338932393562, 74.57605685449961186, 16.27244958310170020 ) ) ;
#30272 = CARTESIAN_POINT ( 'NONE',  ( -62.54085973597664605, 16.81797209566546414, 10.48152732957156630 ) ) ;
#30273 = ORIENTED_EDGE ( 'NONE', *, *, #22726, .F. ) ;
#30274 = DIRECTION ( 'NONE',  ( 0.000000000000000000, 0.000000000000000000, 1.000000000000000000 ) ) ;
#30275 = VERTEX_POINT ( 'NONE', #13085 ) ;
#30276 = DIRECTION ( 'NONE',  ( 0.000000000000000000, 0.000000000000000000, -1.000000000000000000 ) ) ;
#30277 = EDGE_CURVE ( 'NONE', #12796, #21766, #43469, .T. ) ;
#30278 = CARTESIAN_POINT ( 'NONE',  ( 46.80475532923159676, 10.50744084852536986, -17.50383325418069091 ) ) ;
#30279 = EDGE_CURVE ( 'NONE', #39717, #55323, #47760, .T. ) ;
#30280 = CARTESIAN_POINT ( 'NONE',  ( -1.666933348991701536, -64.97862212458815634, 170.0000000000000000 ) ) ;
#30281 = CARTESIAN_POINT ( 'NONE',  ( -442.6627218934918915, 394.9999999999998295, -136.4497041420123367 ) ) ;
#30282 = LINE ( 'NONE', #62974, #23268 ) ;
#30283 = CARTESIAN_POINT ( 'NONE',  ( 313.9975424824652350, 18.00000000000002842, 256.6193948016162381 ) ) ;
#30284 = VERTEX_POINT ( 'NONE', #62989 ) ;
#30285 = CARTESIAN_POINT ( 'NONE',  ( -71.16770070143911653, 19.60548673929831764, 64.23797182331117028 ) ) ;
#30286 = CARTESIAN_POINT ( 'NONE',  ( -170.2801941679960294, 84.02053682015862535, 58.21222663911628104 ) ) ;
#30287 = ORIENTED_EDGE ( 'NONE', *, *, #26512, .T. ) ;
#30288 = ORIENTED_EDGE ( 'NONE', *, *, #16250, .T. ) ;
#30289 = CARTESIAN_POINT ( 'NONE',  ( -154.0775378574013814, 68.15437918458553668, 44.18676606056580169 ) ) ;
#30290 = CYLINDRICAL_SURFACE ( 'NONE', #5224, 5.000000000000000000 ) ;
#30291 = CARTESIAN_POINT ( 'NONE',  ( 176.6214367443248250, 74.20967084876664899, -10.83384295640149730 ) ) ;
#30292 = CARTESIAN_POINT ( 'NONE',  ( 105.7953515382196343, 27.97683113100023888, 70.01405529446219589 ) ) ;
#30293 = LINE ( 'NONE', #55987, #62227 ) ;
#30294 = CIRCLE ( 'NONE', #53854, 21.00000000000000355 ) ;
#30295 = CARTESIAN_POINT ( 'NONE',  ( 57.07246224906423748, 12.39953617563784327, -11.77494754054097470 ) ) ;
#30296 = VERTEX_POINT ( 'NONE', #61944 ) ;
#30297 = AXIS2_PLACEMENT_3D ( 'NONE', #52533, #4356, #31429 ) ;
#30298 = CARTESIAN_POINT ( 'NONE',  ( 24.36509522349078338, -70.94296747916756374, 170.0000000000000000 ) ) ;
#30299 = EDGE_LOOP ( 'NONE', ( #27032, #61335 ) ) ;
#30300 = CARTESIAN_POINT ( 'NONE',  ( 22.28556289340099994, 7.803548444155007147, -46.77340716559223210 ) ) ;
#30301 = CARTESIAN_POINT ( 'NONE',  ( 8.478575283864731915, 7.382882227715640511, 66.05570129574820726 ) ) ;
#30302 = CARTESIAN_POINT ( 'NONE',  ( 211.7451286015360665, 116.5372661580811098, 39.29095847353463711 ) ) ;
#30303 = DIRECTION ( 'NONE',  ( -0.000000000000000000, -0.000000000000000000, -1.000000000000000000 ) ) ;
#30304 = ORIENTED_EDGE ( 'NONE', *, *, #21984, .F. ) ;
#30305 = EDGE_LOOP ( 'NONE', ( #56024, #26430, #49452, #27818 ) ) ;
#30306 = CARTESIAN_POINT ( 'NONE',  ( 113.3057637310466532, -21.67663200833031922, -3.765392563550230332 ) ) ;
#30307 = CARTESIAN_POINT ( 'NONE',  ( -132.8211701626061370, 52.46221387263234703, 94.70213310676591334 ) ) ;
#30308 = CARTESIAN_POINT ( 'NONE',  ( 36.77024545412684375, 9.095083943590502429, -76.99170081823220357 ) ) ;
#30309 = LINE ( 'NONE', #40858, #11862 ) ;
#30310 = CARTESIAN_POINT ( 'NONE',  ( 8.452306438776274078, 6.376630025498653431, 89.60986528594584399 ) ) ;
#30311 = AXIS2_PLACEMENT_3D ( 'NONE', #47516, #10931, #16560 ) ;
#30312 = CARTESIAN_POINT ( 'NONE',  ( 85.67138972405896880, 19.09593469918313247, -77.62004818985134591 ) ) ;
#30313 = ORIENTED_EDGE ( 'NONE', *, *, #65850, .F. ) ;
#30314 = CARTESIAN_POINT ( 'NONE',  ( 70.21761529798025947, 26.35311180610075610, 0.000000000000000000 ) ) ;
#30315 = CARTESIAN_POINT ( 'NONE',  ( 197.6329787101074373, 98.74106466892206413, -46.36182222220342197 ) ) ;
#30316 = ORIENTED_EDGE ( 'NONE', *, *, #35755, .T. ) ;
#30317 = CARTESIAN_POINT ( 'NONE',  ( -80.31691774066406708, 22.95709084517032395, 18.39362405332230566 ) ) ;
#30318 = ORIENTED_EDGE ( 'NONE', *, *, #32168, .F. ) ;
#30319 = CARTESIAN_POINT ( 'NONE',  ( -81.00507684688699328, 23.22613445438387103, -62.32995080790337994 ) ) ;
#30320 = CARTESIAN_POINT ( 'NONE',  ( -45.00000000000002132, -20.00000000000000355, 4.000000000000000000 ) ) ;
#30321 = ORIENTED_EDGE ( 'NONE', *, *, #51865, .T. ) ;
#30322 = ORIENTED_EDGE ( 'NONE', *, *, #12242, .F. ) ;
#30323 = CARTESIAN_POINT ( 'NONE',  ( 13.37820144534468625, 6.435512790162277952, -35.91245910506206940 ) ) ;
#30324 = AXIS2_PLACEMENT_3D ( 'NONE', #54733, #53688, #5508 ) ;
#30325 = DIRECTION ( 'NONE',  ( 0.000000000000000000, 0.000000000000000000, 1.000000000000000000 ) ) ;
#30326 = CARTESIAN_POINT ( 'NONE',  ( 19.53470118933707056, 6.649487981843464013, 4.168281182200566981 ) ) ;
#30327 = ORIENTED_EDGE ( 'NONE', *, *, #31131, .F. ) ;
#30328 = ADVANCED_FACE ( 'NONE', ( #66907 ), #8847, .F. ) ;
#30329 = CARTESIAN_POINT ( 'NONE',  ( -23.93384176999330037, 8.479327181248127232, 91.56969707628782373 ) ) ;
#30330 = CARTESIAN_POINT ( 'NONE',  ( 174.4978817191264682, 73.57770570413207167, -74.16780078678564792 ) ) ;
#30331 = EDGE_CURVE ( 'NONE', #51505, #18983, #46113, .T. ) ;
#30332 = CARTESIAN_POINT ( 'NONE',  ( -126.8016613879753862, 48.30316697011515004, -8.110637278710640885 ) ) ;
#30333 = CARTESIAN_POINT ( 'NONE',  ( 103.0103829243729194, 25.67737053862328267, -41.37271453292686374 ) ) ;
#30334 = DIRECTION ( 'NONE',  ( -0.000000000000000000, 1.000000000000000000, -0.000000000000000000 ) ) ;
#30335 = CARTESIAN_POINT ( 'NONE',  ( -165.9719475799887221, 80.94902045251464529, -93.61803425850247606 ) ) ;
#30336 = VERTEX_POINT ( 'NONE', #29588 ) ;
#30337 = EDGE_CURVE ( 'NONE', #8207, #29750, #25583, .T. ) ;
#30338 = CIRCLE ( 'NONE', #59490, 30.00000000000000000 ) ;
#30339 = VERTEX_POINT ( 'NONE', #40842 ) ;
#30340 = CARTESIAN_POINT ( 'NONE',  ( -80.32755469740935439, 24.04130076192507204, -62.14234554664773214 ) ) ;
#30341 = CARTESIAN_POINT ( 'NONE',  ( -0.4996266546846072631, 6.524616273922395848, -95.00000000000133582 ) ) ;
#30342 = DIRECTION ( 'NONE',  ( 0.7071067811865475727, -0.7071067811865475727, -3.925231146709437301E-16 ) ) ;
#30343 = LINE ( 'NONE', #36657, #19793 ) ;
#30344 = CARTESIAN_POINT ( 'NONE',  ( 126.9201538765324386, 37.39093565120715112, 13.02954706411735053 ) ) ;
#30345 = CARTESIAN_POINT ( 'NONE',  ( 10.55634918610396511, -41.66904755831214402, 2.000000000000001776 ) ) ;
#30346 = CARTESIAN_POINT ( 'NONE',  ( 210.8246821066057635, 116.9679728619736210, 94.73533617371974458 ) ) ;
#30347 = CARTESIAN_POINT ( 'NONE',  ( -447.6627218934914367, 399.9999999999998863, -116.4497041420118393 ) ) ;
#30348 = DIRECTION ( 'NONE',  ( 0.000000000000000000, 1.000000000000000000, -0.000000000000000000 ) ) ;
#30349 = DIRECTION ( 'NONE',  ( -0.9749279121818259508, 0.2225209339563042066, 5.102127870520021228E-18 ) ) ;
#30350 = EDGE_LOOP ( 'NONE', ( #66710, #25128 ) ) ;
#30351 = CARTESIAN_POINT ( 'NONE',  ( 8.337549025192451779, 7.382630697225775585, -17.16211394505371146 ) ) ;
#30352 = VERTEX_POINT ( 'NONE', #14796 ) ;
#30353 = CARTESIAN_POINT ( 'NONE',  ( 203.1511228994173734, 104.2426341584999534, -24.36617736913426668 ) ) ;
#30354 = VERTEX_POINT ( 'NONE', #56328 ) ;
#30355 = EDGE_CURVE ( 'NONE', #31287, #28498, #64453, .T. ) ;
#30356 = CARTESIAN_POINT ( 'NONE',  ( 0.000000000000000000, 0.000000000000000000, 40.00000000000003553 ) ) ;
#30357 = CARTESIAN_POINT ( 'NONE',  ( 187.2384682876461852, 86.54721710842891014, -66.25374784196327482 ) ) ;
#30358 = DIRECTION ( 'NONE',  ( 1.000000000000000000, 1.387778780781445676E-16, 0.000000000000000000 ) ) ;
#30359 = CARTESIAN_POINT ( 'NONE',  ( 65.40032188136231639, 13.23841673691966214, -23.49107392329795019 ) ) ;
#30360 = VECTOR ( 'NONE', #54096, 1000.000000000000114 ) ;
#30361 = CARTESIAN_POINT ( 'NONE',  ( -31.43908319763709969, 10.61114334766715572, 3.371903815725488585 ) ) ;
#30362 = CARTESIAN_POINT ( 'NONE',  ( -107.0751323097254470, 35.28386110859231195, 5.386659267684521524 ) ) ;
#30363 = CARTESIAN_POINT ( 'NONE',  ( 9.819093282782489496, 7.389085782749408970, -38.45181758483611389 ) ) ;
#30364 = DIRECTION ( 'NONE',  ( 0.000000000000000000, 1.000000000000000000, -0.000000000000000000 ) ) ;
#30365 = VERTEX_POINT ( 'NONE', #62299 ) ;
#30366 = ORIENTED_EDGE ( 'NONE', *, *, #1920, .T. ) ;
#30367 = CARTESIAN_POINT ( 'NONE',  ( -7.486743542470078339, 64.58150799671128084, 170.0000000000000000 ) ) ;
#30368 = CYLINDRICAL_SURFACE ( 'NONE', #13925, 65.00000000000000000 ) ;
#30369 = CARTESIAN_POINT ( 'NONE',  ( -78.66644367742111399, 23.39876645725285798, 18.57365054920947500 ) ) ;
#30370 = UNCERTAINTY_MEASURE_WITH_UNIT (LENGTH_MEASURE( 1.000000000000000082E-05 ), #20501, 'distance_accuracy_value', 'NONE');
#30371 = AXIS2_PLACEMENT_3D ( 'NONE', #28987, #45143, #44088 ) ;
#30372 = CARTESIAN_POINT ( 'NONE',  ( 9.058156535714477542, 6.378495712187264743, 7.351094015256990133 ) ) ;
#30373 = FACE_OUTER_BOUND ( 'NONE', #49893, .T. ) ;
#30374 = CARTESIAN_POINT ( 'NONE',  ( 24.91130694661013578, 3.250319586706704733, 0.000000000000000000 ) ) ;
#30375 = FACE_OUTER_BOUND ( 'NONE', #49876, .T. ) ;
#30376 = CARTESIAN_POINT ( 'NONE',  ( -177.5271152834790769, 92.16916858125013334, -36.12493601448592528 ) ) ;
#30377 = CARTESIAN_POINT ( 'NONE',  ( 90.91465859190766707, 20.92790537681857188, -22.63697861787248655 ) ) ;
#30378 = DIRECTION ( 'NONE',  ( 0.000000000000000000, 0.000000000000000000, 1.000000000000000000 ) ) ;
#30379 = CARTESIAN_POINT ( 'NONE',  ( 107.4922189950060982, 21.56887920590508045, 4.337924292484288458 ) ) ;
#30380 = CARTESIAN_POINT ( 'NONE',  ( -54.08504625707234226, 14.42374043447187226, 72.11508717042879368 ) ) ;
#30381 = CARTESIAN_POINT ( 'NONE',  ( -0.3249717932738297455, 6.518578686837482650, 64.94829995873614337 ) ) ;
#30382 = ORIENTED_EDGE ( 'NONE', *, *, #51150, .T. ) ;
#30383 = DIRECTION ( 'NONE',  ( 1.000000000000000000, 0.000000000000000000, 0.000000000000000000 ) ) ;
#30384 = CARTESIAN_POINT ( 'NONE',  ( 44.01696072965949469, 47.84694004974210912, 170.0000000000000000 ) ) ;
#30385 = DIRECTION ( 'NONE',  ( 0.000000000000000000, 0.000000000000000000, 1.000000000000000000 ) ) ;
#30386 = CYLINDRICAL_SURFACE ( 'NONE', #44199, 7.500000000000013323 ) ;
#30387 = FACE_OUTER_BOUND ( 'NONE', #27352, .T. ) ;
#30388 = CONICAL_SURFACE ( 'NONE', #47191, 2.999999999999981792, 0.7853981633974482790 ) ;
#30389 = CARTESIAN_POINT ( 'NONE',  ( -1.298947065946361112, 7.560777410219321482, 94.99999999999866418 ) ) ;
#30390 = ADVANCED_FACE ( 'NONE', ( #3222 ), #36259, .T. ) ;
#30391 = ORIENTED_EDGE ( 'NONE', *, *, #2926, .F. ) ;
#30392 = LINE ( 'NONE', #56089, #10051 ) ;
#30393 = CARTESIAN_POINT ( 'NONE',  ( 209.9999999999999716, 0.000000000000000000, 93.99999999999998579 ) ) ;
#30394 = ORIENTED_EDGE ( 'NONE', *, *, #9484, .T. ) ;
#30395 = EDGE_LOOP ( 'NONE', ( #29540, #42443, #39081 ) ) ;
#30396 = CARTESIAN_POINT ( 'NONE',  ( -7.825402957745085430, 6.891034867348153625, -89.10717191287116634 ) ) ;
#30397 = CARTESIAN_POINT ( 'NONE',  ( -173.9548930713590948, 88.06040582145362805, -76.52175617720489242 ) ) ;
#30398 = CARTESIAN_POINT ( 'NONE',  ( -4.999999999999922728, 46.66904755831208718, 0.000000000000000000 ) ) ;
#30399 = ORIENTED_EDGE ( 'NONE', *, *, #55850, .F. ) ;
#30400 = CARTESIAN_POINT ( 'NONE',  ( -27.00000000000000355, -27.00000000000000355, 12.00000000000000000 ) ) ;
#30401 = DIRECTION ( 'NONE',  ( 0.9639628606958512425, 0.2660368455666826670, -0.000000000000000000 ) ) ;
#30402 = DIRECTION ( 'NONE',  ( -0.000000000000000000, 0.000000000000000000, 1.000000000000000000 ) ) ;
#30403 = VECTOR ( 'NONE', #55875, 1000.000000000000114 ) ;
#30404 = CARTESIAN_POINT ( 'NONE',  ( 60.40531521312255592, 13.11276739283242243, -50.25594387449618949 ) ) ;
#30405 = CARTESIAN_POINT ( 'NONE',  ( -84.55783695959762269, 25.74181993349145259, 42.58591016297526721 ) ) ;
#30406 = CARTESIAN_POINT ( 'NONE',  ( -29.50439180771547143, 10.29976981300626981, -23.23516915157700069 ) ) ;
#30407 = CARTESIAN_POINT ( 'NONE',  ( 135.6842057900327063, 42.53841116629840258, 17.45434489297113956 ) ) ;
#30408 = EDGE_CURVE ( 'NONE', #19323, #58514, #41537, .T. ) ;
#30409 = PRODUCT_DEFINITION_SHAPE ( 'NONE', 'NONE',  #54682 ) ;
#30410 = ORIENTED_EDGE ( 'NONE', *, *, #44466, .T. ) ;
#30411 = EDGE_CURVE ( 'NONE', #35197, #10115, #38411, .T. ) ;
#30412 = DIRECTION ( 'NONE',  ( 0.000000000000000000, -0.000000000000000000, -1.000000000000000000 ) ) ;
#30413 = CARTESIAN_POINT ( 'NONE',  ( 11.21653854975268771, 6.397128675385707730, 70.32495166433241707 ) ) ;
#30414 = FACE_OUTER_BOUND ( 'NONE', #20517, .T. ) ;
#30415 = DIRECTION ( 'NONE',  ( 9.729521452151193035E-15, -5.551115123116034723E-17, 1.000000000000000000 ) ) ;
#30417 = ORIENTED_EDGE ( 'NONE', *, *, #32310, .F. ) ;
#30416 = DIRECTION ( 'NONE',  ( 0.000000000000000000, 0.000000000000000000, 1.000000000000000000 ) ) ;
#30418 = CYLINDRICAL_SURFACE ( 'NONE', #57753, 7.500000000000020428 ) ;
#30419 = VERTEX_POINT ( 'NONE', #46810 ) ;
#30420 = EDGE_CURVE ( 'NONE', #40175, #48508, #8496, .T. ) ;
#30421 = CIRCLE ( 'NONE', #10169, 20.30000000000000071 ) ;
#30422 = ORIENTED_EDGE ( 'NONE', *, *, #40565, .T. ) ;
#30423 = B_SPLINE_CURVE_WITH_KNOTS ( 'NONE', 3,
 ( #42109, #58618, #53334, #10433, #48388, #5165, #10099, #21681, #64253, #52992, #21337, #37867, #32592, #41768, #4813, #37514, #37171, #15379, #20648, #224, #5845, #15033, #53687, #47370, #31554, #69177, #68825, #36491, #42784, #31903, #63567, #43130, #31224, #63908, #57942, #59315, #26961, #42451, #26627, #9762, #48062, #52655, #26281, #36839, #4480 ),
 .UNSPECIFIED., .F., .F.,
 ( 4, 2, 2, 2, 2, 2, 2, 2, 2, 2, 2, 1, 2, 2, 2, 2, 2, 2, 2, 2, 2, 2, 4 ),
 ( 1.430489624538199204E-17, 0.001502898956853375738, 0.002254348435280052656, 0.003005797913706729791, 0.004508696870560122659, 0.005260146348986836223, 0.006011595827413550655, 0.007514494784266991662, 0.009017393741120432668, 0.01052029269797387367, 0.01127174217640060198, 0.01202319165482733029, 0.01277464113325405687, 0.01352609061168078171, 0.01502898956853423486, 0.01578043904696096317, 0.01653188852538768974, 0.01803478748224114289, 0.01953768643909459257, 0.02028913591752131915, 0.02104058539594804572, 0.02254348435280153704, 0.02404638330965502488 ),
 .UNSPECIFIED. ) ;
#30424 = CARTESIAN_POINT ( 'NONE',  ( -147.3614567344829140, 62.37986555269946365, 72.26553695328843219 ) ) ;
#30425 = DIRECTION ( 'NONE',  ( -0.000000000000000000, 0.000000000000000000, 1.000000000000000000 ) ) ;
#30426 = CARTESIAN_POINT ( 'NONE',  ( 198.3926538463959162, 98.07933330386025261, -66.56970357492031098 ) ) ;
#30427 = CARTESIAN_POINT ( 'NONE',  ( 188.4937788906149763, 86.43336847120866651, -15.68169198850661417 ) ) ;
#30428 = DIRECTION ( 'NONE',  ( 0.000000000000000000, 0.000000000000000000, 1.000000000000000000 ) ) ;
#30429 = CARTESIAN_POINT ( 'NONE',  ( 46.66904755831207297, -10.55634918610412853, 2.000000000000001776 ) ) ;
#30430 = DIRECTION ( 'NONE',  ( -0.000000000000000000, -0.000000000000000000, 1.000000000000000000 ) ) ;
#30431 = CARTESIAN_POINT ( 'NONE',  ( -48.70883077256304006, 14.10659259062419046, 33.80919071426065869 ) ) ;
#30432 = ORIENTED_EDGE ( 'NONE', *, *, #17637, .T. ) ;
#30433 = ORIENTED_EDGE ( 'NONE', *, *, #52765, .F. ) ;
#30434 = EDGE_CURVE ( 'NONE', #33041, #4538, #19732, .T. ) ;
#30435 = CARTESIAN_POINT ( 'NONE',  ( -108.0902552660050588, 36.97681740369922920, 6.405841544879333327 ) ) ;
#30436 = CARTESIAN_POINT ( 'NONE',  ( 109.3047266816501093, 28.44977739115299187, 56.49988189436563601 ) ) ;
#30437 = CARTESIAN_POINT ( 'NONE',  ( 102.7610798044536438, 25.57191189614546190, 91.42850727331421012 ) ) ;
#30439 = EDGE_CURVE ( 'NONE', #65355, #9149, #25023, .T. ) ;
#30438 = CYLINDRICAL_SURFACE ( 'NONE', #3781, 7.500000000000013323 ) ;
#30440 = EDGE_CURVE ( 'NONE', #53534, #23514, #18702, .T. ) ;
#30441 = CARTESIAN_POINT ( 'NONE',  ( 30.12852347772543027, 100.0000000000000000, 73.58025477438755502 ) ) ;
#30442 = DIRECTION ( 'NONE',  ( -1.000000000000000000, -0.000000000000000000, -0.000000000000000000 ) ) ;
#30443 = CARTESIAN_POINT ( 'NONE',  ( -144.0382967194035473, 60.96512050924604864, 86.73872642800570532 ) ) ;
#30444 = VERTEX_POINT ( 'NONE', #29947 ) ;
#30445 = VERTEX_POINT ( 'NONE', #62654 ) ;
#30446 = ORIENTED_EDGE ( 'NONE', *, *, #67432, .F. ) ;
#30447 = LINE ( 'NONE', #4741, #7197 ) ;
#30448 = CARTESIAN_POINT ( 'NONE',  ( 0.000000000000000000, 0.000000000000000000, 43.58025477438756212 ) ) ;
#30449 = CARTESIAN_POINT ( 'NONE',  ( 67.92995549349548412, 13.86623459444478534, -48.90726067449875103 ) ) ;
#30450 = CARTESIAN_POINT ( 'NONE',  ( 105.6635180218176231, -21.85802590693743852, 2.510273771313294322 ) ) ;
#30451 = LINE ( 'NONE', #61258, #50277 ) ;
#30452 = VECTOR ( 'NONE', #12448, 1000.000000000000000 ) ;
#30453 = CARTESIAN_POINT ( 'NONE',  ( -38.69449158134470679, 11.92067517118075237, -71.62430901259223504 ) ) ;
#30454 = CARTESIAN_POINT ( 'NONE',  ( 31.96227686234408338, 7.558148489540042370, 63.27730136333553901 ) ) ;
#30455 = CARTESIAN_POINT ( 'NONE',  ( 15.29899606819416569, 6.485153354884285903, -23.67439350822213839 ) ) ;
#30456 = VECTOR ( 'NONE', #51928, 1000.000000000000000 ) ;
#30457 = EDGE_LOOP ( 'NONE', ( #64606, #50999 ) ) ;
#30458 = CARTESIAN_POINT ( 'NONE',  ( 23.17627457812085723, 71.32923872213659422, 43.58025477438756212 ) ) ;
#30459 = DIRECTION ( 'NONE',  ( 0.000000000000000000, 0.000000000000000000, 1.000000000000000000 ) ) ;
#30460 = LINE ( 'NONE', #14625, #61231 ) ;
#30461 = CARTESIAN_POINT ( 'NONE',  ( 66.08620257826612487, 13.40585338179126751, -63.21833551195629752 ) ) ;
#30462 = CARTESIAN_POINT ( 'NONE',  ( 16.76400266940279948, 6.533513613209219528, 56.90669568735162898 ) ) ;
#30463 = CARTESIAN_POINT ( 'NONE',  ( 22.89270809252618477, 7.840160460323052583, -13.75834395622513462 ) ) ;
#30464 = CARTESIAN_POINT ( 'NONE',  ( 8.287863202055541834, 7.382585476140733682, 11.15840143617041669 ) ) ;
#30465 = VECTOR ( 'NONE', #39016, 1000.000000000000000 ) ;
#30466 = AXIS2_PLACEMENT_3D ( 'NONE', #22439, #33706, #60063 ) ;
#30467 = ORIENTED_EDGE ( 'NONE', *, *, #37316, .T. ) ;
#30468 = SHAPE_DEFINITION_REPRESENTATION ( #47266, #35767 ) ;
#30469 = VECTOR ( 'NONE', #16568, 1000.000000000000000 ) ;
#30470 = DIRECTION ( 'NONE',  ( -0.9510565162951545304, 0.3090169943749447312, 2.500042656554810833E-16 ) ) ;
#30471 = CARTESIAN_POINT ( 'NONE',  ( -58.00979178563854077, 29.32343869649098878, 170.0000000000000000 ) ) ;
#30472 = LINE ( 'NONE', #34381, #18845 ) ;
#30473 = CARTESIAN_POINT ( 'NONE',  ( 188.0103583326377645, 87.39896620268123684, -40.83424593798813618 ) ) ;
#30474 = EDGE_LOOP ( 'NONE', ( #48864, #17604, #38930, #5085 ) ) ;
#30475 = EDGE_CURVE ( 'NONE', #58133, #3625, #45761, .T. ) ;
#30476 = ORIENTED_EDGE ( 'NONE', *, *, #12104, .T. ) ;
#30477 = DIRECTION ( 'NONE',  ( -0.000000000000000000, 0.000000000000000000, 1.000000000000000000 ) ) ;
#30478 = CARTESIAN_POINT ( 'NONE',  ( -17.50000000000002842, -18.06806526123148160, -2.000000000000000000 ) ) ;
#30479 = ORIENTED_EDGE ( 'NONE', *, *, #26575, .F. ) ;
#30480 = EDGE_CURVE ( 'NONE', #36510, #34701, #35919, .T. ) ;
#30481 = CARTESIAN_POINT ( 'NONE',  ( 164.7662527831195973, 64.87053726845202561, 88.85073695511873382 ) ) ;
#30482 = EDGE_LOOP ( 'NONE', ( #35492, #62858 ) ) ;
#30483 = CARTESIAN_POINT ( 'NONE',  ( 133.8566784816069344, 42.60093787723652525, -77.86786152285937135 ) ) ;
#30484 = CARTESIAN_POINT ( 'NONE',  ( 132.0582325211145189, 40.34869848118183455, 44.30557495754532482 ) ) ;
#30485 = CARTESIAN_POINT ( 'NONE',  ( -156.8773151811562343, 72.06122063279306644, 39.64036288611060854 ) ) ;
#30486 = CARTESIAN_POINT ( 'NONE',  ( -95.21430597939259144, 29.33390900154322267, 35.45363162692691361 ) ) ;
#30487 = DIRECTION ( 'NONE',  ( -0.8118923937861950435, -0.5838071093367415143, 0.000000000000000000 ) ) ;
#30489 = ORIENTED_EDGE ( 'NONE', *, *, #27685, .F. ) ;
#30488 = DIRECTION ( 'NONE',  ( 1.000000000000000000, 1.024558601614476894E-14, -9.899298618516476860E-15 ) ) ;
#30490 = EDGE_CURVE ( 'NONE', #17838, #18889, #3084, .T. ) ;
#30491 = FACE_OUTER_BOUND ( 'NONE', #65876, .T. ) ;
#30492 = VERTEX_POINT ( 'NONE', #48507 ) ;
#30494 = ORIENTED_EDGE ( 'NONE', *, *, #6840, .T. ) ;
#30493 = EDGE_CURVE ( 'NONE', #30352, #46155, #59424, .T. ) ;
#30495 = CARTESIAN_POINT ( 'NONE',  ( 177.0027897064244371, 75.97676392242540544, 43.11708354611123895 ) ) ;
#30496 = CARTESIAN_POINT ( 'NONE',  ( 16.78635691501517613, 6.000000000000000000, -36.68900338898716740 ) ) ;
#30497 = EDGE_CURVE ( 'NONE', #4217, #62345, #23365, .T. ) ;
#30499 = EDGE_LOOP ( 'NONE', ( #64703, #52601 ) ) ;
#30498 = CARTESIAN_POINT ( 'NONE',  ( 15.78827728214693416, -170.0000000000000000, -43.01894409868580027 ) ) ;
#30500 = DIRECTION ( 'NONE',  ( -1.000000000000000000, 0.000000000000000000, 1.156482317317871478E-16 ) ) ;
#30501 = VECTOR ( 'NONE', #20085, 1000.000000000000000 ) ;
#30502 = DIRECTION ( 'NONE',  ( 0.000000000000000000, 0.000000000000000000, 1.000000000000000000 ) ) ;
#30503 = EDGE_LOOP ( 'NONE', ( #11628, #5798, #59529, #57656 ) ) ;
#30504 = AXIS2_PLACEMENT_3D ( 'NONE', #35777, #56524, #30487 ) ;
#30505 = CARTESIAN_POINT ( 'NONE',  ( -61.86845765289631061, 16.61548683002699889, -19.01154453034531500 ) ) ;
#30506 = AXIS2_PLACEMENT_3D ( 'NONE', #20375, #3866, #41154 ) ;
#30507 = CARTESIAN_POINT ( 'NONE',  ( 135.6793972494603224, 43.71805072851431362, 29.72064904164495758 ) ) ;
#30508 = CARTESIAN_POINT ( 'NONE',  ( 117.6853163455684665, 33.60747889659833021, 38.17223689839699574 ) ) ;
#30509 = CARTESIAN_POINT ( 'NONE',  ( -132.6092625803567557, 52.31125232006264270, 14.62512562566566565 ) ) ;
#30510 = CARTESIAN_POINT ( 'NONE',  ( 64.93224207568368911, 14.16036304753835218, -62.81019525340659726 ) ) ;
#30511 = B_SPLINE_CURVE_WITH_KNOTS ( 'NONE', 3,
 ( #39788, #50683, #49629, #45764, #17992, #23276 ),
 .UNSPECIFIED., .F., .F.,
 ( 4, 2, 4 ),
 ( 2.380731629548242913E-07, 0.002336973833157547729, 0.004673709593152140102 ),
 .UNSPECIFIED. ) ;
#30512 = ORIENTED_EDGE ( 'NONE', *, *, #44296, .F. ) ;
#30513 = ORIENTED_EDGE ( 'NONE', *, *, #46788, .F. ) ;
#30514 = CARTESIAN_POINT ( 'NONE',  ( 12.52293991431295872, 7.423284696525648485, -89.90348070406828640 ) ) ;
#30515 =( GEOMETRIC_REPRESENTATION_CONTEXT ( 3 ) GLOBAL_UNCERTAINTY_ASSIGNED_CONTEXT ( ( #19821 ) ) GLOBAL_UNIT_ASSIGNED_CONTEXT ( ( #69363, #31393, #31729 ) ) REPRESENTATION_CONTEXT ( 'NONE', 'WORKASPACE' ) );
#30516 = CARTESIAN_POINT ( 'NONE',  ( -172.7154982671752350, 86.67743928531949393, -49.71195716475002513 ) ) ;
#30518 = EDGE_CURVE ( 'NONE', #54796, #27634, #4235, .T. ) ;
#30517 = DIRECTION ( 'NONE',  ( 0.000000000000000000, 1.000000000000000000, -0.000000000000000000 ) ) ;
#30519 = EDGE_CURVE ( 'NONE', #31875, #62112, #36951, .T. ) ;
#30520 = CARTESIAN_POINT ( 'NONE',  ( -53.98930025855998593, 14.39893220427481069, -88.97817567444977271 ) ) ;
#30521 = DIRECTION ( 'NONE',  ( 0.000000000000000000, 0.000000000000000000, -1.000000000000000000 ) ) ;
#30522 = DIRECTION ( 'NONE',  ( -0.000000000000000000, -1.000000000000000000, -0.000000000000000000 ) ) ;
#30523 = EDGE_CURVE ( 'NONE', #21329, #50834, #21451, .T. ) ;
#30524 = CARTESIAN_POINT ( 'NONE',  ( 69.83617901654355364, 15.39919709983074547, -46.34986266313208603 ) ) ;
#30525 = DIRECTION ( 'NONE',  ( -1.000000000000000000, 2.279101714840934323E-64, -7.703719777548945123E-34 ) ) ;
#30526 = CARTESIAN_POINT ( 'NONE',  ( -165.9111709580270428, 79.44576090485631426, -66.96989664920324969 ) ) ;
#30527 = ORIENTED_EDGE ( 'NONE', *, *, #60421, .F. ) ;
#30528 = CARTESIAN_POINT ( 'NONE',  ( -102.7494334820056849, 34.14986869751098908, 45.51907450641513009 ) ) ;
#30529 = VERTEX_POINT ( 'NONE', #27069 ) ;
#30530 = CARTESIAN_POINT ( 'NONE',  ( 16.78635691501517613, 6.000000000000000000, -4.435653166495499455 ) ) ;
#30531 = CARTESIAN_POINT ( 'NONE',  ( 85.67165909753197184, 20.15791549876376010, 71.51084241816450060 ) ) ;
#30532 = EDGE_LOOP ( 'NONE', ( #51321, #31893, #65972, #26174 ) ) ;
#30533 = CARTESIAN_POINT ( 'NONE',  ( -80.76833728594722572, 23.13302944128081151, -89.09247661525495232 ) ) ;
#30534 = CARTESIAN_POINT ( 'NONE',  ( 69.68177367721139603, 20.52767805628179332, 170.0000000000000000 ) ) ;
#30535 = FACE_OUTER_BOUND ( 'NONE', #52998, .T. ) ;
#30536 = FACE_OUTER_BOUND ( 'NONE', #10870, .T. ) ;
#30537 = CARTESIAN_POINT ( 'NONE',  ( 31.91375106836930087, 7.553354707452900385, 10.08129055534168117 ) ) ;
#30538 = CARTESIAN_POINT ( 'NONE',  ( -15.13464256769235838, 8.488509377255649468, -41.21959027930886066 ) ) ;
#30539 = CARTESIAN_POINT ( 'NONE',  ( -137.3060924980642596, 138.4631249211268482, 10.00000000000000000 ) ) ;
#30540 = ORIENTED_EDGE ( 'NONE', *, *, #33035, .T. ) ;
#30541 = CARTESIAN_POINT ( 'NONE',  ( -15.55634918610403439, 5.000000000000028422, 2.000000000000001776 ) ) ;
#30542 = ORIENTED_EDGE ( 'NONE', *, *, #53551, .F. ) ;
#30543 = CARTESIAN_POINT ( 'NONE',  ( -57.43251939610646417, 15.33203492375496957, 30.68838339410472926 ) ) ;
#30544 = CARTESIAN_POINT ( 'NONE',  ( -56.97556689808916275, 16.24958672959845174, 71.91524354625708781 ) ) ;
#30545 = CARTESIAN_POINT ( 'NONE',  ( -23.95096213915837069, 8.481591526885942756, 11.36064944404291843 ) ) ;
#30546 = CYLINDRICAL_SURFACE ( 'NONE', #29988, 5.000000000000000000 ) ;
#30547 = CARTESIAN_POINT ( 'NONE',  ( -60.99549137429562506, 16.35576463946026493, -91.82486495769101964 ) ) ;
#30548 = CARTESIAN_POINT ( 'NONE',  ( 19.25636636730773077, 33.14646320116730749, 13.32819397642333392 ) ) ;
#30549 = CARTESIAN_POINT ( 'NONE',  ( 151.3136733342016953, 54.26417151662140270, -39.33353844295554325 ) ) ;
#30550 =( REPRESENTATION_RELATIONSHIP ('NONE','NONE', #40274, #50551 ) REPRESENTATION_RELATIONSHIP_WITH_TRANSFORMATION ( #64638 )SHAPE_REPRESENTATION_RELATIONSHIP( ) );
#30551 = ORIENTED_EDGE ( 'NONE', *, *, #43748, .T. ) ;
#30552 = AXIS2_PLACEMENT_3D ( 'NONE', #28209, #17671, #66228 ) ;
#30553 = DIRECTION ( 'NONE',  ( 4.649058915617843013E-16, 4.266095933352168554E-15, -1.000000000000000000 ) ) ;
#30555 = EDGE_CURVE ( 'NONE', #2845, #56665, #697, .T. ) ;
#30554 = FACE_OUTER_BOUND ( 'NONE', #46917, .T. ) ;
#30556 = DIRECTION ( 'NONE',  ( 1.000000000000000000, 0.000000000000000000, 0.000000000000000000 ) ) ;
#30557 = CARTESIAN_POINT ( 'NONE',  ( -124.1094910780272471, 45.33021696310841975, 30.83172109347568579 ) ) ;
#30558 = CARTESIAN_POINT ( 'NONE',  ( -55.53469534616545644, 14.81076603075803710, -50.21632399845988459 ) ) ;
#30559 = ORIENTED_EDGE ( 'NONE', *, *, #62279, .T. ) ;
#30560 = CARTESIAN_POINT ( 'NONE',  ( -180.4614954900547730, 97.28277348252827039, -70.62524901975936586 ) ) ;
#30561 = AXIS2_PLACEMENT_3D ( 'NONE', #6617, #48805, #49504 ) ;
#30562 = CARTESIAN_POINT ( 'NONE',  ( 126.5464880001513137, 38.33492781348540746, 92.41540379265920535 ) ) ;
#30563 = PRODUCT ( 'stand', 'stand', '', ( #31176 ) ) ;
#30564 = CARTESIAN_POINT ( 'NONE',  ( 115.7561705820728974, 31.51689401996057072, 32.00340604943662015 ) ) ;
#30565 = AXIS2_PLACEMENT_3D ( 'NONE', #25511, #31463, #37416 ) ;
#30567 = AXIS2_PLACEMENT_3D ( 'NONE', #42562, #20079, #37272 ) ;
#30566 = CARTESIAN_POINT ( 'NONE',  ( -125.8938041572051389, -170.0000000000000000, -61.75825448869760237 ) ) ;
#30568 = ADVANCED_FACE ( 'NONE', ( #17923 ), #22149, .F. ) ;
#30569 = DIRECTION ( 'NONE',  ( -0.4338837391175656699, 0.9009688679024155933, 0.000000000000000000 ) ) ;
#30570 = AXIS2_PLACEMENT_3D ( 'NONE', #1420, #22878, #43621 ) ;
#30571 = VERTEX_POINT ( 'NONE', #6314 ) ;
#30572 = CARTESIAN_POINT ( 'NONE',  ( 111.9975424824652634, 172.0000000000000284, 527.9060149868646477 ) ) ;
#30573 = CARTESIAN_POINT ( 'NONE',  ( 117.7411475730015553, 32.50808475802732289, -70.80961951247346065 ) ) ;
#30574 = CARTESIAN_POINT ( 'NONE',  ( 187.0788993276711949, 86.37277723143235164, 32.29480605614903510 ) ) ;
#30575 = CARTESIAN_POINT ( 'NONE',  ( 140.2058232509808988, 46.59155168125934665, 14.18931278570159016 ) ) ;
#30576 = DIRECTION ( 'NONE',  ( 0.000000000000000000, 0.000000000000000000, 1.000000000000000000 ) ) ;
#30577 = CLOSED_SHELL ( 'NONE', ( #29072, #65700, #6915, #67215, #7562, #53173 ) ) ;
#30578 = ORIENTED_EDGE ( 'NONE', *, *, #22559, .T. ) ;
#30579 = EDGE_CURVE ( 'NONE', #25409, #8739, #49917, .T. ) ;
#30580 = DIRECTION ( 'NONE',  ( -0.8160245890732938934, -0.5780171883497599028, 0.000000000000000000 ) ) ;
#30581 = VERTEX_POINT ( 'NONE', #66135 ) ;
#30582 = CARTESIAN_POINT ( 'NONE',  ( -30.00000000000000355, -30.00000000000000355, 0.000000000000000000 ) ) ;
#30583 = CARTESIAN_POINT ( 'NONE',  ( 141.1678131691836029, 46.01782037724119334, 89.01741585174310956 ) ) ;
#30584 = ADVANCED_FACE ( 'NONE', ( #23209 ), #60480, .T. ) ;
#30585 = EDGE_CURVE ( 'NONE', #18908, #28859, #12649, .T. ) ;
#30587 = VERTEX_POINT ( 'NONE', #34108 ) ;
#30586 = DIRECTION ( 'NONE',  ( 0.000000000000000000, 0.000000000000000000, 1.000000000000000000 ) ) ;
#30588 = CARTESIAN_POINT ( 'NONE',  ( -178.5790738944854184, 93.41591512785082330, 43.47135350925507424 ) ) ;
#30589 = DIRECTION ( 'NONE',  ( 1.000000000000000000, 0.000000000000000000, -0.000000000000000000 ) ) ;
#30590 = ADVANCED_FACE ( 'NONE', ( #44659 ), #44288, .F. ) ;
#30591 = CARTESIAN_POINT ( 'NONE',  ( 0.000000000000000000, 0.000000000000000000, 41.38025477438755928 ) ) ;
#30592 = ORIENTED_EDGE ( 'NONE', *, *, #59225, .T. ) ;
#30593 = LINE ( 'NONE', #20721, #7525 ) ;
#30594 = CARTESIAN_POINT ( 'NONE',  ( -102.2801239173131194, -170.0000000000000000, -88.70367844590326456 ) ) ;
#30595 = CARTESIAN_POINT ( 'NONE',  ( 156.0367587612848013, 57.81183863259477818, -89.91473147631771212 ) ) ;
#30596 = LINE ( 'NONE', #3863, #42081 ) ;
#30597 = CARTESIAN_POINT ( 'NONE',  ( -178.2961695431413034, 94.64580896714811331, -90.45313625092560983 ) ) ;
#30598 = CARTESIAN_POINT ( 'NONE',  ( 150.2076397309211870, 52.21780102759851871, 61.86243719087420345 ) ) ;
#30599 = CARTESIAN_POINT ( 'NONE',  ( 94.14197848494937659, 23.19876128416614947, 37.22230832254705746 ) ) ;
#30600 = ORIENTED_EDGE ( 'NONE', *, *, #8624, .F. ) ;
#30601 = CARTESIAN_POINT ( 'NONE',  ( 0.000000000000000000, 70.00000000000000000, 0.000000000000000000 ) ) ;
#30602 = CARTESIAN_POINT ( 'NONE',  ( 0.000000000000000000, 0.000000000000000000, 40.00000000000003553 ) ) ;
#30603 = EDGE_LOOP ( 'NONE', ( #16923, #18250, #16963, #30433 ) ) ;
#30604 = AXIS2_PLACEMENT_3D ( 'NONE', #29880, #62587, #41475 ) ;
#30605 = CARTESIAN_POINT ( 'NONE',  ( 150.2060369882285613, 53.45752899907543565, -14.89401360268165497 ) ) ;
#30606 = CARTESIAN_POINT ( 'NONE',  ( -52.58932868456671628, 14.03406530728571866, 84.39402770761704176 ) ) ;
#30607 = CARTESIAN_POINT ( 'NONE',  ( 107.9342863085848165, 28.93180871323605174, 29.95979435419317127 ) ) ;
#30608 = VECTOR ( 'NONE', #64666, 999.9999999999998863 ) ;
#30609 = B_SPLINE_CURVE_WITH_KNOTS ( 'NONE', 3,
 ( #39669, #34752, #56188, #61124, #39327, #40360, #8004, #34412, #40698, #50919, #2733, #12594, #30166, #45986, #45643, #61808, #7322, #35085, #56537, #29813, #51275, #3087, #19244, #51615, #24884, #46321, #60769, #19596, #14331, #57587, #25236, #30854, #4798, #3766, #69159, #58261, #5144, #41746, #52971, #20287, #15361, #62863, #9395, #15701, #42433, #9742, #46674, #68808, #26263, #52300, #20981, #63207, #68149, #10079, #31539, #19957 ),
 .UNSPECIFIED., .F., .F.,
 ( 4, 2, 2, 2, 2, 2, 2, 2, 2, 2, 2, 2, 2, 2, 2, 2, 2, 2, 2, 2, 2, 2, 2, 2, 2, 2, 2, 4 ),
 ( 0.000000000000000000, 0.001986474333293954727, 0.002979711499940947920, 0.003972948666587941546, 0.004966185833234934739, 0.005959422999881927932, 0.006952660166528921125, 0.007945897333175914318, 0.008939134499822908378, 0.009932371666469900703, 0.01092560883311689303, 0.01191884599976388709, 0.01390532033305785092, 0.01489855749970483111, 0.01589179466635181129, 0.01688503183299879321, 0.01787826899964577165, 0.01986474333293978059, 0.02085798049958679373, 0.02185121766623380687, 0.02383769199952784357, 0.02582416633282188720, 0.02681740349946890381, 0.02781064066611592736, 0.02880387783276294397, 0.02979711499940996405, 0.03079035216605698413, 0.03178358933270400422 ),
 .UNSPECIFIED. ) ;
#30610 = DIRECTION ( 'NONE',  ( -1.000000000000000000, 0.000000000000000000, 0.000000000000000000 ) ) ;
#30611 = CARTESIAN_POINT ( 'NONE',  ( 55.59854697352604092, 11.07381680267640611, 89.83930078720294432 ) ) ;
#30612 = ADVANCED_FACE ( 'NONE', ( #65776 ), #33058, .T. ) ;
#30613 = CARTESIAN_POINT ( 'NONE',  ( 187.5165082312810227, 86.85340440641664372, 6.098473246464705788 ) ) ;
#30614 = CARTESIAN_POINT ( 'NONE',  ( 230.9999999999999432, -35.00000000000000000, 0.000000000000000000 ) ) ;
#30616 = FACE_OUTER_BOUND ( 'NONE', #27305, .T. ) ;
#30615 = CIRCLE ( 'NONE', #27227, 200.0000000000000000 ) ;
#30617 = EDGE_LOOP ( 'NONE', ( #51747, #54988, #33780, #63979, #32163, #42594 ) ) ;
#30618 = CARTESIAN_POINT ( 'NONE',  ( 74.01791526339567895, -12.16185512414844716, 170.0000000000000000 ) ) ;
#30619 = EDGE_LOOP ( 'NONE', ( #66928, #57278, #61417, #6137 ) ) ;
#30620 =( NAMED_UNIT ( * ) PLANE_ANGLE_UNIT ( ) SI_UNIT ( $, .RADIAN. ) );
#30621 = B_SPLINE_CURVE_WITH_KNOTS ( 'NONE', 3,
 ( #58177, #57151, #9995, #31448, #19862, #41317, #47603, #41656, #42000, #69419, #14577, #9651, #57836, #30763, #31114, #69058, #42347, #63806, #15614, #58506, #823, #38807, #49331, #58855, #44058, #27896, #22271, #54615, #38094, #26856, #48282, #43367, #1163, #1509, #43706, #65539, #22974, #22618, #44418, #16638 ),
 .UNSPECIFIED., .F., .F.,
 ( 4, 2, 2, 2, 2, 2, 2, 2, 2, 2, 2, 2, 2, 2, 2, 2, 2, 2, 2, 4 ),
 ( 0.02472759712254455483, 0.02626001169882808198, 0.02779242627511161259, 0.02932484085139513974, 0.03009104813953689117, 0.03085725542767864260, 0.03238967000396211771, 0.03315587729210385526, 0.03392208458024560669, 0.03545449915652906792, 0.03698691373281254302, 0.03851932830909601813, 0.04005174288537948629, 0.04158415746166295446, 0.04311657203794642956, 0.04464898661422990467, 0.04541519390237164222, 0.04618140119051337977, 0.04771381576679688263, 0.04924623034308039243 ),
 .UNSPECIFIED. ) ;
#30622 = CARTESIAN_POINT ( 'NONE',  ( 56.19513604272052731, 11.19349063094192864, -66.93610801037368674 ) ) ;
#30623 =( NAMED_UNIT ( * ) SI_UNIT ( $, .STERADIAN. ) SOLID_ANGLE_UNIT ( ) );
#30624 = FACE_OUTER_BOUND ( 'NONE', #49099, .T. ) ;
#30625 = CARTESIAN_POINT ( 'NONE',  ( -12.88104669460377139, 7.273094923955126134, 85.75516146200649814 ) ) ;
#30626 = AXIS2_PLACEMENT_3D ( 'NONE', #30931, #36202, #52373 ) ;
#30627 = CARTESIAN_POINT ( 'NONE',  ( -102.7447593990059147, 34.14748189312174276, -23.17002667451225761 ) ) ;
#30628 = EDGE_LOOP ( 'NONE', ( #7907, #46578, #58714, #25450 ) ) ;
#30629 = CARTESIAN_POINT ( 'NONE',  ( -75.64857587248467041, 21.19501514561449085, 71.63294696157397823 ) ) ;
#30630 = CARTESIAN_POINT ( 'NONE',  ( 204.3728460619837222, 105.8991018586015684, -90.01503221354896311 ) ) ;
#30631 = VERTEX_POINT ( 'NONE', #50283 ) ;
#30632 = ORIENTED_EDGE ( 'NONE', *, *, #704, .F. ) ;
#30633 = CARTESIAN_POINT ( 'NONE',  ( -157.0077369422017739, 70.81157624963286423, 37.93971990965763297 ) ) ;
#30634 = CARTESIAN_POINT ( 'NONE',  ( 53.32245423372560111, 37.19594572654715137, 170.0000000000000000 ) ) ;
#30635 = CARTESIAN_POINT ( 'NONE',  ( 21.27121078971613244, 61.42097029141973508, 40.00000000000003553 ) ) ;
#30636 = DIRECTION ( 'NONE',  ( -1.000000000000000000, -0.000000000000000000, -0.000000000000000000 ) ) ;
#30637 = LINE ( 'NONE', #20080, #41994 ) ;
#30638 = VERTEX_POINT ( 'NONE', #65064 ) ;
#30639 = CARTESIAN_POINT ( 'NONE',  ( 427.4999999999999432, 207.5000000000000284, 0.000000000000000000 ) ) ;
#30640 = EDGE_LOOP ( 'NONE', ( #6593, #66980, #64949, #8337 ) ) ;
#30641 = CARTESIAN_POINT ( 'NONE',  ( 20.36233635256088448, 7.697399815318435756, -48.98271903251053772 ) ) ;
#30642 = CARTESIAN_POINT ( 'NONE',  ( -146.7404675333698094, 63.17262273741976486, 45.19530540836205290 ) ) ;
#30643 = CARTESIAN_POINT ( 'NONE',  ( 210.0292194063022180, 113.9511645670926470, 41.98791776798442754 ) ) ;
#30644 = FACE_BOUND ( 'NONE', #38164, .T. ) ;
#30645 = ADVANCED_FACE ( 'NONE', ( #23555 ), #16863, .F. ) ;
#30646 = EDGE_CURVE ( 'NONE', #53693, #5113, #7018, .T. ) ;
#30647 = ORIENTED_EDGE ( 'NONE', *, *, #62917, .F. ) ;
#30648 = VERTEX_POINT ( 'NONE', #1390 ) ;
#30649 = CARTESIAN_POINT ( 'NONE',  ( -31.43908319763710679, -170.0000000000000000, 3.371903815725488585 ) ) ;
#30650 = CARTESIAN_POINT ( 'NONE',  ( -126.2499057435234846, 47.93568886205795110, 84.31219562368272591 ) ) ;
#30651 = VECTOR ( 'NONE', #18029, 1000.000000000000000 ) ;
#30652 = CARTESIAN_POINT ( 'NONE',  ( -167.9889421625799457, 81.59140042431234008, -20.85682559493721655 ) ) ;
#30653 = CARTESIAN_POINT ( 'NONE',  ( -149.5074843970971301, -170.0000000000000000, -61.65738112195564469 ) ) ;
#30654 = CARTESIAN_POINT ( 'NONE',  ( 8.389070543067937535, 6.376531511354393444, 89.93455881902842464 ) ) ;
#30655 = CARTESIAN_POINT ( 'NONE',  ( 80.73012746365746750, 17.49169339352361519, -65.50839743993871878 ) ) ;
#30656 = VECTOR ( 'NONE', #64953, 1000.000000000000000 ) ;
#30657 = VERTEX_POINT ( 'NONE', #1047 ) ;
#30658 = LINE ( 'NONE', #3925, #68496 ) ;
#30659 = CARTESIAN_POINT ( 'NONE',  ( -95.63568360745009045, 29.53168204475777259, 61.37563518862691581 ) ) ;
#30660 = ORIENTED_EDGE ( 'NONE', *, *, #33696, .T. ) ;
#30661 = FACE_OUTER_BOUND ( 'NONE', #1188, .T. ) ;
#30662 = VERTEX_POINT ( 'NONE', #59765 ) ;
#30663 = CARTESIAN_POINT ( 'NONE',  ( 200.0000000000000000, 2.999999999999969802, -46.99999999999997158 ) ) ;
#30664 = AXIS2_PLACEMENT_3D ( 'NONE', #43321, #64799, #44019 ) ;
#30665 = EDGE_CURVE ( 'NONE', #35812, #37212, #7411, .T. ) ;
#30666 = EDGE_LOOP ( 'NONE', ( #41401, #62306, #20182, #66419 ) ) ;
#30667 = EDGE_CURVE ( 'NONE', #55132, #23082, #66475, .T. ) ;
#30668 = VECTOR ( 'NONE', #6549, 1000.000000000000000 ) ;
#30669 = EDGE_LOOP ( 'NONE', ( #51480, #10071, #48165, #63699 ) ) ;
#30670 = CARTESIAN_POINT ( 'NONE',  ( 13.14401442664830988, 6.430459733718341120, -35.99624556455200519 ) ) ;
#30671 = DIRECTION ( 'NONE',  ( 1.000000000000000000, 0.000000000000000000, 0.000000000000000000 ) ) ;
#30672 = DIRECTION ( 'NONE',  ( -0.000000000000000000, -0.000000000000000000, -1.000000000000000000 ) ) ;
#30673 = ORIENTED_EDGE ( 'NONE', *, *, #5773, .T. ) ;
#30674 = B_SPLINE_CURVE_WITH_KNOTS ( 'NONE', 3,
 ( #13104, #8519, #35240, #29968, #51766, #35593, #34570, #8865, #2892, #67955, #7823, #46479, #51429, #66927, #62315, #67604, #40173, #30315, #3241, #56012, #56344, #28935, #25044, #13444, #2541, #34210, #45797, #3572, #34906, #19060, #40514, #23652, #19755, #50720, #61961, #7484, #14134, #29273, #50387, #19403, #41214, #45444, #18369, #12750, #55651, #42591, #20433, #57388, #62674, #36280 ),
 .UNSPECIFIED., .F., .F.,
 ( 4, 2, 2, 2, 2, 2, 2, 2, 2, 2, 2, 2, 2, 2, 2, 2, 2, 2, 2, 2, 2, 2, 2, 2, 4 ),
 ( 0.03296461860586801657, 0.03492857779726586676, 0.03689253698866371695, 0.03885649618006156714, 0.04082045537145942427, 0.04278441456285727446, 0.04376639415855620302, 0.04474837375425513852, 0.04573035334995407403, 0.04671233294565300259, 0.04720332274350246687, 0.04769431254135193810, 0.04867629213705086666, 0.04965827173274980216, 0.05064025132844873767, 0.05162223092414766623, 0.05260421051984659480, 0.05358619011554553030, 0.05456816971124446580, 0.05555014930694339437, 0.05653212890264232987, 0.05849608809404027721, 0.06046004728543821760, 0.06242400647683615800, 0.06438796566823409839 ),
 .UNSPECIFIED. ) ;
#30675 = CARTESIAN_POINT ( 'NONE',  ( -38.56832981558923024, 10.87072789871799117, 93.82338543633802885 ) ) ;
#30676 = CARTESIAN_POINT ( 'NONE',  ( 175.0634607207819045, 74.11351956991637735, -66.08984933419260699 ) ) ;
#30677 = PLANE ( 'NONE',  #51627 ) ;
#30678 = LINE ( 'NONE', #4969, #61933 ) ;
#30679 = DIRECTION ( 'NONE',  ( -1.000000000000000000, 0.000000000000000000, 0.000000000000000000 ) ) ;
#30680 = CYLINDRICAL_SURFACE ( 'NONE', #47856, 7.500000000000020428 ) ;
#30681 = VERTEX_POINT ( 'NONE', #39726 ) ;
#30682 = EDGE_LOOP ( 'NONE', ( #15936, #12284 ) ) ;
#30683 = CARTESIAN_POINT ( 'NONE',  ( -440.1146514826277212, 400.0000000000065370, -133.9016337311479958 ) ) ;
#30684 = CARTESIAN_POINT ( 'NONE',  ( -85.75002235020440366, 26.23806300442548078, -66.98273671324270140 ) ) ;
#30685 = CARTESIAN_POINT ( 'NONE',  ( 173.7225111622555005, 72.84868911716898765, 11.42765638463486333 ) ) ;
#30686 = DIRECTION ( 'NONE',  ( 0.5877852522924685852, 0.8090169943749507819, 0.000000000000000000 ) ) ;
#30687 = FACE_OUTER_BOUND ( 'NONE', #21275, .T. ) ;
#30688 = CARTESIAN_POINT ( 'NONE',  ( 133.3996297101684263, 41.14871796345731525, 17.66579024853170310 ) ) ;
#30689 = CARTESIAN_POINT ( 'NONE',  ( -156.1462053606562677, 70.02140399657014314, 14.87619319211899516 ) ) ;
#30690 = CARTESIAN_POINT ( 'NONE',  ( -118.8691191306315318, 43.21907118237575673, -66.61757324505178701 ) ) ;
#30691 = CARTESIAN_POINT ( 'NONE',  ( 212.1488570093002011, 119.0116247937291689, 35.83619200126886994 ) ) ;
#30692 = DIRECTION ( 'NONE',  ( 0.000000000000000000, 1.000000000000000000, -0.000000000000000000 ) ) ;
#30693 = CARTESIAN_POINT ( 'NONE',  ( -109.7816385129979295, 36.75776661907239173, 37.51838681235415152 ) ) ;
#30694 = ORIENTED_EDGE ( 'NONE', *, *, #47021, .F. ) ;
#30695 = AXIS2_PLACEMENT_3D ( 'NONE', #8147, #18350, #61947 ) ;
#30696 = ITEM_DEFINED_TRANSFORMATION ( 'NONE', 'NONE', #1785,  #66832 ) ;
#30697 = CARTESIAN_POINT ( 'NONE',  ( -47.54597338633182346, 13.82996226214091173, 91.56377290884543640 ) ) ;
#30698 = ORIENTED_EDGE ( 'NONE', *, *, #4928, .F. ) ;
#30699 = CARTESIAN_POINT ( 'NONE',  ( 0.7145311798163216377, 4.618802153517004960, 7.999999999999998224 ) ) ;
#30700 = ORIENTED_EDGE ( 'NONE', *, *, #31652, .T. ) ;
#30701 = CARTESIAN_POINT ( 'NONE',  ( 63.01563776193090405, 13.70579113808096672, -89.40979201309708913 ) ) ;
#30702 = AXIS2_PLACEMENT_3D ( 'NONE', #64951, #11460, #27297 ) ;
#30703 = CARTESIAN_POINT ( 'NONE',  ( -60.30072871347308450, 36.58596684574257552, -74.30072871347313423 ) ) ;
#30704 = DIRECTION ( 'NONE',  ( -0.000000000000000000, 0.000000000000000000, -1.000000000000000000 ) ) ;
#30705 = DIRECTION ( 'NONE',  ( 0.000000000000000000, 0.000000000000000000, 1.000000000000000000 ) ) ;
#30706 = CARTESIAN_POINT ( 'NONE',  ( 140.5958192060901695, 46.84598876498523623, -46.82504131882815557 ) ) ;
#30707 = CARTESIAN_POINT ( 'NONE',  ( 36.99625334683020839, 8.108440754877198842, -50.24044060793853816 ) ) ;
#30708 = AXIS2_PLACEMENT_3D ( 'NONE', #40558, #69275, #29663 ) ;
#30709 = CARTESIAN_POINT ( 'NONE',  ( 444.4083459183738682, 365.0000000000043769, 110.6213636698493872 ) ) ;
#30710 = CARTESIAN_POINT ( 'NONE',  ( 10.31616749326173554, 7.393414706728904662, -48.15370678270306826 ) ) ;
#30711 = CARTESIAN_POINT ( 'NONE',  ( 127.6144785300460143, 37.78099129859914740, -47.68851779290559278 ) ) ;
#30712 = ORIENTED_EDGE ( 'NONE', *, *, #36931, .F. ) ;
#30713 = AXIS2_PLACEMENT_3D ( 'NONE', #33120, #6380, #27834 ) ;
#30714 = VERTEX_POINT ( 'NONE', #32703 ) ;
#30715 = VECTOR ( 'NONE', #28383, 1000.000000000000000 ) ;
#30716 = DIRECTION ( 'NONE',  ( -0.000000000000000000, -0.000000000000000000, -1.000000000000000000 ) ) ;
#30717 = DIRECTION ( 'NONE',  ( -0.8090169943749422332, -0.5877852522924802425, 0.000000000000000000 ) ) ;
#30718 = VECTOR ( 'NONE', #51501, 1000.000000000000000 ) ;
#30719 = LINE ( 'NONE', #19114, #6026 ) ;
#30720 = AXIS2_PLACEMENT_3D ( 'NONE', #17175, #54454, #58445 ) ;
#30721 = DIRECTION ( 'NONE',  ( 0.000000000000000000, 0.000000000000000000, 1.000000000000000000 ) ) ;
#30722 = ADVANCED_FACE ( 'NONE', ( #43934 ), #5957, .T. ) ;
#30723 = CARTESIAN_POINT ( 'NONE',  ( 280.6524747721059612, 21.43176909745611169, -4.968265989321519527 ) ) ;
#30724 = ORIENTED_EDGE ( 'NONE', *, *, #58272, .T. ) ;
#30725 = FACE_OUTER_BOUND ( 'NONE', #758, .T. ) ;
#30726 = CARTESIAN_POINT ( 'NONE',  ( 174.1251613516843975, 71.84747073139212148, -67.71850567866349024 ) ) ;
#30727 = LINE ( 'NONE', #25801, #41901 ) ;
#30728 = DIRECTION ( 'NONE',  ( 0.8090169943749422332, 0.5877852522924802425, 0.000000000000000000 ) ) ;
#30729 = CARTESIAN_POINT ( 'NONE',  ( -30.46358361599563835, 10.45190018822943578, 72.01312986667528548 ) ) ;
#30730 = CARTESIAN_POINT ( 'NONE',  ( 44.99999999999999289, -20.00000000000000355, 0.000000000000000000 ) ) ;
#30731 = CARTESIAN_POINT ( 'NONE',  ( -51.77439426130688105, 13.82695438436702418, 71.41181520050716358 ) ) ;
#30732 = ADVANCED_FACE ( 'NONE', ( #60127 ), #17572, .F. ) ;
#30733 = EDGE_CURVE ( 'NONE', #56693, #49487, #41342, .T. ) ;
#30734 = ORIENTED_EDGE ( 'NONE', *, *, #60272, .F. ) ;
#30735 = CARTESIAN_POINT ( 'NONE',  ( -31.11269837220812207, -26.11269837220801193, 85.00100000000000477 ) ) ;
#30736 = EDGE_CURVE ( 'NONE', #33732, #27549, #11615, .T. ) ;
#30737 = CARTESIAN_POINT ( 'NONE',  ( -173.1211646369891355, -170.0000000000000000, 3.977144016177345254 ) ) ;
#30738 = CARTESIAN_POINT ( 'NONE',  ( -107.2385267828037172, 36.51474259889399576, -74.99142853021918143 ) ) ;
#30739 = CARTESIAN_POINT ( 'NONE',  ( -417.6627218934917778, 397.0710678118718988, -111.4497041420121519 ) ) ;
#30740 = FACE_OUTER_BOUND ( 'NONE', #57159, .T. ) ;
#30741 = CARTESIAN_POINT ( 'NONE',  ( -74.52723870109939242, -7.962625360375267469, 41.38025477438755928 ) ) ;
#30742 = EDGE_LOOP ( 'NONE', ( #44080, #33997, #50143, #20790 ) ) ;
#30743 = CARTESIAN_POINT ( 'NONE',  ( 0.000000000000000000, 0.000000000000000000, 170.0000000000000000 ) ) ;
#30744 = DIRECTION ( 'NONE',  ( -1.000000000000000000, 0.000000000000000000, -0.000000000000000000 ) ) ;
#30745 = VERTEX_POINT ( 'NONE', #61529 ) ;
#30746 = VERTEX_POINT ( 'NONE', #67503 ) ;
#30747 = CIRCLE ( 'NONE', #30695, 24.99999999999985434 ) ;
#30748 = CARTESIAN_POINT ( 'NONE',  ( -9.273616082387997395, -77.77273080542778416, 73.58025477438756923 ) ) ;
#30749 = CARTESIAN_POINT ( 'NONE',  ( -48.12872802574198516, -43.70867239603780519, 43.58025477438756923 ) ) ;
#30750 = CARTESIAN_POINT ( 'NONE',  ( 140.7279459667387869, 46.93224938917404643, -94.17646906148590347 ) ) ;
#30751 = EDGE_CURVE ( 'NONE', #25266, #64727, #21103, .T. ) ;
#30752 = ORIENTED_EDGE ( 'NONE', *, *, #60527, .F. ) ;
#30753 = CARTESIAN_POINT ( 'NONE',  ( 427.4999999999999432, -17.50000000000000000, 20.00000000000000000 ) ) ;
#30754 = DIRECTION ( 'NONE',  ( 0.000000000000000000, 0.000000000000000000, 1.000000000000000000 ) ) ;
#30755 = VECTOR ( 'NONE', #17543, 1000.000000000000000 ) ;
#30756 = CARTESIAN_POINT ( 'NONE',  ( 57.09527843067915143, 12.40436368789086963, -47.83156069688324408 ) ) ;
#30757 = CARTESIAN_POINT ( 'NONE',  ( -83.51110947562234799, 25.31252704029287415, 32.18774550040605931 ) ) ;
#30758 = CARTESIAN_POINT ( 'NONE',  ( -24.32776401346968598, 9.546905915310565760, -13.53957171349472510 ) ) ;
#30759 = CARTESIAN_POINT ( 'NONE',  ( 141.0804878838241336, 45.96076546397619467, 12.25136187784951325 ) ) ;
#30760 = AXIS2_PLACEMENT_3D ( 'NONE', #3882, #20061, #37600 ) ;
#30761 = EDGE_LOOP ( 'NONE', ( #14816, #32384, #2876, #65530 ) ) ;
#30762 = VECTOR ( 'NONE', #14212, 1000.000000000000000 ) ;
#30763 = CARTESIAN_POINT ( 'NONE',  ( 103.9685899589048432, 27.18106603025993095, -20.69423234284586499 ) ) ;
#30764 = VECTOR ( 'NONE', #28751, 1000.000000000000000 ) ;
#30765 = CARTESIAN_POINT ( 'NONE',  ( 14.08699529666005823, 6.452200550165255954, 71.66783672710508313 ) ) ;
#30766 = CARTESIAN_POINT ( 'NONE',  ( -23.98747857548120876, 9.501432345103353327, 38.70170266760086264 ) ) ;
#30767 = DIRECTION ( 'NONE',  ( -0.000000000000000000, 0.000000000000000000, -1.000000000000000000 ) ) ;
#30768 = CARTESIAN_POINT ( 'NONE',  ( -125.8938041572051389, -170.0000000000000000, 45.61994787315711619 ) ) ;
#30770 = ORIENTED_EDGE ( 'NONE', *, *, #1915, .T. ) ;
#30769 = DIRECTION ( 'NONE',  ( 0.000000000000000000, -0.000000000000000000, -1.000000000000000000 ) ) ;
#30771 = CARTESIAN_POINT ( 'NONE',  ( 70.50376765786469946, 15.57629333413342820, 36.82268012421604197 ) ) ;
#30772 = ORIENTED_EDGE ( 'NONE', *, *, #11506, .T. ) ;
#30773 = VECTOR ( 'NONE', #40145, 1000.000000000000000 ) ;
#30774 = ORIENTED_EDGE ( 'NONE', *, *, #2544, .F. ) ;
#30775 = FILL_AREA_STYLE ('',( #31801 ) ) ;
#30776 = FACE_OUTER_BOUND ( 'NONE', #45975, .T. ) ;
#30777 = DIRECTION ( 'NONE',  ( 1.000000000000000000, 0.000000000000000000, 0.000000000000000000 ) ) ;
#30778 = DIRECTION ( 'NONE',  ( -0.000000000000000000, -0.000000000000000000, -1.000000000000000000 ) ) ;
#30779 = CARTESIAN_POINT ( 'NONE',  ( -118.6849742182705256, 41.92701402439731595, 67.05091989562900778 ) ) ;
#30780 = FACE_OUTER_BOUND ( 'NONE', #2867, .T. ) ;
#30781 = CARTESIAN_POINT ( 'NONE',  ( 26.99999999999999645, -30.00000000000000355, 12.00000000000000000 ) ) ;
#30782 = CARTESIAN_POINT ( 'NONE',  ( -52.67596829228261868, 15.09584868440940042, 30.68732742033287053 ) ) ;
#30783 = ORIENTED_EDGE ( 'NONE', *, *, #16181, .T. ) ;
#30784 = EDGE_LOOP ( 'NONE', ( #63399, #25132 ) ) ;
#30785 = B_SPLINE_CURVE_WITH_KNOTS ( 'NONE', 3,
 ( #43658, #48234, #16591, #22220, #410, #5680, #64432, #63756, #53521, #20834, #37020, #6025, #31733, #65137, #38047, #32774, #32084, #27487, #16931, #27141, #21519, #53168, #43309, #21865, #42963, #53861, #54202, #11653, #16243, #5001, #48926, #15565, #37695, #26465, #54563, #47902, #767, #59492, #21186, #58457, #6389, #27842, #58798, #5352 ),
 .UNSPECIFIED., .F., .F.,
 ( 4, 2, 2, 2, 2, 2, 2, 2, 2, 2, 2, 2, 2, 2, 2, 2, 2, 2, 2, 2, 2, 4 ),
 ( 0.000000000000000000, 0.001488594467279756757, 0.002232891700919623860, 0.002977188934559490963, 0.004465783401839205219, 0.005954377869118920343, 0.007442972336398633731, 0.008187269570038497798, 0.008931566803678360131, 0.01042016127095808480, 0.01190875573823781293, 0.01265305297187767700, 0.01339735020551753759, 0.01488594467279726052, 0.01563024190643714020, 0.01637453914007701988, 0.01786313360735677577, 0.01935172807463653513, 0.02009602530827639746, 0.02084032254191625633, 0.02232891700919594630, 0.02381751147647563280 ),
 .UNSPECIFIED. ) ;
#30786 = CARTESIAN_POINT ( 'NONE',  ( -102.7494334820056139, 34.14986869751099618, 18.67452391595144334 ) ) ;
#30787 = CARTESIAN_POINT ( 'NONE',  ( -83.69370847062543817, 25.38703975185372386, -48.18640663508916333 ) ) ;
#30788 = CARTESIAN_POINT ( 'NONE',  ( 115.7655322686204755, 31.52170665051862031, 85.71478802353045978 ) ) ;
#30789 = CARTESIAN_POINT ( 'NONE',  ( 8.000000000000000000, 3.871967595402134421, -9.001061386767540640 ) ) ;
#30790 = EDGE_CURVE ( 'NONE', #11742, #135, #29510, .T. ) ;
#30791 = LINE ( 'NONE', #3702, #32606 ) ;
#30792 = DIRECTION ( 'NONE',  ( -0.8660254037844378194, -0.5000000000000014433, 0.000000000000000000 ) ) ;
#30793 = CARTESIAN_POINT ( 'NONE',  ( 164.8471526211111495, 63.62172173173267709, -69.08682052283407415 ) ) ;
#30794 = ORIENTED_EDGE ( 'NONE', *, *, #29557, .T. ) ;
#30795 = VERTEX_POINT ( 'NONE', #2789 ) ;
#30796 = VERTEX_POINT ( 'NONE', #62212 ) ;
#30797 = AXIS2_PLACEMENT_3D ( 'NONE', #28562, #3556, #31337 ) ;
#30798 = CARTESIAN_POINT ( 'NONE',  ( -149.7268278745401631, 65.68859631971237434, -22.96827994102830317 ) ) ;
#30799 = FACE_OUTER_BOUND ( 'NONE', #22294, .T. ) ;
#30800 = CARTESIAN_POINT ( 'NONE',  ( 68.63487067129265995, 14.04635751989139614, -38.22936938732106427 ) ) ;
#30801 = CARTESIAN_POINT ( 'NONE',  ( 107.4947172190871356, -21.56856595115425890, 4.339532581985756643 ) ) ;
#30802 = AXIS2_PLACEMENT_3D ( 'NONE', #30025, #30717, #68353 ) ;
#30803 = FACE_OUTER_BOUND ( 'NONE', #4836, .T. ) ;
#30804 = DIRECTION ( 'NONE',  ( 1.000000000000000000, 1.132072239499580971E-16, -1.697513318603925187E-16 ) ) ;
#30805 = VECTOR ( 'NONE', #33750, 1000.000000000000000 ) ;
#30806 = CARTESIAN_POINT ( 'NONE',  ( 31.99894129856762603, 7.561773404408284271, 63.03122815760148256 ) ) ;
#30807 = CARTESIAN_POINT ( 'NONE',  ( 45.98350631452262149, 9.356976075258891967, 94.71468413938886499 ) ) ;
#30808 = VERTEX_POINT ( 'NONE', #56951 ) ;
#30809 = CARTESIAN_POINT ( 'NONE',  ( 20.74561700410411191, 7.717362891868937425, 16.31941674212566795 ) ) ;
#30810 = PLANE ( 'NONE',  #19488 ) ;
#30811 = CARTESIAN_POINT ( 'NONE',  ( -119.2982054035570769, 42.30181775808005540, 7.695783488898820579 ) ) ;
#30812 = CARTESIAN_POINT ( 'NONE',  ( -133.3122825023497171, 51.57669324886579432, -95.00000000000133582 ) ) ;
#30813 = AXIS2_PLACEMENT_3D ( 'NONE', #60894, #55977, #13750 ) ;
#30814 = CARTESIAN_POINT ( 'NONE',  ( 126.4754729582248132, 37.14269484129875565, -15.32358833706418011 ) ) ;
#30815 = CARTESIAN_POINT ( 'NONE',  ( 20.36233635256087382, 7.697399815318433980, -22.13816844204684386 ) ) ;
#30816 = CARTESIAN_POINT ( 'NONE',  ( 198.7084915431530305, 98.47675983942191635, 59.03003622776400761 ) ) ;
#30817 = VECTOR ( 'NONE', #539, 1000.000000000000000 ) ;
#30818 = EDGE_CURVE ( 'NONE', #13481, #45287, #17246, .T. ) ;
#30819 = VECTOR ( 'NONE', #53732, 1000.000000000000000 ) ;
#30820 = ORIENTED_EDGE ( 'NONE', *, *, #19321, .F. ) ;
#30821 = LINE ( 'NONE', #52265, #58544 ) ;
#30822 = APPLICATION_PROTOCOL_DEFINITION ( 'draft international standard', 'automotive_design', 1998, #62394 ) ;
#30823 = EDGE_CURVE ( 'NONE', #31341, #6300, #35490, .T. ) ;
#30824 = CARTESIAN_POINT ( 'NONE',  ( 128.4157044224114088, 39.39296260757095069, -48.70813808969364089 ) ) ;
#30825 = CARTESIAN_POINT ( 'NONE',  ( -130.1964689553233256, 49.39217932424205060, -36.25302896202752834 ) ) ;
#30826 = CARTESIAN_POINT ( 'NONE',  ( -108.6944271866238978, 37.30738480893074893, -38.59587447743199817 ) ) ;
#30827 = CARTESIAN_POINT ( 'NONE',  ( 188.4918087359957042, 87.93403732562659059, -44.93618865354876135 ) ) ;
#30828 = ORIENTED_EDGE ( 'NONE', *, *, #44235, .T. ) ;
#30829 = ORIENTED_EDGE ( 'NONE', *, *, #25831, .F. ) ;
#30830 = CARTESIAN_POINT ( 'NONE',  ( -26.50364027666003253, 8.832969329054188634, -21.64101123914544900 ) ) ;
#30831 = DIRECTION ( 'NONE',  ( 0.000000000000000000, 1.000000000000000000, -0.000000000000000000 ) ) ;
#30832 = VERTEX_POINT ( 'NONE', #20339 ) ;
#30833 = FACE_OUTER_BOUND ( 'NONE', #59558, .T. ) ;
#30834 = EDGE_CURVE ( 'NONE', #40885, #53508, #26319, .T. ) ;
#30835 = ORIENTED_EDGE ( 'NONE', *, *, #35889, .F. ) ;
#30836 = CARTESIAN_POINT ( 'NONE',  ( -61.53550548562876088, 17.56596194025584978, 14.77635692923447053 ) ) ;
#30837 = CARTESIAN_POINT ( 'NONE',  ( 133.8566784816069628, 41.42467568809806977, 44.51034083899536142 ) ) ;
#30838 = CARTESIAN_POINT ( 'NONE',  ( -190.6985136298601731, 109.1272424661242582, 94.99999999999866418 ) ) ;
#30839 = EDGE_CURVE ( 'NONE', #68152, #6290, #48466, .T. ) ;
#30840 = EDGE_CURVE ( 'NONE', #54103, #7837, #57641, .T. ) ;
#30841 = CARTESIAN_POINT ( 'NONE',  ( -94.79534239005252516, 29.13842790650043568, 37.47587493899962396 ) ) ;
#30842 = CARTESIAN_POINT ( 'NONE',  ( 109.9975424824652634, 18.00000000000002842, 536.6193948016162949 ) ) ;
#30844 = ORIENTED_EDGE ( 'NONE', *, *, #18886, .F. ) ;
#30843 = CARTESIAN_POINT ( 'NONE',  ( -49.42000000000000171, -26.09918303830819397, 10.41169613715280740 ) ) ;
#30845 = CARTESIAN_POINT ( 'NONE',  ( -34.75846525699014933, 54.92585086258208804, 170.0000000000000000 ) ) ;
#30846 = ORIENTED_EDGE ( 'NONE', *, *, #11689, .F. ) ;
#30847 = VERTEX_POINT ( 'NONE', #4172 ) ;
#30848 = CARTESIAN_POINT ( 'NONE',  ( -125.0023254877051784, 45.90912477771775002, -23.02977023342388918 ) ) ;
#30849 = AXIS2_PLACEMENT_3D ( 'NONE', #34050, #55855, #2049 ) ;
#30850 = DIRECTION ( 'NONE',  ( 0.08963930890342655666, 0.9959742939952397345, 5.102127870520019688E-18 ) ) ;
#30851 = CARTESIAN_POINT ( 'NONE',  ( -178.7483298110140311, 93.61800926271534706, -20.33199145141687225 ) ) ;
#30853 = ORIENTED_EDGE ( 'NONE', *, *, #48812, .T. ) ;
#30852 = CARTESIAN_POINT ( 'NONE',  ( -129.3970594949620363, 50.06339481638102029, 58.31657860348069988 ) ) ;
#30854 = CARTESIAN_POINT ( 'NONE',  ( -103.5135803422113980, 34.54427913530279426, 84.30440530529723731 ) ) ;
#30855 = DIRECTION ( 'NONE',  ( 1.000000000000000000, 0.000000000000000000, -0.000000000000000000 ) ) ;
#30856 = CIRCLE ( 'NONE', #32005, 5.000000000000000888 ) ;
#30857 = VERTEX_POINT ( 'NONE', #25640 ) ;
#30858 = CARTESIAN_POINT ( 'NONE',  ( -58.32860549785898741, 15.58423118879329827, -22.62294191281809930 ) ) ;
#30859 = AXIS2_PLACEMENT_3D ( 'NONE', #19284, #68847, #47059 ) ;
#30860 = VECTOR ( 'NONE', #45974, 999.9999999999998863 ) ;
#30861 = CARTESIAN_POINT ( 'NONE',  ( -133.3220917939969752, 52.82057604964898445, -68.18860869838340477 ) ) ;
#30862 = CARTESIAN_POINT ( 'NONE',  ( 57.01498327362266139, 11.36040931982467406, -92.39178327290893833 ) ) ;
#30863 = VECTOR ( 'NONE', #58171, 1000.000000000000000 ) ;
#30864 = DIRECTION ( 'NONE',  ( 1.000000000000000000, 0.000000000000000000, 0.000000000000000000 ) ) ;
#30865 = CARTESIAN_POINT ( 'NONE',  ( 68.63585058221467250, 15.08566240483131438, -75.05603185210503625 ) ) ;
#30866 = ORIENTED_EDGE ( 'NONE', *, *, #28738, .F. ) ;
#30867 = ORIENTED_EDGE ( 'NONE', *, *, #40848, .F. ) ;
#30868 = CARTESIAN_POINT ( 'NONE',  ( -142.0084862216822899, 59.34995487985342777, -14.88985590709667228 ) ) ;
#30869 = CARTESIAN_POINT ( 'NONE',  ( -171.0758681675584683, 84.87997360100517596, -34.98379575707922129 ) ) ;
#30870 = DIRECTION ( 'NONE',  ( 1.387778780781445429E-16, -1.000000000000000000, -3.081487911019577365E-33 ) ) ;
#30871 = DIRECTION ( 'NONE',  ( -1.020422603260505347E-14, 1.000000000000000000, 5.551115123125782702E-17 ) ) ;
#30872 = CARTESIAN_POINT ( 'NONE',  ( -74.20136529587827567, 21.74007521413448885, 43.94919298524185791 ) ) ;
#30873 = EDGE_CURVE ( 'NONE', #10821, #44801, #15068, .T. ) ;
#30874 = CARTESIAN_POINT ( 'NONE',  ( -52.00772213768630081, 26.43299429372219578, 27.58472315868181113 ) ) ;
#30875 = CARTESIAN_POINT ( 'NONE',  ( -149.2910611247328063, 63.99625741915658494, 45.72082123989907387 ) ) ;
#30876 = CARTESIAN_POINT ( 'NONE',  ( -65.99999999999995737, 29.79383981485516131, -25.00000000000001066 ) ) ;
#30877 = CARTESIAN_POINT ( 'NONE',  ( 209.6525588430077960, 113.3929734759396695, 57.91716753057085754 ) ) ;
#30878 = EDGE_LOOP ( 'NONE', ( #10306, #38321, #22065, #48487 ) ) ;
#30879 = DIRECTION ( 'NONE',  ( -0.000000000000000000, 0.000000000000000000, -1.000000000000000000 ) ) ;
#30880 = ORIENTED_EDGE ( 'NONE', *, *, #31094, .T. ) ;
#30881 = ADVANCED_FACE ( 'NONE', ( #31259 ), #25975, .F. ) ;
#30882 = CARTESIAN_POINT ( 'NONE',  ( -36.37663950036513683, 10.45389057208228678, 16.53845768755774870 ) ) ;
#30883 = CARTESIAN_POINT ( 'NONE',  ( 0.000000000000000000, 0.000000000000000000, 40.00000000000003553 ) ) ;
#30884 = CARTESIAN_POINT ( 'NONE',  ( -84.05562056347102384, 24.44784460338496501, -91.07024174204663325 ) ) ;
#30885 = DIRECTION ( 'NONE',  ( 0.8584487936018655452, 0.5128992774059071280, 0.000000000000000000 ) ) ;
#30886 = DIRECTION ( 'NONE',  ( 0.000000000000000000, 1.000000000000000000, 0.000000000000000000 ) ) ;
#30887 = CARTESIAN_POINT ( 'NONE',  ( 32.46582151331404020, 7.608418548522501546, 13.45366444727946487 ) ) ;
#30888 = CARTESIAN_POINT ( 'NONE',  ( -14.84903512415885274, 8.461292896365067762, -40.27624087600150915 ) ) ;
#30889 = CARTESIAN_POINT ( 'NONE',  ( -38.16652041892308489, 11.81761816422915778, -19.32439935686155152 ) ) ;
#30890 = VERTEX_POINT ( 'NONE', #44205 ) ;
#30891 = DIRECTION ( 'NONE',  ( -0.000000000000000000, 1.000000000000000000, -0.000000000000000000 ) ) ;
#30892 = ORIENTED_EDGE ( 'NONE', *, *, #31356, .T. ) ;
#30893 = FACE_OUTER_BOUND ( 'NONE', #3434, .T. ) ;
#30894 = CARTESIAN_POINT ( 'NONE',  ( -190.4968431727839118, 108.8425311198515004, 7.400362157239960936 ) ) ;
#30895 = EDGE_CURVE ( 'NONE', #32175, #2381, #39299, .T. ) ;
#30896 = DIRECTION ( 'NONE',  ( 0.000000000000000000, -1.000000000000000000, 0.000000000000000000 ) ) ;
#30897 = CARTESIAN_POINT ( 'NONE',  ( -8.811275908848681837, 6.956777180392053062, -77.21364321485079074 ) ) ;
#30898 = CARTESIAN_POINT ( 'NONE',  ( 25.57615758091871427, 44.89060318276072792, 26.66469104408690427 ) ) ;
#30899 = EDGE_CURVE ( 'NONE', #58924, #23841, #66048, .T. ) ;
#30900 = CARTESIAN_POINT ( 'NONE',  ( 150.2060369882285897, 53.45752899907544986, -41.73856419314534349 ) ) ;
#30901 = AXIS2_PLACEMENT_3D ( 'NONE', #25514, #15291, #19880 ) ;
#30902 = EDGE_CURVE ( 'NONE', #36681, #14130, #27684, .T. ) ;
#30903 = ORIENTED_EDGE ( 'NONE', *, *, #15852, .T. ) ;
#30904 = VECTOR ( 'NONE', #52808, 1000.000000000000000 ) ;
#30905 = DIRECTION ( 'NONE',  ( 0.9183650514339902760, 1.072752997544057507E-14, -0.3957342950827543171 ) ) ;
#30906 = EDGE_CURVE ( 'NONE', #9188, #57503, #11856, .T. ) ;
#30907 = CARTESIAN_POINT ( 'NONE',  ( -156.6644740249450081, 71.86407434531899696, 62.80635761803053896 ) ) ;
#30908 = DIRECTION ( 'NONE',  ( 1.000000000000000000, 0.000000000000000000, 0.000000000000000000 ) ) ;
#30909 = CARTESIAN_POINT ( 'NONE',  ( -103.2164890789475464, 34.39030697009943793, 72.31974941879711594 ) ) ;
#30910 = CARTESIAN_POINT ( 'NONE',  ( -102.2801239173131194, -170.0000000000000000, 64.86362509687882039 ) ) ;
#30911 = EDGE_LOOP ( 'NONE', ( #8150, #6313 ) ) ;
#30913 = CARTESIAN_POINT ( 'NONE',  ( -176.3763474213711504, 92.36993073950281996, -75.82728650921367830 ) ) ;
#30912 = AXIS2_PLACEMENT_3D ( 'NONE', #36055, #57509, #9318 ) ;
#30914 = CARTESIAN_POINT ( 'NONE',  ( 93.86680996363766383, 22.01878169039501998, 66.03955257416123459 ) ) ;
#30915 =( GEOMETRIC_REPRESENTATION_CONTEXT ( 3 ) GLOBAL_UNCERTAINTY_ASSIGNED_CONTEXT ( ( #18429 ) ) GLOBAL_UNIT_ASSIGNED_CONTEXT ( ( #44825, #44472, #17381 ) ) REPRESENTATION_CONTEXT ( 'NONE', 'WORKASPACE' ) );
#30916 = CARTESIAN_POINT ( 'NONE',  ( 115.0692128464502701, 31.17922615202198955, 42.87276276046937085 ) ) ;
#30917 = AXIS2_PLACEMENT_3D ( 'NONE', #58175, #52878, #63804 ) ;
#30918 = DIRECTION ( 'NONE',  ( -0.000000000000000000, 1.000000000000000000, -0.000000000000000000 ) ) ;
#30919 = VECTOR ( 'NONE', #16724, 1000.000000000000000 ) ;
#30920 = CARTESIAN_POINT ( 'NONE',  ( -118.5043919384112030, 41.81711884544880320, -67.94780606738419237 ) ) ;
#30921 = EDGE_CURVE ( 'NONE', #48044, #17255, #11495, .T. ) ;
#30922 = VERTEX_POINT ( 'NONE', #49478 ) ;
#30923 = CARTESIAN_POINT ( 'NONE',  ( 197.8572563162090319, 97.41072138832259952, 39.79780622203359997 ) ) ;
#30924 = CARTESIAN_POINT ( 'NONE',  ( 116.6734749296698936, 31.97209464358270026, -66.37505032600662958 ) ) ;
#30925 = CARTESIAN_POINT ( 'NONE',  ( -6.000000000000000000, 23.07878402833891229, -5.000000000000000000 ) ) ;
#30926 = LINE ( 'NONE', #62225, #38889 ) ;
#30927 = DIRECTION ( 'NONE',  ( 1.020422603260505347E-14, -1.000000000000000000, -5.551115123125782702E-17 ) ) ;
#30928 = EDGE_CURVE ( 'NONE', #52659, #42507, #32560, .T. ) ;
#30929 = EDGE_CURVE ( 'NONE', #24824, #66476, #62483, .T. ) ;
#30930 = VERTEX_POINT ( 'NONE', #56163 ) ;
#30931 = CARTESIAN_POINT ( 'NONE',  ( 0.000000000000000000, 0.000000000000000000, 30.00000000000000000 ) ) ;
#30932 = VERTEX_POINT ( 'NONE', #19570 ) ;
#30933 = CARTESIAN_POINT ( 'NONE',  ( -107.7893514267588273, 35.66840175773127442, -47.62729620103424821 ) ) ;
#30934 = CARTESIAN_POINT ( 'NONE',  ( 140.0012045870120687, 45.26048451937214878, 94.99999999999866418 ) ) ;
#30935 = CARTESIAN_POINT ( 'NONE',  ( -62.30100056228378946, 16.74548393487070541, 39.80882454632615719 ) ) ;
#30937 = ORIENTED_EDGE ( 'NONE', *, *, #14756, .F. ) ;
#30936 = DIRECTION ( 'NONE',  ( -1.000000000000000000, 0.000000000000000000, 0.000000000000000000 ) ) ;
#30938 = CARTESIAN_POINT ( 'NONE',  ( -179.9014775667593540, 95.00669833041663992, 35.10404331463944061 ) ) ;
#30939 = DIRECTION ( 'NONE',  ( -1.000000000000000000, -6.405132834375901070E-16, -5.170250902511168442E-32 ) ) ;
#30940 = CARTESIAN_POINT ( 'NONE',  ( 117.7442255600442422, 33.63739995216995737, -43.92135388644469174 ) ) ;
#30941 = ORIENTED_EDGE ( 'NONE', *, *, #44619, .F. ) ;
#30942 = CARTESIAN_POINT ( 'NONE',  ( 6.400000000000000355, 9.237604307034018802, 0.000000000000000000 ) ) ;
#30943 = LINE ( 'NONE', #23931, #32090 ) ;
#30944 = VECTOR ( 'NONE', #26280, 1000.000000000000000 ) ;
#30945 = ORIENTED_EDGE ( 'NONE', *, *, #26202, .T. ) ;
#30946 = CARTESIAN_POINT ( 'NONE',  ( 139.2921620648437226, 44.80435067172500396, 58.66407138463905824 ) ) ;
#30947 = CARTESIAN_POINT ( 'NONE',  ( 447.3372781065085633, 365.0000000000001137, -146.4497041420118251 ) ) ;
#30948 = CARTESIAN_POINT ( 'NONE',  ( -33.13098007862450345, 9.875138601866732202, -62.35103961865778643 ) ) ;
#30949 = CARTESIAN_POINT ( 'NONE',  ( 133.8566784816069060, 41.42467568809810530, -77.86786152285937135 ) ) ;
#30950 = ORIENTED_EDGE ( 'NONE', *, *, #54068, .F. ) ;
#30951 = CARTESIAN_POINT ( 'NONE',  ( 41.33434189587761409, 9.684413566891871383, 17.82021384918356688 ) ) ;
#30952 = ORIENTED_EDGE ( 'NONE', *, *, #65618, .T. ) ;
#30953 = VECTOR ( 'NONE', #15297, 1000.000000000000000 ) ;
#30954 = DIRECTION ( 'NONE',  ( 0.000000000000000000, 0.000000000000000000, 1.000000000000000000 ) ) ;
#30955 = CARTESIAN_POINT ( 'NONE',  ( -62.55951243933055395, 16.82361985462172171, 91.56887453183679781 ) ) ;
#30956 = AXIS2_PLACEMENT_3D ( 'NONE', #19031, #23965, #66899 ) ;
#30957 = AXIS2_PLACEMENT_3D ( 'NONE', #7980, #34021, #50543 ) ;
#30958 = CARTESIAN_POINT ( 'NONE',  ( 110.2429982417149574, 29.99119854320846201, 29.61121420573730489 ) ) ;
#30959 = CARTESIAN_POINT ( 'NONE',  ( -0.3740447803642803493, 7.527031846085010969, 36.63165479535449975 ) ) ;
#30960 = CARTESIAN_POINT ( 'NONE',  ( -42.36049017605964195, 61.90437280228238848, 43.58025477438756923 ) ) ;
#30961 = CARTESIAN_POINT ( 'NONE',  ( 187.8965227056808089, 87.27289477191501987, 13.11287507554345488 ) ) ;
#30962 = CARTESIAN_POINT ( 'NONE',  ( 21.80334764943355452, -25.33568884114822239, 6.893342937333462928 ) ) ;
#30963 = VECTOR ( 'NONE', #38535, 1000.000000000000000 ) ;
#30964 = CARTESIAN_POINT ( 'NONE',  ( 176.6258282025054882, 74.21441092921637050, 3.928463118842791424 ) ) ;
#30965 = VERTEX_POINT ( 'NONE', #61778 ) ;
#30966 = ADVANCED_FACE ( 'NONE', ( #18190 ), #39642, .F. ) ;
#30968 = VECTOR ( 'NONE', #51368, 1000.000000000000000 ) ;
#30967 = FACE_OUTER_BOUND ( 'NONE', #37616, .T. ) ;
#30969 = ORIENTED_EDGE ( 'NONE', *, *, #27850, .F. ) ;
#30970 = APPLICATION_CONTEXT ( 'automotive_design' ) ;
#30971 = CARTESIAN_POINT ( 'NONE',  ( 60.62939143133407072, 12.13148391928981162, -77.19219116658004509 ) ) ;
#30972 = FACE_OUTER_BOUND ( 'NONE', #17398, .T. ) ;
#30973 = DIRECTION ( 'NONE',  ( 1.000000000000000000, -0.000000000000000000, -0.000000000000000000 ) ) ;
#30974 = CARTESIAN_POINT ( 'NONE',  ( 16.28382582968307091, 7.523443033994206885, 45.01470767270525641 ) ) ;
#30975 = CARTESIAN_POINT ( 'NONE',  ( -105.8683518445188838, 35.77995342500075537, -22.27314921212501275 ) ) ;
#30976 = EDGE_LOOP ( 'NONE', ( #7941, #40763 ) ) ;
#30977 = CARTESIAN_POINT ( 'NONE',  ( -7.329206686002009974E-14, -41.66904755831212270, 85.00100000000000477 ) ) ;
#30978 = CARTESIAN_POINT ( 'NONE',  ( 0.000000000000000000, 2.449293598294706907E-15, -20.00000000000000355 ) ) ;
#30979 = EDGE_LOOP ( 'NONE', ( #2930, #17163 ) ) ;
#30980 = ORIENTED_EDGE ( 'NONE', *, *, #24880, .F. ) ;
#30981 = ADVANCED_FACE ( 'NONE', ( #2707 ), #13601, .F. ) ;
#30982 = CARTESIAN_POINT ( 'NONE',  ( -8.000000000000000000, -3.867591403079184253, -0.4976753153245863648 ) ) ;
#30983 = DIRECTION ( 'NONE',  ( 1.000000000000000000, 0.000000000000000000, 0.000000000000000000 ) ) ;
#30984 = CARTESIAN_POINT ( 'NONE',  ( 179.4207200232661705, 76.93724985992179199, -9.516548198904395406 ) ) ;
#30985 = CARTESIAN_POINT ( 'NONE',  ( -46.45214326556835971, 35.29454257130760908, 27.58472315868180402 ) ) ;
#30986 = LINE ( 'NONE', #21443, #16176 ) ;
#30987 = ADVANCED_FACE ( 'NONE', ( #18882 ), #41026, .F. ) ;
#30988 = ORIENTED_EDGE ( 'NONE', *, *, #42196, .T. ) ;
#30989 = EDGE_CURVE ( 'NONE', #8357, #2382, #24168, .T. ) ;
#30990 = CARTESIAN_POINT ( 'NONE',  ( -133.0835080491125098, 52.64966140620843049, 35.96838589234516093 ) ) ;
#30991 = VERTEX_POINT ( 'NONE', #45955 ) ;
#30992 = CARTESIAN_POINT ( 'NONE',  ( 212.0180052085437694, 116.9552462415714871, 11.52689105391897861 ) ) ;
#30993 = CARTESIAN_POINT ( 'NONE',  ( 10.15118267943872077, 7.391905976536033762, 59.40606955087935148 ) ) ;
#30994 = CARTESIAN_POINT ( 'NONE',  ( 212.1707951106656935, 117.1901534358506041, 37.36565939486786192 ) ) ;
#30995 = DIRECTION ( 'NONE',  ( -0.000000000000000000, -0.000000000000000000, -1.000000000000000000 ) ) ;
#30996 = AXIS2_PLACEMENT_3D ( 'NONE', #31462, #8637, #3686 ) ;
#30997 = ORIENTED_EDGE ( 'NONE', *, *, #25806, .T. ) ;
#30998 = VERTEX_POINT ( 'NONE', #51244 ) ;
#30999 = CARTESIAN_POINT ( 'NONE',  ( 110.0000000000000284, -21.42428528562853529, 5.000000000000004441 ) ) ;
#31000 = CARTESIAN_POINT ( 'NONE',  ( -120.6576327989070450, 44.32766273560634573, 86.43031013461866507 ) ) ;
#31001 = CIRCLE ( 'NONE', #20896, 8.000000000000000000 ) ;
#31002 = CARTESIAN_POINT ( 'NONE',  ( 38.90907126433564400, 9.359889524363179447, -62.46436805589143404 ) ) ;
#31003 = CARTESIAN_POINT ( 'NONE',  ( 64.97411640938599930, 37.36411256620309018, 41.38025477438755928 ) ) ;
#31004 = CARTESIAN_POINT ( 'NONE',  ( 22.25657943806483274, 6.793941046373902282, 94.99999999999866418 ) ) ;
#31005 = EDGE_CURVE ( 'NONE', #9445, #28100, #6526, .T. ) ;
#31006 = CARTESIAN_POINT ( 'NONE',  ( 81.04675113612954362, 17.59091904316106181, -65.13359550991796709 ) ) ;
#31007 = AXIS2_PLACEMENT_3D ( 'NONE', #53957, #5786, #49032 ) ;
#31008 = AXIS2_PLACEMENT_3D ( 'NONE', #38073, #38425, #47578 ) ;
#31009 = VERTEX_POINT ( 'NONE', #2364 ) ;
#31010 = AXIS2_PLACEMENT_3D ( 'NONE', #17475, #32967, #31938 ) ;
#31011 = EDGE_CURVE ( 'NONE', #41654, #30206, #39987, .T. ) ;
#31012 = DIRECTION ( 'NONE',  ( -1.000000000000000000, 0.000000000000000000, 0.000000000000000000 ) ) ;
#31013 = CIRCLE ( 'NONE', #668, 65.00000000000000000 ) ;
#31014 = CARTESIAN_POINT ( 'NONE',  ( -96.02415295709708687, 29.71480036090584420, 60.71932897351158687 ) ) ;
#31015 = EDGE_LOOP ( 'NONE', ( #23916, #7778, #28411, #43766 ) ) ;
#31016 = CARTESIAN_POINT ( 'NONE',  ( -79.62258606008208517, 22.68765733708494281, 3.619629083515957468 ) ) ;
#31017 = ORIENTED_EDGE ( 'NONE', *, *, #13490, .T. ) ;
#31018 = B_SPLINE_CURVE_WITH_KNOTS ( 'NONE', 3,
 ( #26207, #30116, #24830, #9692, #47642, #62810, #9338, #57189, #51567, #9004, #14954, #20927, #42381, #51900, #52249, #31157, #63844, #36418 ),
 .UNSPECIFIED., .F., .F.,
 ( 4, 2, 2, 2, 2, 2, 2, 2, 4 ),
 ( 0.01023491291840469483, 0.01150387722361230318, 0.01277284152881991153, 0.01404180583402751814, 0.01531077013923512649, 0.01657973444444273484, 0.01784869874965034145, 0.01911766305485795153, 0.02038662736006555815 ),
 .UNSPECIFIED. ) ;
#31019 = AXIS2_PLACEMENT_3D ( 'NONE', #8469, #51381, #3196 ) ;
#31020 = DIRECTION ( 'NONE',  ( -0.7071067811865475727, 0.000000000000000000, -0.7071067811865475727 ) ) ;
#31021 = ORIENTED_EDGE ( 'NONE', *, *, #6828, .F. ) ;
#31022 = VERTEX_POINT ( 'NONE', #57209 ) ;
#31023 = CARTESIAN_POINT ( 'NONE',  ( 13.37366753069833791, 6.435102282077984626, -50.13664276337100034 ) ) ;
#31024 = CARTESIAN_POINT ( 'NONE',  ( -177.5271152834791337, 92.16916858125016176, 71.25326634736879328 ) ) ;
#31025 = CARTESIAN_POINT ( 'NONE',  ( 132.9440032680863055, 40.87616997986730638, 56.40712532407142987 ) ) ;
#31026 = ORIENTED_EDGE ( 'NONE', *, *, #51372, .T. ) ;
#31027 = CARTESIAN_POINT ( 'NONE',  ( -38.85807996819452370, 10.92741605234837188, 92.55207049280542719 ) ) ;
#31028 = CARTESIAN_POINT ( 'NONE',  ( 173.6700117628886915, 72.79957362875116189, -69.39913175793722644 ) ) ;
#31029 = CARTESIAN_POINT ( 'NONE',  ( -4.999999999999922728, 51.66904755831208718, 85.00100000000000477 ) ) ;
#31030 = CARTESIAN_POINT ( 'NONE',  ( 109.7774723066848566, 28.66666416591279898, -50.92243756565371626 ) ) ;
#31031 = CARTESIAN_POINT ( 'NONE',  ( -6.774725108395606377, -24.06456107444444825, 0.000000000000000000 ) ) ;
#31032 = DIRECTION ( 'NONE',  ( 1.000000000000000000, 0.000000000000000000, 0.000000000000000000 ) ) ;
#31033 = ORIENTED_EDGE ( 'NONE', *, *, #21133, .T. ) ;
#31034 = CARTESIAN_POINT ( 'NONE',  ( 60.40479419793796012, -24.00543350795315334, 40.00000000000003553 ) ) ;
#31035 = CARTESIAN_POINT ( 'NONE',  ( -84.53753601793928851, 25.73343139558517123, -74.15369040441258619 ) ) ;
#31036 = CARTESIAN_POINT ( 'NONE',  ( 173.5836858989432017, 72.71885240881783830, 10.25081972939208441 ) ) ;
#31037 = LINE ( 'NONE', #36309, #31173 ) ;
#31038 = PLANE ( 'NONE',  #40023 ) ;
#31039 = CARTESIAN_POINT ( 'NONE',  ( 128.0568017572569488, 38.03085713813913316, 5.383796554812978918 ) ) ;
#31040 = CARTESIAN_POINT ( 'NONE',  ( 35.46869960875725525, 7.930278842742511713, -90.40974432087365642 ) ) ;
#31041 = CARTESIAN_POINT ( 'NONE',  ( -122.1940143064357187, 45.29738883755585732, -62.73011510844082750 ) ) ;
#31042 = ADVANCED_FACE ( 'NONE', ( #8335 ), #23816, .F. ) ;
#31043 = CARTESIAN_POINT ( 'NONE',  ( 211.8382652195006699, 118.5282575235989952, 39.02422649141074373 ) ) ;
#31044 = CARTESIAN_POINT ( 'NONE',  ( -82.33596576276350731, 24.83688096733768447, 71.32179102043865271 ) ) ;
#31045 = CARTESIAN_POINT ( 'NONE',  ( -109.3553681454883844, 36.52260784104392854, 35.47894457937506019 ) ) ;
#31046 = VERTEX_POINT ( 'NONE', #67421 ) ;
#31047 = CIRCLE ( 'NONE', #23155, 243.4957430088094839 ) ;
#31048 = EDGE_CURVE ( 'NONE', #27671, #45386, #19216, .T. ) ;
#31049 = ITEM_DEFINED_TRANSFORMATION ( 'NONE', 'NONE', #52289,  #66832 ) ;
#31050 = CARTESIAN_POINT ( 'NONE',  ( -48.41612563322100016, 14.03642305406760471, 94.99999999999866418 ) ) ;
#31051 = ORIENTED_EDGE ( 'NONE', *, *, #56774, .T. ) ;
#31052 = DIRECTION ( 'NONE',  ( -0.000000000000000000, 1.000000000000000000, -0.000000000000000000 ) ) ;
#31053 = ORIENTED_EDGE ( 'NONE', *, *, #10466, .F. ) ;
#31054 = CARTESIAN_POINT ( 'NONE',  ( 17.72748965151693668, 7.577488030789625739, -62.61435461240134970 ) ) ;
#31055 = VECTOR ( 'NONE', #67069, 1000.000000000000000 ) ;
#31056 = CARTESIAN_POINT ( 'NONE',  ( -172.7173255566597163, 88.18461381371096763, 30.82169460664102800 ) ) ;
#31057 = DIRECTION ( 'NONE',  ( 0.000000000000000000, 0.000000000000000000, 1.000000000000000000 ) ) ;
#31058 = CARTESIAN_POINT ( 'NONE',  ( 134.7708899521911121, 43.15864772107692460, -50.97092526706858706 ) ) ;
#31059 = VECTOR ( 'NONE', #35842, 1000.000000000000000 ) ;
#31060 = CARTESIAN_POINT ( 'NONE',  ( -7.825402957745081878, 7.899365992529268965, 3.271030448983517580 ) ) ;
#31061 = DIRECTION ( 'NONE',  ( -0.000000000000000000, -0.000000000000000000, -1.000000000000000000 ) ) ;
#31062 = CARTESIAN_POINT ( 'NONE',  ( 212.1700216741374447, 117.1889356120871213, -71.39816962747791251 ) ) ;
#31063 = DIRECTION ( 'NONE',  ( -1.000000000000000000, 0.000000000000000000, -0.000000000000000000 ) ) ;
#31064 = CARTESIAN_POINT ( 'NONE',  ( -89.99999999999998579, 1.102182119232617596E-14, -10.00000000000000000 ) ) ;
#31065 = ORIENTED_EDGE ( 'NONE', *, *, #50300, .T. ) ;
#31066 = VERTEX_POINT ( 'NONE', #56867 ) ;
#31067 = EDGE_CURVE ( 'NONE', #1172, #15636, #66745, .T. ) ;
#31068 = B_SPLINE_CURVE_WITH_KNOTS ( 'NONE', 3,
 ( #45770, #29577, #35560, #18690, #46102, #30286, #45413, #3540, #50692, #45061, #3212, #35906, #46444, #2856, #19028, #34874, #67572, #13751, #13073, #39795, #19371, #40480, #57019, #67925, #35209, #61926, #61599, #8485, #40829, #41182, #66547, #57359, #56313, #9170, #29933, #51045, #8836, #51400, #61253, #2512, #25706, #46799, #26041, #26386, #64011, #4919 ),
 .UNSPECIFIED., .F., .F.,
 ( 4, 2, 2, 2, 2, 2, 2, 2, 2, 2, 2, 2, 2, 2, 2, 2, 2, 2, 2, 2, 2, 2, 4 ),
 ( 0.02989107162308291682, 0.03170280136394029724, 0.03351453110479767072, 0.03532626084565505115, 0.03713799058651242463, 0.03894972032736980505, 0.03985558519779850567, 0.04076145006822720629, 0.04166731493865591385, 0.04257317980908461447, 0.04347904467951332202, 0.04438490954994202264, 0.04529077442037073020, 0.04619663929079943776, 0.04710250416122813838, 0.04800836903165683900, 0.04891423390208554656, 0.04982009877251425412, 0.05163182851337159290, 0.05344355825422893169, 0.05525528799508627742, 0.05706701773594362315, 0.05887874747680096194 ),
 .UNSPECIFIED. ) ;
#31069 = CARTESIAN_POINT ( 'NONE',  ( 173.5958500711059571, 72.73022245412229836, 91.08498831883019875 ) ) ;
#31070 = AXIS2_PLACEMENT_3D ( 'NONE', #59146, #10966, #48573 ) ;
#31071 = CYLINDRICAL_SURFACE ( 'NONE', #26168, 65.00000000000000000 ) ;
#31072 = CARTESIAN_POINT ( 'NONE',  ( -24.19091603582231542, 8.513464105188679909, -67.71881203971585705 ) ) ;
#31073 = EDGE_CURVE ( 'NONE', #33925, #8790, #30137, .T. ) ;
#31074 = ADVANCED_FACE ( 'NONE', ( #61446 ), #67770, .F. ) ;
#31075 = UNCERTAINTY_MEASURE_WITH_UNIT (LENGTH_MEASURE( 1.000000000000000082E-05 ), #69381, 'distance_accuracy_value', 'NONE');
#31076 = CARTESIAN_POINT ( 'NONE',  ( 15.78827728214693416, 6.500811158483284835, 3.170157082241545687 ) ) ;
#31077 = CYLINDRICAL_SURFACE ( 'NONE', #14328, 5.000000000000004441 ) ;
#31078 = DIRECTION ( 'NONE',  ( 1.000000000000000000, 0.000000000000000000, -0.000000000000000000 ) ) ;
#31079 = FACE_OUTER_BOUND ( 'NONE', #46396, .T. ) ;
#31080 = CARTESIAN_POINT ( 'NONE',  ( -173.5394735271662512, 87.59446374803710000, -49.71195716474999671 ) ) ;
#31081 = DIRECTION ( 'NONE',  ( -1.000000000000000000, 0.000000000000000000, -0.000000000000000000 ) ) ;
#31082 = CARTESIAN_POINT ( 'NONE',  ( -173.1211646369891071, 87.12891641440859303, 18.97714401617737678 ) ) ;
#31083 = CARTESIAN_POINT ( 'NONE',  ( 204.6977192012829789, 106.3443248447423599, -78.17048162308530834 ) ) ;
#31084 = CARTESIAN_POINT ( 'NONE',  ( -52.66507163626135934, 14.05394608175175364, 71.78805517841820460 ) ) ;
#31085 = ORIENTED_EDGE ( 'NONE', *, *, #51775, .T. ) ;
#31086 = CARTESIAN_POINT ( 'NONE',  ( 130.7457207912710828, 40.74300766298682674, 3.325828997484891580 ) ) ;
#31087 = CARTESIAN_POINT ( 'NONE',  ( -742.9236288613935812, -685.7537703392392814, 10.00000000000000000 ) ) ;
#31088 = CARTESIAN_POINT ( 'NONE',  ( -54.56685407443680447, 15.59259313022788085, 72.16187836339487660 ) ) ;
#31089 = CYLINDRICAL_SURFACE ( 'NONE', #35473, 7.500000000000013323 ) ;
#31090 = CARTESIAN_POINT ( 'NONE',  ( -53.14475157111024828, 14.17819596930906734, -49.97361403301091087 ) ) ;
#31091 = DIRECTION ( 'NONE',  ( 0.000000000000000000, 1.000000000000000000, -0.000000000000000000 ) ) ;
#31092 = DIRECTION ( 'NONE',  ( 0.000000000000000000, 0.000000000000000000, 1.000000000000000000 ) ) ;
#31093 = VERTEX_POINT ( 'NONE', #9027 ) ;
#31094 = EDGE_CURVE ( 'NONE', #15354, #48257, #30472, .T. ) ;
#31095 = CARTESIAN_POINT ( 'NONE',  ( 0.01678220609565910654, 0.7854258609844486649, 7.999999999999998224 ) ) ;
#31096 = CARTESIAN_POINT ( 'NONE',  ( -55.54058841405666413, 14.81234591756537711, 72.16187836339486239 ) ) ;
#31097 = ORIENTED_EDGE ( 'NONE', *, *, #68485, .T. ) ;
#31098 = VECTOR ( 'NONE', #55789, 1000.000000000000227 ) ;
#31099 = VERTEX_POINT ( 'NONE', #36441 ) ;
#31100 = CARTESIAN_POINT ( 'NONE',  ( 31.91241427070456993, 8.564321958137947277, 91.88119559238364786 ) ) ;
#31101 = DIRECTION ( 'NONE',  ( -0.000000000000000000, -0.000000000000000000, -1.000000000000000000 ) ) ;
#31102 = DIRECTION ( 'NONE',  ( 0.000000000000000000, 1.000000000000000000, -0.000000000000000000 ) ) ;
#31103 = ORIENTED_EDGE ( 'NONE', *, *, #41160, .F. ) ;
#31104 = VECTOR ( 'NONE', #51662, 999.9999999999998863 ) ;
#31105 = FACE_BOUND ( 'NONE', #52074, .T. ) ;
#31106 = DIRECTION ( 'NONE',  ( 0.7530714660036195163, -0.6579387259397027066, 0.000000000000000000 ) ) ;
#31107 = CARTESIAN_POINT ( 'NONE',  ( 33.44527180510250020, 7.709232309484722379, -20.85868167691871733 ) ) ;
#31108 = CARTESIAN_POINT ( 'NONE',  ( 173.7225111622555005, 72.84868911716898765, -42.26144479629255102 ) ) ;
#31109 = AXIS2_PLACEMENT_3D ( 'NONE', #63089, #62045, #31092 ) ;
#31110 = LINE ( 'NONE', #42679, #6897 ) ;
#31111 = CARTESIAN_POINT ( 'NONE',  ( 93.92280655489132357, 22.03989931749466535, 35.44608963825557169 ) ) ;
#31112 = CIRCLE ( 'NONE', #46969, 65.00000000000000000 ) ;
#31113 = ORIENTED_EDGE ( 'NONE', *, *, #52807, .F. ) ;
#31114 = CARTESIAN_POINT ( 'NONE',  ( 103.8325688302027459, 27.12251147381400784, -20.47917175127302869 ) ) ;
#31115 = AXIS2_PLACEMENT_3D ( 'NONE', #61213, #41146, #7758 ) ;
#31116 = CARTESIAN_POINT ( 'NONE',  ( 8.336882341125873452, 6.376438415325263342, 63.37576547410991878 ) ) ;
#31117 = DIRECTION ( 'NONE',  ( -0.9510565162951499785, -0.3090169943749582204, 0.000000000000000000 ) ) ;
#31118 = CARTESIAN_POINT ( 'NONE',  ( 197.2847860006354495, 98.30530166401516112, 35.55649062842450547 ) ) ;
#31119 = CARTESIAN_POINT ( 'NONE',  ( -71.43567564266649583, 20.76245642981890427, 89.58950873541245130 ) ) ;
#31121 = ORIENTED_EDGE ( 'NONE', *, *, #50441, .T. ) ;
#31120 = FACE_OUTER_BOUND ( 'NONE', #64572, .T. ) ;
#31122 = CARTESIAN_POINT ( 'NONE',  ( 157.4703587214989398, -170.0000000000000000, 63.75401806271707983 ) ) ;
#31123 = ORIENTED_EDGE ( 'NONE', *, *, #55332, .F. ) ;
#31124 = EDGE_CURVE ( 'NONE', #17942, #66072, #56115, .T. ) ;
#31126 = EDGE_LOOP ( 'NONE', ( #52310, #37276, #30446, #15278 ) ) ;
#31125 = EDGE_CURVE ( 'NONE', #41110, #11896, #52269, .T. ) ;
#31127 = CARTESIAN_POINT ( 'NONE',  ( 116.6436511186860514, 33.08230081168870385, -66.34972720225196952 ) ) ;
#31128 = DIRECTION ( 'NONE',  ( -0.9009688679024218105, 0.4338837391175525693, 0.000000000000000000 ) ) ;
#31129 = FACE_OUTER_BOUND ( 'NONE', #39169, .T. ) ;
#31130 = CARTESIAN_POINT ( 'NONE',  ( 181.0840389613909736, 78.60582251573006829, 71.15314469597512925 ) ) ;
#31131 = EDGE_CURVE ( 'NONE', #64093, #25266, #4091, .T. ) ;
#31132 = DIRECTION ( 'NONE',  ( 0.000000000000000000, 1.000000000000000000, -0.000000000000000000 ) ) ;
#31133 = CARTESIAN_POINT ( 'NONE',  ( -86.15466590221103615, 26.40813842494317498, -15.27875085681931999 ) ) ;
#31134 = CARTESIAN_POINT ( 'NONE',  ( 18.19980344696536889, 6.589834367837005047, -23.28036388989822925 ) ) ;
#31135 = ADVANCED_FACE ( 'NONE', ( #20949 ), #15332, .F. ) ;
#31136 = CARTESIAN_POINT ( 'NONE',  ( -152.5067928559255961, 66.76529500553621688, -49.20136729112984142 ) ) ;
#31137 = ORIENTED_EDGE ( 'NONE', *, *, #61076, .F. ) ;
#31138 = B_SPLINE_CURVE_WITH_KNOTS ( 'NONE', 3,
 ( #65830, #22550, #391, #38378 ),
 .UNSPECIFIED., .F., .F.,
 ( 4, 4 ),
 ( 0.1259919275528357530, 0.1829744153748744939 ),
 .UNSPECIFIED. ) ;
#31139 = ORIENTED_EDGE ( 'NONE', *, *, #28925, .T. ) ;
#31140 = LINE ( 'NONE', #10020, #9612 ) ;
#31141 = EDGE_CURVE ( 'NONE', #26264, #26262, #20853, .T. ) ;
#31142 = DIRECTION ( 'NONE',  ( 1.000000000000000000, 0.000000000000000000, 0.000000000000000000 ) ) ;
#31143 = CARTESIAN_POINT ( 'NONE',  ( 110.6184472392236700, 29.05585583753637735, 83.30291117284286884 ) ) ;
#31144 = CARTESIAN_POINT ( 'NONE',  ( -149.5074843970971017, 65.50121172469319220, 18.87627064943540134 ) ) ;
#31145 = EDGE_CURVE ( 'NONE', #35508, #34656, #33247, .T. ) ;
#31147 = CARTESIAN_POINT ( 'NONE',  ( 181.5127080940606561, 79.03904173130084132, -36.22505766587960352 ) ) ;
#31146 = VECTOR ( 'NONE', #54056, 1000.000000000000114 ) ;
#31148 = DIRECTION ( 'NONE',  ( -0.000000000000000000, -0.000000000000000000, -1.000000000000000000 ) ) ;
#31149 = CARTESIAN_POINT ( 'NONE',  ( -156.7943706409895412, 71.98431607767156493, 93.71821196632575379 ) ) ;
#31150 = ORIENTED_EDGE ( 'NONE', *, *, #45340, .T. ) ;
#31151 = ORIENTED_EDGE ( 'NONE', *, *, #22330, .T. ) ;
#31152 = ORIENTED_EDGE ( 'NONE', *, *, #13797, .F. ) ;
#31153 = AXIS2_PLACEMENT_3D ( 'NONE', #45765, #24321, #39791 ) ;
#31154 = PRESENTATION_STYLE_ASSIGNMENT (( #35736 ) ) ;
#31155 = CARTESIAN_POINT ( 'NONE',  ( -80.55742067659893735, 23.05042616197515670, 57.48945466102705382 ) ) ;
#31156 = EDGE_CURVE ( 'NONE', #63882, #42425, #37815, .T. ) ;
#31157 = CARTESIAN_POINT ( 'NONE',  ( 103.3213573731405290, 25.80935123464501046, -94.19314425201019958 ) ) ;
#31158 = ADVANCED_FACE ( 'NONE', ( #32536 ), #49396, .F. ) ;
#31159 = CARTESIAN_POINT ( 'NONE',  ( -37.52119286077851967, 11.69341290629617802, -74.05703107814400710 ) ) ;
#31160 = CARTESIAN_POINT ( 'NONE',  ( -150.3898662070192245, 64.92828409760431896, -7.968279941028269420 ) ) ;
#31161 = AXIS2_PLACEMENT_3D ( 'NONE', #63544, #21311, #63885 ) ;
#31162 = CARTESIAN_POINT ( 'NONE',  ( 38.42020198992004509, 8.283430712587442457, 56.80691058368965685 ) ) ;
#31163 = CARTESIAN_POINT ( 'NONE',  ( 11.82322073186613487, 6.406156243758799107, -22.54526628955453660 ) ) ;
#31164 = AXIS2_PLACEMENT_3D ( 'NONE', #22656, #65580, #17372 ) ;
#31165 = CARTESIAN_POINT ( 'NONE',  ( -7.330690860789850660, 6.858814156830897346, -35.41807073194382838 ) ) ;
#31166 = CARTESIAN_POINT ( 'NONE',  ( 32.67633850029795184, 58.08495024160666276, 34.48241795236665297 ) ) ;
#31167 = CARTESIAN_POINT ( 'NONE',  ( -125.4481990864045002, 46.20056605584954923, 3.775397282693378820 ) ) ;
#31168 = CARTESIAN_POINT ( 'NONE',  ( 69.50572373348798294, 14.27208627753790005, -66.27431351737995158 ) ) ;
#31169 = CARTESIAN_POINT ( 'NONE',  ( 131.6005058089755835, 40.07838125795770878, -23.84668524735129225 ) ) ;
#31170 = B_SPLINE_CURVE_WITH_KNOTS ( 'NONE', 3,
 ( #495, #43396, #31817, #38123, #5077, #47976, #9681, #63485, #52579, #21258, #15300, #36755, #64166, #37429, #4398, #52909, #4731, #55701, #6473, #54993, #28626, #28983, #12802, #44446, #59566, #6814, #11382, #32850, #50078, #28264, #7171, #23000, #65935, #50430, #12447, #33906 ),
 .UNSPECIFIED., .F., .F.,
 ( 4, 2, 2, 2, 2, 2, 2, 2, 2, 2, 2, 2, 2, 2, 2, 2, 2, 4 ),
 ( 3.469446951953614189E-18, 0.001545474820159053976, 0.003090949640318104482, 0.004636424460477154771, 0.006181899280636205495, 0.007727374100795257085, 0.008500111510874769002, 0.009272848920954281787, 0.01081832374111331256, 0.01236379856127234160, 0.01390927338143137064, 0.01545474820159039968, 0.01700022302174943045, 0.01854569784190845602, 0.02009117266206748506, 0.02163664748222651410, 0.02318212230238553273, 0.02472759712254455483 ),
 .UNSPECIFIED. ) ;
#31171 = CARTESIAN_POINT ( 'NONE',  ( 17.72748965151693312, 7.577488030789624851, -8.925253431473967325 ) ) ;
#31172 = CARTESIAN_POINT ( 'NONE',  ( 8.336237313193164411, 7.382629160459398321, 11.64778143086688011 ) ) ;
#31173 = VECTOR ( 'NONE', #40540, 1000.000000000000000 ) ;
#31174 = ORIENTED_EDGE ( 'NONE', *, *, #52390, .T. ) ;
#31175 = DIRECTION ( 'NONE',  ( -0.000000000000000000, 1.000000000000000000, -0.000000000000000000 ) ) ;
#31176 = PRODUCT_CONTEXT ( 'NONE', #3532, 'mechanical' ) ;
#31177 = CARTESIAN_POINT ( 'NONE',  ( 173.9413349464226997, 71.67637800842355489, 34.50366122527430690 ) ) ;
#31178 = CARTESIAN_POINT ( 'NONE',  ( -40.24154210098712525, -63.23235722614506216, 41.38025477438755928 ) ) ;
#31179 = CARTESIAN_POINT ( 'NONE',  ( 42.03492317486904994, 8.766487167902388578, -76.99122434333160925 ) ) ;
#31180 = CARTESIAN_POINT ( 'NONE',  ( 184.9757174666827382, 84.09845285279334348, -50.14020102364498399 ) ) ;
#31181 = ORIENTED_EDGE ( 'NONE', *, *, #23426, .T. ) ;
#31182 = VERTEX_POINT ( 'NONE', #529 ) ;
#31183 = CARTESIAN_POINT ( 'NONE',  ( -24.70911172866234295, 8.583078995053023519, -19.31926905173414966 ) ) ;
#31184 = CARTESIAN_POINT ( 'NONE',  ( 200.8303160266299301, 102.8412051751308809, 16.30336876723097106 ) ) ;
#31185 = ORIENTED_EDGE ( 'NONE', *, *, #42540, .F. ) ;
#31186 = CARTESIAN_POINT ( 'NONE',  ( 113.8748103246145575, 30.59837980920004696, 70.53553382418881768 ) ) ;
#31187 = VERTEX_POINT ( 'NONE', #21977 ) ;
#31188 = CARTESIAN_POINT ( 'NONE',  ( -133.3122825023497171, -170.0000000000000000, -95.00000000000133582 ) ) ;
#31189 = DIRECTION ( 'NONE',  ( 1.000000000000000000, 0.000000000000000000, 0.000000000000000000 ) ) ;
#31190 = CARTESIAN_POINT ( 'NONE',  ( 0.000000000000000000, 0.000000000000000000, 0.000000000000000000 ) ) ;
#31191 = CARTESIAN_POINT ( 'NONE',  ( 0.000000000000000000, 0.000000000000000000, -9.474599999999998801 ) ) ;
#31192 = CARTESIAN_POINT ( 'NONE',  ( 0.000000000000000000, 0.000000000000000000, 41.38025477438755928 ) ) ;
#31194 = ORIENTED_EDGE ( 'NONE', *, *, #33532, .F. ) ;
#31193 = PLANE ( 'NONE',  #23028 ) ;
#31195 = DIRECTION ( 'NONE',  ( 0.000000000000000000, 0.000000000000000000, 1.000000000000000000 ) ) ;
#31196 = ORIENTED_EDGE ( 'NONE', *, *, #22396, .T. ) ;
#31197 = VERTEX_POINT ( 'NONE', #44116 ) ;
#31198 = VECTOR ( 'NONE', #28191, 1000.000000000000000 ) ;
#31199 = CARTESIAN_POINT ( 'NONE',  ( -119.1795380580999790, 42.22910606512925114, -18.92106183394395202 ) ) ;
#31200 = CARTESIAN_POINT ( 'NONE',  ( 412.3372781065085633, 179.4906275429376024, 113.5502958579881749 ) ) ;
#31201 = CARTESIAN_POINT ( 'NONE',  ( -175.1920326508032701, 89.46239303019291356, -22.58843696369808285 ) ) ;
#31202 = VECTOR ( 'NONE', #44836, 1000.000000000000000 ) ;
#31204 = ORIENTED_EDGE ( 'NONE', *, *, #55175, .F. ) ;
#31203 = CARTESIAN_POINT ( 'NONE',  ( -131.2955621888335429, 51.38237199780174080, 59.73917619575056648 ) ) ;
#31205 = CARTESIAN_POINT ( 'NONE',  ( 62.53356220515463093, 13.59349015304564467, 2.968410348757589023 ) ) ;
#31206 = PLANE ( 'NONE',  #55295 ) ;
#31207 = VECTOR ( 'NONE', #42929, 1000.000000000000000 ) ;
#31208 = VERTEX_POINT ( 'NONE', #38871 ) ;
#31209 = CARTESIAN_POINT ( 'NONE',  ( 0.000000000000000000, 0.000000000000000000, 170.0000000000000000 ) ) ;
#31210 = ADVANCED_FACE ( 'NONE', ( #43770 ), #11414, .T. ) ;
#31211 = VECTOR ( 'NONE', #64068, 1000.000000000000000 ) ;
#31212 = CARTESIAN_POINT ( 'NONE',  ( -126.8016613879753578, 48.30316697011514293, -61.79973845963801438 ) ) ;
#31213 = DIRECTION ( 'NONE',  ( -0.000000000000000000, 0.000000000000000000, -1.000000000000000000 ) ) ;
#31214 = DIRECTION ( 'NONE',  ( -0.000000000000000000, 1.000000000000000000, -0.000000000000000000 ) ) ;
#31215 = DIRECTION ( 'NONE',  ( -0.000000000000000000, -0.000000000000000000, -1.000000000000000000 ) ) ;
#31216 = ORIENTED_EDGE ( 'NONE', *, *, #51063, .F. ) ;
#31217 = ORIENTED_EDGE ( 'NONE', *, *, #37302, .F. ) ;
#31218 = EDGE_CURVE ( 'NONE', #35061, #17896, #38507, .T. ) ;
#31219 = DIRECTION ( 'NONE',  ( 0.000000000000000000, 0.000000000000000000, 1.000000000000000000 ) ) ;
#31220 = LINE ( 'NONE', #52651, #32308 ) ;
#31221 = FACE_BOUND ( 'NONE', #33575, .T. ) ;
#31222 = CARTESIAN_POINT ( 'NONE',  ( -190.6985136298601731, 109.1272424661242582, 94.99999999999866418 ) ) ;
#31223 = DIRECTION ( 'NONE',  ( 1.000000000000000000, 0.000000000000000000, 0.000000000000000000 ) ) ;
#31224 = CARTESIAN_POINT ( 'NONE',  ( 80.72161230109726660, 17.48902961068030137, 32.56519435810803742 ) ) ;
#31225 = CARTESIAN_POINT ( 'NONE',  ( -143.2464978228200039, 59.04559547356111437, 42.35829187257395745 ) ) ;
#31226 = CARTESIAN_POINT ( 'NONE',  ( 15.78827728214693416, -170.0000000000000000, -62.36349468914946925 ) ) ;
#31227 = CARTESIAN_POINT ( 'NONE',  ( -165.7143741370937278, 79.24519349471960084, -70.27428026180706411 ) ) ;
#31228 = ORIENTED_EDGE ( 'NONE', *, *, #64969, .T. ) ;
#31229 = CARTESIAN_POINT ( 'NONE',  ( -109.7290872258107157, 36.72869630780160577, -16.68929740702757769 ) ) ;
#31230 = ORIENTED_EDGE ( 'NONE', *, *, #45253, .F. ) ;
#31231 = CARTESIAN_POINT ( 'NONE',  ( 80.92695752160176426, 18.60786019495465027, -92.06836682371273639 ) ) ;
#31232 =( LENGTH_UNIT ( ) NAMED_UNIT ( * ) SI_UNIT ( .MILLI., .METRE. ) );
#31233 = LINE ( 'NONE', #56928, #50936 ) ;
#31234 = EDGE_CURVE ( 'NONE', #62926, #30795, #59952, .T. ) ;
#31235 = DIRECTION ( 'NONE',  ( -0.000000000000000000, -0.000000000000000000, -1.000000000000000000 ) ) ;
#31236 = DIRECTION ( 'NONE',  ( -0.8118923937861950435, -0.5838071093367415143, 0.000000000000000000 ) ) ;
#31237 = DIRECTION ( 'NONE',  ( -4.270088556250601699E-16, -0.000000000000000000, -1.000000000000000000 ) ) ;
#31238 = CARTESIAN_POINT ( 'NONE',  ( 36.99625334683018707, 8.108440754877204171, 3.448660572988824669 ) ) ;
#31239 = CARTESIAN_POINT ( 'NONE',  ( -34.96012151086436859, -55.23134702900938464, 41.38025477438755928 ) ) ;
#31240 = CARTESIAN_POINT ( 'NONE',  ( -35.99414836699283882, 11.40630460607620122, -21.95128177927970725 ) ) ;
#31241 = VERTEX_POINT ( 'NONE', #65242 ) ;
#31242 = VECTOR ( 'NONE', #62056, 1000.000000000000000 ) ;
#31243 = CARTESIAN_POINT ( 'NONE',  ( -122.1170451552604277, 45.24844212239635510, -89.61962605176735508 ) ) ;
#31244 = EDGE_LOOP ( 'NONE', ( #28851, #6144, #60718, #13238 ) ) ;
#31245 = DIRECTION ( 'NONE',  ( -0.000000000000000000, 1.000000000000000000, 0.000000000000000000 ) ) ;
#31246 = CARTESIAN_POINT ( 'NONE',  ( 8.288696687633803961, 7.382586467017839382, -70.36437873598936221 ) ) ;
#31247 = CARTESIAN_POINT ( 'NONE',  ( -23.98903001682803904, 8.486614814224626713, 9.877694052388251933 ) ) ;
#31248 = CARTESIAN_POINT ( 'NONE',  ( 211.7634543339367781, -170.0000000000000000, -95.00000000000133582 ) ) ;
#31249 = CARTESIAN_POINT ( 'NONE',  ( -11.57808265946730231, 7.164483090579921942, -76.26091628640612896 ) ) ;
#31250 = CARTESIAN_POINT ( 'NONE',  ( -95.50384525802330415, 29.46973564057718065, -12.44541413338938440 ) ) ;
#31251 =( BOUNDED_CURVE ( )  B_SPLINE_CURVE ( 3, ( #15754, #57640, #10470, #47750 ),
 .UNSPECIFIED., .F., .F. ) 
 B_SPLINE_CURVE_WITH_KNOTS ( ( 4, 4 ),
 ( 1.570796326794897002, 3.141592653589793560 ),
 .UNSPECIFIED. ) 
 CURVE ( )  GEOMETRIC_REPRESENTATION_ITEM ( )  RATIONAL_B_SPLINE_CURVE ( ( 1.000000000000000000, 0.8047378541243649375, 0.8047378541243649375, 1.000000000000000000 ) ) 
 REPRESENTATION_ITEM ( '' )  );
#31252 = CIRCLE ( 'NONE', #49178, 5.000000000000000888 ) ;
#31253 = CARTESIAN_POINT ( 'NONE',  ( 156.5993887774280324, 58.24868799840906064, -51.07665877090285989 ) ) ;
#31254 = AXIS2_PLACEMENT_3D ( 'NONE', #345, #37990, #16536 ) ;
#31255 = ORIENTED_EDGE ( 'NONE', *, *, #24546, .F. ) ;
#31256 = DIRECTION ( 'NONE',  ( 0.9108602745606095841, 0.4127148655274864297, -7.174295345542695177E-15 ) ) ;
#31257 = DIRECTION ( 'NONE',  ( 0.1342332658176522420, 0.9909497617679352555, -0.000000000000000000 ) ) ;
#31258 = CARTESIAN_POINT ( 'NONE',  ( 176.6238742729555611, 75.60943990211369226, -22.92894773880436077 ) ) ;
#31259 = FACE_OUTER_BOUND ( 'NONE', #64042, .T. ) ;
#31260 = CARTESIAN_POINT ( 'NONE',  ( -55.05276343752910151, 14.68156374112636264, -50.21632399845989170 ) ) ;
#31261 = ORIENTED_EDGE ( 'NONE', *, *, #33936, .T. ) ;
#31262 = DIRECTION ( 'NONE',  ( 0.000000000000000000, 0.000000000000000000, 1.000000000000000000 ) ) ;
#31263 = CARTESIAN_POINT ( 'NONE',  ( -0.5158933718595597462, 6.525180340836103099, -14.37622864181621374 ) ) ;
#31264 = CARTESIAN_POINT ( 'NONE',  ( 201.5987353083855567, 103.8544727311227263, -23.82465923633973048 ) ) ;
#31265 = CARTESIAN_POINT ( 'NONE',  ( -148.5360305860837116, 63.35984549844194902, 84.46819988047289485 ) ) ;
#31266 = CIRCLE ( 'NONE', #12174, 5.000000000000004441 ) ;
#31267 = CARTESIAN_POINT ( 'NONE',  ( 139.3067271572849677, 44.81402783181198402, 42.16869312922494117 ) ) ;
#31268 = ORIENTED_EDGE ( 'NONE', *, *, #32168, .T. ) ;
#31269 = LINE ( 'NONE', #15079, #64867 ) ;
#31270 = CARTESIAN_POINT ( 'NONE',  ( 113.4351684956570097, 30.38657459074489253, -77.07004752621021737 ) ) ;
#31271 = CARTESIAN_POINT ( 'NONE',  ( 181.0840389613909736, 80.03940679743415387, 44.30859410551141764 ) ) ;
#31272 = CARTESIAN_POINT ( 'NONE',  ( 156.5993887774280324, 58.24868799840906064, 29.45699300048817193 ) ) ;
#31273 = LINE ( 'NONE', #52700, #1581 ) ;
#31274 = ORIENTED_EDGE ( 'NONE', *, *, #18267, .T. ) ;
#31275 = EDGE_CURVE ( 'NONE', #50282, #50676, #45177, .T. ) ;
#31276 = CARTESIAN_POINT ( 'NONE',  ( 176.6238742729555327, 75.60943990211367804, 57.60470403258671013 ) ) ;
#31277 = ORIENTED_EDGE ( 'NONE', *, *, #63552, .F. ) ;
#31278 = EDGE_CURVE ( 'NONE', #24269, #18376, #46209, .T. ) ;
#31279 = CARTESIAN_POINT ( 'NONE',  ( -76.32962633615589709, 21.44528079176261670, -22.90158379948196199 ) ) ;
#31280 = CARTESIAN_POINT ( 'NONE',  ( 70.25990036603477051, 14.47042233282418700, -68.10757834462343396 ) ) ;
#31281 = CARTESIAN_POINT ( 'NONE',  ( -56.02027488966933078, 14.94257193099086045, 45.27018892150354645 ) ) ;
#31283 = ORIENTED_EDGE ( 'NONE', *, *, #52628, .T. ) ;
#31282 = CARTESIAN_POINT ( 'NONE',  ( 150.2941978382489197, 53.52137138947625061, 7.867929705122802986 ) ) ;
#31284 = CARTESIAN_POINT ( 'NONE',  ( -180.0175713311536470, 95.14770835574078944, 35.35984136943162071 ) ) ;
#31285 = DIRECTION ( 'NONE',  ( -1.000000000000000000, 0.000000000000000000, 0.000000000000000000 ) ) ;
#31286 = LINE ( 'NONE', #52715, #21547 ) ;
#31287 = VERTEX_POINT ( 'NONE', #40254 ) ;
#31288 = LINE ( 'NONE', #31971, #65927 ) ;
#31289 = ADVANCED_FACE ( 'NONE', ( #61701 ), #66317, .F. ) ;
#31290 = EDGE_CURVE ( 'NONE', #30681, #38509, #52525, .T. ) ;
#31291 = CIRCLE ( 'NONE', #7697, 89.99999999999998579 ) ;
#31292 = CARTESIAN_POINT ( 'NONE',  ( 109.9975424824652777, 296.0000000000000000, 418.0000000000000000 ) ) ;
#31293 = CARTESIAN_POINT ( 'NONE',  ( 140.4897729434290170, 45.57634363643750675, 67.39407047049898836 ) ) ;
#31294 = DIRECTION ( 'NONE',  ( -0.000000000000000000, 1.000000000000000000, -0.000000000000000000 ) ) ;
#31295 = CYLINDRICAL_SURFACE ( 'NONE', #65063, 2.999999999999999112 ) ;
#31296 = DIRECTION ( 'NONE',  ( 1.000000000000000000, 0.000000000000000000, 0.000000000000000000 ) ) ;
#31297 = ORIENTED_EDGE ( 'NONE', *, *, #64162, .T. ) ;
#31298 = VECTOR ( 'NONE', #6326, 1000.000000000000000 ) ;
#31299 = FACE_OUTER_BOUND ( 'NONE', #15517, .T. ) ;
#31300 = ORIENTED_EDGE ( 'NONE', *, *, #55674, .T. ) ;
#31301 = EDGE_CURVE ( 'NONE', #50848, #925, #2619, .T. ) ;
#31302 = DIRECTION ( 'NONE',  ( -0.8805955318567321166, -0.4738686624730094055, 0.000000000000000000 ) ) ;
#31303 = CARTESIAN_POINT ( 'NONE',  ( 211.8345664497466316, 118.5225165986914533, -19.30918099180828307 ) ) ;
#31304 = CARTESIAN_POINT ( 'NONE',  ( 103.0124792097646491, 26.77148435100181345, 35.05276459316780091 ) ) ;
#31305 = DIRECTION ( 'NONE',  ( -0.000000000000000000, -0.000000000000000000, -1.000000000000000000 ) ) ;
#31306 = DIRECTION ( 'NONE',  ( 0.7660444431189771253, 0.6427876096865404731, 1.661094098900087138E-16 ) ) ;
#31307 = CARTESIAN_POINT ( 'NONE',  ( 187.8973304652193690, 87.27378997243177139, 6.817108339809598405 ) ) ;
#31308 = CARTESIAN_POINT ( 'NONE',  ( 205.5105258529713410, 107.4632495673648691, -36.35903942194123317 ) ) ;
#31309 = CARTESIAN_POINT ( 'NONE',  ( -6.214074333988410359, 32.84308755423718651, 6.893343212288937316 ) ) ;
#31310 = ORIENTED_EDGE ( 'NONE', *, *, #5761, .F. ) ;
#31311 = CARTESIAN_POINT ( 'NONE',  ( -417.6627218934913230, 219.4906275429376308, 113.5502958579881749 ) ) ;
#31312 = ORIENTED_EDGE ( 'NONE', *, *, #68526, .F. ) ;
#31313 = CARTESIAN_POINT ( 'NONE',  ( -73.80418150970712077, 21.59712875466424009, 59.03090319298773636 ) ) ;
#31314 = CARTESIAN_POINT ( 'NONE',  ( -7.916219337932451694, 70.00000000000000000, 6.110112224316693208 ) ) ;
#31315 = EDGE_CURVE ( 'NONE', #53910, #20254, #30051, .T. ) ;
#31316 = CARTESIAN_POINT ( 'NONE',  ( 55.61382797299290104, 11.07686102552915486, -71.30009820847813273 ) ) ;
#31317 = DIRECTION ( 'NONE',  ( -0.000000000000000000, -0.000000000000000000, 1.000000000000000000 ) ) ;
#31318 = DIRECTION ( 'NONE',  ( -0.000000000000000000, -1.000000000000000000, -0.000000000000000000 ) ) ;
#31319 = CARTESIAN_POINT ( 'NONE',  ( -2.101755354351193539, 6.585774088635568901, 86.44700550218486512 ) ) ;
#31320 = EDGE_CURVE ( 'NONE', #23841, #55226, #34651, .T. ) ;
#31321 = EDGE_CURVE ( 'NONE', #43258, #13094, #18105, .T. ) ;
#31322 = CARTESIAN_POINT ( 'NONE',  ( 164.9547823171479877, 65.03046442419432083, -71.02841637048652501 ) ) ;
#31323 = ORIENTED_EDGE ( 'NONE', *, *, #23136, .T. ) ;
#31324 = DIRECTION ( 'NONE',  ( -1.850371928290090422E-16, 1.000000000000000000, 1.110223024625156171E-16 ) ) ;
#31325 = CARTESIAN_POINT ( 'NONE',  ( 200.2082720696348588, 100.3848492891406750, -91.49428350888068451 ) ) ;
#31326 = EDGE_LOOP ( 'NONE', ( #6665, #26349, #67446, #6952 ) ) ;
#31327 = ORIENTED_EDGE ( 'NONE', *, *, #52357, .T. ) ;
#31328 = DIRECTION ( 'NONE',  ( 1.000000000000000000, 0.000000000000000000, 0.000000000000000000 ) ) ;
#31329 = DIRECTION ( 'NONE',  ( -1.000000000000000000, 0.000000000000000000, 0.000000000000000000 ) ) ;
#31330 = DIRECTION ( 'NONE',  ( 0.000000000000000000, -1.000000000000000000, 0.000000000000000000 ) ) ;
#31331 = CARTESIAN_POINT ( 'NONE',  ( 0.000000000000000000, -27.00000000000000355, -0.000000000000000000 ) ) ;
#31332 = ORIENTED_EDGE ( 'NONE', *, *, #53903, .F. ) ;
#31333 = CARTESIAN_POINT ( 'NONE',  ( -131.3096895243910751, 51.39228038925230635, 43.33102018556300550 ) ) ;
#31334 = EDGE_LOOP ( 'NONE', ( #49714, #7266, #19075, #28788 ) ) ;
#31335 = CARTESIAN_POINT ( 'NONE',  ( 15.78827728214693416, 7.507518794609589818, -50.51894409868581448 ) ) ;
#31336 = CARTESIAN_POINT ( 'NONE',  ( 11.81843724556920883, 7.412394300769734379, 70.72722298566459642 ) ) ;
#31337 = DIRECTION ( 'NONE',  ( 0.000000000000000000, 0.000000000000000000, -1.000000000000000000 ) ) ;
#31338 = CARTESIAN_POINT ( 'NONE',  ( -2.699999999999990408, 2.449293598294706119E-15, 19.99999999999999645 ) ) ;
#31339 = VERTEX_POINT ( 'NONE', #8244 ) ;
#31340 = AXIS2_PLACEMENT_3D ( 'NONE', #32894, #22343, #43437 ) ;
#31341 = VERTEX_POINT ( 'NONE', #40942 ) ;
#31342 = CARTESIAN_POINT ( 'NONE',  ( 114.4935831913009565, -21.89011901571377194, 2.216886222927851868 ) ) ;
#31343 = CARTESIAN_POINT ( 'NONE',  ( -132.6811329440527061, 52.36246882380746115, 94.99999999999866418 ) ) ;
#31344 = CARTESIAN_POINT ( 'NONE',  ( -166.3188283541501846, 79.86268666707378827, -18.53829102832942510 ) ) ;
#31345 = DIRECTION ( 'NONE',  ( 0.9561276726666719794, 0.000000000000000000, 0.2929502919626694180 ) ) ;
#31346 = CARTESIAN_POINT ( 'NONE',  ( 67.92995549349549833, 13.86623459444476758, 31.62639109689230921 ) ) ;
#31347 = CARTESIAN_POINT ( 'NONE',  ( 8.368703124675214156, 7.382636543903409176, 89.92552182398135585 ) ) ;
#31348 = B_SPLINE_CURVE_WITH_KNOTS ( 'NONE', 3,
 ( #8553, #24038, #55335, #39518, #13143, #44796, #39179, #51464, #28974, #19094, #12791, #61661, #40548, #28619, #60622, #34607, #7860, #2240, #22992, #50759, #50068, #45479, #45832, #29308, #44436, #39861, #65925, #12438, #18068, #60966, #61999, #67308, #2580, #1899, #66961, #8202, #55691, #24390, #23689, #23353, #34940, #56381, #51115, #13815, #33897 ),
 .UNSPECIFIED., .F., .F.,
 ( 4, 2, 2, 2, 2, 2, 2, 2, 1, 2, 2, 2, 2, 2, 2, 2, 2, 2, 2, 2, 2, 2, 4 ),
 ( 1.734723475976807094E-18, 0.001467747071934204835, 0.002201620607901308771, 0.002935494143868413140, 0.004403241215802621011, 0.005870988287736829750, 0.007338735359671038488, 0.008072608895638135051, 0.008806482431605229880, 0.009540355967572328177, 0.01027422950353942301, 0.01174197657547363521, 0.01247585011144074219, 0.01320972364740784742, 0.01467747071934208045, 0.01541134425530918742, 0.01614521779127629092, 0.01761296486321051874, 0.01908071193514474656, 0.01981458547111185353, 0.02054845900707896744, 0.02201620607901318832, 0.02348395315094740227 ),
 .UNSPECIFIED. ) ;
#31349 = ORIENTED_EDGE ( 'NONE', *, *, #47317, .T. ) ;
#31350 = EDGE_CURVE ( 'NONE', #3906, #11364, #29349, .T. ) ;
#31351 = CARTESIAN_POINT ( 'NONE',  ( -1.224646799147352468E-15, 16.00000000000000000, 6.196318915105386793 ) ) ;
#31352 = CARTESIAN_POINT ( 'NONE',  ( -99.98930671699733352, 31.63190627461931470, 57.70662428919617071 ) ) ;
#31353 = ORIENTED_EDGE ( 'NONE', *, *, #44062, .T. ) ;
#31354 = CARTESIAN_POINT ( 'NONE',  ( -83.52505811737952968, 24.23179517241435121, 5.338914906993961651 ) ) ;
#31355 = ORIENTED_EDGE ( 'NONE', *, *, #8078, .T. ) ;
#31356 = EDGE_CURVE ( 'NONE', #34646, #65008, #24084, .T. ) ;
#31357 = B_SPLINE_CURVE_WITH_KNOTS ( 'NONE', 3,
 ( #40957, #46572, #37391, #48972, #21560, #43357, #45016, #18290, #27183, #59186, #21229, #48615, #64831, #13030, #26504, #43004, #64478, #38086, #50307, #16292, #11008, #12669, #66158, #59530, #23238, #5724, #64130, #15946, #32471, #17949, #39749, #11348, #34134, #61204, #39400, #53212, #53904, #60849, #58845, #48275, #5042, #47941, #16630, #10659, #26849, #21910, #103 ),
 .UNSPECIFIED., .F., .F.,
 ( 4, 2, 2, 2, 2, 2, 2, 2, 2, 2, 2, 2, 1, 2, 2, 2, 2, 2, 2, 2, 2, 2, 2, 4 ),
 ( 0.000000000000000000, 0.001493793014771646350, 0.002240689522157466706, 0.002987586029543287496, 0.004481379044314894380, 0.005228275551700687848, 0.005975172059086479581, 0.007468965073858052639, 0.008215861581243833964, 0.008962758088629617023, 0.01045655110340117273, 0.01120344761078695232, 0.01195034411817272844, 0.01269724062555850803, 0.01344413713294428762, 0.01493793014771584333, 0.01568482665510159690, 0.01643172316248735221, 0.01792551617725889404, 0.01941930919203043934, 0.02016620569941620852, 0.02091310220680198811, 0.02240689522157354729, 0.02390068823634510647 ),
 .UNSPECIFIED. ) ;
#31358 = VERTEX_POINT ( 'NONE', #28661 ) ;
#31359 = EDGE_LOOP ( 'NONE', ( #54915, #41905, #11024, #69509 ) ) ;
#31360 = CARTESIAN_POINT ( 'NONE',  ( -124.9915686518654638, 47.10215472274615678, 18.77539728269343300 ) ) ;
#31361 = CARTESIAN_POINT ( 'NONE',  ( -178.2381786520593323, 93.01028335822120141, 70.65477212569948051 ) ) ;
#31362 = CARTESIAN_POINT ( 'NONE',  ( 19.11168290073778664, 6.629794975642856691, 17.39810640889013982 ) ) ;
#31363 = ORIENTED_EDGE ( 'NONE', *, *, #47455, .F. ) ;
#31364 = EDGE_CURVE ( 'NONE', #26796, #46943, #50803, .T. ) ;
#31365 = EDGE_CURVE ( 'NONE', #19302, #36305, #26719, .T. ) ;
#31366 = EDGE_CURVE ( 'NONE', #44661, #4035, #45525, .T. ) ;
#31367 = CARTESIAN_POINT ( 'NONE',  ( -25.76662357285300686, 8.728786737612503899, 86.48839091911142418 ) ) ;
#31368 = CARTESIAN_POINT ( 'NONE',  ( 150.0889146124742979, 52.13243511955543852, 35.55320488847186766 ) ) ;
#31369 = CARTESIAN_POINT ( 'NONE',  ( -450.6627218934913230, 217.8591479523843475, -111.4497041420117966 ) ) ;
#31370 = DIRECTION ( 'NONE',  ( -0.000000000000000000, -0.000000000000000000, -1.000000000000000000 ) ) ;
#31371 = ADVANCED_FACE ( 'NONE', ( #29695 ), #51161, .F. ) ;
#31372 = CARTESIAN_POINT ( 'NONE',  ( -29.51060362117876679, 9.282716514427262311, 30.46451046403358731 ) ) ;
#31373 = CARTESIAN_POINT ( 'NONE',  ( -146.5309471467635944, 62.99917515507669208, -62.26958893730678568 ) ) ;
#31374 = ORIENTED_EDGE ( 'NONE', *, *, #27295, .F. ) ;
#31375 = DIRECTION ( 'NONE',  ( -0.000000000000000000, -1.000000000000000000, -0.000000000000000000 ) ) ;
#31376 = CARTESIAN_POINT ( 'NONE',  ( -82.33596576276349310, 24.83688096733768447, -62.90096193187974194 ) ) ;
#31377 = DIRECTION ( 'NONE',  ( 0.000000000000000000, -1.000000000000000000, 0.000000000000000000 ) ) ;
#31378 = CARTESIAN_POINT ( 'NONE',  ( -60.41792053122280493, 24.01035990323434177, 3.061616997868437868E-16 ) ) ;
#31379 = DIRECTION ( 'NONE',  ( 0.000000000000000000, 0.000000000000000000, 1.000000000000000000 ) ) ;
#31380 = CARTESIAN_POINT ( 'NONE',  ( 133.8566784816069628, 41.42467568809806977, 17.66579024853170310 ) ) ;
#31381 = CARTESIAN_POINT ( 'NONE',  ( -157.0069704378501854, 70.81086990254190994, 11.95845096291080800 ) ) ;
#31382 = CARTESIAN_POINT ( 'NONE',  ( -124.9915686518654496, 47.10215472274615678, -61.75825448869760237 ) ) ;
#31383 = CARTESIAN_POINT ( 'NONE',  ( 63.49940197359695304, 12.78497925206075614, 2.968410348757586803 ) ) ;
#31384 = PLANE ( 'NONE',  #32154 ) ;
#31385 = CARTESIAN_POINT ( 'NONE',  ( -109.0297561673456386, 36.34391931706015555, 41.29912065558960421 ) ) ;
#31386 = ORIENTED_EDGE ( 'NONE', *, *, #17114, .T. ) ;
#31387 = CARTESIAN_POINT ( 'NONE',  ( -51.71962244998664460, 14.85104855202525087, 84.78028665116053730 ) ) ;
#31388 = ORIENTED_EDGE ( 'NONE', *, *, #15301, .F. ) ;
#31389 = CARTESIAN_POINT ( 'NONE',  ( -442.9415673952016732, 394.9999999999997726, 92.47907109491421807 ) ) ;
#31390 = ORIENTED_EDGE ( 'NONE', *, *, #61830, .F. ) ;
#31391 = AXIS2_PLACEMENT_3D ( 'NONE', #19491, #12850, #55749 ) ;
#31392 = DIRECTION ( 'NONE',  ( 0.000000000000000000, 0.000000000000000000, 1.000000000000000000 ) ) ;
#31393 =( NAMED_UNIT ( * ) PLANE_ANGLE_UNIT ( ) SI_UNIT ( $, .RADIAN. ) );
#31394 = CARTESIAN_POINT ( 'NONE',  ( -171.5023337025455703, 86.83681590836894770, 30.98698263294540922 ) ) ;
#31395 = CARTESIAN_POINT ( 'NONE',  ( 64.69649025047539226, 13.06878919510321069, -23.68941227953380491 ) ) ;
#31396 = EDGE_CURVE ( 'NONE', #69476, #60419, #24772, .T. ) ;
#31397 = ADVANCED_FACE ( 'NONE', ( #13860 ), #61619, .F. ) ;
#31399 = CARTESIAN_POINT ( 'NONE',  ( 138.5684226926155134, 45.53585076428271350, -37.66822987502320785 ) ) ;
#31398 = VECTOR ( 'NONE', #17400, 1000.000000000000000 ) ;
#31400 = CARTESIAN_POINT ( 'NONE',  ( 38.90894112122322213, 8.345444037631240874, -35.61981746542777216 ) ) ;
#31401 = CARTESIAN_POINT ( 'NONE',  ( 150.2809931605061990, 52.27058242113232467, -45.77730096997402853 ) ) ;
#31402 = CARTESIAN_POINT ( 'NONE',  ( 24.39800339187933176, -60.26242556095669300, 170.0000000000000000 ) ) ;
#31403 = EDGE_CURVE ( 'NONE', #22804, #49146, #19137, .T. ) ;
#31404 = FACE_OUTER_BOUND ( 'NONE', #37310, .T. ) ;
#31405 = ORIENTED_EDGE ( 'NONE', *, *, #1432, .F. ) ;
#31406 = ORIENTED_EDGE ( 'NONE', *, *, #53653, .F. ) ;
#31407 = CARTESIAN_POINT ( 'NONE',  ( 174.1490454011869247, 73.24869551604541584, 87.53382120110444475 ) ) ;
#31408 = DIRECTION ( 'NONE',  ( 0.000000000000000000, 0.000000000000000000, 1.000000000000000000 ) ) ;
#31409 = CARTESIAN_POINT ( 'NONE',  ( -168.0052514572427071, 83.06849406765624622, -9.877606560333585861 ) ) ;
#31410 = CIRCLE ( 'NONE', #17905, 60.00000000000000000 ) ;
#31411 = DIRECTION ( 'NONE',  ( -0.000000000000000000, 1.000000000000000000, -0.000000000000000000 ) ) ;
#31412 = CARTESIAN_POINT ( 'NONE',  ( 282.2224082406586945, 21.53716320950900709, 4.490767689115649830 ) ) ;
#31413 = CARTESIAN_POINT ( 'NONE',  ( 230.9999999999999432, -57.00000000000007816, -2.000000000000000000 ) ) ;
#31414 = CARTESIAN_POINT ( 'NONE',  ( 29.86848256228521237, 58.14280299503737837, 41.38025477438755928 ) ) ;
#31415 = CARTESIAN_POINT ( 'NONE',  ( 2.349104707051926800E-15, -7.124194613927633313, -3.660532965668826133 ) ) ;
#31416 = CARTESIAN_POINT ( 'NONE',  ( 92.21267147730743829, 21.40196534721317079, -11.44563081337609134 ) ) ;
#31417 = DIRECTION ( 'NONE',  ( -1.000000000000000000, 0.000000000000000000, 0.000000000000000000 ) ) ;
#31418 = CARTESIAN_POINT ( 'NONE',  ( 109.6730658560643974, 21.42428528562853174, -5.000000000000004441 ) ) ;
#31419 = CARTESIAN_POINT ( 'NONE',  ( 163.1313205310724754, 63.49733392291052780, 68.67987254822025989 ) ) ;
#31420 = ORIENTED_EDGE ( 'NONE', *, *, #16966, .T. ) ;
#31421 = CARTESIAN_POINT ( 'NONE',  ( 127.4669243510812890, 38.85312661085429653, 14.12496005488912054 ) ) ;
#31422 = CARTESIAN_POINT ( 'NONE',  ( -5.066666666666664653, 8.000000000000000000, 43.13333333333333286 ) ) ;
#31423 = DIRECTION ( 'NONE',  ( -0.000000000000000000, -0.000000000000000000, -1.000000000000000000 ) ) ;
#31424 = CARTESIAN_POINT ( 'NONE',  ( -108.1180879163843400, 36.99199941971029659, -64.62439509494042511 ) ) ;
#31425 = CARTESIAN_POINT ( 'NONE',  ( -47.55235941796721022, 12.79790236059689512, -42.47865514628445993 ) ) ;
#31426 = AXIS2_PLACEMENT_3D ( 'NONE', #2754, #50589, #66097 ) ;
#31427 = CARTESIAN_POINT ( 'NONE',  ( -0.5066725584836090368, 7.531654729013470551, 89.63377582999561355 ) ) ;
#31428 = EDGE_LOOP ( 'NONE', ( #47181, #21986, #49418, #34237 ) ) ;
#31429 = DIRECTION ( 'NONE',  ( 0.000000000000000000, 0.000000000000000000, 1.000000000000000000 ) ) ;
#31430 = LINE ( 'NONE', #64123, #18107 ) ;
#31431 = ORIENTED_EDGE ( 'NONE', *, *, #56947, .T. ) ;
#31432 = ORIENTED_EDGE ( 'NONE', *, *, #7235, .F. ) ;
#31433 = EDGE_CURVE ( 'NONE', #4944, #48269, #51510, .T. ) ;
#31434 = CARTESIAN_POINT ( 'NONE',  ( 33.22375030330210421, 8.697783996218335645, 86.83782710728377197 ) ) ;
#31435 = CARTESIAN_POINT ( 'NONE',  ( -180.5231752320737826, 95.76423526868923375, -67.80882487326303476 ) ) ;
#31436 = CARTESIAN_POINT ( 'NONE',  ( 140.1190804604727589, 46.53525738079846263, -93.06488777412555180 ) ) ;
#31437 = ORIENTED_EDGE ( 'NONE', *, *, #6584, .T. ) ;
#31438 = AXIS2_PLACEMENT_3D ( 'NONE', #61723, #60687, #55765 ) ;
#31439 = CARTESIAN_POINT ( 'NONE',  ( 69.68177367721139603, 20.52767805628179332, 43.58025477438756923 ) ) ;
#31440 = FACE_OUTER_BOUND ( 'NONE', #58349, .T. ) ;
#31441 = CARTESIAN_POINT ( 'NONE',  ( 34.45817031441433187, 7.817703378455679086, -21.93692879055299016 ) ) ;
#31442 = DIRECTION ( 'NONE',  ( -0.8118923937861950435, -0.5838071093367415143, 0.000000000000000000 ) ) ;
#31443 = VECTOR ( 'NONE', #7119, 1000.000000000000000 ) ;
#31444 = LINE ( 'NONE', #32130, #8062 ) ;
#31445 = LINE ( 'NONE', #21565, #35428 ) ;
#31446 = ADVANCED_FACE ( 'NONE', ( #55377 ), #52187, .F. ) ;
#31447 = ORIENTED_EDGE ( 'NONE', *, *, #45675, .F. ) ;
#31448 = CARTESIAN_POINT ( 'NONE',  ( 108.3942953861066485, 29.14039925067523740, -23.86156525699782094 ) ) ;
#31449 = DIRECTION ( 'NONE',  ( -0.000000000000000000, -0.000000000000000000, 1.000000000000000000 ) ) ;
#31450 = EDGE_CURVE ( 'NONE', #671, #69476, #61574, .T. ) ;
#31451 = CARTESIAN_POINT ( 'NONE',  ( 9.045716588192249219, 7.384596431530733973, 40.83588045389161891 ) ) ;
#31452 = CARTESIAN_POINT ( 'NONE',  ( 197.2199569260504006, 98.22436319491367840, 37.37150111065846403 ) ) ;
#31453 = ADVANCED_FACE ( 'NONE', ( #5966 ), #48515, .T. ) ;
#31454 = CARTESIAN_POINT ( 'NONE',  ( -85.59501769175496122, 26.17305447445046696, 88.66329033029090567 ) ) ;
#31456 = ORIENTED_EDGE ( 'NONE', *, *, #41613, .T. ) ;
#31455 = PLANE ( 'NONE',  #69146 ) ;
#31457 = ORIENTED_EDGE ( 'NONE', *, *, #26351, .F. ) ;
#31458 = AXIS2_PLACEMENT_3D ( 'NONE', #65119, #53842, #27826 ) ;
#31459 = ORIENTED_EDGE ( 'NONE', *, *, #65093, .F. ) ;
#31460 = CARTESIAN_POINT ( 'NONE',  ( 115.7612476187724013, 32.64200929566224119, -65.16402729089644197 ) ) ;
#31461 = CYLINDRICAL_SURFACE ( 'NONE', #12071, 7.500000000000013323 ) ;
#31462 = CARTESIAN_POINT ( 'NONE',  ( 0.000000000000000000, 0.000000000000000000, 0.000000000000000000 ) ) ;
#31463 = DIRECTION ( 'NONE',  ( 0.000000000000000000, 0.000000000000000000, 1.000000000000000000 ) ) ;
#31464 = FACE_OUTER_BOUND ( 'NONE', #13113, .T. ) ;
#31465 = CARTESIAN_POINT ( 'NONE',  ( 151.7819978880463907, 53.35998893001568177, -75.36307041061454015 ) ) ;
#31466 = CYLINDRICAL_SURFACE ( 'NONE', #23007, 19.99999999999999289 ) ;
#31467 = CARTESIAN_POINT ( 'NONE',  ( -154.2585856850055848, 68.31650218414630160, -48.12096048054596764 ) ) ;
#31468 = ORIENTED_EDGE ( 'NONE', *, *, #18972, .T. ) ;
#31469 =( REPRESENTATION_RELATIONSHIP ('NONE','NONE', #40274, #45199 ) REPRESENTATION_RELATIONSHIP_WITH_TRANSFORMATION ( #52607 )SHAPE_REPRESENTATION_RELATIONSHIP( ) );
#31470 = ORIENTED_EDGE ( 'NONE', *, *, #62911, .T. ) ;
#31471 = LINE ( 'NONE', #492, #30953 ) ;
#31472 = CARTESIAN_POINT ( 'NONE',  ( -79.14094329813315198, 23.58034730000058588, -50.11545063171793402 ) ) ;
#31473 = CARTESIAN_POINT ( 'NONE',  ( 164.0298848570286907, 62.93631132702880393, 67.42917240860492711 ) ) ;
#31474 = CIRCLE ( 'NONE', #53891, 5.000000000000004441 ) ;
#31475 = CARTESIAN_POINT ( 'NONE',  ( -156.9919426121902575, 72.16759471857101005, 11.93913789850172336 ) ) ;
#31476 = DIRECTION ( 'NONE',  ( 0.000000000000000000, 0.000000000000000000, -1.000000000000000000 ) ) ;
#31477 = CARTESIAN_POINT ( 'NONE',  ( 16.77391662606471456, 6.533867394142991003, 44.96609377977839728 ) ) ;
#31478 = EDGE_CURVE ( 'NONE', #30275, #61402, #9633, .T. ) ;
#31479 = CARTESIAN_POINT ( 'NONE',  ( 437.3372781065085633, 400.0000000000000568, -141.4497041420118251 ) ) ;
#31480 = ORIENTED_EDGE ( 'NONE', *, *, #67117, .T. ) ;
#31481 = ORIENTED_EDGE ( 'NONE', *, *, #68150, .F. ) ;
#31482 = VERTEX_POINT ( 'NONE', #59432 ) ;
#31483 = CARTESIAN_POINT ( 'NONE',  ( 109.9975424824652634, 295.6904194069557548, 539.5330678552892323 ) ) ;
#31484 = CARTESIAN_POINT ( 'NONE',  ( 34.82939798935584719, 8.870855050008909615, -37.15461301836749186 ) ) ;
#31485 = B_SPLINE_CURVE_WITH_KNOTS ( 'NONE', 3,
 ( #1489, #7116, #7481, #55294, #17675, #23309 ),
 .UNSPECIFIED., .F., .F.,
 ( 4, 2, 4 ),
 ( 2.380731629582122378E-07, 0.002336973833157553367, 0.004673709593152147908 ),
 .UNSPECIFIED. ) ;
#31486 = CARTESIAN_POINT ( 'NONE',  ( 105.2579562709429268, -21.94247096656776819, -1.618386763725522037 ) ) ;
#31487 = CARTESIAN_POINT ( 'NONE',  ( -38.16652041892308489, 11.81761816422914535, -73.01350053778892857 ) ) ;
#31488 = CARTESIAN_POINT ( 'NONE',  ( 197.3756653044964082, 98.41886189307119537, 61.92014655920272759 ) ) ;
#31489 = AXIS2_PLACEMENT_3D ( 'NONE', #45105, #34221, #18039 ) ;
#31490 = ORIENTED_EDGE ( 'NONE', *, *, #23846, .F. ) ;
#31491 = CARTESIAN_POINT ( 'NONE',  ( 0.000000000000000000, 0.000000000000000000, 2.000000000000000000 ) ) ;
#31492 = CARTESIAN_POINT ( 'NONE',  ( 46.48120921213031664, 9.436135543404052584, 88.60415001228606968 ) ) ;
#31493 = SHAPE_REPRESENTATION_RELATIONSHIP ( 'NONE' , 'NONE' ,  #22184, #38232 ) ;
#31494 = CARTESIAN_POINT ( 'NONE',  ( 16.77104078056616387, 7.540619757007626767, 18.12152667333544898 ) ) ;
#31495 = CARTESIAN_POINT ( 'NONE',  ( 181.0840389613909736, 78.60582251573003987, 56.15314469597509373 ) ) ;
#31496 = FACE_OUTER_BOUND ( 'NONE', #26078, .T. ) ;
#31497 = CARTESIAN_POINT ( 'NONE',  ( -84.22570405563702423, 24.51726571826274537, -37.55730470497496754 ) ) ;
#31498 = CARTESIAN_POINT ( 'NONE',  ( 128.0568017572569488, 38.03085713813911184, -21.46075403565069450 ) ) ;
#31499 = DIRECTION ( 'NONE',  ( -1.000000000000000000, -0.000000000000000000, -0.000000000000000000 ) ) ;
#31500 = CARTESIAN_POINT ( 'NONE',  ( 10.31616749326173910, 7.393414706728907326, 5.535394398224304346 ) ) ;
#31501 = VERTEX_POINT ( 'NONE', #59087 ) ;
#31502 = CARTESIAN_POINT ( 'NONE',  ( 185.5572090022886016, 83.24697331286186852, 16.00218672843412548 ) ) ;
#31503 = SHAPE_DEFINITION_REPRESENTATION ( #64137, #50551 ) ;
#31504 = VECTOR ( 'NONE', #18078, 1000.000000000000000 ) ;
#31505 = CARTESIAN_POINT ( 'NONE',  ( 176.4367926094705297, 74.03315361639847936, 30.91700671302049841 ) ) ;
#31506 = DIRECTION ( 'NONE',  ( -0.7071067811865405783, -7.105427357601001070E-15, 0.7071067811865545671 ) ) ;
#31507 = CARTESIAN_POINT ( 'NONE',  ( -106.7004823116342607, 36.22460663120047997, -36.43660411563737966 ) ) ;
#31508 = DIRECTION ( 'NONE',  ( -0.000000000000000000, 1.000000000000000000, -0.000000000000000000 ) ) ;
#31509 = EDGE_LOOP ( 'NONE', ( #34744, #24988, #33253, #36670 ) ) ;
#31510 = EDGE_CURVE ( 'NONE', #26272, #13054, #27080, .T. ) ;
#31511 = VERTEX_POINT ( 'NONE', #62401 ) ;
#31512 = ADVANCED_FACE ( 'NONE', ( #41633 ), #42903, .F. ) ;
#31513 = LINE ( 'NONE', #48344, #32489 ) ;
#31514 = EDGE_CURVE ( 'NONE', #47483, #32488, #6532, .T. ) ;
#31515 = CARTESIAN_POINT ( 'NONE',  ( 173.8519557319370392, 71.59321990351749321, 88.50132255048274033 ) ) ;
#31516 = ORIENTED_EDGE ( 'NONE', *, *, #12627, .T. ) ;
#31517 = EDGE_CURVE ( 'NONE', #46033, #37671, #10903, .T. ) ;
#31518 = CARTESIAN_POINT ( 'NONE',  ( 114.6890011751076202, 30.99337387307414815, 70.01517709306831705 ) ) ;
#31519 = B_SPLINE_CURVE_WITH_KNOTS ( 'NONE', 3,
 ( #43381, #64851, #49344, #38820, #32836, #16651, #44431, #50062, #45825, #56373, #65917, #33891, #56037, #50753, #60268, #12086, #29300, #7516, #61654, #22987, #60616, #18060, #29643, #33553, #7853, #55328, #51108, #1892, #2573, #6797, #2917, #44789, #23346, #66270, #34931, #24030, #28248, #24381, #67302, #13136, #1524, #7152, #49694 ),
 .UNSPECIFIED., .F., .F.,
 ( 4, 2, 2, 2, 2, 2, 2, 2, 2, 2, 2, 2, 1, 2, 2, 2, 2, 2, 2, 2, 2, 4 ),
 ( 0.02390068823634510300, 0.02538837671117074798, 0.02613222094858357047, 0.02687606518599639296, 0.02836375366082206223, 0.02985144213564773150, 0.03059528637306055399, 0.03133913061047337995, 0.03282681908529903186, 0.03431450756012468378, 0.03580219603495033570, 0.03654604027236316166, 0.03728988450977598068, 0.03803372874718881358, 0.03877757298460163260, 0.04026526145942728452, 0.04175294993425293644, 0.04324063840907858836, 0.04398448264649141431, 0.04472832688390424027, 0.04621601535872986444, 0.04770370383355549554 ),
 .UNSPECIFIED. ) ;
#31520 = EDGE_LOOP ( 'NONE', ( #55569, #47425, #42525, #59911 ) ) ;
#31521 = CARTESIAN_POINT ( 'NONE',  ( 63.74253542338309586, -39.54050679744447194, 170.0000000000000000 ) ) ;
#31522 = FACE_OUTER_BOUND ( 'NONE', #18913, .T. ) ;
#31523 = DIRECTION ( 'NONE',  ( 0.000000000000000000, 1.000000000000000000, 0.000000000000000000 ) ) ;
#31524 = VECTOR ( 'NONE', #7883, 1000.000000000000000 ) ;
#31525 = CARTESIAN_POINT ( 'NONE',  ( 163.8800397297740972, 62.81151592172381726, -93.41319794146498623 ) ) ;
#31526 = CARTESIAN_POINT ( 'NONE',  ( 93.63037639125410294, 21.92981100938040484, -40.61996566342161685 ) ) ;
#31528 = VERTEX_POINT ( 'NONE', #36013 ) ;
#31527 = LINE ( 'NONE', #53988, #58907 ) ;
#31529 = CARTESIAN_POINT ( 'NONE',  ( 6.375108774214766072E-14, 36.11269837220805812, 85.00100000000000477 ) ) ;
#31530 = ORIENTED_EDGE ( 'NONE', *, *, #52485, .T. ) ;
#31531 = VERTEX_POINT ( 'NONE', #5623 ) ;
#31532 = CARTESIAN_POINT ( 'NONE',  ( -118.4622862908118606, 41.79153065058244465, -14.52264416072287112 ) ) ;
#31533 = LINE ( 'NONE', #20975, #39232 ) ;
#31534 = ADVANCED_FACE ( 'NONE', ( #57467, #8940, #25473, #3653, #53800, #30387 ), #25126, .T. ) ;
#31535 = CARTESIAN_POINT ( 'NONE',  ( -180.3158531669105855, 95.51092859788508349, -17.50723337383704958 ) ) ;
#31536 = ADVANCED_FACE ( 'NONE', ( #30740 ), #46910, .F. ) ;
#31538 = ORIENTED_EDGE ( 'NONE', *, *, #56638, .F. ) ;
#31537 = CARTESIAN_POINT ( 'NONE',  ( -145.3109762780891288, 60.69959559383372749, -36.07957426329402750 ) ) ;
#31539 = CARTESIAN_POINT ( 'NONE',  ( -109.1625286449147296, 37.56522729164488084, 94.70638889232425583 ) ) ;
#31540 = VERTEX_POINT ( 'NONE', #21803 ) ;
#31541 = CARTESIAN_POINT ( 'NONE',  ( -59.56523643198717366, 15.93788386494078502, -9.876116202400169186 ) ) ;
#31542 = CARTESIAN_POINT ( 'NONE',  ( -132.8150886319751578, 52.45790550853838141, -72.15884298396014174 ) ) ;
#31543 = CARTESIAN_POINT ( 'NONE',  ( 56.67004931728209982, 11.28989923258780159, 94.99999999999866418 ) ) ;
#31544 = LINE ( 'NONE', #69506, #60595 ) ;
#31545 = CARTESIAN_POINT ( 'NONE',  ( 0.000000000000000000, 0.000000000000000000, 41.38025477438755928 ) ) ;
#31546 = ORIENTED_EDGE ( 'NONE', *, *, #61214, .F. ) ;
#31547 = EDGE_LOOP ( 'NONE', ( #9297, #3223, #25867, #55481 ) ) ;
#31548 = AXIS2_PLACEMENT_3D ( 'NONE', #8586, #36344, #20163 ) ;
#31549 = CARTESIAN_POINT ( 'NONE',  ( 188.4389256074243804, 86.37278721358583766, -69.07214298238083927 ) ) ;
#31550 = CARTESIAN_POINT ( 'NONE',  ( -165.6210506643949429, 79.15024150453837137, -41.91068780496413382 ) ) ;
#31551 = FACE_OUTER_BOUND ( 'NONE', #25323, .T. ) ;
#31552 = PLANE ( 'NONE',  #37808 ) ;
#31553 = CARTESIAN_POINT ( 'NONE',  ( -71.23176719684944658, 20.69188312694500809, 38.93799383707774098 ) ) ;
#31554 = CARTESIAN_POINT ( 'NONE',  ( 79.19132716134491545, 17.01584750883627351, 36.21715455800038086 ) ) ;
#31555 = CARTESIAN_POINT ( 'NONE',  ( 63.01563776193090405, 13.70579113808098271, -35.72069083216973695 ) ) ;
#31556 = CARTESIAN_POINT ( 'NONE',  ( -118.5151419614604720, 43.00218563933589877, 39.48948330295599618 ) ) ;
#31557 = FACE_OUTER_BOUND ( 'NONE', #65439, .T. ) ;
#31558 = PRODUCT_DEFINITION_SHAPE ( 'NONE', 'NONE',  #46114 ) ;
#31559 = ORIENTED_EDGE ( 'NONE', *, *, #46604, .T. ) ;
#31560 = CARTESIAN_POINT ( 'NONE',  ( 70.21761529798065737, -26.35311180609978976, 0.000000000000000000 ) ) ;
#31561 = VERTEX_POINT ( 'NONE', #708 ) ;
#31562 = VECTOR ( 'NONE', #37924, 1000.000000000000000 ) ;
#31563 = CARTESIAN_POINT ( 'NONE',  ( -15.32550079334878923, 7.496023944924841587, -43.15998724655409546 ) ) ;
#31564 = CARTESIAN_POINT ( 'NONE',  ( 45.74764628539832501, -59.37057832282265935, 41.38025477438755928 ) ) ;
#31565 = CARTESIAN_POINT ( 'NONE',  ( 94.06416612695404922, 23.16920323269610194, 65.07509206730203744 ) ) ;
#31566 = CARTESIAN_POINT ( 'NONE',  ( 152.3102623290680242, 53.74757787434987932, -11.33146698698797472 ) ) ;
#31567 = CARTESIAN_POINT ( 'NONE',  ( 32.38493285958205803, 8.611594965040678673, 7.909991613938172961 ) ) ;
#31568 = DIRECTION ( 'NONE',  ( 0.000000000000000000, -1.000000000000000000, 0.000000000000000000 ) ) ;
#31569 = CARTESIAN_POINT ( 'NONE',  ( 34.84173759613682364, 7.859847277726514925, -63.98992801080245840 ) ) ;
#31570 = CARTESIAN_POINT ( 'NONE',  ( -96.76336539645315327, 31.18045094643428428, -74.46404432994987133 ) ) ;
#31571 = CIRCLE ( 'NONE', #20321, 10.00000000000000178 ) ;
#31572 = CARTESIAN_POINT ( 'NONE',  ( -34.74563762132953570, 11.17960945723135424, -9.236443799584387548 ) ) ;
#31573 = ORIENTED_EDGE ( 'NONE', *, *, #59840, .F. ) ;
#31574 = CARTESIAN_POINT ( 'NONE',  ( -7.825402957745081878, 7.899365992529270741, 56.96013162991089018 ) ) ;
#31575 = VERTEX_POINT ( 'NONE', #14892 ) ;
#31576 = CARTESIAN_POINT ( 'NONE',  ( -89.99999999999998579, 1.102182119232617596E-14, 10.00000000000000000 ) ) ;
#31577 = CARTESIAN_POINT ( 'NONE',  ( -190.3074740493606782, 108.5764897054613272, 7.695633288411995565 ) ) ;
#31578 = LINE ( 'NONE', #63251, #40087 ) ;
#31579 = CARTESIAN_POINT ( 'NONE',  ( -5.885876544836659896, 6.772369038004113939, 30.36654913812938261 ) ) ;
#31580 = DIRECTION ( 'NONE',  ( -0.000000000000000000, -0.000000000000000000, -1.000000000000000000 ) ) ;
#31581 = CARTESIAN_POINT ( 'NONE',  ( 152.8373718734505076, 55.38925997611394081, -37.70618783639333316 ) ) ;
#31582 = EDGE_LOOP ( 'NONE', ( #29934, #24087, #62521, #48621 ) ) ;
#31583 = DIRECTION ( 'NONE',  ( -0.0003772202979824377123, 0.9999999288524207275, 4.069661274641589443E-15 ) ) ;
#31584 = CARTESIAN_POINT ( 'NONE',  ( 8.000000000000001776, 0.000000000000000000, -9.500000000000000000 ) ) ;
#31585 = CARTESIAN_POINT ( 'NONE',  ( 177.7964363391245115, 76.75162026635256041, -23.63659886028308676 ) ) ;
#31586 = CARTESIAN_POINT ( 'NONE',  ( -104.1225399044495674, 34.86084180570099278, 57.58965421403807028 ) ) ;
#31587 = EDGE_CURVE ( 'NONE', #35180, #10168, #36357, .T. ) ;
#31588 = ITEM_DEFINED_TRANSFORMATION ( 'NONE', 'NONE', #15286,  #66832 ) ;
#31589 = CARTESIAN_POINT ( 'NONE',  ( 0.01688885742776758889, 7.321065037175426227, 3.319543390096036717 ) ) ;
#31590 = ORIENTED_EDGE ( 'NONE', *, *, #48882, .F. ) ;
#31591 = DIRECTION ( 'NONE',  ( 0.000000000000000000, -1.000000000000000000, 0.000000000000000000 ) ) ;
#31592 = CARTESIAN_POINT ( 'NONE',  ( -2.174378755909792460, 6.588636630831475216, -11.11814556240371132 ) ) ;
#31593 = CARTESIAN_POINT ( 'NONE',  ( 199.2049631873262854, 100.7347227143600321, -11.86830923348487055 ) ) ;
#31594 = EDGE_CURVE ( 'NONE', #28243, #43052, #57107, .T. ) ;
#31595 = CARTESIAN_POINT ( 'NONE',  ( -142.1931036653837737, 58.21544485181838269, 90.21602549727161602 ) ) ;
#31596 = EDGE_CURVE ( 'NONE', #14304, #3292, #7703, .T. ) ;
#31597 = CARTESIAN_POINT ( 'NONE',  ( 141.2811136745703493, 46.09188267874203859, 35.91509209166238747 ) ) ;
#31598 = ORIENTED_EDGE ( 'NONE', *, *, #37765, .F. ) ;
#31599 = DIRECTION ( 'NONE',  ( 1.000000000000000000, 0.000000000000000000, -0.000000000000000000 ) ) ;
#31600 = CARTESIAN_POINT ( 'NONE',  ( 84.05289558242220949, 19.61733656419351846, 3.319883102769282335 ) ) ;
#31601 = CARTESIAN_POINT ( 'NONE',  ( 164.9706294237033717, 65.04392654036657007, 9.790795167083055972 ) ) ;
#31602 = EDGE_CURVE ( 'NONE', #50613, #23880, #54142, .T. ) ;
#31603 = CARTESIAN_POINT ( 'NONE',  ( 34.41143668122512622, -66.58502636910473882, 41.38025477438755928 ) ) ;
#31604 = CIRCLE ( 'NONE', #59643, 24.99999999999985434 ) ;
#31605 = CIRCLE ( 'NONE', #51792, 65.00000000000000000 ) ;
#31606 = ORIENTED_EDGE ( 'NONE', *, *, #9484, .F. ) ;
#31607 = DIRECTION ( 'NONE',  ( -1.000000000000000000, 0.000000000000000000, 0.000000000000000000 ) ) ;
#31608 = VECTOR ( 'NONE', #27109, 1000.000000000000000 ) ;
#31609 = AXIS2_PLACEMENT_3D ( 'NONE', #56400, #35990, #46186 ) ;
#31610 = ORIENTED_EDGE ( 'NONE', *, *, #29638, .F. ) ;
#31611 = CARTESIAN_POINT ( 'NONE',  ( -104.5827168854524416, 33.96561401163047123, -49.66786823832703135 ) ) ;
#31612 = CARTESIAN_POINT ( 'NONE',  ( -452.6627218934860934, 395.0000000000064801, -133.9497041420121377 ) ) ;
#31613 = EDGE_CURVE ( 'NONE', #48432, #18701, #1760, .T. ) ;
#31614 = FACE_OUTER_BOUND ( 'NONE', #50388, .T. ) ;
#31616 = EDGE_LOOP ( 'NONE', ( #36249, #20541, #8557, #28696 ) ) ;
#31615 = CARTESIAN_POINT ( 'NONE',  ( 0.000000000000000000, 0.000000000000000000, 41.38025477438755928 ) ) ;
#31617 = CARTESIAN_POINT ( 'NONE',  ( -175.9970298498767534, 90.38640259140139221, 31.38186942925006662 ) ) ;
#31618 =( GEOMETRIC_REPRESENTATION_CONTEXT ( 3 ) GLOBAL_UNCERTAINTY_ASSIGNED_CONTEXT ( ( #47224 ) ) GLOBAL_UNIT_ASSIGNED_CONTEXT ( ( #27565, #43733, #22644 ) ) REPRESENTATION_CONTEXT ( 'NONE', 'WORKASPACE' ) );
#31619 = CARTESIAN_POINT ( 'NONE',  ( 10.55634918610400419, -10.55634918610406281, 85.00100000000000477 ) ) ;
#31620 = CARTESIAN_POINT ( 'NONE',  ( 113.8724110608469005, 31.71510301790680941, -50.00321340998061714 ) ) ;
#31621 = ORIENTED_EDGE ( 'NONE', *, *, #41778, .T. ) ;
#31622 = CYLINDRICAL_SURFACE ( 'NONE', #26582, 4.999999999999990230 ) ;
#31623 = DIRECTION ( 'NONE',  ( 4.314083075427411048E-32, 1.000000000000000000, 6.123233995736763571E-17 ) ) ;
#31624 = CYLINDRICAL_SURFACE ( 'NONE', #16780, 7.500000000000013323 ) ;
#31625 = CARTESIAN_POINT ( 'NONE',  ( -31.93184248720558926, 9.672312402099827011, -62.16174795566553257 ) ) ;
#31626 = CARTESIAN_POINT ( 'NONE',  ( 188.0081045302010807, 85.89855126821615272, -19.77675329002309468 ) ) ;
#31627 = VERTEX_POINT ( 'NONE', #59776 ) ;
#31628 = CARTESIAN_POINT ( 'NONE',  ( 26.99999999999999645, -27.00000000000000355, 12.00000000000000000 ) ) ;
#31629 = ORIENTED_EDGE ( 'NONE', *, *, #69550, .F. ) ;
#31630 = B_SPLINE_CURVE_WITH_KNOTS ( 'NONE', 3,
 ( #52280, #14990, #56518, #51599 ),
 .UNSPECIFIED., .F., .F.,
 ( 4, 4 ),
 ( 9.900409499157970321E-07, 0.05658314289920115397 ),
 .UNSPECIFIED. ) ;
#31631 = DIRECTION ( 'NONE',  ( 0.000000000000000000, -0.000000000000000000, 1.000000000000000000 ) ) ;
#31632 = CARTESIAN_POINT ( 'NONE',  ( -59.75659776108101084, 15.99281909568473026, 85.62955986424741184 ) ) ;
#31633 = CARTESIAN_POINT ( 'NONE',  ( -50.88541732109811022, 55.03078243218087806, 41.38025477438755928 ) ) ;
#31634 = CARTESIAN_POINT ( 'NONE',  ( 21.98745393275193294, 71.71550996510526943, 170.0000000000000000 ) ) ;
#31635 = CARTESIAN_POINT ( 'NONE',  ( 67.07698108884261501, 13.65136238353903408, 84.68817323788672979 ) ) ;
#31636 = DIRECTION ( 'NONE',  ( 0.7227948638273878901, 0.6910626489868685329, -0.000000000000000000 ) ) ;
#31637 = DIRECTION ( 'NONE',  ( -0.000000000000000000, -0.000000000000000000, -1.000000000000000000 ) ) ;
#31638 = CARTESIAN_POINT ( 'NONE',  ( 63.69186821587179281, -39.51023455020688857, 41.38025477438755928 ) ) ;
#31640 = ORIENTED_EDGE ( 'NONE', *, *, #34000, .F. ) ;
#31639 = SHAPE_REPRESENTATION ( 'top cover', ( #66832 ), #29803 ) ;
#31641 = CARTESIAN_POINT ( 'NONE',  ( 429.8372781065087906, 388.0000000000109708, 101.0502958579843806 ) ) ;
#31642 = VERTEX_POINT ( 'NONE', #23563 ) ;
#31643 = DIRECTION ( 'NONE',  ( -0.000000000000000000, -0.000000000000000000, -1.000000000000000000 ) ) ;
#31644 = CARTESIAN_POINT ( 'NONE',  ( 57.39674746172462250, 11.43903079040059012, -65.07340723825461737 ) ) ;
#31645 =( NAMED_UNIT ( * ) PLANE_ANGLE_UNIT ( ) SI_UNIT ( $, .RADIAN. ) );
#31646 = CARTESIAN_POINT ( 'NONE',  ( -121.5928001448268958, 44.91559452735375402, 71.12660519080166921 ) ) ;
#31647 = CARTESIAN_POINT ( 'NONE',  ( 23.23965501943000334, 7.861749956303023978, 36.53097551103099505 ) ) ;
#31648 = VECTOR ( 'NONE', #15511, 1000.000000000000114 ) ;
#31649 = CARTESIAN_POINT ( 'NONE',  ( 164.8433205901838789, 64.93586312665799198, -69.06606882681678883 ) ) ;
#31650 = VERTEX_POINT ( 'NONE', #28125 ) ;
#31651 = AXIS2_PLACEMENT_3D ( 'NONE', #10224, #47501, #68961 ) ;
#31652 = EDGE_CURVE ( 'NONE', #2785, #68173, #26765, .T. ) ;
#31653 = CARTESIAN_POINT ( 'NONE',  ( -72.78737098446266884, 20.16853011470089285, 60.07899134986872269 ) ) ;
#31654 = CARTESIAN_POINT ( 'NONE',  ( 198.8923184520479026, 98.70864400575095488, -92.76185446744425178 ) ) ;
#31655 = EDGE_LOOP ( 'NONE', ( #24007, #55696, #56742 ) ) ;
#31656 = EDGE_LOOP ( 'NONE', ( #38987, #15750 ) ) ;
#31657 = CARTESIAN_POINT ( 'NONE',  ( -8.000000000000000000, -3.098204225878178342, -0.3157906771918749800 ) ) ;
#31658 = DIRECTION ( 'NONE',  ( 1.000000000000000000, 0.000000000000000000, 0.000000000000000000 ) ) ;
#31659 = B_SPLINE_CURVE_WITH_KNOTS ( 'NONE', 3,
 ( #63855, #15664, #4755, #43761, #58554, #26562, #20937, #47999, #32875, #10717, #10371, #5784, #31837, #31497, #54307, #65232, #32191, #53273, #38497, #26218, #42393, #47657, #69462, #53623, #26902, #21281, #48328, #42730, #37447, #64186, #58901, #21620, #27241, #43066, #16347, #517, #21967, #60304, #33237, #54668, #65955, #44109, #6496, #56076, #38864, #55016, #23721 ),
 .UNSPECIFIED., .F., .F.,
 ( 4, 2, 2, 2, 2, 2, 2, 2, 2, 2, 2, 2, 1, 2, 2, 2, 2, 2, 2, 2, 2, 2, 2, 4 ),
 ( 0.000000000000000000, 0.001520400357568958694, 0.002280600536353455388, 0.003040800715137951648, 0.004561201072706938531, 0.005321401251491414408, 0.006081601430275891153, 0.007602001787844816887, 0.008362201966629284958, 0.009122402145413752161, 0.01064280250298270565, 0.01140300268176718326, 0.01216320286055166087, 0.01292340303933613849, 0.01368360321812061610, 0.01520400357568958000, 0.01596420375447405934, 0.01672440393325854216, 0.01824480429082751820, 0.01976520464839649424, 0.02052540482718098400, 0.02128560500596547028, 0.02280600536353445673, 0.02432640572110343624 ),
 .UNSPECIFIED. ) ;
#31661 = PLANE ( 'NONE',  #18837 ) ;
#31660 = VECTOR ( 'NONE', #2660, 1000.000000000000000 ) ;
#31662 = AXIS2_PLACEMENT_3D ( 'NONE', #12723, #61937, #23631 ) ;
#31663 = DIRECTION ( 'NONE',  ( -1.000000000000000000, 0.000000000000000000, 0.000000000000000000 ) ) ;
#31664 = DIRECTION ( 'NONE',  ( 0.000000000000000000, 0.000000000000000000, 1.000000000000000000 ) ) ;
#31665 = AXIS2_PLACEMENT_3D ( 'NONE', #52037, #57669, #41832 ) ;
#31666 = CLOSED_SHELL ( 'NONE', ( #68159, #36537, #31135, #24009, #6040, #64627 ) ) ;
#31667 = ORIENTED_EDGE ( 'NONE', *, *, #62333, .F. ) ;
#31668 = CARTESIAN_POINT ( 'NONE',  ( -132.8257891167039304, 52.46553896898736014, 40.99495158203683332 ) ) ;
#31669 = ORIENTED_EDGE ( 'NONE', *, *, #52351, .F. ) ;
#31670 = CARTESIAN_POINT ( 'NONE',  ( 38.43102714813441878, 9.298961820315048143, -23.72831626942832628 ) ) ;
#31671 = CARTESIAN_POINT ( 'NONE',  ( -148.6471085600700235, 64.76880961642446266, 30.75770659792187800 ) ) ;
#31672 = CARTESIAN_POINT ( 'NONE',  ( 205.1049299651096760, 106.9023875785546664, 44.20772073876946706 ) ) ;
#31673 = CARTESIAN_POINT ( 'NONE',  ( 69.68177367721197868, -20.52767805628085895, 43.58025477438756923 ) ) ;
#31674 =( NAMED_UNIT ( * ) PLANE_ANGLE_UNIT ( ) SI_UNIT ( $, .RADIAN. ) );
#31675 = EDGE_CURVE ( 'NONE', #57182, #25430, #33769, .T. ) ;
#31676 = DIRECTION ( 'NONE',  ( 0.000000000000000000, 0.000000000000000000, 1.000000000000000000 ) ) ;
#31677 = EDGE_LOOP ( 'NONE', ( #6624, #46055, #25319, #50375, #9451 ) ) ;
#31678 = ORIENTED_EDGE ( 'NONE', *, *, #12801, .F. ) ;
#31679 = CARTESIAN_POINT ( 'NONE',  ( -60.41792053122248518, -24.01035990323518021, 41.38025477438755928 ) ) ;
#31680 = CARTESIAN_POINT ( 'NONE',  ( 10.55634918610396511, -46.66904755831214402, 85.00100000000000477 ) ) ;
#31681 = CARTESIAN_POINT ( 'NONE',  ( -170.2801941679960578, 84.02053682015871061, -22.32142513227474367 ) ) ;
#31682 = CARTESIAN_POINT ( 'NONE',  ( 9.249622075198342230, 0.000000000000000000, 3.800590936420744193 ) ) ;
#31683 = EDGE_CURVE ( 'NONE', #59496, #29751, #36679, .T. ) ;
#31684 = CARTESIAN_POINT ( 'NONE',  ( -27.00000000000000355, -27.00000000000000355, 0.000000000000000000 ) ) ;
#31685 = CARTESIAN_POINT ( 'NONE',  ( 8.639536176317964333, 7.383242619405921303, 93.49568538271768148 ) ) ;
#31686 = EDGE_LOOP ( 'NONE', ( #66007, #48105, #66395, #25610 ) ) ;
#31687 = CARTESIAN_POINT ( 'NONE',  ( -45.00000000000002132, 20.00000000000000355, 4.000000000000000000 ) ) ;
#31688 = CARTESIAN_POINT ( 'NONE',  ( -94.89192151156326815, 29.18342430963126688, 63.54748444646997285 ) ) ;
#31689 = ORIENTED_EDGE ( 'NONE', *, *, #52318, .F. ) ;
#31690 = CARTESIAN_POINT ( 'NONE',  ( -81.90020664963799391, 23.57971581008656514, 4.302302874625238083 ) ) ;
#31691 = ORIENTED_EDGE ( 'NONE', *, *, #35993, .F. ) ;
#31692 = EDGE_CURVE ( 'NONE', #54421, #61065, #39387, .T. ) ;
#31693 = VECTOR ( 'NONE', #57652, 1000.000000000000000 ) ;
#31694 = ORIENTED_EDGE ( 'NONE', *, *, #40789, .F. ) ;
#31695 = CARTESIAN_POINT ( 'NONE',  ( -119.5404913382140109, 43.63271406506959238, 7.281364596653088661 ) ) ;
#31696 = EDGE_CURVE ( 'NONE', #43800, #28328, #13016, .T. ) ;
#31698 = EDGE_CURVE ( 'NONE', #14003, #64820, #50376, .T. ) ;
#31697 = CARTESIAN_POINT ( 'NONE',  ( -177.1540936177022445, 91.73126115633625943, 58.82771625204114940 ) ) ;
#31699 = CARTESIAN_POINT ( 'NONE',  ( 126.6576865394846152, 37.24426596493988484, 65.97471202277128555 ) ) ;
#31700 = AXIS2_PLACEMENT_3D ( 'NONE', #53055, #20367, #25322 ) ;
#31701 = VERTEX_POINT ( 'NONE', #27783 ) ;
#31702 = VECTOR ( 'NONE', #6283, 1000.000000000000000 ) ;
#31703 = CARTESIAN_POINT ( 'NONE',  ( -34.85922420997363957, 10.17769528929257561, 84.72309154256973329 ) ) ;
#31704 = CARTESIAN_POINT ( 'NONE',  ( 149.9552318559266837, 52.03645904563048674, 36.93262037564134914 ) ) ;
#31705 = DIRECTION ( 'NONE',  ( -1.000000000000000000, 0.000000000000000000, 0.000000000000000000 ) ) ;
#31706 = CARTESIAN_POINT ( 'NONE',  ( 103.4696172145934838, 25.87254488218943749, -40.19200279096821760 ) ) ;
#31707 = CARTESIAN_POINT ( 'NONE',  ( 138.1901928158493149, 45.29454828899441310, -64.22858801807878137 ) ) ;
#31708 = LINE ( 'NONE', #26440, #50086 ) ;
#31709 = ORIENTED_EDGE ( 'NONE', *, *, #67817, .T. ) ;
#31710 = VECTOR ( 'NONE', #38258, 1000.000000000000000 ) ;
#31711 = LINE ( 'NONE', #10249, #32041 ) ;
#31712 = CARTESIAN_POINT ( 'NONE',  ( -1.310872448937997703, 8.480771745766402248, -9.182649155111340278 ) ) ;
#31713 = CARTESIAN_POINT ( 'NONE',  ( 179.4074606910091347, 78.34362448405026669, 17.32480475505861506 ) ) ;
#31714 = DIRECTION ( 'NONE',  ( -0.000000000000000000, -0.000000000000000000, -1.000000000000000000 ) ) ;
#31715 = DIRECTION ( 'NONE',  ( 0.000000000000000000, 0.000000000000000000, 1.000000000000000000 ) ) ;
#31716 = CARTESIAN_POINT ( 'NONE',  ( -74.58602291351368763, 7.967916035251061402, 170.0000000000000000 ) ) ;
#31717 = CARTESIAN_POINT ( 'NONE',  ( -156.0300823189602397, 69.91528270335481920, 7.635611034400681341 ) ) ;
#31718 = CARTESIAN_POINT ( 'NONE',  ( -121.5928001448268816, 44.91559452735373981, -63.09614776151676097 ) ) ;
#31719 = CARTESIAN_POINT ( 'NONE',  ( 68.63487067129261732, 14.04635751989138726, 15.45973179360630922 ) ) ;
#31720 = CARTESIAN_POINT ( 'NONE',  ( -85.90077524418997257, 26.30132018890135370, 66.75733766280808368 ) ) ;
#31721 = CARTESIAN_POINT ( 'NONE',  ( -108.6634958860518338, 36.14357436892402831, 41.96444054384087252 ) ) ;
#31722 = ORIENTED_EDGE ( 'NONE', *, *, #64162, .F. ) ;
#31723 = ITEM_DEFINED_TRANSFORMATION ( 'NONE', 'NONE', #2889,  #66832 ) ;
#31724 = FACE_OUTER_BOUND ( 'NONE', #16934, .T. ) ;
#31725 = ORIENTED_EDGE ( 'NONE', *, *, #15095, .F. ) ;
#31726 = CARTESIAN_POINT ( 'NONE',  ( 200.0000000000000000, 3.000000000000030198, 0.000000000000000000 ) ) ;
#31727 = EDGE_LOOP ( 'NONE', ( #37492, #20556, #24407, #9537 ) ) ;
#31728 = CARTESIAN_POINT ( 'NONE',  ( 22.72762739171800206, 7.830015800126070680, -66.98700550285960276 ) ) ;
#31729 =( NAMED_UNIT ( * ) SI_UNIT ( $, .STERADIAN. ) SOLID_ANGLE_UNIT ( ) );
#31730 = CARTESIAN_POINT ( 'NONE',  ( -148.6426892915312123, 64.76241938621076599, 72.56537183036277838 ) ) ;
#31731 = CARTESIAN_POINT ( 'NONE',  ( 70.51601918574517924, 14.53832276813547608, -16.13771727979073489 ) ) ;
#31732 = CARTESIAN_POINT ( 'NONE',  ( 46.66904755831212981, 15.55634918610394379, 2.000000000000001776 ) ) ;
#31733 = CARTESIAN_POINT ( 'NONE',  ( -49.13048465129992337, 14.20828170588045936, -64.93260343570349846 ) ) ;
#31734 = EDGE_CURVE ( 'NONE', #22434, #21697, #66145, .T. ) ;
#31735 = PLANE ( 'NONE',  #61088 ) ;
#31736 = DIRECTION ( 'NONE',  ( 4.974206872490772509E-18, 1.135330258912677140E-18, -1.000000000000000000 ) ) ;
#31737 = EDGE_LOOP ( 'NONE', ( #22224, #37337, #34597, #46172 ) ) ;
#31738 = EDGE_LOOP ( 'NONE', ( #50263, #53525, #22739, #41982 ) ) ;
#31739 = EDGE_CURVE ( 'NONE', #66403, #62711, #33512, .T. ) ;
#31740 = CARTESIAN_POINT ( 'NONE',  ( -34.75846525699014933, 54.92585086258208804, 40.00000000000003553 ) ) ;
#31741 = LINE ( 'NONE', #1736, #37399 ) ;
#31742 = CARTESIAN_POINT ( 'NONE',  ( 127.3613131747807472, 38.79352689838291468, -93.43917518758931351 ) ) ;
#31743 = PRODUCT_DEFINITION_CONTEXT ( 'detailed design', #50279, 'design' ) ;
#31744 = AXIS2_PLACEMENT_3D ( 'NONE', #22376, #6553, #31897 ) ;
#31745 = CARTESIAN_POINT ( 'NONE',  ( 69.01423235029108127, 15.18386996031285996, -92.38905430490223125 ) ) ;
#31746 = DIRECTION ( 'NONE',  ( 0.000000000000000000, 1.000000000000000000, -0.000000000000000000 ) ) ;
#31747 = CARTESIAN_POINT ( 'NONE',  ( 185.5412249395995730, 84.70425786165998261, -22.91669308973334651 ) ) ;
#31748 = DIRECTION ( 'NONE',  ( -0.000000000000000000, 0.000000000000000000, -1.000000000000000000 ) ) ;
#31749 = VECTOR ( 'NONE', #61143, 1000.000000000000000 ) ;
#31750 = SHAPE_REPRESENTATION_RELATIONSHIP ( 'NONE' , 'NONE' ,  #45625, #53289 ) ;
#31751 = CARTESIAN_POINT ( 'NONE',  ( -174.7800083645696532, 88.99302808536934606, -49.53816181598559609 ) ) ;
#31752 = CARTESIAN_POINT ( 'NONE',  ( 88.99522780200243233, 20.24180937454203644, -9.355914456664107703 ) ) ;
#31753 = CARTESIAN_POINT ( 'NONE',  ( 412.3372781065086201, 400.0000000000000568, -146.4497041420118251 ) ) ;
#31754 = FACE_OUTER_BOUND ( 'NONE', #2145, .T. ) ;
#31755 = EDGE_CURVE ( 'NONE', #22892, #21953, #49222, .T. ) ;
#31756 = LINE ( 'NONE', #32452, #58010 ) ;
#31757 = CIRCLE ( 'NONE', #45265, 65.36598343705435354 ) ;
#31758 = ADVANCED_FACE ( 'NONE', ( #39048 ), #1056, .F. ) ;
#31759 = AXIS2_PLACEMENT_3D ( 'NONE', #14874, #46189, #30721 ) ;
#31760 = EDGE_CURVE ( 'NONE', #9029, #63051, #55994, .T. ) ;
#31761 = ORIENTED_EDGE ( 'NONE', *, *, #19628, .T. ) ;
#31762 = CARTESIAN_POINT ( 'NONE',  ( -123.4416615615272832, 44.90042688650405012, -35.32212343775866970 ) ) ;
#31763 = CARTESIAN_POINT ( 'NONE',  ( 280.0000000000000000, -22.00000000000000000, -4.999999999999990230 ) ) ;
#31764 = VECTOR ( 'NONE', #65285, 1000.000000000000000 ) ;
#31765 = CARTESIAN_POINT ( 'NONE',  ( 154.0281735872262630, 56.28213428456460576, 70.42142694816533322 ) ) ;
#31766 = CARTESIAN_POINT ( 'NONE',  ( -7.825402957745087207, -170.0000000000000000, 64.46013162991090439 ) ) ;
#31767 = EDGE_CURVE ( 'NONE', #16525, #67731, #39134, .T. ) ;
#31768 = CARTESIAN_POINT ( 'NONE',  ( 151.3309484205704791, 53.03078371058071383, 14.38017068174847246 ) ) ;
#31769 = CARTESIAN_POINT ( 'NONE',  ( -12.11199156453544923, 8.217753791142426323, 85.14174289210440350 ) ) ;
#31770 = ORIENTED_EDGE ( 'NONE', *, *, #27568, .F. ) ;
#31771 = CARTESIAN_POINT ( 'NONE',  ( 0.7145311798163216377, 4.618802153517004960, 7.999999999999998224 ) ) ;
#31772 = CARTESIAN_POINT ( 'NONE',  ( 0.3173508448886549482, 8.480771745766404024, 1.310872448937998813 ) ) ;
#31773 = ORIENTED_EDGE ( 'NONE', *, *, #55506, .F. ) ;
#31774 = ORIENTED_EDGE ( 'NONE', *, *, #62688, .F. ) ;
#31775 = LINE ( 'NONE', #53208, #29702 ) ;
#31776 = DIRECTION ( 'NONE',  ( 0.000000000000000000, 0.000000000000000000, 1.000000000000000000 ) ) ;
#31777 = CARTESIAN_POINT ( 'NONE',  ( 136.9816124143867455, 44.53086385938545533, -90.39170542592599134 ) ) ;
#31778 = ORIENTED_EDGE ( 'NONE', *, *, #67836, .F. ) ;
#31779 = CYLINDRICAL_SURFACE ( 'NONE', #59189, 5.000000000000004441 ) ;
#31780 = CARTESIAN_POINT ( 'NONE',  ( 0.000000000000000000, 0.000000000000000000, 40.00000000000003553 ) ) ;
#31781 = CARTESIAN_POINT ( 'NONE',  ( -0.3255842968951676020, 7.525381170773408179, 11.26331030618680096 ) ) ;
#31782 = EDGE_CURVE ( 'NONE', #33970, #43782, #29877, .T. ) ;
#31784 = EDGE_CURVE ( 'NONE', #11268, #22437, #13327, .T. ) ;
#31783 = CARTESIAN_POINT ( 'NONE',  ( 173.6007744016332879, 72.73482010729019009, -43.14319336715800546 ) ) ;
#31785 = CARTESIAN_POINT ( 'NONE',  ( -149.7268278745401631, 65.68859631971241697, -76.65738112195569443 ) ) ;
#31786 = CARTESIAN_POINT ( 'NONE',  ( -439.4229916354183842, 400.0000000000065370, -123.9497041420119530 ) ) ;
#31787 = EDGE_CURVE ( 'NONE', #14720, #67398, #51677, .T. ) ;
#31788 = ORIENTED_EDGE ( 'NONE', *, *, #64793, .T. ) ;
#31789 = CARTESIAN_POINT ( 'NONE',  ( 0.7145311798163198613, -4.618802153516998743, 7.999999999999998224 ) ) ;
#31790 = AXIS2_PLACEMENT_3D ( 'NONE', #33405, #28105, #49199 ) ;
#31791 = CARTESIAN_POINT ( 'NONE',  ( -17.50000000000002842, -18.06806526123148160, 378.0000000000000000 ) ) ;
#31792 = CARTESIAN_POINT ( 'NONE',  ( 15.29912143387263512, 7.491799981865496783, 30.01470767270521733 ) ) ;
#31793 = CARTESIAN_POINT ( 'NONE',  ( 198.8752826725511511, 100.3130050945023726, 31.97338715271266096 ) ) ;
#31794 = CARTESIAN_POINT ( 'NONE',  ( 79.13491102535617472, 16.99860516843601133, 90.45089180137320284 ) ) ;
#31796 = ORIENTED_EDGE ( 'NONE', *, *, #55046, .F. ) ;
#31795 = DIRECTION ( 'NONE',  ( 0.000000000000000000, 0.000000000000000000, -1.000000000000000000 ) ) ;
#31797 = VERTEX_POINT ( 'NONE', #35147 ) ;
#31798 = CONICAL_SURFACE ( 'NONE', #49758, 65.00000000000000000, 0.7853981633974497223 ) ;
#31799 = VERTEX_POINT ( 'NONE', #61539 ) ;
#31800 = AXIS2_PLACEMENT_3D ( 'NONE', #49091, #929, #18154 ) ;
#31801 = FILL_AREA_STYLE_COLOUR ( '', #34632 ) ;
#31802 = DIRECTION ( 'NONE',  ( -0.000000000000000000, -0.000000000000000000, 1.000000000000000000 ) ) ;
#31803 = CARTESIAN_POINT ( 'NONE',  ( -31.43908319763709969, 10.61114334766715928, 57.06100499665286208 ) ) ;
#31804 = CARTESIAN_POINT ( 'NONE',  ( -317.6627218934913230, 394.9999999999997158, -11.44970414201176823 ) ) ;
#31805 = VECTOR ( 'NONE', #28742, 1000.000000000000000 ) ;
#31806 = CARTESIAN_POINT ( 'NONE',  ( -417.6627218934913230, 179.4906275429376308, -144.4497041420118819 ) ) ;
#31807 = CARTESIAN_POINT ( 'NONE',  ( 154.4550750032601911, 55.34393534448157226, -63.59772041800123787 ) ) ;
#31808 = CARTESIAN_POINT ( 'NONE',  ( -17.50000000000002842, 207.5000000000000284, 380.0000000000000000 ) ) ;
#31809 = AXIS2_PLACEMENT_3D ( 'NONE', #59429, #30995, #5618 ) ;
#31810 = CYLINDRICAL_SURFACE ( 'NONE', #9326, 7.500000000000013323 ) ;
#31811 = VERTEX_POINT ( 'NONE', #35848 ) ;
#31812 = VERTEX_POINT ( 'NONE', #25305 ) ;
#31813 = CARTESIAN_POINT ( 'NONE',  ( 70.26936813788617542, 15.51386666370915535, -18.34636768599548517 ) ) ;
#31814 = CARTESIAN_POINT ( 'NONE',  ( -83.51110947562234799, 25.31252704029287059, -48.34590627098496896 ) ) ;
#31815 = AXIS2_PLACEMENT_3D ( 'NONE', #69447, #69093, #21603 ) ;
#31816 = CARTESIAN_POINT ( 'NONE',  ( 161.7209903610254571, 61.03262545641846515, 69.95060923550748555 ) ) ;
#31817 = CARTESIAN_POINT ( 'NONE',  ( 111.1829448509513298, 30.43012797723691776, -9.122365715518217399 ) ) ;
#31818 = B_SPLINE_CURVE_WITH_KNOTS ( 'NONE', 3,
 ( #57025, #56671, #29582, #30635 ),
 .UNSPECIFIED., .F., .F.,
 ( 4, 4 ),
 ( 0.1259919275528358640, 0.1829744153748747992 ),
 .UNSPECIFIED. ) ;
#31819 = CARTESIAN_POINT ( 'NONE',  ( 185.5572090022886300, 83.24697331286185431, -37.68691445249324801 ) ) ;
#31820 = CARTESIAN_POINT ( 'NONE',  ( 21.42484406671928454, 6.746536496442161912, 32.56092050209711886 ) ) ;
#31821 = CARTESIAN_POINT ( 'NONE',  ( -156.4791144138197296, 71.69273398181533707, 94.69527957875486379 ) ) ;
#31822 = ORIENTED_EDGE ( 'NONE', *, *, #35435, .F. ) ;
#31823 = VERTEX_POINT ( 'NONE', #62925 ) ;
#31824 = ORIENTED_EDGE ( 'NONE', *, *, #39110, .T. ) ;
#31825 = EDGE_CURVE ( 'NONE', #27278, #42385, #57302, .T. ) ;
#31826 = CARTESIAN_POINT ( 'NONE',  ( -155.2836587093738956, 70.59655508952972980, -20.25880271682157385 ) ) ;
#31827 = CARTESIAN_POINT ( 'NONE',  ( 32.29578462738145817, 8.602609172809794202, -40.70879380640250389 ) ) ;
#31828 = CARTESIAN_POINT ( 'NONE',  ( 176.6214367443247681, 74.20967084876663478, 69.69980881498953806 ) ) ;
#31829 = FACE_OUTER_BOUND ( 'NONE', #1343, .T. ) ;
#31830 = CARTESIAN_POINT ( 'NONE',  ( 447.3372781065086201, 400.0000000000044338, 113.5502958579838122 ) ) ;
#31831 = ORIENTED_EDGE ( 'NONE', *, *, #55743, .T. ) ;
#31832 = CARTESIAN_POINT ( 'NONE',  ( 37.46254810722765427, 8.164772623042711786, 56.99704862271182293 ) ) ;
#31833 = CARTESIAN_POINT ( 'NONE',  ( 8.480442907658517271, 6.376693431076494889, -14.46955541742294038 ) ) ;
#31834 = CARTESIAN_POINT ( 'NONE',  ( 9.962235950564874543, 64.23203137738424573, 40.00000000000003553 ) ) ;
#31835 = CARTESIAN_POINT ( 'NONE',  ( 183.9986899696430669, 81.60141257362812439, 56.72931473510586642 ) ) ;
#31836 = FACE_BOUND ( 'NONE', #27428, .T. ) ;
#31837 = CARTESIAN_POINT ( 'NONE',  ( -83.69653436244855982, 24.30167057287990673, -37.04694618773496018 ) ) ;
#31838 = FACE_OUTER_BOUND ( 'NONE', #68113, .T. ) ;
#31839 = ADVANCED_FACE ( 'NONE', ( #30228 ), #24610, .T. ) ;
#31840 = CARTESIAN_POINT ( 'NONE',  ( 26.11269837220800127, -26.11269837220812562, 85.00100000000000477 ) ) ;
#31841 = CARTESIAN_POINT ( 'NONE',  ( 0.000000000000000000, 0.000000000000000000, -8.949444346342716017 ) ) ;
#31842 = CIRCLE ( 'NONE', #49808, 10.00000000000000000 ) ;
#31843 = EDGE_CURVE ( 'NONE', #31540, #53628, #8069, .T. ) ;
#31844 = ADVANCED_FACE ( 'NONE', ( #18626 ), #40083, .F. ) ;
#31845 = ORIENTED_EDGE ( 'NONE', *, *, #62681, .F. ) ;
#31847 = FACE_OUTER_BOUND ( 'NONE', #1585, .T. ) ;
#31846 = VECTOR ( 'NONE', #44969, 1000.000000000000000 ) ;
#31848 = CARTESIAN_POINT ( 'NONE',  ( 174.1251613516844543, 71.84747073139212148, 39.65969668319120700 ) ) ;
#31849 = DIRECTION ( 'NONE',  ( 0.000000000000000000, 0.000000000000000000, 1.000000000000000000 ) ) ;
#31850 = CARTESIAN_POINT ( 'NONE',  ( -105.8683518445188270, 35.77995342500074827, -49.11769980258868884 ) ) ;
#31851 = EDGE_CURVE ( 'NONE', #15622, #38606, #18973, .T. ) ;
#31852 = CARTESIAN_POINT ( 'NONE',  ( 58.47885130911550533, 12.69429933094348506, -76.05780093763492289 ) ) ;
#31853 = ORIENTED_EDGE ( 'NONE', *, *, #68145, .T. ) ;
#31854 = AXIS2_PLACEMENT_3D ( 'NONE', #44971, #60459, #50597 ) ;
#31855 = ORIENTED_EDGE ( 'NONE', *, *, #17068, .T. ) ;
#31856 = CIRCLE ( 'NONE', #19455, 4.999999999999996447 ) ;
#31857 = CARTESIAN_POINT ( 'NONE',  ( -29.02794087136070544, 9.207646203414356023, -8.854141498921386244 ) ) ;
#31858 = AXIS2_PLACEMENT_3D ( 'NONE', #50379, #24348, #14124 ) ;
#31859 = CARTESIAN_POINT ( 'NONE',  ( 201.9721407532275350, 104.3507814346148308, 16.86238661557147367 ) ) ;
#31860 = ORIENTED_EDGE ( 'NONE', *, *, #46788, .T. ) ;
#31861 = VECTOR ( 'NONE', #6686, 1000.000000000000114 ) ;
#31862 = CARTESIAN_POINT ( 'NONE',  ( -2.000000000000000000, 192.0000000000000000, 378.0000000000000000 ) ) ;
#31863 = ORIENTED_EDGE ( 'NONE', *, *, #45566, .T. ) ;
#31864 = CARTESIAN_POINT ( 'NONE',  ( 0.000000000000000000, 70.00000000000000000, 0.000000000000000000 ) ) ;
#31865 = DIRECTION ( 'NONE',  ( -1.000000000000000000, 0.000000000000000000, 2.220446049250313081E-16 ) ) ;
#31866 = DIRECTION ( 'NONE',  ( -1.000000000000000000, 0.000000000000000000, 0.000000000000000000 ) ) ;
#31867 = AXIS2_PLACEMENT_3D ( 'NONE', #64529, #27234, #508 ) ;
#31868 = EDGE_CURVE ( 'NONE', #16148, #34252, #13695, .T. ) ;
#31869 = CARTESIAN_POINT ( 'NONE',  ( -95.61819996182569525, 29.52346081122273347, 41.47345898016966004 ) ) ;
#31870 = CARTESIAN_POINT ( 'NONE',  ( 87.58098510096633049, 19.74745174099416900, -50.77640564174353699 ) ) ;
#31872 = ORIENTED_EDGE ( 'NONE', *, *, #31594, .F. ) ;
#31871 = CARTESIAN_POINT ( 'NONE',  ( -7.825402957745087207, -170.0000000000000000, -69.76262132240751157 ) ) ;
#31873 = EDGE_CURVE ( 'NONE', #10603, #18346, #20720, .T. ) ;
#31874 = ORIENTED_EDGE ( 'NONE', *, *, #30480, .T. ) ;
#31875 = VERTEX_POINT ( 'NONE', #47415 ) ;
#31876 = CARTESIAN_POINT ( 'NONE',  ( -120.1259246007803512, 42.81147313035990010, -10.74822668097895928 ) ) ;
#31877 = FACE_BOUND ( 'NONE', #67643, .T. ) ;
#31878 = APPLICATION_CONTEXT ( 'automotive_design' ) ;
#31879 = CARTESIAN_POINT ( 'NONE',  ( -179.5082312244189211, 94.53075638132058600, -19.30745591354370205 ) ) ;
#31880 = CARTESIAN_POINT ( 'NONE',  ( -167.4860113959265391, 82.52233889531187572, -64.10065570822085590 ) ) ;
#31882 = EDGE_LOOP ( 'NONE', ( #30794, #34826, #14598, #35412 ) ) ;
#31881 = CARTESIAN_POINT ( 'NONE',  ( -143.2471548081023514, 59.04577938365764567, -46.47464696708835419 ) ) ;
#31883 = CARTESIAN_POINT ( 'NONE',  ( 26.11269837220809364, 15.55634918610396866, 2.000000000000001776 ) ) ;
#31884 = ORIENTED_EDGE ( 'NONE', *, *, #20976, .F. ) ;
#31885 = CARTESIAN_POINT ( 'NONE',  ( -133.3765738414514601, 51.62252165471731757, 38.69660473656405486 ) ) ;
#31886 = CARTESIAN_POINT ( 'NONE',  ( -56.72814287166055891, 15.13700122306437557, -8.557341907245762158 ) ) ;
#31887 = CARTESIAN_POINT ( 'NONE',  ( 82.14449817946437804, 17.93919511903896691, -10.46065494932177842 ) ) ;
#31888 = CARTESIAN_POINT ( 'NONE',  ( -23.70047331481904607, -76.98764151615553430, 73.58025477438756923 ) ) ;
#31890 = DIRECTION ( 'NONE',  ( -0.000000000000000000, 1.000000000000000000, -0.000000000000000000 ) ) ;
#31889 = AXIS2_PLACEMENT_3D ( 'NONE', #58065, #25380, #62303 ) ;
#31891 = CARTESIAN_POINT ( 'NONE',  ( 0.000000000000000000, 6.000000000000000000, 0.000000000000000000 ) ) ;
#31892 = CARTESIAN_POINT ( 'NONE',  ( -10.00000000000000000, 0.000000000000000000, 2.000000000000001776 ) ) ;
#31893 = ORIENTED_EDGE ( 'NONE', *, *, #15818, .F. ) ;
#31894 = ORIENTED_EDGE ( 'NONE', *, *, #36201, .F. ) ;
#31895 = AXIS2_PLACEMENT_3D ( 'NONE', #2000, #40647, #62103 ) ;
#31896 = CARTESIAN_POINT ( 'NONE',  ( 188.0081045302011944, 85.89855126821616693, -73.46585447095047527 ) ) ;
#31897 = DIRECTION ( 'NONE',  ( 0.000000000000000000, 0.000000000000000000, 1.000000000000000000 ) ) ;
#31898 = CARTESIAN_POINT ( 'NONE',  ( -20.55634918610405748, -10.55634918610400597, 0.000000000000000000 ) ) ;
#31899 = LINE ( 'NONE', #53331, #17170 ) ;
#31900 = AXIS2_PLACEMENT_3D ( 'NONE', #24753, #46188, #57106 ) ;
#31901 = CARTESIAN_POINT ( 'NONE',  ( 106.6322547488295385, 28.34756922280615399, -76.85819378913427613 ) ) ;
#31902 = CARTESIAN_POINT ( 'NONE',  ( -15.55634918610408945, -31.11269837220804035, 0.000000000000000000 ) ) ;
#31903 = CARTESIAN_POINT ( 'NONE',  ( 79.93126905972556528, 17.24332478304276961, 33.82846076375348332 ) ) ;
#31904 = CARTESIAN_POINT ( 'NONE',  ( 66.30230369578302430, 14.49551544185123930, -49.96661566441417079 ) ) ;
#31905 = VECTOR ( 'NONE', #27739, 1000.000000000000114 ) ;
#31906 = CARTESIAN_POINT ( 'NONE',  ( 46.23304607317101755, 10.41544405387738692, -46.22577417019589063 ) ) ;
#31907 = CARTESIAN_POINT ( 'NONE',  ( 210.5178985598939221, 114.6803933586780886, 68.28892203333299449 ) ) ;
#31909 = EDGE_LOOP ( 'NONE', ( #3748, #69400, #15306, #39862 ) ) ;
#31908 = ADVANCED_FACE ( 'NONE', ( #11169 ), #31949, .F. ) ;
#31911 = FACE_OUTER_BOUND ( 'NONE', #44101, .T. ) ;
#31910 = VECTOR ( 'NONE', #22261, 1000.000000000000000 ) ;
#31912 = VERTEX_POINT ( 'NONE', #15425 ) ;
#31913 = CARTESIAN_POINT ( 'NONE',  ( -14.55390976651257162, 7.422979442794212623, -46.24041557031399918 ) ) ;
#31914 = ADVANCED_FACE ( 'NONE', ( #47081 ), #5210, .T. ) ;
#31915 = CIRCLE ( 'NONE', #40900, 0.3000000000000051514 ) ;
#31916 = CARTESIAN_POINT ( 'NONE',  ( 79.22872707466393649, 18.07970189365809688, 65.29920498983847210 ) ) ;
#31917 = CARTESIAN_POINT ( 'NONE',  ( 91.11019107624154856, 22.06959540317787116, 70.07588725628826865 ) ) ;
#31918 = CARTESIAN_POINT ( 'NONE',  ( 151.6351261592328683, 53.25263237790400694, -12.06117684806004675 ) ) ;
#31919 = LINE ( 'NONE', #4491, #43320 ) ;
#31920 = CARTESIAN_POINT ( 'NONE',  ( 37.00112095025831138, 8.109340230899350743, -62.85478614795575680 ) ) ;
#31921 = DIRECTION ( 'NONE',  ( -0.000000000000000000, -0.000000000000000000, -1.000000000000000000 ) ) ;
#31922 = VECTOR ( 'NONE', #31411, 1000.000000000000000 ) ;
#31923 = DIRECTION ( 'NONE',  ( 0.04486483035051862939, -0.9989930665413143673, 0.000000000000000000 ) ) ;
#31924 = ORIENTED_EDGE ( 'NONE', *, *, #24972, .F. ) ;
#31925 = LINE ( 'NONE', #48078, #28651 ) ;
#31926 = VERTEX_POINT ( 'NONE', #48103 ) ;
#31927 = DIRECTION ( 'NONE',  ( -0.000000000000000000, 1.000000000000000000, -0.000000000000000000 ) ) ;
#31928 = CARTESIAN_POINT ( 'NONE',  ( 10.31616749326172844, 7.393414706728908214, -74.99825737316675145 ) ) ;
#31929 = CARTESIAN_POINT ( 'NONE',  ( -28.35330809568272770, 9.105138953156437509, 17.71201881402830836 ) ) ;
#31930 = DIRECTION ( 'NONE',  ( 0.000000000000000000, -1.000000000000000000, 0.000000000000000000 ) ) ;
#31931 = EDGE_CURVE ( 'NONE', #69411, #38117, #42824, .T. ) ;
#31932 = CARTESIAN_POINT ( 'NONE',  ( 280.6598192889778716, -21.43204465433285932, 4.967071677942358932 ) ) ;
#31933 = DIRECTION ( 'NONE',  ( 0.000000000000000000, 0.000000000000000000, -1.000000000000000000 ) ) ;
#31934 = CARTESIAN_POINT ( 'NONE',  ( 79.26839340764567510, 18.09188476209940433, 89.42367620941877249 ) ) ;
#31935 = EDGE_CURVE ( 'NONE', #61115, #53628, #47006, .T. ) ;
#31936 = EDGE_CURVE ( 'NONE', #35650, #64382, #21381, .T. ) ;
#31937 = EDGE_LOOP ( 'NONE', ( #28943, #59280, #18762, #21178 ) ) ;
#31938 = DIRECTION ( 'NONE',  ( -9.389072067404547989E-15, 3.421211351543888735E-15, -1.000000000000000000 ) ) ;
#31939 = CARTESIAN_POINT ( 'NONE',  ( -153.6994314938755508, 69.16570456337670691, 71.30114417014331707 ) ) ;
#31940 = CARTESIAN_POINT ( 'NONE',  ( 174.2468109002381880, 73.34092405459587383, -13.78573923642201393 ) ) ;
#31941 = CARTESIAN_POINT ( 'NONE',  ( -104.5740066103013106, 35.09687312794778080, 57.71916911584846588 ) ) ;
#31942 = CARTESIAN_POINT ( 'NONE',  ( -132.2161740628506266, 52.03204870034953444, -46.45640934042872061 ) ) ;
#31943 = ORIENTED_EDGE ( 'NONE', *, *, #28827, .T. ) ;
#31944 = DIRECTION ( 'NONE',  ( -0.000000000000000000, 0.000000000000000000, 1.000000000000000000 ) ) ;
#31945 = CARTESIAN_POINT ( 'NONE',  ( -0.5780275525703851836, 6.527356703336896437, -18.01939305138792591 ) ) ;
#31946 = SURFACE_STYLE_FILL_AREA ( #36882 ) ;
#31947 = CARTESIAN_POINT ( 'NONE',  ( -156.4787762129735711, 70.32547257834129084, 94.69602752494165543 ) ) ;
#31948 = VECTOR ( 'NONE', #20624, 1000.000000000000000 ) ;
#31949 = PLANE ( 'NONE',  #68355 ) ;
#31950 = EDGE_LOOP ( 'NONE', ( #63608, #31181, #1018, #43485 ) ) ;
#31951 = PLANE ( 'NONE',  #50314 ) ;
#31952 = DIRECTION ( 'NONE',  ( -1.000000000000000000, 0.000000000000000000, 0.000000000000000000 ) ) ;
#31953 = CARTESIAN_POINT ( 'NONE',  ( 164.8908506817023749, 64.97619709085122963, 11.18946311072333799 ) ) ;
#31954 = CARTESIAN_POINT ( 'NONE',  ( 311.9975424824652350, 22.00669820036272384, 401.6295345748407613 ) ) ;
#31955 = AXIS2_PLACEMENT_3D ( 'NONE', #15497, #31664, #10890 ) ;
#31956 = ORIENTED_EDGE ( 'NONE', *, *, #52779, .F. ) ;
#31957 = EDGE_CURVE ( 'NONE', #66812, #6692, #4335, .T. ) ;
#31958 = CARTESIAN_POINT ( 'NONE',  ( 173.6007744016332595, 72.73482010729017588, 64.23500899469674152 ) ) ;
#31959 = VECTOR ( 'NONE', #7712, 1000.000000000000000 ) ;
#31960 = EDGE_LOOP ( 'NONE', ( #13703, #11386 ) ) ;
#31961 = CARTESIAN_POINT ( 'NONE',  ( -103.2129897037411013, 33.25684593987700310, -35.05838499450624113 ) ) ;
#31962 = DIRECTION ( 'NONE',  ( -0.000000000000000000, -1.000000000000000000, 1.156482317317871725E-15 ) ) ;
#31963 = CIRCLE ( 'NONE', #63401, 65.00000000000000000 ) ;
#31964 = CARTESIAN_POINT ( 'NONE',  ( -61.38706483483512244, 16.47181058798475917, 41.84068912785072314 ) ) ;
#31966 = ORIENTED_EDGE ( 'NONE', *, *, #68240, .F. ) ;
#31965 = CARTESIAN_POINT ( 'NONE',  ( 8.113421703707349053, 0.000000000000000000, 5.845715376051984435 ) ) ;
#31967 = CARTESIAN_POINT ( 'NONE',  ( -179.5178913137216909, 94.54206947403388028, 42.27584261177923253 ) ) ;
#31968 = CARTESIAN_POINT ( 'NONE',  ( 10.00000000000000000, 1.224646799147353256E-15, 0.000000000000000000 ) ) ;
#31969 = DIRECTION ( 'NONE',  ( 0.000000000000000000, -1.000000000000000000, 0.000000000000000000 ) ) ;
#31970 = EDGE_LOOP ( 'NONE', ( #53423, #57744, #13084, #4945 ) ) ;
#31971 = CARTESIAN_POINT ( 'NONE',  ( 112.3013380801406100, 400.0000000000077307, 91.05029585798746439 ) ) ;
#31972 = CARTESIAN_POINT ( 'NONE',  ( 111.9975424824652634, 170.0000000000000284, 354.1673509436691347 ) ) ;
#31973 = LINE ( 'NONE', #42851, #66232 ) ;
#31974 = CARTESIAN_POINT ( 'NONE',  ( 130.7457207912710828, 40.74300766298685517, 57.01493017841226418 ) ) ;
#31975 = ORIENTED_EDGE ( 'NONE', *, *, #3843, .F. ) ;
#31976 = CARTESIAN_POINT ( 'NONE',  ( 43.96062659677685502, 10.06332325923985671, 16.54484489615712306 ) ) ;
#31977 = ORIENTED_EDGE ( 'NONE', *, *, #15817, .T. ) ;
#31978 = VERTEX_POINT ( 'NONE', #65342 ) ;
#31979 = CARTESIAN_POINT ( 'NONE',  ( 6.400000000000000355, 0.000000000000000000, 0.000000000000000000 ) ) ;
#31980 = EDGE_CURVE ( 'NONE', #1198, #40354, #65699, .T. ) ;
#31981 = CARTESIAN_POINT ( 'NONE',  ( -57.24414243706566197, 15.27981560285317109, 84.32688172081668654 ) ) ;
#31982 = DIRECTION ( 'NONE',  ( 0.000000000000000000, 0.000000000000000000, 1.000000000000000000 ) ) ;
#31983 = CARTESIAN_POINT ( 'NONE',  ( -156.8764584803562059, 70.69066846313526753, -70.58134442723202540 ) ) ;
#31984 = CARTESIAN_POINT ( 'NONE',  ( -108.1183077156918841, 35.84680167036558629, 86.98961108605696779 ) ) ;
#31985 = CARTESIAN_POINT ( 'NONE',  ( -26.00000000000000000, 0.000000000000000000, -2.818925648462311923E-15 ) ) ;
#31986 = LINE ( 'NONE', #59732, #41811 ) ;
#31987 = EDGE_CURVE ( 'NONE', #42819, #67708, #67263, .T. ) ;
#31988 = FACE_OUTER_BOUND ( 'NONE', #2431, .T. ) ;
#31989 = ORIENTED_EDGE ( 'NONE', *, *, #30109, .F. ) ;
#31990 = CIRCLE ( 'NONE', #29737, 65.36598343705435354 ) ;
#31991 = CARTESIAN_POINT ( 'NONE',  ( -101.8638894403611204, 33.69766868189126541, -88.70367844590323614 ) ) ;
#31993 = ORIENTED_EDGE ( 'NONE', *, *, #20414, .F. ) ;
#31992 = ADVANCED_FACE ( 'NONE', ( #49486 ), #27695, .T. ) ;
#31994 = CARTESIAN_POINT ( 'NONE',  ( -71.15374617000810531, 20.66492714610675918, 64.77291441092350510 ) ) ;
#31995 = CARTESIAN_POINT ( 'NONE',  ( 211.1200456646896555, 115.5868795682033721, -66.78691274028477665 ) ) ;
#31996 = CARTESIAN_POINT ( 'NONE',  ( 42.71247067544611298, 9.879726907348445053, -23.00956250308817275 ) ) ;
#31998 = CARTESIAN_POINT ( 'NONE',  ( -73.79615177260656367, 20.52570924097572203, 16.79824538533793543 ) ) ;
#31997 = AXIS2_PLACEMENT_3D ( 'NONE', #9641, #31101, #30064 ) ;
#31999 = CARTESIAN_POINT ( 'NONE',  ( -120.1650841064594033, 44.02024060322521848, 69.81157495390961287 ) ) ;
#32000 = EDGE_CURVE ( 'NONE', #22100, #35032, #64998, .T. ) ;
#32001 = CARTESIAN_POINT ( 'NONE',  ( 23.28809538736929241, 7.864824219997537114, 38.00689959157113407 ) ) ;
#32002 = CARTESIAN_POINT ( 'NONE',  ( 199.0123542265578180, 98.86010591893334265, 85.49239298808598164 ) ) ;
#32004 = FACE_OUTER_BOUND ( 'NONE', #63836, .T. ) ;
#32003 = AXIS2_PLACEMENT_3D ( 'NONE', #15460, #52055, #62952 ) ;
#32005 = AXIS2_PLACEMENT_3D ( 'NONE', #48944, #37717, #10983 ) ;
#32006 = ORIENTED_EDGE ( 'NONE', *, *, #26983, .F. ) ;
#32007 = DIRECTION ( 'NONE',  ( 0.000000000000000000, -0.000000000000000000, -1.000000000000000000 ) ) ;
#32008 = DIRECTION ( 'NONE',  ( -1.000000000000000000, -0.000000000000000000, -0.000000000000000000 ) ) ;
#32009 = ORIENTED_EDGE ( 'NONE', *, *, #58117, .T. ) ;
#32010 = ORIENTED_EDGE ( 'NONE', *, *, #16376, .F. ) ;
#32011 = AXIS2_PLACEMENT_3D ( 'NONE', #25664, #4537, #46060 ) ;
#32012 = CARTESIAN_POINT ( 'NONE',  ( -26.88635117726413881, 9.904687797303051155, -63.68164643894200339 ) ) ;
#32013 = CARTESIAN_POINT ( 'NONE',  ( 55.76066037845575352, 11.10616952318089545, -45.18587298604916924 ) ) ;
#32014 = CARTESIAN_POINT ( 'NONE',  ( -59.09450113343203270, -27.07101652673575032, 40.00000000000003553 ) ) ;
#32015 = DIRECTION ( 'NONE',  ( 0.3930250316539278255, -0.9195277725514487965, 0.000000000000000000 ) ) ;
#32016 = VECTOR ( 'NONE', #57545, 1000.000000000000000 ) ;
#32017 = CARTESIAN_POINT ( 'NONE',  ( -146.1260528621668300, 61.36307454672304118, 4.665803956922211171 ) ) ;
#32018 = EDGE_CURVE ( 'NONE', #57123, #50465, #7750, .T. ) ;
#32019 = EDGE_LOOP ( 'NONE', ( #40217, #5610, #48502, #18083 ) ) ;
#32020 = VERTEX_POINT ( 'NONE', #2031 ) ;
#32021 = CARTESIAN_POINT ( 'NONE',  ( -126.3495878770406478, 48.00153794568857535, 45.61994787315711619 ) ) ;
#32022 = ORIENTED_EDGE ( 'NONE', *, *, #10769, .T. ) ;
#32023 = CARTESIAN_POINT ( 'NONE',  ( -430.1627218934916641, 395.0000000000064801, -123.9497041420119530 ) ) ;
#32024 = CARTESIAN_POINT ( 'NONE',  ( 181.0840389613909736, 80.03940679743415387, -89.91415884680696990 ) ) ;
#32025 = CARTESIAN_POINT ( 'NONE',  ( 58.48209831743721310, 11.66636741727081805, 70.15205218717414937 ) ) ;
#32026 = DIRECTION ( 'NONE',  ( 1.000000000000000000, 0.000000000000000000, -0.000000000000000000 ) ) ;
#32027 = DIRECTION ( 'NONE',  ( 0.000000000000000000, 0.000000000000000000, 1.000000000000000000 ) ) ;
#32028 = ORIENTED_EDGE ( 'NONE', *, *, #66565, .F. ) ;
#32029 = ORIENTED_EDGE ( 'NONE', *, *, #67134, .T. ) ;
#32030 = PLANE ( 'NONE',  #53601 ) ;
#32031 = CARTESIAN_POINT ( 'NONE',  ( -31.11269837220804035, 15.55634918610408945, 0.000000000000000000 ) ) ;
#32032 = CARTESIAN_POINT ( 'NONE',  ( -172.7154982671752350, 86.67743928531946551, -22.86740657428632417 ) ) ;
#32033 = CARTESIAN_POINT ( 'NONE',  ( 7.762887554996211747E-14, 46.66904755831208718, 2.000000000000001776 ) ) ;
#32034 = CARTESIAN_POINT ( 'NONE',  ( 68.63487067129263153, 14.04635751989139258, 42.30428238407001373 ) ) ;
#32035 = CARTESIAN_POINT ( 'NONE',  ( 9.446081536138994039, 7.386671790239061508, 87.18713865022354526 ) ) ;
#32036 = ORIENTED_EDGE ( 'NONE', *, *, #40407, .T. ) ;
#32037 = CARTESIAN_POINT ( 'NONE',  ( -94.79166046756731134, 29.13671350128076654, 65.35457784805571180 ) ) ;
#32038 = ORIENTED_EDGE ( 'NONE', *, *, #9996, .T. ) ;
#32039 = CARTESIAN_POINT ( 'NONE',  ( -76.31381168750412769, 21.43908608416556660, 45.05567668390800407 ) ) ;
#32040 = ORIENTED_EDGE ( 'NONE', *, *, #51706, .F. ) ;
#32041 = VECTOR ( 'NONE', #63031, 1000.000000000000000 ) ;
#32042 = ORIENTED_EDGE ( 'NONE', *, *, #56706, .T. ) ;
#32043 = CARTESIAN_POINT ( 'NONE',  ( 9.058156535714475766, 6.378495712187264743, -46.33800716567037625 ) ) ;
#32044 = LINE ( 'NONE', #42261, #67 ) ;
#32045 = CARTESIAN_POINT ( 'NONE',  ( 128.9253503890652155, 38.52561778336669818, 58.19870550832551004 ) ) ;
#32046 = VECTOR ( 'NONE', #37457, 1000.000000000000000 ) ;
#32047 = ORIENTED_EDGE ( 'NONE', *, *, #45610, .T. ) ;
#32048 = ADVANCED_FACE ( 'NONE', ( #54413 ), #23485, .F. ) ;
#32049 =( GEOMETRIC_REPRESENTATION_CONTEXT ( 3 ) GLOBAL_UNCERTAINTY_ASSIGNED_CONTEXT ( ( #19115 ) ) GLOBAL_UNIT_ASSIGNED_CONTEXT ( ( #9698, #13930, #62468 ) ) REPRESENTATION_CONTEXT ( 'NONE', 'WORKASPACE' ) );
#32050 = AXIS2_PLACEMENT_3D ( 'NONE', #17341, #18050, #28607 ) ;
#32051 = SHAPE_REPRESENTATION ( 'angular contact ball bearing_68_iso_ISO 15 ABB - 1740 - 38,SI,NC,38_68', ( #66832 ), #621 ) ;
#32052 = CARTESIAN_POINT ( 'NONE',  ( 150.5550643769628891, 52.46819381604269239, 33.99397750223288028 ) ) ;
#32053 = AXIS2_PLACEMENT_3D ( 'NONE', #8639, #47281, #35363 ) ;
#32054 = CARTESIAN_POINT ( 'NONE',  ( 259.4165763529819060, 225.8585178651493948, 128.9999999999999716 ) ) ;
#32055 = CARTESIAN_POINT ( 'NONE',  ( 19.00668540189274225, -62.54164772954691642, 6.377659838150142862E-18 ) ) ;
#32056 = CARTESIAN_POINT ( 'NONE',  ( 0.000000000000000000, 0.000000000000000000, 0.000000000000000000 ) ) ;
#32057 = DIRECTION ( 'NONE',  ( 1.000000000000000000, 0.000000000000000000, 0.000000000000000000 ) ) ;
#32058 = CARTESIAN_POINT ( 'NONE',  ( -146.7404675333698378, 63.17262273741972223, -62.18289695349267276 ) ) ;
#32059 = ORIENTED_EDGE ( 'NONE', *, *, #46537, .T. ) ;
#32060 = FACE_BOUND ( 'NONE', #30979, .T. ) ;
#32061 = LINE ( 'NONE', #58775, #47747 ) ;
#32062 = CARTESIAN_POINT ( 'NONE',  ( -15.55634918610403439, 2.818925648462311528E-14, 85.00100000000000477 ) ) ;
#32063 = CARTESIAN_POINT ( 'NONE',  ( 113.2864006930874297, 30.31414150890303816, -90.21175991542801853 ) ) ;
#32064 = CARTESIAN_POINT ( 'NONE',  ( -120.4666325602655945, 44.20829586446608772, -47.59616471546328142 ) ) ;
#32065 = CARTESIAN_POINT ( 'NONE',  ( -85.73740570227380431, 26.23277384689414049, 8.560564749426776032 ) ) ;
#32066 = DIRECTION ( 'NONE',  ( 0.000000000000000000, 0.000000000000000000, 1.000000000000000000 ) ) ;
#32067 = CARTESIAN_POINT ( 'NONE',  ( -150.3898662070191961, 64.92828409760429054, 18.87627064943540134 ) ) ;
#32068 = CARTESIAN_POINT ( 'NONE',  ( -75.37104758724677822, 21.09346139657355579, -89.55357651485830672 ) ) ;
#32069 = ADVANCED_FACE ( 'NONE', ( #22773 ), #48783, .F. ) ;
#32070 = CARTESIAN_POINT ( 'NONE',  ( 63.01563776193091826, 12.67277567978500308, 2.968410348757589023 ) ) ;
#32071 = DIRECTION ( 'NONE',  ( -1.000000000000000000, 0.000000000000000000, 0.000000000000000000 ) ) ;
#32072 = CARTESIAN_POINT ( 'NONE',  ( 45.20420770554357404, 10.25329097499119513, -92.03875038294617639 ) ) ;
#32073 = ORIENTED_EDGE ( 'NONE', *, *, #44284, .F. ) ;
#32074 = CARTESIAN_POINT ( 'NONE',  ( -36.38071096718370967, 11.47804921491337282, 16.53490236032401839 ) ) ;
#32075 = ORIENTED_EDGE ( 'NONE', *, *, #54050, .F. ) ;
#32076 = CARTESIAN_POINT ( 'NONE',  ( -5.000000000000073719, -46.66904755831211560, 85.00100000000000477 ) ) ;
#32077 = ORIENTED_EDGE ( 'NONE', *, *, #7394, .T. ) ;
#32078 = LINE ( 'NONE', #21513, #6226 ) ;
#32079 = CARTESIAN_POINT ( 'NONE',  ( -447.6627218934918346, 367.0710678118609280, 108.5502958579925519 ) ) ;
#32080 = DIRECTION ( 'NONE',  ( 0.000000000000000000, 0.000000000000000000, -1.000000000000000000 ) ) ;
#32081 = ADVANCED_FACE ( 'NONE', ( #44215 ), #33343, .T. ) ;
#32082 = CARTESIAN_POINT ( 'NONE',  ( 46.66904755831210139, 0.000000000000000000, 0.000000000000000000 ) ) ;
#32083 = CARTESIAN_POINT ( 'NONE',  ( 137.3861614007145704, 44.78548268714477132, -36.90154586889402566 ) ) ;
#32084 = CARTESIAN_POINT ( 'NONE',  ( -48.23766733091051151, 13.99378332280059212, -66.41992323350672223 ) ) ;
#32085 = CARTESIAN_POINT ( 'NONE',  ( 450.2085304802404266, 188.0000000000000000, 7.478223336038896996 ) ) ;
#32086 = DIRECTION ( 'NONE',  ( 1.000000000000000000, 0.000000000000000000, -0.000000000000000000 ) ) ;
#32087 = ORIENTED_EDGE ( 'NONE', *, *, #36448, .F. ) ;
#32088 = ORIENTED_EDGE ( 'NONE', *, *, #33549, .T. ) ;
#32089 = CARTESIAN_POINT ( 'NONE',  ( 209.9518228411288874, 190.0000000000000000, 31.43423095485942298 ) ) ;
#32090 = VECTOR ( 'NONE', #45381, 1000.000000000000114 ) ;
#32091 = CARTESIAN_POINT ( 'NONE',  ( -452.6627218934913230, 177.8591479523843475, 78.55029585798814651 ) ) ;
#32092 = LINE ( 'NONE', #42971, #52133 ) ;
#32093 = B_SPLINE_CURVE_WITH_KNOTS ( 'NONE', 3,
 ( #66951, #45123, #45470, #24725, #19085, #66268 ),
 .UNSPECIFIED., .F., .F.,
 ( 4, 2, 4 ),
 ( 0.03218933845493725937, 0.06469832000440833841, 0.09720730155387943827 ),
 .UNSPECIFIED. ) ;
#32094 = EDGE_CURVE ( 'NONE', #67398, #47824, #12228, .T. ) ;
#32095 = VECTOR ( 'NONE', #1905, 1000.000000000000000 ) ;
#32096 = DIRECTION ( 'NONE',  ( -0.000000000000000000, -1.000000000000000000, -0.000000000000000000 ) ) ;
#32097 = ORIENTED_EDGE ( 'NONE', *, *, #56532, .F. ) ;
#32098 = DIRECTION ( 'NONE',  ( -0.8465179929926601732, -0.5323601107705934199, 0.000000000000000000 ) ) ;
#32099 = AXIS2_PLACEMENT_3D ( 'NONE', #64118, #58831, #64815 ) ;
#32100 = CARTESIAN_POINT ( 'NONE',  ( -14.76369756425704871, 7.442560416198674034, 67.33920332730103553 ) ) ;
#32101 = CARTESIAN_POINT ( 'NONE',  ( -84.22570405563701001, 24.51726571826273826, -10.71275411451128434 ) ) ;
#32102 =( NAMED_UNIT ( * ) PLANE_ANGLE_UNIT ( ) SI_UNIT ( $, .RADIAN. ) );
#32103 = DIRECTION ( 'NONE',  ( -0.000000000000000000, -1.000000000000000000, -0.000000000000000000 ) ) ;
#32104 = CARTESIAN_POINT ( 'NONE',  ( 45.04360969585142271, 9.210232288266690048, -11.30927456569269651 ) ) ;
#32105 = CARTESIAN_POINT ( 'NONE',  ( -7.825402957745087207, -170.0000000000000000, 71.96013162991091860 ) ) ;
#32106 = FACE_OUTER_BOUND ( 'NONE', #9375, .T. ) ;
#32107 = AXIS2_PLACEMENT_3D ( 'NONE', #15412, #14715, #36522 ) ;
#32108 = DIRECTION ( 'NONE',  ( -0.000000000000000000, -0.000000000000000000, 1.000000000000000000 ) ) ;
#32109 = AXIS2_PLACEMENT_3D ( 'NONE', #7143, #22981, #49338 ) ;
#32110 = AXIS2_PLACEMENT_3D ( 'NONE', #40211, #61659, #50418 ) ;
#32111 = ORIENTED_EDGE ( 'NONE', *, *, #2104, .F. ) ;
#32112 = CARTESIAN_POINT ( 'NONE',  ( 0.000000000000000000, 0.000000000000000000, -0.002000000000002000178 ) ) ;
#32113 = CYLINDRICAL_SURFACE ( 'NONE', #59699, 7.500000000000013323 ) ;
#32114 = FACE_BOUND ( 'NONE', #40147, .T. ) ;
#32115 = DIRECTION ( 'NONE',  ( 1.000000000000000000, 0.000000000000000000, 0.000000000000000000 ) ) ;
#32116 = DIRECTION ( 'NONE',  ( 1.000000000000000000, 0.000000000000000000, 0.000000000000000000 ) ) ;
#32117 = DIRECTION ( 'NONE',  ( 1.000000000000000000, 0.000000000000000000, 0.000000000000000000 ) ) ;
#32118 = ORIENTED_EDGE ( 'NONE', *, *, #64631, .T. ) ;
#32119 = LINE ( 'NONE', #9636, #3330 ) ;
#32120 = CARTESIAN_POINT ( 'NONE',  ( 21.38432669263065122, -61.76910524360950916, 41.38025477438755928 ) ) ;
#32121 = EDGE_LOOP ( 'NONE', ( #29551, #7205, #40680, #53091 ) ) ;
#32122 = VERTEX_POINT ( 'NONE', #28395 ) ;
#32123 = CARTESIAN_POINT ( 'NONE',  ( 38.10887197045263264, 9.258695140773173904, 83.70795236904210412 ) ) ;
#32124 = DIRECTION ( 'NONE',  ( 0.3930250316539148359, 0.9195277725514544587, -0.000000000000000000 ) ) ;
#32125 = CARTESIAN_POINT ( 'NONE',  ( 140.3402251947021000, 46.67919788697790295, -93.41835240302059162 ) ) ;
#32126 = ORIENTED_EDGE ( 'NONE', *, *, #37814, .T. ) ;
#32127 = PLANE ( 'NONE',  #62593 ) ;
#32128 = CARTESIAN_POINT ( 'NONE',  ( 32.28603806442400526, 7.590310383548725781, -18.69525418143827267 ) ) ;
#32129 = CARTESIAN_POINT ( 'NONE',  ( 181.0840389613909736, 80.03940679743416808, -51.22505766587963905 ) ) ;
#32130 = CARTESIAN_POINT ( 'NONE',  ( -20.00000000000002842, 3.680555555555560243, 0.000000000000000000 ) ) ;
#32131 = CARTESIAN_POINT ( 'NONE',  ( 91.49345572560145001, 21.13836538408681776, 31.49813976496750811 ) ) ;
#32132 = EDGE_CURVE ( 'NONE', #1714, #2078, #41438, .T. ) ;
#32133 = ORIENTED_EDGE ( 'NONE', *, *, #10290, .F. ) ;
#32135 = EDGE_CURVE ( 'NONE', #25958, #308, #68566, .T. ) ;
#32134 = CARTESIAN_POINT ( 'NONE',  ( -48.23766733091052572, 13.99378332280059212, -39.57537264304307456 ) ) ;
#32136 = VECTOR ( 'NONE', #21247, 1000.000000000000000 ) ;
#32137 = CARTESIAN_POINT ( 'NONE',  ( 12.99074365121454910, -21.50298515537749822, 3.061616997868437868E-16 ) ) ;
#32138 = CARTESIAN_POINT ( 'NONE',  ( 15.78827728214693416, 7.507518794609589818, 30.01470767270522089 ) ) ;
#32139 = DIRECTION ( 'NONE',  ( 0.000000000000000000, 0.000000000000000000, 1.000000000000000000 ) ) ;
#32140 = CARTESIAN_POINT ( 'NONE',  ( 123.4242852856285566, 0.000000000000000000, -20.00000000000000000 ) ) ;
#32141 = CIRCLE ( 'NONE', #10796, 242.4895526022646379 ) ;
#32143 = ORIENTED_EDGE ( 'NONE', *, *, #25273, .T. ) ;
#32142 = CARTESIAN_POINT ( 'NONE',  ( -2.700000000000004619, 0.000000000000000000, 0.000000000000000000 ) ) ;
#32144 = ORIENTED_EDGE ( 'NONE', *, *, #43753, .F. ) ;
#32145 = VECTOR ( 'NONE', #50546, 1000.000000000000000 ) ;
#32146 = VECTOR ( 'NONE', #38083, 1000.000000000000000 ) ;
#32147 = VERTEX_POINT ( 'NONE', #6599 ) ;
#32148 = DIRECTION ( 'NONE',  ( 1.000000000000000000, 0.000000000000000000, 0.000000000000000000 ) ) ;
#32149 = CARTESIAN_POINT ( 'NONE',  ( -166.1020662756963588, 81.08306215305039188, 94.67661392444711055 ) ) ;
#32150 = CARTESIAN_POINT ( 'NONE',  ( 38.07387156563210340, -34.92400885808820021, 26.66469104408689006 ) ) ;
#32151 = CARTESIAN_POINT ( 'NONE',  ( 100.0000000000000284, 2.449293598294708091E-15, -20.00000000000001421 ) ) ;
#32152 = PRODUCT_DEFINITION_FORMATION_WITH_SPECIFIED_SOURCE ( 'ANY', '', #37747, .NOT_KNOWN. ) ;
#32153 = EDGE_CURVE ( 'NONE', #16002, #26339, #43864, .T. ) ;
#32155 = CARTESIAN_POINT ( 'NONE',  ( -37.75148815634407384, 54.92203319703903475, 34.48241823996504252 ) ) ;
#32154 = AXIS2_PLACEMENT_3D ( 'NONE', #26102, #27127, #42619 ) ;
#32156 = ADVANCED_FACE ( 'NONE', ( #11869 ), #54870, .T. ) ;
#32157 = CARTESIAN_POINT ( 'NONE',  ( -13.77312480593389310, 8.361845410302541026, -20.64904994316430376 ) ) ;
#32158 = CARTESIAN_POINT ( 'NONE',  ( 151.7956716830627215, 53.36999433148316285, -65.55858710784085019 ) ) ;
#32159 = DIRECTION ( 'NONE',  ( -0.000000000000000000, 1.000000000000000000, -0.000000000000000000 ) ) ;
#32160 = EDGE_LOOP ( 'NONE', ( #16106, #59838, #33744, #49558 ) ) ;
#32161 = VECTOR ( 'NONE', #15483, 1000.000000000000000 ) ;
#32162 = CARTESIAN_POINT ( 'NONE',  ( -150.3791492925491582, 64.92185203933371440, -49.77484619116003017 ) ) ;
#32163 = ORIENTED_EDGE ( 'NONE', *, *, #49764, .F. ) ;
#32164 = VERTEX_POINT ( 'NONE', #17492 ) ;
#32165 = CARTESIAN_POINT ( 'NONE',  ( 63.98689050258325750, 13.93365232918668006, -8.923645743953048992 ) ) ;
#32166 = CARTESIAN_POINT ( 'NONE',  ( -85.36298448216592760, 26.07611629625834127, -39.20033059854998214 ) ) ;
#32167 = CARTESIAN_POINT ( 'NONE',  ( 117.6673027744877658, 32.47081449954681887, 89.68066879645499512 ) ) ;
#32168 = EDGE_CURVE ( 'NONE', #44628, #68305, #8854, .T. ) ;
#32169 = CARTESIAN_POINT ( 'NONE',  ( -156.9232798886536955, 72.10386843399172108, 10.21938759049889178 ) ) ;
#32170 = B_SPLINE_CURVE_WITH_KNOTS ( 'NONE', 3,
 ( #52644, #64591, #58954, #25927 ),
 .UNSPECIFIED., .F., .F.,
 ( 4, 4 ),
 ( 9.900409499142632672E-07, 0.05658314289920113316 ),
 .UNSPECIFIED. ) ;
#32171 = CARTESIAN_POINT ( 'NONE',  ( 184.0013086981202832, 81.60415045669144263, -36.80231263419718601 ) ) ;
#32172 = CARTESIAN_POINT ( 'NONE',  ( 20.74852474914888845, 6.709938988646749536, 43.16143151702989655 ) ) ;
#32173 = DIRECTION ( 'NONE',  ( -0.04486483035051862939, 0.9989930665413143673, 0.000000000000000000 ) ) ;
#32174 = ORIENTED_EDGE ( 'NONE', *, *, #3173, .T. ) ;
#32175 = VERTEX_POINT ( 'NONE', #55121 ) ;
#32176 = ORIENTED_EDGE ( 'NONE', *, *, #57908, .F. ) ;
#32177 = CARTESIAN_POINT ( 'NONE',  ( -8.807541152391511474, 6.956521193351526300, 18.22245856944851283 ) ) ;
#32178 = CARTESIAN_POINT ( 'NONE',  ( 33.77444274891859521, 8.756048688386682599, -48.08388456350459705 ) ) ;
#32179 = EDGE_CURVE ( 'NONE', #27145, #18627, #25725, .T. ) ;
#32180 = CARTESIAN_POINT ( 'NONE',  ( -2.116120943112233643, 74.98056102853672655, 170.0000000000000000 ) ) ;
#32181 = EDGE_CURVE ( 'NONE', #15124, #41255, #60506, .T. ) ;
#32182 = CARTESIAN_POINT ( 'NONE',  ( 230.9999999999999432, 225.0000000000000000, 0.000000000000000000 ) ) ;
#32183 = EDGE_CURVE ( 'NONE', #17738, #62756, #46629, .T. ) ;
#32184 = ORIENTED_EDGE ( 'NONE', *, *, #39300, .F. ) ;
#32185 = EDGE_CURVE ( 'NONE', #46840, #50390, #22335, .T. ) ;
#32186 = LINE ( 'NONE', #5442, #8708 ) ;
#32187 = CARTESIAN_POINT ( 'NONE',  ( -152.9119739516381458, 67.12135129037710612, 58.36714245934808787 ) ) ;
#32188 = CARTESIAN_POINT ( 'NONE',  ( 21.44191228441539465, 7.755009954762318358, 5.717230818571867879 ) ) ;
#32189 = CARTESIAN_POINT ( 'NONE',  ( 200.0000000000000000, 2.999999999999969802, 0.000000000000000000 ) ) ;
#32190 = DIRECTION ( 'NONE',  ( 0.000000000000000000, -0.000000000000000000, 1.000000000000000000 ) ) ;
#32191 = CARTESIAN_POINT ( 'NONE',  ( -85.09761763353364472, 24.87634954265998388, -38.74851144219385191 ) ) ;
#32192 = CARTESIAN_POINT ( 'NONE',  ( 22.53041628628729143, 6.810083298012985509, 67.68129265094559344 ) ) ;
#32193 = CARTESIAN_POINT ( 'NONE',  ( 15.55634918610406103, 15.55634918610400241, 0.000000000000000000 ) ) ;
#32194 = CARTESIAN_POINT ( 'NONE',  ( 13.84120792123769128, 6.445822122644895735, -77.12289573830005907 ) ) ;
#32195 = CIRCLE ( 'NONE', #16467, 246.3582898394606957 ) ;
#32196 = EDGE_LOOP ( 'NONE', ( #41412, #14368, #18494, #19792, #48066, #21738, #62188, #62840, #49779 ) ) ;
#32197 = CIRCLE ( 'NONE', #34425, 4.999999999999999112 ) ;
#32198 = CARTESIAN_POINT ( 'NONE',  ( -4.999999999999936939, 31.11269837220806167, 0.000000000000000000 ) ) ;
#32199 = SHAPE_DEFINITION_REPRESENTATION ( #17578, #34334 ) ;
#32200 = CARTESIAN_POINT ( 'NONE',  ( 174.9042454172880525, 72.57746269938725447, 41.08881398978587640 ) ) ;
#32201 = CARTESIAN_POINT ( 'NONE',  ( -129.6165111262477296, 48.99406349865699895, -48.92884824319389736 ) ) ;
#32202 = CARTESIAN_POINT ( 'NONE',  ( 43.96465529479667822, 9.046527005589323878, -75.93720877633131749 ) ) ;
#32203 = CARTESIAN_POINT ( 'NONE',  ( -27.00000000000000355, 26.99999999999999289, 15.00000000000000000 ) ) ;
#32204 = ORIENTED_EDGE ( 'NONE', *, *, #15336, .F. ) ;
#32205 = VECTOR ( 'NONE', #44837, 1000.000000000000114 ) ;
#32206 = CARTESIAN_POINT ( 'NONE',  ( -15.55634918610411077, -46.66904755831208718, 2.000000000000001776 ) ) ;
#32207 = ORIENTED_EDGE ( 'NONE', *, *, #12788, .T. ) ;
#32208 = CARTESIAN_POINT ( 'NONE',  ( -29.49620345460275317, 9.280093073089039635, -8.712006218224214393 ) ) ;
#32209 = CARTESIAN_POINT ( 'NONE',  ( 197.2199569260504006, 98.22436319491367840, 10.52695052019480570 ) ) ;
#32210 = EDGE_LOOP ( 'NONE', ( #42061, #17684, #63432, #34788 ) ) ;
#32211 = ORIENTED_EDGE ( 'NONE', *, *, #43017, .F. ) ;
#32212 = CARTESIAN_POINT ( 'NONE',  ( 150.6633721218480275, 53.78936049964467259, 93.76803445655194480 ) ) ;
#32213 = ORIENTED_EDGE ( 'NONE', *, *, #37854, .F. ) ;
#32214 = CARTESIAN_POINT ( 'NONE',  ( 127.2107679985236217, 38.70844091144995502, -66.85294649915745424 ) ) ;
#32215 = CARTESIAN_POINT ( 'NONE',  ( 0.000000000000000000, 0.000000000000000000, 40.00000000000003553 ) ) ;
#32216 = CARTESIAN_POINT ( 'NONE',  ( 136.9822423813093337, 44.53121110416874018, 57.03315645636024556 ) ) ;
#32217 = CARTESIAN_POINT ( 'NONE',  ( 110.2429982417149432, 29.99119854320847267, 2.766663615273645682 ) ) ;
#32218 = CARTESIAN_POINT ( 'NONE',  ( 163.9881357112706723, 62.90166026738586424, -93.59647863210024354 ) ) ;
#32219 = CARTESIAN_POINT ( 'NONE',  ( 94.12988949694084795, 22.11811104795076588, -43.08587400594926464 ) ) ;
#32220 = DIRECTION ( 'NONE',  ( -1.048079516971690241E-11, 0.000000000000000000, -1.000000000000000000 ) ) ;
#32221 = VERTEX_POINT ( 'NONE', #26583 ) ;
#32222 = ORIENTED_EDGE ( 'NONE', *, *, #17625, .T. ) ;
#32224 = EDGE_CURVE ( 'NONE', #7326, #10885, #64206, .T. ) ;
#32223 = CARTESIAN_POINT ( 'NONE',  ( -166.5742238910466142, 81.57147158222488770, 7.807693272540740637 ) ) ;
#32225 = DIRECTION ( 'NONE',  ( -1.000000000000000000, 0.000000000000000000, 0.000000000000000000 ) ) ;
#32226 = CARTESIAN_POINT ( 'NONE',  ( -177.1540936177023582, 91.73126115633628785, -21.70593551934987886 ) ) ;
#32227 = CARTESIAN_POINT ( 'NONE',  ( -165.7149569557575433, 80.68479365246972179, -67.83569924512404725 ) ) ;
#32229 = ORIENTED_EDGE ( 'NONE', *, *, #35498, .T. ) ;
#32228 = CARTESIAN_POINT ( 'NONE',  ( 0.000000000000000000, 0.000000000000000000, 41.38025477438755928 ) ) ;
#32230 = CARTESIAN_POINT ( 'NONE',  ( 55.51637278631174865, 12.08345311280958789, 9.958762847333103352 ) ) ;
#32231 = ORIENTED_EDGE ( 'NONE', *, *, #50505, .T. ) ;
#32232 = CARTESIAN_POINT ( 'NONE',  ( -128.7650348665116837, 48.41336321950710442, 45.05237689147213587 ) ) ;
#32233 = LINE ( 'NONE', #48373, #22160 ) ;
#32234 = EDGE_CURVE ( 'NONE', #46420, #52493, #24837, .T. ) ;
#32235 = ADVANCED_FACE ( 'NONE', ( #30833 ), #36450, .F. ) ;
#32236 = ADVANCED_FACE ( 'NONE', ( #9374 ), #53643, .F. ) ;
#32237 = CARTESIAN_POINT ( 'NONE',  ( 84.27368848767928000, 18.63026910897604438, -23.61379479314351570 ) ) ;
#32238 = VECTOR ( 'NONE', #2853, 1000.000000000000000 ) ;
#32239 = CARTESIAN_POINT ( 'NONE',  ( 93.70675391435743506, 21.95852801827563283, -72.66083171198076229 ) ) ;
#32240 = CARTESIAN_POINT ( 'NONE',  ( 0.000000000000000000, 0.000000000000000000, 0.000000000000000000 ) ) ;
#32241 = FACE_OUTER_BOUND ( 'NONE', #7811, .T. ) ;
#32242 = CARTESIAN_POINT ( 'NONE',  ( -154.7844486873554217, 68.78754123322237035, -90.65283450566464296 ) ) ;
#32243 = VERTEX_POINT ( 'NONE', #31862 ) ;
#32244 = ORIENTED_EDGE ( 'NONE', *, *, #40760, .T. ) ;
#32245 = EDGE_CURVE ( 'NONE', #68939, #4283, #20091, .T. ) ;
#32246 = VECTOR ( 'NONE', #24247, 1000.000000000000000 ) ;
#32247 = CARTESIAN_POINT ( 'NONE',  ( 187.5272808203428099, 85.37192123373904451, -74.44646421899427935 ) ) ;
#32248 = LINE ( 'NONE', #21331, #61028 ) ;
#32249 = CARTESIAN_POINT ( 'NONE',  ( 444.9999999999999432, 225.0000000000000000, 0.000000000000000000 ) ) ;
#32250 = LINE ( 'NONE', #27999, #7102 ) ;
#32251 = VECTOR ( 'NONE', #44848, 1000.000000000000000 ) ;
#32252 = FACE_OUTER_BOUND ( 'NONE', #52609, .T. ) ;
#32253 = CARTESIAN_POINT ( 'NONE',  ( -73.10086105983764071, 21.34631349770505082, -64.40865245798021022 ) ) ;
#32254 = CONICAL_SURFACE ( 'NONE', #9817, 4.174999999999999822, 0.9599310885968758145 ) ;
#32255 = LINE ( 'NONE', #27653, #26576 ) ;
#32256 = CARTESIAN_POINT ( 'NONE',  ( 46.90170507415071199, 10.52318308703818239, -42.62448673664831489 ) ) ;
#32257 = CARTESIAN_POINT ( 'NONE',  ( 210.6741002223296562, 114.9147155784838219, 68.09108095163148278 ) ) ;
#32258 = ORIENTED_EDGE ( 'NONE', *, *, #13977, .F. ) ;
#32259 = CARTESIAN_POINT ( 'NONE',  ( -109.5025362253418706, 36.60371748273998094, -13.58337307779724767 ) ) ;
#32260 = ORIENTED_EDGE ( 'NONE', *, *, #67454, .T. ) ;
#32262 = VECTOR ( 'NONE', #21246, 1000.000000000000000 ) ;
#32261 = CARTESIAN_POINT ( 'NONE',  ( -8.320652113663529192, 6.923290556636830573, -35.41807073194381417 ) ) ;
#32263 = CARTESIAN_POINT ( 'NONE',  ( -85.69951099329024657, 25.12635487938836931, 88.98224730508108848 ) ) ;
#32264 = CARTESIAN_POINT ( 'NONE',  ( 91.67776154311749792, 22.27748043241297538, 69.60850208772687608 ) ) ;
#32265 = CARTESIAN_POINT ( 'NONE',  ( 150.7926588734435427, 52.63999027731881597, -13.35493234247606154 ) ) ;
#32266 = CARTESIAN_POINT ( 'NONE',  ( 31.95163392065794739, 8.568192436298476267, 9.577667117831884624 ) ) ;
#32267 = CARTESIAN_POINT ( 'NONE',  ( -96.02159028238561689, 30.82695531378849196, -65.21878469105446641 ) ) ;
#32268 = CARTESIAN_POINT ( 'NONE',  ( -9.119248870808011276, 0.000000000000000000, 4.103571619000548232 ) ) ;
#32269 = ADVANCED_FACE ( 'NONE', ( #5119 ), #64914, .T. ) ;
#32270 = ADVANCED_FACE ( 'NONE', ( #891 ), #30196, .T. ) ;
#32271 = EDGE_LOOP ( 'NONE', ( #49506, #2092, #20210, #39875 ) ) ;
#32272 = CARTESIAN_POINT ( 'NONE',  ( 211.7624483073558110, 116.5638334585939333, 92.92243069068229033 ) ) ;
#32273 = CARTESIAN_POINT ( 'NONE',  ( 8.000000000000007105, 249.8719672152120381, 94.99999999999866418 ) ) ;
#32274 = ORIENTED_EDGE ( 'NONE', *, *, #41999, .F. ) ;
#32275 = DIRECTION ( 'NONE',  ( -0.000000000000000000, -0.000000000000000000, -1.000000000000000000 ) ) ;
#32277 = EDGE_CURVE ( 'NONE', #27210, #14795, #33953, .T. ) ;
#32276 = PLANE ( 'NONE',  #7305 ) ;
#32278 = CARTESIAN_POINT ( 'NONE',  ( 46.90170507415071910, 10.52318308703818062, -69.46903732711203361 ) ) ;
#32279 = CARTESIAN_POINT ( 'NONE',  ( 282.5114001799272501, -21.56931564127029688, 4.335727404899786919 ) ) ;
#32280 = DIRECTION ( 'NONE',  ( -1.000000000000000000, 0.000000000000000000, 0.000000000000000000 ) ) ;
#32281 = CARTESIAN_POINT ( 'NONE',  ( 80.34841469379381351, 18.42674688750400946, 94.99999999999866418 ) ) ;
#32282 = EDGE_LOOP ( 'NONE', ( #64179, #334, #31274, #3076 ) ) ;
#32283 = DIRECTION ( 'NONE',  ( 9.444454853639938104E-15, -4.018160899990246952E-15, 0.9999999999999998890 ) ) ;
#32284 = CARTESIAN_POINT ( 'NONE',  ( -190.4968431727838833, 108.8425311198514720, -19.44418843322370805 ) ) ;
#32285 = CARTESIAN_POINT ( 'NONE',  ( -130.6002960060536964, 49.67125682092490990, 5.415878727382473556 ) ) ;
#32286 = CARTESIAN_POINT ( 'NONE',  ( -103.2061297292849531, 34.38496953192504435, 57.40642899071801963 ) ) ;
#32287 = CARTESIAN_POINT ( 'NONE',  ( -132.4896623150434323, 52.22616402022728721, -38.83446270130018974 ) ) ;
#32288 = ORIENTED_EDGE ( 'NONE', *, *, #25989, .T. ) ;
#32289 = FACE_OUTER_BOUND ( 'NONE', #32831, .T. ) ;
#32290 = CARTESIAN_POINT ( 'NONE',  ( 93.63037639125413136, 21.92981100938040484, 66.75823669843309460 ) ) ;
#32291 = VECTOR ( 'NONE', #45002, 1000.000000000000114 ) ;
#32292 = B_SPLINE_CURVE_WITH_KNOTS ( 'NONE', 3,
 ( #20612, #64215, #31870, #38174, #42072, #189, #69141, #59616, #15690, #11430, #21647, #63536, #59276, #37482, #11094, #5477, #32557, #53299, #15350, #42420, #63880, #53987, #10066, #32219, #37138, #5812, #27266, #48706, #58582, #36806, #31526, #26590, #48027, #60332, #12153, #43787, #39920, #22696, #49760, #49063, #12856, #33619, #55047, #38525, #2300, #1244 ),
 .UNSPECIFIED., .F., .F.,
 ( 4, 2, 2, 2, 2, 2, 2, 2, 2, 2, 2, 2, 2, 2, 2, 2, 2, 2, 2, 2, 2, 2, 4 ),
 ( 0.02404638330965502488, 0.02555608299537557443, 0.02631093283823585441, 0.02706578268109613092, 0.02857548236681668741, 0.02933033220967695698, 0.03008518205253722655, 0.03159488173825776569, 0.03310458142397830483, 0.03385943126683858134, 0.03461428110969885785, 0.03612398079541943863, 0.03687883063827972208, 0.03763368048114001246, 0.03838853032400030285, 0.03914338016686058630, 0.04065307985258116708, 0.04216277953830173397, 0.04367247922402230781, 0.04518217890974288165, 0.04593702875260315122, 0.04669187859546342079, 0.04820157828118395993 ),
 .UNSPECIFIED. ) ;
#32293 = CARTESIAN_POINT ( 'NONE',  ( -439.4229916354182706, 394.9999999999998295, -123.9497041420119530 ) ) ;
#32294 = CARTESIAN_POINT ( 'NONE',  ( -149.0738659721762076, 63.81256528267484640, 84.41759755226209450 ) ) ;
#32295 = CIRCLE ( 'NONE', #49134, 10.00000000000000178 ) ;
#32296 = APPLICATION_CONTEXT ( 'automotive_design' ) ;
#32297 = CARTESIAN_POINT ( 'NONE',  ( 140.9169160367233076, 45.85398962664667977, 39.59428667614358233 ) ) ;
#32298 = ORIENTED_EDGE ( 'NONE', *, *, #49351, .T. ) ;
#32299 = CARTESIAN_POINT ( 'NONE',  ( 311.9975424824652350, 170.0000000000000284, 255.6641978984094408 ) ) ;
#32300 = CARTESIAN_POINT ( 'NONE',  ( 79.22872707466396491, 18.07970189365808622, 11.61010380891110572 ) ) ;
#32301 = VECTOR ( 'NONE', #7545, 1000.000000000000000 ) ;
#32302 = FACE_OUTER_BOUND ( 'NONE', #33730, .T. ) ;
#32303 = DIRECTION ( 'NONE',  ( 0.000000000000000000, 0.000000000000000000, 1.000000000000000000 ) ) ;
#32304 = ORIENTED_EDGE ( 'NONE', *, *, #26202, .F. ) ;
#32305 = VECTOR ( 'NONE', #33450, 1000.000000000000000 ) ;
#32306 = LINE ( 'NONE', #17500, #18270 ) ;
#32307 = ORIENTED_EDGE ( 'NONE', *, *, #25587, .T. ) ;
#32308 = VECTOR ( 'NONE', #68163, 1000.000000000000000 ) ;
#32310 = EDGE_CURVE ( 'NONE', #48012, #42925, #33257, .T. ) ;
#32309 = CARTESIAN_POINT ( 'NONE',  ( -73.63346300764936814, 20.46798018699518451, -21.33674241584527920 ) ) ;
#32311 = CARTESIAN_POINT ( 'NONE',  ( 70.26722489419888973, 14.47234958177330455, -72.04276696937047575 ) ) ;
#32312 = DIRECTION ( 'NONE',  ( 1.000000000000000000, 0.000000000000000000, 0.000000000000000000 ) ) ;
#32314 = ORIENTED_EDGE ( 'NONE', *, *, #14638, .F. ) ;
#32313 = FACE_OUTER_BOUND ( 'NONE', #37588, .T. ) ;
#32315 = CARTESIAN_POINT ( 'NONE',  ( 164.9709596662455056, 63.72607097915132357, 37.17312740752070965 ) ) ;
#32316 = DIRECTION ( 'NONE',  ( -0.000000000000000000, -0.000000000000000000, -1.000000000000000000 ) ) ;
#32317 = CYLINDRICAL_SURFACE ( 'NONE', #56455, 20.00000000000000355 ) ;
#32318 = VERTEX_POINT ( 'NONE', #22690 ) ;
#32319 = DIRECTION ( 'NONE',  ( -0.000000000000000000, 1.000000000000000000, -0.000000000000000000 ) ) ;
#32320 = ADVANCED_FACE ( 'NONE', ( #27612 ), #54692, .T. ) ;
#32321 = CARTESIAN_POINT ( 'NONE',  ( -422.6627218934913230, 1.665334536937734811E-13, 113.5502958579881749 ) ) ;
#32322 = CARTESIAN_POINT ( 'NONE',  ( -166.7049310409072405, 80.25944422923581101, 42.21435027861289768 ) ) ;
#32323 = CARTESIAN_POINT ( 'NONE',  ( 133.4058733589413634, 42.32720528873925048, 56.35489142945903751 ) ) ;
#32324 = EDGE_CURVE ( 'NONE', #37671, #57004, #3229, .T. ) ;
#32325 = ORIENTED_EDGE ( 'NONE', *, *, #68737, .F. ) ;
#32326 = EDGE_CURVE ( 'NONE', #3913, #5640, #50124, .T. ) ;
#32327 = ORIENTED_EDGE ( 'NONE', *, *, #12726, .T. ) ;
#32328 = ORIENTED_EDGE ( 'NONE', *, *, #64810, .F. ) ;
#32329 = FACE_OUTER_BOUND ( 'NONE', #1389, .T. ) ;
#32330 = CARTESIAN_POINT ( 'NONE',  ( -107.0544991134679691, 36.41543129049375693, 5.385398075284562047 ) ) ;
#32331 = CARTESIAN_POINT ( 'NONE',  ( -65.36598343705435354, 0.000000000000000000, 41.38025477438755928 ) ) ;
#32332 = CARTESIAN_POINT ( 'NONE',  ( -156.4841188516943191, 70.33041971808555104, -71.92384636904367312 ) ) ;
#32333 = AXIS2_PLACEMENT_3D ( 'NONE', #26246, #63528, #63875 ) ;
#32334 = CARTESIAN_POINT ( 'NONE',  ( 69.36122620657974380, 14.23458312296499528, 94.99999999999866418 ) ) ;
#32335 = PLANE ( 'NONE',  #3362 ) ;
#32336 = CARTESIAN_POINT ( 'NONE',  ( 0.000000000000000000, 0.000000000000000000, 41.38025477438755928 ) ) ;
#32337 = CARTESIAN_POINT ( 'NONE',  ( 68.07999999999999829, -26.09918303830819397, 30.00000000000000000 ) ) ;
#32338 = ORIENTED_EDGE ( 'NONE', *, *, #35097, .T. ) ;
#32339 = CIRCLE ( 'NONE', #34622, 5.000000000000004441 ) ;
#32340 = FACE_OUTER_BOUND ( 'NONE', #28153, .T. ) ;
#32341 = ORIENTED_EDGE ( 'NONE', *, *, #11548, .F. ) ;
#32342 = CARTESIAN_POINT ( 'NONE',  ( -84.49322488516129681, 0.000000000000000000, 43.58025477438756212 ) ) ;
#32343 = CARTESIAN_POINT ( 'NONE',  ( 211.7419975634645368, 116.5322580952101532, -73.32492906585233072 ) ) ;
#32344 = CARTESIAN_POINT ( 'NONE',  ( -20.55634918610400419, 15.55634918610405748, 85.00100000000000477 ) ) ;
#32345 = AXIS2_PLACEMENT_3D ( 'NONE', #9106, #23897, #7724 ) ;
#32346 = CARTESIAN_POINT ( 'NONE',  ( 412.3372781065085633, 397.0710678118654755, -111.4497041420117824 ) ) ;
#32347 = FACE_OUTER_BOUND ( 'NONE', #24116, .T. ) ;
#32348 = CARTESIAN_POINT ( 'NONE',  ( 23.09590709048883994, 7.852755081912510704, 39.22044207619089917 ) ) ;
#32349 = CARTESIAN_POINT ( 'NONE',  ( 197.8045642144698206, 97.34517417643259307, 93.35912461664177897 ) ) ;
#32350 = VECTOR ( 'NONE', #28509, 1000.000000000000000 ) ;
#32351 = LINE ( 'NONE', #48153, #33330 ) ;
#32352 = ORIENTED_EDGE ( 'NONE', *, *, #60104, .F. ) ;
#32353 = DIRECTION ( 'NONE',  ( -0.000000000000000000, -0.000000000000000000, -1.000000000000000000 ) ) ;
#32354 = DIRECTION ( 'NONE',  ( -0.000000000000000000, -0.000000000000000000, 1.000000000000000000 ) ) ;
#32355 = ORIENTED_EDGE ( 'NONE', *, *, #54860, .F. ) ;
#32356 = EDGE_CURVE ( 'NONE', #35709, #58120, #42526, .T. ) ;
#32357 = VERTEX_POINT ( 'NONE', #65617 ) ;
#32358 = CARTESIAN_POINT ( 'NONE',  ( -29.50439180771548564, 10.29976981300624850, -76.92427033250436352 ) ) ;
#32359 = CARTESIAN_POINT ( 'NONE',  ( 58.09436971064712907, 11.58462396079456980, -37.53989357320173781 ) ) ;
#32360 = CARTESIAN_POINT ( 'NONE',  ( -24.32937228292060894, 8.531905774118440533, 62.12288946467717210 ) ) ;
#32361 = VECTOR ( 'NONE', #28540, 1000.000000000000000 ) ;
#32362 = LINE ( 'NONE', #58724, #54371 ) ;
#32363 = B_SPLINE_CURVE_WITH_KNOTS ( 'NONE', 3,
 ( #38786, #45088, #50382, #50024, #34208, #12398, #28572, #1858, #55644, #2198, #2537, #66574, #34566, #31006, #30655, #4269, #46131, #57385, #29606, #40509, #66921, #18716, #57047, #56341, #19057, #14127, #61957, #62312, #41553, #14477, #61625, #46474, #34902, #2885, #62670, #36273, #25040, #13777, #35237, #56692, #24694, #63007, #30312, #40168, #35933 ),
 .UNSPECIFIED., .F., .F.,
 ( 4, 2, 2, 2, 2, 2, 2, 2, 2, 2, 2, 1, 2, 2, 2, 2, 2, 2, 2, 2, 2, 2, 4 ),
 ( 1.430489624538199204E-17, 0.001502898956853363811, 0.002254348435280040513, 0.003005797913706716781, 0.004508696870560108781, 0.005260146348986821478, 0.006011595827413535043, 0.007514494784267020284, 0.009017393741120507261, 0.01052029269797399164, 0.01127174217640075117, 0.01202319165482751070, 0.01277464113325426677, 0.01352609061168102457, 0.01502898956853450201, 0.01578043904696122338, 0.01653188852538794301, 0.01803478748224135106, 0.01953768643909475911, 0.02028913591752146486, 0.02104058539594816715, 0.02254348435280160989, 0.02404638330965504917 ),
 .UNSPECIFIED. ) ;
#32364 = EDGE_LOOP ( 'NONE', ( #39753, #17011, #47505, #59219 ) ) ;
#32365 = VERTEX_POINT ( 'NONE', #49409 ) ;
#32366 = CARTESIAN_POINT ( 'NONE',  ( -128.9863978264385196, 49.78205252558957739, 44.95660336865451967 ) ) ;
#32367 = ORIENTED_EDGE ( 'NONE', *, *, #39061, .T. ) ;
#32368 = LINE ( 'NONE', #42570, #30090 ) ;
#32369 = CARTESIAN_POINT ( 'NONE',  ( -142.8492950481059438, 60.01492924994603584, 34.75812731920188270 ) ) ;
#32370 = CARTESIAN_POINT ( 'NONE',  ( 55.90536342106781831, 11.13510150712953362, 61.72041802730606719 ) ) ;
#32371 = CARTESIAN_POINT ( 'NONE',  ( -24.87827947785784133, 3.494138152041632583, 0.000000000000000000 ) ) ;
#32372 = SURFACE_SIDE_STYLE ('',( #5620 ) ) ;
#32373 = LINE ( 'NONE', #27078, #56260 ) ;
#32374 = DIRECTION ( 'NONE',  ( 0.000000000000000000, -1.000000000000000000, -1.110223024625156171E-16 ) ) ;
#32375 = VERTEX_POINT ( 'NONE', #28671 ) ;
#32376 = ORIENTED_EDGE ( 'NONE', *, *, #34324, .F. ) ;
#32377 = PLANE ( 'NONE',  #40170 ) ;
#32378 = CARTESIAN_POINT ( 'NONE',  ( 0.000000000000000000, 0.000000000000000000, 0.000000000000000000 ) ) ;
#32379 = CARTESIAN_POINT ( 'NONE',  ( -171.4814970982679938, 85.32124710276288226, -8.037032661340148820 ) ) ;
#32380 = FACE_OUTER_BOUND ( 'NONE', #52321, .T. ) ;
#32381 = CARTESIAN_POINT ( 'NONE',  ( 70.51601918574517924, 14.53832276813547608, 37.55138390113663149 ) ) ;
#32382 = CARTESIAN_POINT ( 'NONE',  ( 8.621086886543794847, 7.383195413572584798, 88.96999900602391165 ) ) ;
#32383 = EDGE_CURVE ( 'NONE', #28214, #22131, #23472, .T. ) ;
#32384 = ORIENTED_EDGE ( 'NONE', *, *, #55773, .F. ) ;
#32385 = EDGE_CURVE ( 'NONE', #16778, #24416, #1237, .T. ) ;
#32386 = ADVANCED_BREP_SHAPE_REPRESENTATION ( '', ( #20791, #66832 ), #29803 ) ;
#32387 = CARTESIAN_POINT ( 'NONE',  ( 82.14449817946437804, 17.93919511903896336, 16.38389564114189412 ) ) ;
#32388 = EDGE_CURVE ( 'NONE', #67298, #9035, #29093, .T. ) ;
#32389 = ORIENTED_EDGE ( 'NONE', *, *, #12905, .F. ) ;
#32391 = CARTESIAN_POINT ( 'NONE',  ( -75.64857587248467041, 21.19501514561449440, 44.78839637111028082 ) ) ;
#32390 = VECTOR ( 'NONE', #19051, 1000.000000000000114 ) ;
#32392 = VERTEX_POINT ( 'NONE', #38882 ) ;
#32393 = EDGE_CURVE ( 'NONE', #61540, #61512, #60326, .T. ) ;
#32394 = VECTOR ( 'NONE', #56782, 1000.000000000000000 ) ;
#32395 = ORIENTED_EDGE ( 'NONE', *, *, #22057, .T. ) ;
#32396 = CARTESIAN_POINT ( 'NONE',  ( -121.5680658099884113, 44.89994870382101055, 5.130273036901130901 ) ) ;
#32397 = CARTESIAN_POINT ( 'NONE',  ( -179.0654441437004323, 93.99779465816534696, 60.58611069645034775 ) ) ;
#32398 = DIRECTION ( 'NONE',  ( -0.8118923937861950435, -0.5838071093367415143, 0.000000000000000000 ) ) ;
#32399 = ORIENTED_EDGE ( 'NONE', *, *, #16820, .F. ) ;
#32400 = CARTESIAN_POINT ( 'NONE',  ( 157.4703587214989113, 57.65129005721576050, -9.279633708673953763 ) ) ;
#32401 = CARTESIAN_POINT ( 'NONE',  ( 151.6351261592328683, 53.25263237790399273, 41.62792433286728766 ) ) ;
#32402 = CARTESIAN_POINT ( 'NONE',  ( 69.49112875363883290, 15.30845942322121367, 33.52089747499180561 ) ) ;
#32403 = DIRECTION ( 'NONE',  ( 0.000000000000000000, -1.000000000000000000, 1.479221584281239571E-31 ) ) ;
#32404 = CARTESIAN_POINT ( 'NONE',  ( 0.000000000000000000, 0.000000000000000000, 170.0000000000000000 ) ) ;
#32405 = ADVANCED_FACE ( 'NONE', ( #17772 ), #11085, .F. ) ;
#32406 = DIRECTION ( 'NONE',  ( 0.000000000000000000, 0.000000000000000000, 1.000000000000000000 ) ) ;
#32407 = CARTESIAN_POINT ( 'NONE',  ( 136.9654665832767932, 44.52067472585214603, -63.53847950313026871 ) ) ;
#32409 = ADVANCED_FACE ( 'NONE', ( #65255 ), #60675, .F. ) ;
#32408 = CARTESIAN_POINT ( 'NONE',  ( -142.3187766126154941, 59.59460822661993973, -71.36695520502316015 ) ) ;
#32410 = VERTEX_POINT ( 'NONE', #39229 ) ;
#32411 = FACE_BOUND ( 'NONE', #18407, .T. ) ;
#32412 = CARTESIAN_POINT ( 'NONE',  ( -5.885876544836655455, 6.772369038004113939, -77.01165322372530397 ) ) ;
#32413 = CARTESIAN_POINT ( 'NONE',  ( -179.2128128997734109, 95.75254520622991095, 60.76269154493880364 ) ) ;
#32414 = CARTESIAN_POINT ( 'NONE',  ( 50.03867889673374236, -42.05760816978110483, 3.125053320693570611E-16 ) ) ;
#32415 = CARTESIAN_POINT ( 'NONE',  ( -118.4106078162223668, 42.93830006159888768, -41.84395280496732283 ) ) ;
#32416 = CARTESIAN_POINT ( 'NONE',  ( -82.32006615997345023, 24.83050031643766431, 4.505854562011677444 ) ) ;
#32417 = PLANE ( 'NONE',  #40441 ) ;
#32418 = CARTESIAN_POINT ( 'NONE',  ( -153.5002794404625774, 67.64160439471098130, 5.023374128941582306 ) ) ;
#32419 = CARTESIAN_POINT ( 'NONE',  ( -6.843910203392212566, 7.836697961436722260, -8.622009400863452910 ) ) ;
#32420 = CARTESIAN_POINT ( 'NONE',  ( 70.38121398871578549, 14.50253776029980557, 11.94555559055825711 ) ) ;
#32421 = CARTESIAN_POINT ( 'NONE',  ( -86.16710354151693707, 26.41338104675949339, 64.99724543193327975 ) ) ;
#32422 = CARTESIAN_POINT ( 'NONE',  ( 91.11019107624154856, 22.06959540317787827, -10.45776451510279159 ) ) ;
#32423 = VERTEX_POINT ( 'NONE', #7215 ) ;
#32424 = CARTESIAN_POINT ( 'NONE',  ( -35.17296606710972640, 11.25626711331309160, 4.348805324083214074 ) ) ;
#32425 = VERTEX_POINT ( 'NONE', #53978 ) ;
#32426 = CARTESIAN_POINT ( 'NONE',  ( -54.99999999999995026, 7.960204194457792519E-15, 0.000000000000000000 ) ) ;
#32427 = ORIENTED_EDGE ( 'NONE', *, *, #62455, .T. ) ;
#32428 = CARTESIAN_POINT ( 'NONE',  ( 19.54326199789021246, 7.657220834818548205, -76.36046258218678418 ) ) ;
#32429 = CARTESIAN_POINT ( 'NONE',  ( 108.6949225693525847, 29.27769766909357330, 83.45484555132844662 ) ) ;
#32430 = CARTESIAN_POINT ( 'NONE',  ( -146.5230751932348596, 62.99205605665029850, 58.17019016430769796 ) ) ;
#32431 = CARTESIAN_POINT ( 'NONE',  ( 68.95451040317564662, 14.12887482153123031, -11.76939062271155656 ) ) ;
#32432 = CARTESIAN_POINT ( 'NONE',  ( -29.03891846981456126, 10.22741474064059020, -49.93962856602705358 ) ) ;
#32433 = CARTESIAN_POINT ( 'NONE',  ( 208.0011962801381458, 112.7551321982796111, -90.77262215979118309 ) ) ;
#32434 = CARTESIAN_POINT ( 'NONE',  ( -71.48055013538424873, 20.77798539480599160, -94.11067968272816131 ) ) ;
#32435 = CARTESIAN_POINT ( 'NONE',  ( -124.9915686518654638, 47.10215472274616388, -8.069153307770244865 ) ) ;
#32436 = ORIENTED_EDGE ( 'NONE', *, *, #56304, .T. ) ;
#32437 = ORIENTED_EDGE ( 'NONE', *, *, #10456, .F. ) ;
#32438 = CARTESIAN_POINT ( 'NONE',  ( 37.45439421541016145, 9.177432671831372346, 71.51784865638920508 ) ) ;
#32439 = CARTESIAN_POINT ( 'NONE',  ( -173.1211646369891355, 88.63826465341152527, 72.66624519710475738 ) ) ;
#32440 = DIRECTION ( 'NONE',  ( 0.000000000000000000, 0.000000000000000000, -1.000000000000000000 ) ) ;
#32441 = AXIS2_PLACEMENT_3D ( 'NONE', #53293, #52615, #4440 ) ;
#32442 = PRODUCT_DEFINITION_CONTEXT ( 'detailed design', #51204, 'design' ) ;
#32443 = LINE ( 'NONE', #53871, #40909 ) ;
#32444 = ORIENTED_EDGE ( 'NONE', *, *, #50903, .T. ) ;
#32445 = CARTESIAN_POINT ( 'NONE',  ( 284.3399910931246950, 21.85871988289598988, 2.504349266409120478 ) ) ;
#32446 = CARTESIAN_POINT ( 'NONE',  ( 188.4374648754671284, 87.87346242052439038, -18.38533621105863958 ) ) ;
#32447 = FACE_OUTER_BOUND ( 'NONE', #65889, .T. ) ;
#32448 = DIRECTION ( 'NONE',  ( -0.000000000000000000, -0.000000000000000000, 1.000000000000000000 ) ) ;
#32449 = CARTESIAN_POINT ( 'NONE',  ( 422.4999999999999432, 207.5000000000000284, 1.999999999999998224 ) ) ;
#32450 = CARTESIAN_POINT ( 'NONE',  ( 209.4789161463551181, 113.1367444519304115, -22.76410597263823377 ) ) ;
#32451 = DIRECTION ( 'NONE',  ( 1.000000000000000000, -9.109522253334613014E-16, 0.000000000000000000 ) ) ;
#32452 = CARTESIAN_POINT ( 'NONE',  ( -149.5074843970971301, -170.0000000000000000, 3.876270649435373805 ) ) ;
#32453 = ORIENTED_EDGE ( 'NONE', *, *, #32554, .T. ) ;
#32454 = DIRECTION ( 'NONE',  ( -0.000000000000000000, 0.000000000000000000, -1.000000000000000000 ) ) ;
#32455 = DIRECTION ( 'NONE',  ( 1.000000000000000000, 0.000000000000000000, 0.000000000000000000 ) ) ;
#32456 = CARTESIAN_POINT ( 'NONE',  ( -48.71337292867759317, 14.10768470390587659, 68.67724857654715720 ) ) ;
#32457 = CARTESIAN_POINT ( 'NONE',  ( -5.000000000000073719, -46.66904755831211560, 2.000000000000001776 ) ) ;
#32458 = DIRECTION ( 'NONE',  ( 0.000000000000000000, 0.000000000000000000, 1.000000000000000000 ) ) ;
#32459 = CARTESIAN_POINT ( 'NONE',  ( 417.3372781065085633, 400.0000000000000568, -146.4497041420118251 ) ) ;
#32460 = ORIENTED_EDGE ( 'NONE', *, *, #49625, .T. ) ;
#32461 = CARTESIAN_POINT ( 'NONE',  ( 61.33627421985470818, 12.28939706835343237, 17.78195680140521162 ) ) ;
#32462 = FACE_OUTER_BOUND ( 'NONE', #8279, .T. ) ;
#32463 = EDGE_CURVE ( 'NONE', #57236, #38237, #26814, .T. ) ;
#32464 = VERTEX_POINT ( 'NONE', #540 ) ;
#32465 = ORIENTED_EDGE ( 'NONE', *, *, #52861, .F. ) ;
#32466 = CARTESIAN_POINT ( 'NONE',  ( 46.90632335736349745, 10.52393368783804561, 90.89396992506641482 ) ) ;
#32467 = DIRECTION ( 'NONE',  ( -0.3754023374827052950, 0.9268613172740186590, -0.001087912492708085609 ) ) ;
#32468 = ADVANCED_FACE ( 'NONE', ( #59269 ), #5805, .F. ) ;
#32469 = CARTESIAN_POINT ( 'NONE',  ( 103.8093541423578898, 26.01745837747064982, 33.22445973737408309 ) ) ;
#32470 = ORIENTED_EDGE ( 'NONE', *, *, #7255, .T. ) ;
#32471 = CARTESIAN_POINT ( 'NONE',  ( -62.30463872474476972, 16.74658165105247321, -71.53854161899334940 ) ) ;
#32472 = EDGE_CURVE ( 'NONE', #60845, #64884, #45189, .T. ) ;
#32473 = CARTESIAN_POINT ( 'NONE',  ( 32.56927464314650678, 7.618924692399903442, -19.37770249060224614 ) ) ;
#32474 = CARTESIAN_POINT ( 'NONE',  ( 175.5498284945444709, 74.57669191966280664, -48.81277339523749959 ) ) ;
#32475 = CARTESIAN_POINT ( 'NONE',  ( 164.6177656728407044, 63.42876281302249453, 88.29515807379765135 ) ) ;
#32476 = CARTESIAN_POINT ( 'NONE',  ( 8.000000000000000000, 4.618802153517024500, -8.785468820183664818 ) ) ;
#32477 = VERTEX_POINT ( 'NONE', #8256 ) ;
#32478 = CARTESIAN_POINT ( 'NONE',  ( -50.14523569787233725, 14.45648954445650780, -48.40948618845168738 ) ) ;
#32479 = DIRECTION ( 'NONE',  ( 2.312964634635743450E-16, -0.000000000000000000, 1.000000000000000000 ) ) ;
#32481 = EDGE_CURVE ( 'NONE', #42236, #9171, #7911, .T. ) ;
#32480 = CARTESIAN_POINT ( 'NONE',  ( 11.20486344102687326, 7.403248964808830657, 43.47161425690537584 ) ) ;
#32482 = LINE ( 'NONE', #53914, #111 ) ;
#32484 = FACE_BOUND ( 'NONE', #1283, .T. ) ;
#32483 = CIRCLE ( 'NONE', #61714, 242.4895526022646379 ) ;
#32485 = CARTESIAN_POINT ( 'NONE',  ( -85.35521056349260505, 26.07297753498038873, 94.99999999999866418 ) ) ;
#32487 = ORIENTED_EDGE ( 'NONE', *, *, #52728, .T. ) ;
#32486 = CARTESIAN_POINT ( 'NONE',  ( -24.53636015449704644, -60.58612729876431047, 3.125053320693577513E-16 ) ) ;
#32488 = VERTEX_POINT ( 'NONE', #61710 ) ;
#32489 = VECTOR ( 'NONE', #53290, 1000.000000000000000 ) ;
#32490 = VERTEX_POINT ( 'NONE', #46221 ) ;
#32491 = CARTESIAN_POINT ( 'NONE',  ( -14.66033866466834823, 7.432913330382389105, -19.17095739190610004 ) ) ;
#32492 = FACE_OUTER_BOUND ( 'NONE', #24686, .T. ) ;
#32493 = CARTESIAN_POINT ( 'NONE',  ( 0.000000000000000000, 0.000000000000000000, -25.03750572909317285 ) ) ;
#32494 = CARTESIAN_POINT ( 'NONE',  ( 0.000000000000000000, 0.000000000000000000, 41.38025477438755928 ) ) ;
#32495 = CARTESIAN_POINT ( 'NONE',  ( -36.38071096718371678, 11.47804921491337993, 70.22400354125137767 ) ) ;
#32496 = CARTESIAN_POINT ( 'NONE',  ( -11.56945424397728672, 8.173256823723106024, -22.57675618948779217 ) ) ;
#32497 = CARTESIAN_POINT ( 'NONE',  ( 0.000000000000000000, 0.000000000000000000, 0.000000000000000000 ) ) ;
#32498 = CARTESIAN_POINT ( 'NONE',  ( 16.77391662606470391, 6.533867394142986562, -8.723007401148960227 ) ) ;
#32499 = VERTEX_POINT ( 'NONE', #23743 ) ;
#32500 = CARTESIAN_POINT ( 'NONE',  ( 63.01563776193091826, -170.0000000000000000, -16.37614024170606797 ) ) ;
#32501 = ORIENTED_EDGE ( 'NONE', *, *, #10997, .F. ) ;
#32502 = ORIENTED_EDGE ( 'NONE', *, *, #2252, .F. ) ;
#32503 = CARTESIAN_POINT ( 'NONE',  ( 67.55199883153193241, 14.80832170058782715, -22.36842963500835069 ) ) ;
#32504 = DIRECTION ( 'NONE',  ( -0.000000000000000000, 0.000000000000000000, -1.000000000000000000 ) ) ;
#32505 = CARTESIAN_POINT ( 'NONE',  ( -24.14271535429456605, 9.522144728394469126, 89.63976553000811975 ) ) ;
#32506 = AXIS2_PLACEMENT_3D ( 'NONE', #18920, #37158, #5153 ) ;
#32507 = CARTESIAN_POINT ( 'NONE',  ( -157.0079874970173535, 72.18249880494043680, 11.64991257542693859 ) ) ;
#32508 = CYLINDRICAL_SURFACE ( 'NONE', #21446, 89.99999999999998579 ) ;
#32509 = CARTESIAN_POINT ( 'NONE',  ( 445.3372781065085633, 217.8591479523844612, -111.4497041420119388 ) ) ;
#32510 = CARTESIAN_POINT ( 'NONE',  ( -156.2646585454849344, 71.49501546611418235, 88.63874933570780001 ) ) ;
#32511 = VERTEX_POINT ( 'NONE', #3662 ) ;
#32512 = EDGE_LOOP ( 'NONE', ( #22601, #30247, #43036, #42455 ) ) ;
#32513 = ORIENTED_EDGE ( 'NONE', *, *, #8907, .F. ) ;
#32514 = CARTESIAN_POINT ( 'NONE',  ( 0.000000000000000000, 0.000000000000000000, 0.000000000000000000 ) ) ;
#32515 = CARTESIAN_POINT ( 'NONE',  ( 0.000000000000000000, 200.0000000000000000, -10.00000000000000000 ) ) ;
#32516 = CARTESIAN_POINT ( 'NONE',  ( -38.15923928782688535, 10.79140400702258695, 67.90023288991038442 ) ) ;
#32517 = VECTOR ( 'NONE', #21418, 1000.000000000000000 ) ;
#32518 = CARTESIAN_POINT ( 'NONE',  ( 197.2847860006354495, 98.30530166401517533, 62.40104121888823130 ) ) ;
#32519 = ORIENTED_EDGE ( 'NONE', *, *, #34342, .T. ) ;
#32520 = CARTESIAN_POINT ( 'NONE',  ( 188.4918087359956189, 87.93403732562654795, 62.44201370830596431 ) ) ;
#32521 = CARTESIAN_POINT ( 'NONE',  ( -153.6931187576189188, 67.81270084382354923, 58.83762594297919435 ) ) ;
#32522 =( NAMED_UNIT ( * ) SI_UNIT ( $, .STERADIAN. ) SOLID_ANGLE_UNIT ( ) );
#32523 = ADVANCED_FACE ( 'NONE', ( #29361 ), #39914, .F. ) ;
#32524 = CARTESIAN_POINT ( 'NONE',  ( 45.39413431650373809, 0.000000000000000000, 5.000000000000000000 ) ) ;
#32525 = CARTESIAN_POINT ( 'NONE',  ( 103.8317086684999992, 26.02720265156212776, 14.16654748491671256 ) ) ;
#32526 = DIRECTION ( 'NONE',  ( 0.7071067811865476838, -5.551115123125782086E-17, 0.7071067811865473507 ) ) ;
#32527 = CARTESIAN_POINT ( 'NONE',  ( -443.6249203811465804, 394.9114286947786354, -131.6832696988547298 ) ) ;
#32528 = CYLINDRICAL_SURFACE ( 'NONE', #56662, 65.36598343705435354 ) ;
#32529 = FACE_OUTER_BOUND ( 'NONE', #29690, .T. ) ;
#32530 = CARTESIAN_POINT ( 'NONE',  ( 55.00000000000000000, 16.00000000000000000, 6.196318915105386793 ) ) ;
#32531 = VERTEX_POINT ( 'NONE', #50814 ) ;
#32532 = DIRECTION ( 'NONE',  ( -0.000000000000000000, -0.000000000000000000, -1.000000000000000000 ) ) ;
#32533 = CONTEXT_DEPENDENT_SHAPE_REPRESENTATION ( #61968, #1282 ) ;
#32534 = CARTESIAN_POINT ( 'NONE',  ( 179.4207200232660853, 76.93724985992177778, 44.17255298202294256 ) ) ;
#32535 = CARTESIAN_POINT ( 'NONE',  ( -133.0808647576834289, 51.41195281028756625, -40.25360747411231443 ) ) ;
#32536 = FACE_OUTER_BOUND ( 'NONE', #11292, .T. ) ;
#32537 = AXIS2_PLACEMENT_3D ( 'NONE', #61459, #11874, #2037 ) ;
#32538 = CARTESIAN_POINT ( 'NONE',  ( 181.9295958320008708, 80.90438706151873305, -51.18938441524608152 ) ) ;
#32539 = ORIENTED_EDGE ( 'NONE', *, *, #10463, .T. ) ;
#32540 = EDGE_LOOP ( 'NONE', ( #32832, #7291, #46023, #3080 ) ) ;
#32541 = ADVANCED_FACE ( 'NONE', ( #18119 ), #67356, .T. ) ;
#32542 = CARTESIAN_POINT ( 'NONE',  ( -78.66644367742111399, -170.0000000000000000, 72.26275173013684139 ) ) ;
#32543 = CARTESIAN_POINT ( 'NONE',  ( 174.8714394078361352, 72.54688047260668782, 94.71445689663468670 ) ) ;
#32544 = EDGE_CURVE ( 'NONE', #2294, #65415, #18944, .T. ) ;
#32545 = ORIENTED_EDGE ( 'NONE', *, *, #7043, .F. ) ;
#32546 = ORIENTED_EDGE ( 'NONE', *, *, #67973, .T. ) ;
#32547 = PLANE ( 'NONE',  #48749 ) ;
#32548 = DIRECTION ( 'NONE',  ( 0.000000000000000000, -0.04541273895899431562, 0.9989683093773507050 ) ) ;
#32549 = VERTEX_POINT ( 'NONE', #24783 ) ;
#32550 = CARTESIAN_POINT ( 'NONE',  ( 117.3145357257065911, 33.41973663092564806, 66.50590971767826431 ) ) ;
#32551 = CARTESIAN_POINT ( 'NONE',  ( 424.8372781065088475, 395.0000000000001137, -123.9497041420121235 ) ) ;
#32552 = CARTESIAN_POINT ( 'NONE',  ( 141.1220430186942565, 47.19066702031173577, 65.73481338491475867 ) ) ;
#32553 = CARTESIAN_POINT ( 'NONE',  ( -71.22878586122430988, 19.62649588091171893, -41.61736384448404635 ) ) ;
#32554 = EDGE_CURVE ( 'NONE', #25366, #66496, #13195, .T. ) ;
#32555 = VECTOR ( 'NONE', #52733, 1000.000000000000000 ) ;
#32556 = CARTESIAN_POINT ( 'NONE',  ( 86.23158543793178410, 19.28538367132613374, -89.51066537983908233 ) ) ;
#32557 = CARTESIAN_POINT ( 'NONE',  ( 93.32502112557683915, 21.81526022999039327, -46.73702075745129036 ) ) ;
#32558 = B_SPLINE_CURVE_WITH_KNOTS ( 'NONE', 3,
 ( #2007, #3042, #66383, #2347, #39971, #55808, #44901, #8317, #24504, #7630, #46275, #19196, #40657, #67752, #19552, #26212, #41699, #52592, #57194, #47303, #42041, #4075, #14620, #36422, #30454, #30806, #68764, #14957, #25539, #41012, #68101, #25193, #15313, #46975, #47652, #46626, #20931, #10035, #26557, #63164, #4749, #31832, #31162, #9012, #5097 ),
 .UNSPECIFIED., .F., .F.,
 ( 4, 2, 2, 2, 2, 2, 2, 2, 1, 2, 2, 2, 2, 2, 2, 2, 2, 2, 2, 2, 2, 2, 4 ),
 ( 0.000000000000000000, 0.001470449819620697676, 0.002205674729431036755, 0.002940899639241375402, 0.004411349458862033612, 0.005881799278482692690, 0.007352249098103350901, 0.008087474007913679139, 0.008822698917724009979, 0.009557923827534337349, 0.01029314873734466819, 0.01176359855696528650, 0.01249882346677559479, 0.01323404837658590308, 0.01470449819620656823, 0.01543972310601690427, 0.01617494801582724032, 0.01764539783544789159, 0.01911584765506854633, 0.01985107256487888411, 0.02058629747468921842, 0.02205674729430988704, 0.02352719711393055566 ),
 .UNSPECIFIED. ) ;
#32559 = CARTESIAN_POINT ( 'NONE',  ( 311.8713128290285113, 188.0000000000000000, 346.5826552340383842 ) ) ;
#32560 = B_SPLINE_CURVE_WITH_KNOTS ( 'NONE', 3,
 ( #37902, #7289, #22763, #54053, #59683, #1311, #43511, #22069, #16783, #28385, #17120, #32972, #60401, #12564, #5877, #59349, #65690, #17479, #49127, #50196, #38958, #54405, #12216, #44572, #33684, #28744, #27336, #38597, #21716, #55113, #43162, #64637, #16450, #11160, #48774, #6935, #49832, #6230, #17842, #32626, #612, #968, #22417, #43856, #65332, #60039 ),
 .UNSPECIFIED., .F., .F.,
 ( 4, 2, 2, 2, 2, 2, 2, 2, 2, 2, 2, 2, 2, 2, 2, 2, 2, 2, 2, 2, 2, 2, 4 ),
 ( 1.387778780781445676E-17, 0.003635178948345826107, 0.005452768422518705117, 0.007270357896691583693, 0.008179152633778011272, 0.009087947370864437116, 0.01090553684503733911, 0.01181433158212381353, 0.01272312631921028968, 0.01363192105629676409, 0.01454071579338324025, 0.01544951053046971640, 0.01635830526755619255, 0.01726710000464266523, 0.01817589474172914138, 0.01908468947881561753, 0.01999348421590209368, 0.02090227895298856983, 0.02181107369007504251, 0.02362866316424793584, 0.02544625263842082569, 0.02726384211259371554, 0.02908143158676660886 ),
 .UNSPECIFIED. ) ;
#32561 = ORIENTED_EDGE ( 'NONE', *, *, #54469, .F. ) ;
#32562 = ORIENTED_EDGE ( 'NONE', *, *, #44830, .F. ) ;
#32563 = CARTESIAN_POINT ( 'NONE',  ( 149.0250918491436494, 6.000000000000000000, -46.68900338898718161 ) ) ;
#32564 = PLANE ( 'NONE',  #19036 ) ;
#32565 = EDGE_CURVE ( 'NONE', #1235, #53714, #45887, .T. ) ;
#32566 = CARTESIAN_POINT ( 'NONE',  ( -142.8556048422594813, 60.01994222009839319, -38.83800050151604921 ) ) ;
#32567 = CARTESIAN_POINT ( 'NONE',  ( -167.6566265204789943, 82.70140535081095834, -63.91361994493567522 ) ) ;
#32569 = ORIENTED_EDGE ( 'NONE', *, *, #59368, .F. ) ;
#32568 = CARTESIAN_POINT ( 'NONE',  ( -143.7151964745329451, 59.41799441280377891, -47.08409988814416636 ) ) ;
#32570 = CYLINDRICAL_SURFACE ( 'NONE', #504, 7.500000000000013323 ) ;
#32571 = AXIS2_PLACEMENT_3D ( 'NONE', #23701, #18418, #49362 ) ;
#32572 = EDGE_CURVE ( 'NONE', #41662, #45190, #2986, .T. ) ;
#32573 = EDGE_CURVE ( 'NONE', #26680, #65664, #62595, .T. ) ;
#32574 = EDGE_LOOP ( 'NONE', ( #48315, #46174, #11789, #26580 ) ) ;
#32575 = CARTESIAN_POINT ( 'NONE',  ( -142.1381007084227122, 58.17237452544241449, 63.64461756446542040 ) ) ;
#32576 = CARTESIAN_POINT ( 'NONE',  ( 123.4242852856285566, 6.000000000000000000, -20.00000000000000000 ) ) ;
#32577 = CARTESIAN_POINT ( 'NONE',  ( -44.26023579658939866, 48.10138582123772721, 43.58025477438756212 ) ) ;
#32578 = CARTESIAN_POINT ( 'NONE',  ( 82.34195123877073286, 18.00239921638039675, -10.31852367068890430 ) ) ;
#32579 = CARTESIAN_POINT ( 'NONE',  ( 91.67571176799441446, 21.20498955963029530, -75.71976116502800380 ) ) ;
#32580 = CARTESIAN_POINT ( 'NONE',  ( 203.1511228994173734, 104.2426341584999250, 2.478373221329412068 ) ) ;
#32581 = DIRECTION ( 'NONE',  ( 1.000000000000000000, 0.000000000000000000, 0.000000000000000000 ) ) ;
#32582 = CARTESIAN_POINT ( 'NONE',  ( -96.00016893459645928, 29.70347032303886436, -65.25124674057008178 ) ) ;
#32583 = VERTEX_POINT ( 'NONE', #40602 ) ;
#32584 = ORIENTED_EDGE ( 'NONE', *, *, #25906, .F. ) ;
#32585 = VECTOR ( 'NONE', #43572, 1000.000000000000000 ) ;
#32586 = CARTESIAN_POINT ( 'NONE',  ( 186.2722199822849802, 84.01218714714249813, -65.13350658560696615 ) ) ;
#32587 = CARTESIAN_POINT ( 'NONE',  ( -3.841371665203041630E-11, 0.000000000000000000, 0.000000000000000000 ) ) ;
#32588 = DIRECTION ( 'NONE',  ( -0.000000000000000000, 1.000000000000000000, -0.000000000000000000 ) ) ;
#32589 = CARTESIAN_POINT ( 'NONE',  ( 266.9165763529819628, -2.000000000000001776, 128.9999999999999716 ) ) ;
#32590 = AXIS2_PLACEMENT_3D ( 'NONE', #31191, #19940, #35421 ) ;
#32591 = LINE ( 'NONE', #26279, #42282 ) ;
#32592 = CARTESIAN_POINT ( 'NONE',  ( 81.57482918025355900, 17.75786713398421668, 42.75847996119852468 ) ) ;
#32593 = CARTESIAN_POINT ( 'NONE',  ( 5.722401031430903728, 32.93231310368437903, 6.893343212288939093 ) ) ;
#32594 = CARTESIAN_POINT ( 'NONE',  ( 39.89582146299186860, 9.488756994579082615, -35.61981746542775795 ) ) ;
#32595 = DIRECTION ( 'NONE',  ( -1.850169831522831466E-16, 1.000000000000000000, 1.110223024625156294E-16 ) ) ;
#32596 = EDGE_LOOP ( 'NONE', ( #67958, #61971, #6102, #68427 ) ) ;
#32597 = CARTESIAN_POINT ( 'NONE',  ( -25.48750459758502274, 9.705678256319574260, 6.281801299306986053 ) ) ;
#32598 = EDGE_LOOP ( 'NONE', ( #64789, #23653, #2553, #36459 ) ) ;
#32599 = CARTESIAN_POINT ( 'NONE',  ( -13.47680110791658059, 7.324966777230639714, -47.87354606939886281 ) ) ;
#32600 = CARTESIAN_POINT ( 'NONE',  ( 410.0000000000000000, 0.000000000000000000, 175.2157797990580832 ) ) ;
#32601 = DIRECTION ( 'NONE',  ( -0.000000000000000000, 1.000000000000000000, -0.000000000000000000 ) ) ;
#32602 = B_SPLINE_CURVE_WITH_KNOTS ( 'NONE', 3,
 ( #37530, #10798, #8315, #38940, #34708, #12546, #29761, #50177, #3040, #61427, #35045, #24149, #2346, #34363, #55093, #44899, #61079, #45938, #7274, #55441, #2683, #44554, #55806, #28727, #45591, #67072, #23799, #39284, #66382, #2006, #12904, #60386, #56145, #39624, #34006, #6918 ),
 .UNSPECIFIED., .F., .F.,
 ( 4, 2, 2, 2, 2, 2, 2, 2, 2, 2, 2, 2, 2, 2, 2, 2, 2, 4 ),
 ( 1.734723475976807094E-18, 0.001548367318450188240, 0.003096734636900374746, 0.004645101955350561251, 0.006193469273800747757, 0.007741836592250927324, 0.008516020251476004096, 0.009290203910701080869, 0.01083857122915123268, 0.01238693854760138449, 0.01393530586605153804, 0.01548367318450169158, 0.01703204050295184513, 0.01858040782140199521, 0.02012877513985214528, 0.02167714245830229536, 0.02322550977675244543, 0.02477387709520258857 ),
 .UNSPECIFIED. ) ;
#32603 = CARTESIAN_POINT ( 'NONE',  ( 152.8430172091323129, 54.14068524174420816, -22.68681308951628850 ) ) ;
#32604 = CARTESIAN_POINT ( 'NONE',  ( -51.66904755831212981, -15.55634918610397222, 2.000000000000001776 ) ) ;
#32605 = CARTESIAN_POINT ( 'NONE',  ( -97.86516199987806885, 31.71158167298307617, -75.44090550092165870 ) ) ;
#32606 = VECTOR ( 'NONE', #14267, 1000.000000000000000 ) ;
#32607 = CARTESIAN_POINT ( 'NONE',  ( -17.72433019600386217, 70.00000000000000000, -35.39385180692614341 ) ) ;
#32608 = ORIENTED_EDGE ( 'NONE', *, *, #56294, .F. ) ;
#32609 = CARTESIAN_POINT ( 'NONE',  ( -18.24318075359455804, -17.27206262134411574, 0.000000000000000000 ) ) ;
#32610 = DIRECTION ( 'NONE',  ( 0.6234898018587318180, 0.7818314824680311359, 0.000000000000000000 ) ) ;
#32612 = ORIENTED_EDGE ( 'NONE', *, *, #50686, .T. ) ;
#32611 = EDGE_CURVE ( 'NONE', #23144, #32692, #67016, .T. ) ;
#32613 = CARTESIAN_POINT ( 'NONE',  ( 56.29445224195349340, 12.24017809212663010, 60.79306025269804792 ) ) ;
#32614 = LINE ( 'NONE', #53706, #10587 ) ;
#32615 = CARTESIAN_POINT ( 'NONE',  ( -27.48703802937315288, 8.975952825337598640, 17.25091243039942057 ) ) ;
#32616 = LINE ( 'NONE', #39887, #41288 ) ;
#32617 = CARTESIAN_POINT ( 'NONE',  ( -0.7174461528505738928, 6.532311451815524528, 40.02128953067827410 ) ) ;
#32618 = CARTESIAN_POINT ( 'NONE',  ( -105.4556185321791162, 34.42302275449792859, -62.54804870380231563 ) ) ;
#32619 = CARTESIAN_POINT ( 'NONE',  ( 80.86930862966734423, 18.59011988975001728, 86.08600358295961996 ) ) ;
#32620 = EDGE_CURVE ( 'NONE', #61020, #33777, #62054, .T. ) ;
#32621 = ORIENTED_EDGE ( 'NONE', *, *, #64468, .F. ) ;
#32622 = CARTESIAN_POINT ( 'NONE',  ( 606.3996493186646148, 920.9591914119063176, 498.3734933915376928 ) ) ;
#32623 = CIRCLE ( 'NONE', #34900, 74.95140232871122521 ) ;
#32624 = DIRECTION ( 'NONE',  ( 0.000000000000000000, 0.000000000000000000, 1.000000000000000000 ) ) ;
#32625 = CARTESIAN_POINT ( 'NONE',  ( -126.3508039230932809, 46.79479538767115798, 18.77539728269342234 ) ) ;
#32626 = CARTESIAN_POINT ( 'NONE',  ( -169.8885678771098071, 85.07765565657317097, -48.99404913829265951 ) ) ;
#32627 = CONTEXT_DEPENDENT_SHAPE_REPRESENTATION ( #52114, #6903 ) ;
#32628 = CARTESIAN_POINT ( 'NONE',  ( -130.1938957973835329, 50.61368074696266461, -48.57623976542650013 ) ) ;
#32629 = ORIENTED_EDGE ( 'NONE', *, *, #67944, .F. ) ;
#32630 = LINE ( 'NONE', #53372, #40276 ) ;
#32631 = CARTESIAN_POINT ( 'NONE',  ( -3.857727530059801513, 6.665032499723450243, -9.704207997736320479 ) ) ;
#32632 = EDGE_CURVE ( 'NONE', #19572, #53112, #54924, .T. ) ;
#32633 = CARTESIAN_POINT ( 'NONE',  ( -156.7916867929804994, 70.61267366697164505, 93.72828952245049550 ) ) ;
#32634 = EDGE_CURVE ( 'NONE', #56777, #55170, #4422, .T. ) ;
#32635 = CARTESIAN_POINT ( 'NONE',  ( 51.39999999999999858, 0.000000000000000000, 0.000000000000000000 ) ) ;
#32636 = EDGE_CURVE ( 'NONE', #18983, #22088, #20140, .T. ) ;
#32637 = ORIENTED_EDGE ( 'NONE', *, *, #21731, .F. ) ;
#32638 = DIRECTION ( 'NONE',  ( -0.000000000000000000, -0.000000000000000000, 1.000000000000000000 ) ) ;
#32639 = CARTESIAN_POINT ( 'NONE',  ( 82.14396250120408638, 18.99560174459422157, 4.351623306195690155 ) ) ;
#32640 = LINE ( 'NONE', #47088, #15044 ) ;
#32641 = ORIENTED_EDGE ( 'NONE', *, *, #27390, .T. ) ;
#32642 = CARTESIAN_POINT ( 'NONE',  ( 174.6242782760050147, 73.69713439533578025, 67.47305218060527920 ) ) ;
#32643 = ORIENTED_EDGE ( 'NONE', *, *, #52935, .T. ) ;
#32644 = ORIENTED_EDGE ( 'NONE', *, *, #26747, .T. ) ;
#32645 = CARTESIAN_POINT ( 'NONE',  ( 179.0091171455096912, 77.94933395983139235, 29.58847966245846095 ) ) ;
#32646 = FACE_OUTER_BOUND ( 'NONE', #5049, .T. ) ;
#32648 = ORIENTED_EDGE ( 'NONE', *, *, #56944, .F. ) ;
#32647 = FACE_OUTER_BOUND ( 'NONE', #20139, .T. ) ;
#32649 = CARTESIAN_POINT ( 'NONE',  ( 163.7464701930790341, 62.69993100427431898, 32.77245788678815330 ) ) ;
#32650 = VECTOR ( 'NONE', #60632, 1000.000000000000114 ) ;
#32651 = CARTESIAN_POINT ( 'NONE',  ( 8.000000000000007105, 249.8719672152120381, 94.99999999999866418 ) ) ;
#32652 = ADVANCED_FACE ( 'NONE', ( #61023 ), #8610, .F. ) ;
#32653 = EDGE_CURVE ( 'NONE', #18376, #15244, #45950, .T. ) ;
#32654 = CARTESIAN_POINT ( 'NONE',  ( -62.31345272479909880, 18.49415068377641447, 40.00000000000003553 ) ) ;
#32655 = PRODUCT_DEFINITION_SHAPE ( 'NONE', 'NONE',  #69627 ) ;
#32656 = EDGE_LOOP ( 'NONE', ( #53943, #66107, #17669, #28021 ) ) ;
#32657 =( GEOMETRIC_REPRESENTATION_CONTEXT ( 3 ) GLOBAL_UNCERTAINTY_ASSIGNED_CONTEXT ( ( #52169 ) ) GLOBAL_UNIT_ASSIGNED_CONTEXT ( ( #7025, #40080, #61536 ) ) REPRESENTATION_CONTEXT ( 'NONE', 'WORKASPACE' ) );
#32658 = EDGE_CURVE ( 'NONE', #44889, #32499, #58842, .T. ) ;
#32659 = CARTESIAN_POINT ( 'NONE',  ( -144.7329995847092050, 61.52689957297653223, -90.21374520017691623 ) ) ;
#32660 = CIRCLE ( 'NONE', #46166, 0.3000000000000051514 ) ;
#32661 = CARTESIAN_POINT ( 'NONE',  ( -33.13098007862451055, 9.875138601866705557, -8.661938437730437812 ) ) ;
#32662 = CARTESIAN_POINT ( 'NONE',  ( -178.5750994113944898, 94.98114813978521909, 33.14926202597649763 ) ) ;
#32663 = CARTESIAN_POINT ( 'NONE',  ( 132.2818448028687328, 41.65267246304671289, 56.51853981166434693 ) ) ;
#32664 = VERTEX_POINT ( 'NONE', #52200 ) ;
#32665 = VERTEX_POINT ( 'NONE', #10313 ) ;
#32666 = ORIENTED_EDGE ( 'NONE', *, *, #5325, .T. ) ;
#32667 = AXIS2_PLACEMENT_3D ( 'NONE', #3778, #25250, #45659 ) ;
#32668 = CARTESIAN_POINT ( 'NONE',  ( 209.9999999999999716, 190.0000000000000000, 72.99999999999998579 ) ) ;
#32669 = CARTESIAN_POINT ( 'NONE',  ( -48.07236379518559488, 12.92027279314125288, 88.68666546384376659 ) ) ;
#32670 = CARTESIAN_POINT ( 'NONE',  ( -64.61430802170484355, -7.070445451048284369, 170.0000000000000000 ) ) ;
#32671 = CARTESIAN_POINT ( 'NONE',  ( -154.7998111145352880, 68.80117179139331540, -74.49316838609406943 ) ) ;
#32672 = CARTESIAN_POINT ( 'NONE',  ( 70.39075050212761653, 14.50499482275434460, 92.52271767195246355 ) ) ;
#32673 = DIRECTION ( 'NONE',  ( 0.3513748240813435175, -0.9362348706397369824, 5.102127870520019688E-18 ) ) ;
#32674 = LINE ( 'NONE', #16144, #11448 ) ;
#32675 = CARTESIAN_POINT ( 'NONE',  ( 43.10136267511096264, 39.31639556316177675, 27.58472369426656812 ) ) ;
#32676 = VERTEX_POINT ( 'NONE', #47589 ) ;
#32677 = DIRECTION ( 'NONE',  ( -1.850371928290090422E-16, 1.000000000000000000, 1.110223024625156171E-16 ) ) ;
#32678 = ORIENTED_EDGE ( 'NONE', *, *, #1920, .F. ) ;
#32679 = DIRECTION ( 'NONE',  ( 1.000000000000000000, 0.000000000000000000, -0.000000000000000000 ) ) ;
#32680 = CARTESIAN_POINT ( 'NONE',  ( 183.1865184929770294, 80.75677158533821398, 29.60613287127756621 ) ) ;
#32681 = DIRECTION ( 'NONE',  ( 1.000000000000000000, 0.000000000000000000, 0.000000000000000000 ) ) ;
#32682 = CARTESIAN_POINT ( 'NONE',  ( -71.59086462055192612, 19.75139532313339785, 8.573663426099198404 ) ) ;
#32683 = DIRECTION ( 'NONE',  ( -1.000000000000000000, 0.000000000000000000, 0.000000000000000000 ) ) ;
#32684 = CARTESIAN_POINT ( 'NONE',  ( 0.000000000000000000, 26.99999999999999645, 15.00000000000000000 ) ) ;
#32685 = CARTESIAN_POINT ( 'NONE',  ( 200.7308788951040697, 101.0577854064628980, 84.00080373449807780 ) ) ;
#32686 = CARTESIAN_POINT ( 'NONE',  ( 150.0501577908836737, 52.10460126680130344, -42.49831103806872079 ) ) ;
#32687 = DIRECTION ( 'NONE',  ( -1.000000000000000000, 0.000000000000000000, -0.000000000000000000 ) ) ;
#32688 = VERTEX_POINT ( 'NONE', #58492 ) ;
#32689 = CARTESIAN_POINT ( 'NONE',  ( 0.000000000000000000, 0.000000000000000000, 0.000000000000000000 ) ) ;
#32690 = CARTESIAN_POINT ( 'NONE',  ( 311.9732115134679020, 188.0000000000000000, -151.4173343409194672 ) ) ;
#32691 = ORIENTED_EDGE ( 'NONE', *, *, #12817, .T. ) ;
#32692 = VERTEX_POINT ( 'NONE', #57480 ) ;
#32693 = CARTESIAN_POINT ( 'NONE',  ( -86.06016868996613312, 25.27707703029501474, 39.20171598925913514 ) ) ;
#32694 = CARTESIAN_POINT ( 'NONE',  ( 156.5993887774280324, 58.24868799840905353, -77.92120936136656439 ) ) ;
#32695 = DIRECTION ( 'NONE',  ( -0.000000000000000000, -0.000000000000000000, -1.000000000000000000 ) ) ;
#32696 = CARTESIAN_POINT ( 'NONE',  ( -23.95096213915836714, 8.481591526885939203, 65.04975062497030081 ) ) ;
#32697 = EDGE_CURVE ( 'NONE', #40620, #24801, #13421, .T. ) ;
#32698 = PLANE ( 'NONE',  #46558 ) ;
#32699 = B_SPLINE_CURVE_WITH_KNOTS ( 'NONE', 3,
 ( #59615, #32556, #69487, #64568, #21305, #42754, #5811, #64213, #16026, #64919, #16377, #10748, #53649, #27265, #54338, #39235, #23054, #28677, #59970, #38524 ),
 .UNSPECIFIED., .F., .F.,
 ( 4, 2, 2, 2, 2, 2, 2, 2, 2, 4 ),
 ( 0.01005966960094808842, 0.01130938760903082291, 0.01255910561711355913, 0.01380882362519629536, 0.01505854163327902985, 0.01568340063732039796, 0.01630825964136176781, 0.01755797764944450404, 0.01880769565752724026, 0.02005741366560997996 ),
 .UNSPECIFIED. ) ;
#32700 = ORIENTED_EDGE ( 'NONE', *, *, #61307, .F. ) ;
#32701 = VECTOR ( 'NONE', #45076, 1000.000000000000000 ) ;
#32702 = ORIENTED_EDGE ( 'NONE', *, *, #69229, .T. ) ;
#32703 = CARTESIAN_POINT ( 'NONE',  ( 3.000000000000006217, 0.000000000000000000, -23.50000000000000000 ) ) ;
#32704 = ORIENTED_EDGE ( 'NONE', *, *, #55766, .T. ) ;
#32705 = CARTESIAN_POINT ( 'NONE',  ( 36.77024545412684375, 9.095083943590502429, -23.30259963730480877 ) ) ;
#32706 = CARTESIAN_POINT ( 'NONE',  ( 29.69502258243350923, 57.82046033912877903, 73.58025477438755502 ) ) ;
#32707 = AXIS2_PLACEMENT_3D ( 'NONE', #21550, #63443, #16283 ) ;
#32708 = CARTESIAN_POINT ( 'NONE',  ( 56.66775172211443135, 11.28938863449063135, 68.15943088655339466 ) ) ;
#32709 = CARTESIAN_POINT ( 'NONE',  ( 137.7927399796681414, 45.04243838361963270, 84.30735228466484443 ) ) ;
#32710 = EDGE_CURVE ( 'NONE', #10586, #54090, #59192, .T. ) ;
#32711 = PRODUCT_DEFINITION_SHAPE ( 'NONE', 'NONE',  #13877 ) ;
#32712 = CARTESIAN_POINT ( 'NONE',  ( -31.11269837220812207, -31.11269837220801193, 0.000000000000000000 ) ) ;
#32713 = VECTOR ( 'NONE', #38263, 1000.000000000000000 ) ;
#32715 = STYLED_ITEM ( 'NONE', ( #5689 ), #17567 ) ;
#32714 = CARTESIAN_POINT ( 'NONE',  ( 0.000000000000000000, 0.000000000000000000, 0.000000000000000000 ) ) ;
#32716 = EDGE_CURVE ( 'NONE', #51453, #22434, #36368, .T. ) ;
#32717 = DIRECTION ( 'NONE',  ( 1.000000000000000000, -2.220446049250313081E-14, 0.000000000000000000 ) ) ;
#32718 = VERTEX_POINT ( 'NONE', #69409 ) ;
#32719 = ADVANCED_FACE ( 'NONE', ( #52869 ), #15605, .F. ) ;
#32720 = VERTEX_POINT ( 'NONE', #9642 ) ;
#32721 = CARTESIAN_POINT ( 'NONE',  ( 24.34685647902980676, 70.88683439560453792, 41.38025477438755928 ) ) ;
#32722 = FACE_OUTER_BOUND ( 'NONE', #10018, .T. ) ;
#32723 = PLANE ( 'NONE',  #55498 ) ;
#32724 = CARTESIAN_POINT ( 'NONE',  ( 136.9798231265810102, 43.34196232604179500, -77.20246944962947566 ) ) ;
#32725 = CARTESIAN_POINT ( 'NONE',  ( 69.50572373348801136, 14.27208627753790893, 41.10388884447479541 ) ) ;
#32726 = COLOUR_RGB ( '',0.7921568627450980005, 0.8196078431372548767, 0.9333333333333333481 ) ;
#32727 = ORIENTED_EDGE ( 'NONE', *, *, #7254, .T. ) ;
#32728 = CARTESIAN_POINT ( 'NONE',  ( 84.97343609940683962, 18.86260005312943022, 17.68632826205469399 ) ) ;
#32729 = VERTEX_POINT ( 'NONE', #53210 ) ;
#32730 = CARTESIAN_POINT ( 'NONE',  ( -76.10397364431021572, 21.36211154336729834, 30.86549673594327814 ) ) ;
#32731 = ORIENTED_EDGE ( 'NONE', *, *, #39463, .T. ) ;
#32732 = ORIENTED_EDGE ( 'NONE', *, *, #58048, .F. ) ;
#32733 = DIRECTION ( 'NONE',  ( 0.000000000000000000, 0.000000000000000000, 1.000000000000000000 ) ) ;
#32734 = CARTESIAN_POINT ( 'NONE',  ( 3.904274462092029996, 38.13465922106460226, 13.32819299319724138 ) ) ;
#32735 = CARTESIAN_POINT ( 'NONE',  ( -447.6627218934913230, 392.9289321881344108, 108.5502958579880328 ) ) ;
#32736 = ORIENTED_EDGE ( 'NONE', *, *, #50252, .T. ) ;
#32737 = EDGE_CURVE ( 'NONE', #34992, #3775, #32483, .T. ) ;
#32738 = CARTESIAN_POINT ( 'NONE',  ( -65.36598343705435354, 0.000000000000000000, 41.38025477438755928 ) ) ;
#32739 = DIRECTION ( 'NONE',  ( -0.9009688679024218105, 0.4338837391175525693, 0.000000000000000000 ) ) ;
#32740 = CARTESIAN_POINT ( 'NONE',  ( 151.1607415860635513, 52.90668588398090577, 32.82304110344981041 ) ) ;
#32741 = CARTESIAN_POINT ( 'NONE',  ( -174.7903139851460139, 90.53182997092835649, -34.88798999700193804 ) ) ;
#32742 = CARTESIAN_POINT ( 'NONE',  ( -39.29440389294403246, 17.09499999999999886, 4.000000000000000000 ) ) ;
#32743 = CARTESIAN_POINT ( 'NONE',  ( 70.60157554497493493, -25.16207943727098950, 41.38025477438755928 ) ) ;
#32744 = PLANE ( 'NONE',  #13633 ) ;
#32745 = EDGE_LOOP ( 'NONE', ( #68187, #42519, #39396, #26358 ) ) ;
#32746 = CARTESIAN_POINT ( 'NONE',  ( 136.1037846510193390, 43.98155406734453265, -63.19752277197763846 ) ) ;
#32747 = CARTESIAN_POINT ( 'NONE',  ( -45.00000000000002132, -20.00000000000000355, 4.000000000000000000 ) ) ;
#32748 = VERTEX_POINT ( 'NONE', #15943 ) ;
#32749 = VECTOR ( 'NONE', #60229, 999.9999999999998863 ) ;
#32750 = FACE_BOUND ( 'NONE', #11387, .T. ) ;
#32751 = FACE_OUTER_BOUND ( 'NONE', #20951, .T. ) ;
#32752 = CARTESIAN_POINT ( 'NONE',  ( -1.683356153842356262, -65.34430428700412108, 41.38025477438755928 ) ) ;
#32753 = CARTESIAN_POINT ( 'NONE',  ( 0.000000000000000000, 0.000000000000000000, 0.000000000000000000 ) ) ;
#32754 = CARTESIAN_POINT ( 'NONE',  ( -83.53167274806556009, 25.32068190668984187, 16.80234616661474334 ) ) ;
#32755 = LINE ( 'NONE', #16572, #25845 ) ;
#32756 = B_SPLINE_CURVE_WITH_KNOTS ( 'NONE', 3,
 ( #39620, #45586, #61073, #67067, #12541, #66029, #18862, #54741, #40310, #22744, #7625, #23456, #44179, #65668, #55801, #6912, #1636, #34001, #44894, #38934, #44548, #60382, #17822, #55437, #66376, #40649, #14953, #51898, #47298, #35737, #29757, #41356, #3374, #41693, #46971, #46269, #57874, #62808, #19190, #57187, #9002, #36417, #13921, #31155, #36073, #19544, #67746 ),
 .UNSPECIFIED., .F., .F.,
 ( 4, 2, 2, 2, 2, 2, 2, 2, 2, 2, 2, 2, 1, 2, 2, 2, 2, 2, 2, 2, 2, 2, 2, 4 ),
 ( 0.000000000000000000, 0.001520400357568927252, 0.002280600536353409851, 0.003040800715137892234, 0.004561201072706856999, 0.005321401251491323335, 0.006081601430275789671, 0.007602001787844721477, 0.008362201966629198222, 0.009122402145413675834, 0.01064280250298263106, 0.01140300268176712775, 0.01216320286055162618, 0.01292340303933612461, 0.01368360321812062477, 0.01520400357568962683, 0.01596420375447412179, 0.01672440393325861502, 0.01824480429082758065, 0.01976520464839655322, 0.02052540482718103604, 0.02128560500596551885, 0.02280600536353448102, 0.02432640572110344665 ),
 .UNSPECIFIED. ) ;
#32757 = CARTESIAN_POINT ( 'NONE',  ( -150.3791492925491298, 64.92185203933371440, 3.914254989767345094 ) ) ;
#32758 = CARTESIAN_POINT ( 'NONE',  ( -120.6420427933462349, 44.31795133507807094, -74.61821363998994627 ) ) ;
#32760 = DIRECTION ( 'NONE',  ( 1.000000000000000000, 0.000000000000000000, 0.000000000000000000 ) ) ;
#32759 = AXIS2_PLACEMENT_3D ( 'NONE', #26779, #53491, #43630 ) ;
#32761 = AXIS2_PLACEMENT_3D ( 'NONE', #37285, #16182, #59431 ) ;
#32762 = CARTESIAN_POINT ( 'NONE',  ( 159.6725804802005655, 59.38339663535510482, 17.24836648525045035 ) ) ;
#32763 = CARTESIAN_POINT ( 'NONE',  ( 94.02499804464933675, 23.15433260743126453, -15.20501225471814877 ) ) ;
#32764 = ORIENTED_EDGE ( 'NONE', *, *, #15715, .T. ) ;
#32765 = CARTESIAN_POINT ( 'NONE',  ( -36.89224332184166855, 11.57404295377975600, 5.717042333022100742 ) ) ;
#32766 = VERTEX_POINT ( 'NONE', #4695 ) ;
#32767 = FACE_OUTER_BOUND ( 'NONE', #50606, .T. ) ;
#32768 = CARTESIAN_POINT ( 'NONE',  ( 83.38619203015947789, 19.39783821526630803, -76.94561659048915203 ) ) ;
#32769 = CARTESIAN_POINT ( 'NONE',  ( 117.3315207373142215, 33.42838861910006898, 88.32577119086282380 ) ) ;
#32770 = CARTESIAN_POINT ( 'NONE',  ( 26.12852347772543737, 70.00000000000000000, 77.58025477438755502 ) ) ;
#32771 = CARTESIAN_POINT ( 'NONE',  ( -9.964117946889912147, 64.24592483216710548, 170.0000000000000000 ) ) ;
#32772 = AXIS2_PLACEMENT_3D ( 'NONE', #4236, #19716, #25700 ) ;
#32773 = CARTESIAN_POINT ( 'NONE',  ( -26.49928411671542960, 9.848831533840670005, -37.15254042537868173 ) ) ;
#32774 = CARTESIAN_POINT ( 'NONE',  ( -48.34500911884041585, 14.01939034823941732, -66.19665500006401260 ) ) ;
#32775 = B_SPLINE_CURVE_WITH_KNOTS ( 'NONE', 3,
 ( #52924, #36423, #62817, #4750, #47304, #36083, #4413, #20932, #15659, #24835, #57540, #20580, #41700, #19908, #3715, #26213, #58549, #41364, #68435, #31833, #10367, #52254, #51906, #46276, #25878, #63165, #9342, #47653, #14284, #57879, #67753, #63851, #19553, #4076, #31163, #62467, #35743, #68765, #42042, #9013, #69107, #30455, #25540 ),
 .UNSPECIFIED., .F., .F.,
 ( 4, 2, 2, 2, 2, 2, 2, 2, 1, 2, 2, 2, 2, 2, 2, 2, 2, 2, 2, 2, 2, 4 ),
 ( 0.000000000000000000, 0.001465684626643344503, 0.002198526939965016972, 0.002931369253286689007, 0.004397053879930033944, 0.005862738506573378014, 0.007328423133216722084, 0.008061265446538396287, 0.008794107759860073092, 0.009526950073181746428, 0.01025979238650342150, 0.01172547701314677338, 0.01319116163979012525, 0.01465684626643347713, 0.01538968857975514873, 0.01612253089307682033, 0.01758821551972016353, 0.01905390014636350327, 0.01978674245968517140, 0.02051958477300683953, 0.02198526939965017579, 0.02345095402629350512 ),
 .UNSPECIFIED. ) ;
#32776 = FACE_OUTER_BOUND ( 'NONE', #34262, .T. ) ;
#32777 = CARTESIAN_POINT ( 'NONE',  ( 104.0290905220488469, 26.11184870228230892, 94.99999999999866418 ) ) ;
#32778 = ORIENTED_EDGE ( 'NONE', *, *, #23667, .F. ) ;
#32779 = VERTEX_POINT ( 'NONE', #14902 ) ;
#32780 = ADVANCED_FACE ( 'NONE', ( #64128 ), #19848, .T. ) ;
#32781 = CARTESIAN_POINT ( 'NONE',  ( 34.83823433017387572, 8.871835168107974567, 58.28624973792864239 ) ) ;
#32782 = CARTESIAN_POINT ( 'NONE',  ( -171.4943428135322847, 86.82484920477511992, 72.53627115242575485 ) ) ;
#32783 = EDGE_CURVE ( 'NONE', #37085, #19763, #37388, .T. ) ;
#32784 = CARTESIAN_POINT ( 'NONE',  ( -168.0003605155415016, 83.06333427281268200, -20.85263118173764951 ) ) ;
#32785 = DIRECTION ( 'NONE',  ( -0.000000000000000000, -0.000000000000000000, -1.000000000000000000 ) ) ;
#32786 = ORIENTED_EDGE ( 'NONE', *, *, #68683, .T. ) ;
#32787 = DIRECTION ( 'NONE',  ( -0.5323601107705935309, 0.8465179929926602842, 0.000000000000000000 ) ) ;
#32788 = CARTESIAN_POINT ( 'NONE',  ( 187.5165082312810227, 86.85340440641657267, -20.74607734399896231 ) ) ;
#32789 = PLANE ( 'NONE',  #1223 ) ;
#32790 =( NAMED_UNIT ( * ) SI_UNIT ( $, .STERADIAN. ) SOLID_ANGLE_UNIT ( ) );
#32791 = CARTESIAN_POINT ( 'NONE',  ( -78.66644367742109978, 23.39876645725289706, -88.80455181264524356 ) ) ;
#32792 = CARTESIAN_POINT ( 'NONE',  ( 46.70715146412976537, 9.472433765546997009, -17.99120794428602821 ) ) ;
#32793 = CARTESIAN_POINT ( 'NONE',  ( 210.4897348480408255, 114.6382060222044714, -21.75249441828651698 ) ) ;
#32794 = CYLINDRICAL_SURFACE ( 'NONE', #54228, 7.500000000000020428 ) ;
#32795 = CARTESIAN_POINT ( 'NONE',  ( 160.9099843287284841, 61.67000084894968381, 57.07340599545204185 ) ) ;
#32797 = ADVANCED_FACE ( 'NONE', ( #20186 ), #63100, .F. ) ;
#32796 =( REPRESENTATION_RELATIONSHIP ('NONE','NONE', #40274, #64096 ) REPRESENTATION_RELATIONSHIP_WITH_TRANSFORMATION ( #62128 )SHAPE_REPRESENTATION_RELATIONSHIP( ) );
#32798 = EDGE_LOOP ( 'NONE', ( #11210, #1875 ) ) ;
#32799 = EDGE_CURVE ( 'NONE', #8782, #30746, #12250, .T. ) ;
#32800 = CARTESIAN_POINT ( 'NONE',  ( -26.00000000000000000, 0.000000000000000000, -2.818925648462311923E-15 ) ) ;
#32801 = CARTESIAN_POINT ( 'NONE',  ( -31.43908319763709969, 9.591432048623765638, 57.06100499665286208 ) ) ;
#32802 = AXIS2_PLACEMENT_3D ( 'NONE', #60840, #65789, #49576 ) ;
#32803 = CARTESIAN_POINT ( 'NONE',  ( -51.34562532494749831, 14.75613283840035983, 71.19973610574378142 ) ) ;
#32804 = CARTESIAN_POINT ( 'NONE',  ( -20.55634918610400419, 20.55634918610405748, 85.00100000000000477 ) ) ;
#32805 = CARTESIAN_POINT ( 'NONE',  ( -21.95369412746239846, -11.95973721106846455, 0.000000000000000000 ) ) ;
#32806 = CARTESIAN_POINT ( 'NONE',  ( -15.23124449227264066, 8.497728762338836006, 89.95007870748302992 ) ) ;
#32807 = ORIENTED_EDGE ( 'NONE', *, *, #20089, .F. ) ;
#32808 = CARTESIAN_POINT ( 'NONE',  ( 59.72897338775215559, 11.93428797217974591, 3.722467926232761126 ) ) ;
#32809 = CARTESIAN_POINT ( 'NONE',  ( -56.97107423601134712, 15.20373812575556194, 57.39529982396223318 ) ) ;
#32810 = ORIENTED_EDGE ( 'NONE', *, *, #38176, .T. ) ;
#32811 = VECTOR ( 'NONE', #38292, 1000.000000000000000 ) ;
#32812 = ORIENTED_EDGE ( 'NONE', *, *, #50303, .T. ) ;
#32813 = DIRECTION ( 'NONE',  ( -0.000000000000000000, -0.000000000000000000, 1.000000000000000000 ) ) ;
#32814 = LINE ( 'NONE', #6065, #1839 ) ;
#32815 = CARTESIAN_POINT ( 'NONE',  ( 104.7034219878852213, 26.40210929103715998, 32.03102971527638232 ) ) ;
#32816 = EDGE_LOOP ( 'NONE', ( #27018, #55823 ) ) ;
#32817 = AXIS2_PLACEMENT_3D ( 'NONE', #6260, #645, #38624 ) ;
#32818 = CARTESIAN_POINT ( 'NONE',  ( 0.7145311798161619876, -4.618802153517266085, -8.000000000000000000 ) ) ;
#32819 = VECTOR ( 'NONE', #67524, 1000.000000000000000 ) ;
#32820 = CARTESIAN_POINT ( 'NONE',  ( 86.62931800182293784, -170.0000000000000000, -16.47701360844803986 ) ) ;
#32821 = CARTESIAN_POINT ( 'NONE',  ( 31.11269837220800127, -31.11269837220812562, 85.00100000000000477 ) ) ;
#32822 = CARTESIAN_POINT ( 'NONE',  ( -35.00000000000002842, -35.00000000000000000, -2.000000000000000000 ) ) ;
#32823 = DIRECTION ( 'NONE',  ( -1.000000000000000000, 0.000000000000000000, 0.000000000000000000 ) ) ;
#32824 = CARTESIAN_POINT ( 'NONE',  ( -4.999999999999971578, 15.55634918610403084, 2.000000000000000000 ) ) ;
#32825 = CARTESIAN_POINT ( 'NONE',  ( -51.13576748034041231, 14.70354244225167584, -49.11681489039352044 ) ) ;
#32826 = CYLINDRICAL_SURFACE ( 'NONE', #6679, 5.000000000000000888 ) ;
#32827 = CARTESIAN_POINT ( 'NONE',  ( 13.37708032728285623, 7.441924986912762385, 30.40862419550404994 ) ) ;
#32828 = DIRECTION ( 'NONE',  ( -0.9639628606958550172, 0.2660368455666687892, 0.000000000000000000 ) ) ;
#32829 = CARTESIAN_POINT ( 'NONE',  ( 79.29307999139646768, 17.04697453199588963, 92.49707517143880864 ) ) ;
#32831 = EDGE_LOOP ( 'NONE', ( #10882, #3573, #7016, #36322 ) ) ;
#32830 = DIRECTION ( 'NONE',  ( 1.000000000000000000, 0.000000000000000000, 0.000000000000000000 ) ) ;
#32832 = ORIENTED_EDGE ( 'NONE', *, *, #18750, .F. ) ;
#32833 = ORIENTED_EDGE ( 'NONE', *, *, #6822, .F. ) ;
#32834 = CARTESIAN_POINT ( 'NONE',  ( -15.32550079334879278, 7.496023944924841587, -16.31543665609040872 ) ) ;
#32835 = CYLINDRICAL_SURFACE ( 'NONE', #42800, 7.500000000000013323 ) ;
#32836 = CARTESIAN_POINT ( 'NONE',  ( -53.14475157111026249, 14.17819596930906556, -23.12906344254722413 ) ) ;
#32837 = DIRECTION ( 'NONE',  ( -0.000000000000000000, -0.000000000000000000, -1.000000000000000000 ) ) ;
#32838 = CARTESIAN_POINT ( 'NONE',  ( -34.52542994698664813, 11.14027065218089518, 71.40085072621459972 ) ) ;
#32839 = LINE ( 'NONE', #5417, #23078 ) ;
#32840 = CARTESIAN_POINT ( 'NONE',  ( 150.9184679586219886, 52.73111408630724384, -66.80947418898379908 ) ) ;
#32841 = CARTESIAN_POINT ( 'NONE',  ( 23.28869764673362042, 6.856674305776599532, -15.68603375068130390 ) ) ;
#32842 = ORIENTED_EDGE ( 'NONE', *, *, #26599, .T. ) ;
#32843 = DIRECTION ( 'NONE',  ( 0.9749279121818259508, -0.2225209339563042066, 2.500042656554809847E-16 ) ) ;
#32844 = VERTEX_POINT ( 'NONE', #59528 ) ;
#32845 = ORIENTED_EDGE ( 'NONE', *, *, #36922, .F. ) ;
#32846 = CARTESIAN_POINT ( 'NONE',  ( -17.50000000000002842, 207.5000000000000284, 378.0000000000000000 ) ) ;
#32847 = VECTOR ( 'NONE', #64045, 1000.000000000000000 ) ;
#32848 = CARTESIAN_POINT ( 'NONE',  ( -59.10270545739309966, 16.85145316017989714, -90.07846592657732288 ) ) ;
#32849 = CARTESIAN_POINT ( 'NONE',  ( -24.30908968323081254, 9.544419512845170317, 93.82125383429070098 ) ) ;
#32850 = CARTESIAN_POINT ( 'NONE',  ( 115.0606351894211627, 32.29586232625067765, -22.34698907665701384 ) ) ;
#32851 = EDGE_CURVE ( 'NONE', #35076, #26400, #27180, .T. ) ;
#32852 = AXIS2_PLACEMENT_3D ( 'NONE', #44701, #33799, #7063 ) ;
#32853 = CARTESIAN_POINT ( 'NONE',  ( -108.6634958860518196, 36.14357436892402831, 15.11988995337718933 ) ) ;
#32854 = PLANE ( 'NONE',  #48306 ) ;
#32855 = CARTESIAN_POINT ( 'NONE',  ( 141.0792860804899362, 47.16255757051794006, -18.76987349801746774 ) ) ;
#32856 = ORIENTED_EDGE ( 'NONE', *, *, #9778, .T. ) ;
#32857 = ORIENTED_EDGE ( 'NONE', *, *, #11573, .F. ) ;
#32858 = EDGE_CURVE ( 'NONE', #31501, #34735, #52479, .T. ) ;
#32859 = VERTEX_POINT ( 'NONE', #2549 ) ;
#32860 = CONICAL_SURFACE ( 'NONE', #53034, 65.00000000000000000, 0.7853981633974497223 ) ;
#32861 = CARTESIAN_POINT ( 'NONE',  ( 53.32245423372560111, 37.19594572654715137, 170.0000000000000000 ) ) ;
#32862 = CARTESIAN_POINT ( 'NONE',  ( -156.8728827992624133, 72.05711009495556141, -16.91073671683209056 ) ) ;
#32863 = EDGE_CURVE ( 'NONE', #8346, #51470, #13451, .T. ) ;
#32864 = CARTESIAN_POINT ( 'NONE',  ( 88.59828180051356128, 21.16853032775269838, -89.76271995981053919 ) ) ;
#32865 = EDGE_CURVE ( 'NONE', #49747, #65764, #34217, .T. ) ;
#32866 = VECTOR ( 'NONE', #19945, 1000.000000000000000 ) ;
#32867 = CARTESIAN_POINT ( 'NONE',  ( -35.17686701826945495, 10.23452050416468140, 71.08151450555706674 ) ) ;
#32868 = CARTESIAN_POINT ( 'NONE',  ( -149.5074843970971017, 64.17983161892348676, -22.96827994102829962 ) ) ;
#32869 = ORIENTED_EDGE ( 'NONE', *, *, #4701, .F. ) ;
#32870 = CARTESIAN_POINT ( 'NONE',  ( -35.00000000000002842, -35.00000000000000000, 378.0000000000000000 ) ) ;
#32871 = LINE ( 'NONE', #27586, #7962 ) ;
#32872 = CARTESIAN_POINT ( 'NONE',  ( -6.125624616441583292, 7.794071945221091369, -35.60914887735208367 ) ) ;
#32873 = CARTESIAN_POINT ( 'NONE',  ( 102.8111940033033989, 25.59308899183600872, 11.30835609773350647 ) ) ;
#32874 = FACE_OUTER_BOUND ( 'NONE', #52264, .T. ) ;
#32875 = CARTESIAN_POINT ( 'NONE',  ( -82.32750425780473336, 23.74963782027935011, -36.05213690621574329 ) ) ;
#32876 = CARTESIAN_POINT ( 'NONE',  ( 19.11168290073777598, 6.629794975642855803, 71.08720758981752397 ) ) ;
#32877 = DIRECTION ( 'NONE',  ( 0.000000000000000000, 1.000000000000000000, 0.000000000000000000 ) ) ;
#32878 = CARTESIAN_POINT ( 'NONE',  ( 12.46277766093406569, 6.416700641561363661, -63.12311374513074469 ) ) ;
#32879 = EDGE_CURVE ( 'NONE', #7708, #45932, #29279, .T. ) ;
#32880 = VERTEX_POINT ( 'NONE', #61634 ) ;
#32881 = CARTESIAN_POINT ( 'NONE',  ( -51.66904755831210139, 0.000000000000000000, 2.000000000000000000 ) ) ;
#32882 = PRODUCT_CONTEXT ( 'NONE', #49323, 'mechanical' ) ;
#32883 = CARTESIAN_POINT ( 'NONE',  ( -132.0958200534847435, 50.71531800824805458, -73.48295987508291205 ) ) ;
#32884 = CARTESIAN_POINT ( 'NONE',  ( -132.6161619568759136, 51.08240647571219739, -45.74966482454154715 ) ) ;
#32885 = CARTESIAN_POINT ( 'NONE',  ( 45.49006904354232006, 9.279592366778887325, -74.35131477850875115 ) ) ;
#32886 = DIRECTION ( 'NONE',  ( 0.6234898018587318180, 0.7818314824680311359, 0.000000000000000000 ) ) ;
#32887 = ORIENTED_EDGE ( 'NONE', *, *, #25102, .F. ) ;
#32888 = EDGE_LOOP ( 'NONE', ( #54365, #38536, #3148, #4262 ) ) ;
#32889 = FILL_AREA_STYLE ('',( #23734 ) ) ;
#32890 = DIRECTION ( 'NONE',  ( -0.000000000000000000, -0.000000000000000000, 1.000000000000000000 ) ) ;
#32891 = ORIENTED_EDGE ( 'NONE', *, *, #19929, .F. ) ;
#32892 = EDGE_LOOP ( 'NONE', ( #10007, #58609, #38077, #16098 ) ) ;
#32893 = CARTESIAN_POINT ( 'NONE',  ( 176.0745160362858428, 73.68684431790050837, -38.13833935887404891 ) ) ;
#32894 = CARTESIAN_POINT ( 'NONE',  ( 0.000000000000000000, 70.00000000000000000, 0.000000000000000000 ) ) ;
#32895 = ORIENTED_EDGE ( 'NONE', *, *, #32565, .F. ) ;
#32896 = LINE ( 'NONE', #53295, #14369 ) ;
#32897 = CARTESIAN_POINT ( 'NONE',  ( 139.1306635769909121, 45.89653412152168954, 58.51687394488192950 ) ) ;
#32898 = CARTESIAN_POINT ( 'NONE',  ( -71.37402418445425667, 19.67651958824262337, -44.38599607864244945 ) ) ;
#32899 = VECTOR ( 'NONE', #4993, 1000.000000000000114 ) ;
#32900 = CARTESIAN_POINT ( 'NONE',  ( 164.6046919270428930, 63.41782451559755174, -95.00000000000133582 ) ) ;
#32901 = PLANE ( 'NONE',  #55199 ) ;
#32902 = AXIS2_PLACEMENT_3D ( 'NONE', #41423, #57600, #36488 ) ;
#32903 = CARTESIAN_POINT ( 'NONE',  ( -48.58279704072701577, 14.07632445131079457, -12.07026367287715019 ) ) ;
#32904 = EDGE_LOOP ( 'NONE', ( #31123, #9207, #40171, #54989, #12893, #15963, #28134, #58169, #24724 ) ) ;
#32905 = AXIS2_PLACEMENT_3D ( 'NONE', #38947, #39289, #39629 ) ;
#32906 = CARTESIAN_POINT ( 'NONE',  ( -123.6619986853278306, 45.04188181212062148, -8.405249343855505373 ) ) ;
#32907 = FACE_BOUND ( 'NONE', #22522, .T. ) ;
#32908 = CARTESIAN_POINT ( 'NONE',  ( -143.4048679855200703, 60.45763799613827416, -37.94565703660070000 ) ) ;
#32909 = LINE ( 'NONE', #27632, #33121 ) ;
#32911 = ORIENTED_EDGE ( 'NONE', *, *, #53817, .F. ) ;
#32910 = CARTESIAN_POINT ( 'NONE',  ( -142.0081215801269536, 58.07066293384866640, -42.61264745997317505 ) ) ;
#32912 = CARTESIAN_POINT ( 'NONE',  ( 57.41085175769455873, 12.46982565415947519, 5.478706012108088608 ) ) ;
#32913 = VECTOR ( 'NONE', #65563, 1000.000000000000000 ) ;
#32914 = EDGE_LOOP ( 'NONE', ( #61292, #16173, #41723, #34327 ) ) ;
#32916 = EDGE_CURVE ( 'NONE', #25612, #31482, #67283, .T. ) ;
#32915 = CARTESIAN_POINT ( 'NONE',  ( -128.9925397612933580, 48.56800623462828526, 31.28606989344878642 ) ) ;
#32917 = CARTESIAN_POINT ( 'NONE',  ( 0.000000000000000000, 0.000000000000000000, 0.000000000000000000 ) ) ;
#32918 = DIRECTION ( 'NONE',  ( -1.000000000000000000, 0.000000000000000000, 0.000000000000000000 ) ) ;
#32919 = DIRECTION ( 'NONE',  ( 0.000000000000000000, 0.02271222823333338484, -0.9997420440737084801 ) ) ;
#32920 = CARTESIAN_POINT ( 'NONE',  ( 0.7145311798163349604, -9.237604307034033013, 2.857026868940023748E-16 ) ) ;
#32921 = CARTESIAN_POINT ( 'NONE',  ( 94.11746922806581495, 22.11341285603780449, -69.67410109035120058 ) ) ;
#32922 = CARTESIAN_POINT ( 'NONE',  ( 31.11269837220806522, -6.375108774214766072E-14, 2.000000000000001776 ) ) ;
#32923 = CARTESIAN_POINT ( 'NONE',  ( -95.61819996182569525, 29.52346081122274413, 14.62890838970597329 ) ) ;
#32924 = CARTESIAN_POINT ( 'NONE',  ( -149.5074843970970733, 65.50121172469319220, -34.81283053149196149 ) ) ;
#32925 = ORIENTED_EDGE ( 'NONE', *, *, #10165, .T. ) ;
#32926 = ORIENTED_EDGE ( 'NONE', *, *, #6766, .F. ) ;
#32927 = CARTESIAN_POINT ( 'NONE',  ( 41.35041461497707616, 8.670465437677201237, 44.67304901252469307 ) ) ;
#32928 = CARTESIAN_POINT ( 'NONE',  ( 12.03317402819681625, 6.409531826169460267, 31.01780596777689425 ) ) ;
#32929 = DIRECTION ( 'NONE',  ( 1.000000000000000000, -0.000000000000000000, -0.000000000000000000 ) ) ;
#32930 = DIRECTION ( 'NONE',  ( 0.000000000000000000, 0.000000000000000000, -1.000000000000000000 ) ) ;
#32931 = CARTESIAN_POINT ( 'NONE',  ( 207.4566510040494904, 111.9649643341356580, -50.80316001813071125 ) ) ;
#32932 = DIRECTION ( 'NONE',  ( 0.000000000000000000, 0.000000000000000000, 1.000000000000000000 ) ) ;
#32933 = DIRECTION ( 'NONE',  ( -0.000000000000000000, -0.000000000000000000, 1.000000000000000000 ) ) ;
#32934 = CARTESIAN_POINT ( 'NONE',  ( 43.96062659677685502, 10.06332325923986204, -37.14425628477024333 ) ) ;
#32935 = DIRECTION ( 'NONE',  ( 0.7100673072878298520, 0.7041338076821836989, 0.000000000000000000 ) ) ;
#32936 = ORIENTED_EDGE ( 'NONE', *, *, #15518, .F. ) ;
#32937 = CARTESIAN_POINT ( 'NONE',  ( -102.2801239173131052, 32.78103895658057354, -23.17002667451225406 ) ) ;
#32938 = EDGE_CURVE ( 'NONE', #27607, #50057, #19066, .T. ) ;
#32939 = EDGE_LOOP ( 'NONE', ( #33949, #65244, #13452, #19383, #11432, #23553, #65026, #41816, #23541, #9322, #23354, #684 ) ) ;
#32940 = CARTESIAN_POINT ( 'NONE',  ( -10.23402954931276732, 7.059791383763807993, -35.81110276668997017 ) ) ;
#32941 = VECTOR ( 'NONE', #21880, 1000.000000000000000 ) ;
#32942 = CARTESIAN_POINT ( 'NONE',  ( -190.6985136298601731, 109.1272424661242582, 94.99999999999866418 ) ) ;
#32943 = CARTESIAN_POINT ( 'NONE',  ( 90.91356992076218546, 21.99794663086831648, 70.21725602554428747 ) ) ;
#32944 = CARTESIAN_POINT ( 'NONE',  ( 155.2910738464913152, 55.97560547655804442, -23.97026548063870521 ) ) ;
#32945 = CYLINDRICAL_SURFACE ( 'NONE', #34377, 21.99999999999998579 ) ;
#32946 = CARTESIAN_POINT ( 'NONE',  ( -25.87147652227456263, 100.0000000000000000, 129.5802547743875550 ) ) ;
#32947 = VECTOR ( 'NONE', #42954, 1000.000000000000000 ) ;
#32948 = ADVANCED_FACE ( 'NONE', ( #1867 ), #56704, .F. ) ;
#32949 = CARTESIAN_POINT ( 'NONE',  ( 113.2766812233866318, 31.42710996230401577, -90.24119829850059205 ) ) ;
#32950 = AXIS2_PLACEMENT_3D ( 'NONE', #46013, #9428, #62189 ) ;
#32951 = B_SPLINE_CURVE_WITH_KNOTS ( 'NONE', 3,
 ( #55671, #7504, #44419, #28957, #29288, #39842, #18045, #50402, #66943, #44778, #28237, #33540, #13123, #40195, #49682, #55317, #6446, #27897, #2219, #23668, #49332, #45112, #66595, #60254, #34591, #38808, #50741, #54968, #2561, #1510, #33879, #22975, #17702, #39161, #12421, #67292, #57067, #47183, #62338, #3256, #46491, #8880, #67624, #13461 ),
 .UNSPECIFIED., .F., .F.,
 ( 4, 2, 2, 2, 2, 2, 2, 2, 2, 2, 2, 2, 2, 2, 2, 2, 2, 2, 2, 2, 2, 4 ),
 ( 0.000000000000000000, 0.001488594467279762395, 0.002232891700919633834, 0.002977188934559505274, 0.004465783401839225168, 0.005954377869118944629, 0.007442972336398671895, 0.008187269570038539432, 0.008931566803678405234, 0.01042016127095814551, 0.01190875573823788405, 0.01265305297187775332, 0.01339735020551761913, 0.01488594467279734899, 0.01563024190643721653, 0.01637453914007708233, 0.01786313360735681047, 0.01935172807463653513, 0.02009602530827639399, 0.02084032254191624939, 0.02232891700919594630, 0.02381751147647563627 ),
 .UNSPECIFIED. ) ;
#32952 = CARTESIAN_POINT ( 'NONE',  ( 211.9998916201001293, 116.9275145151761990, 92.12172642968158698 ) ) ;
#32953 = LINE ( 'NONE', #54392, #61187 ) ;
#32954 = ORIENTED_EDGE ( 'NONE', *, *, #42849, .F. ) ;
#32955 = CARTESIAN_POINT ( 'NONE',  ( 62.04382205963241859, 13.48099884269679904, 71.61031193528864947 ) ) ;
#32956 = DIRECTION ( 'NONE',  ( -1.000000000000000000, 0.000000000000000000, 0.000000000000000000 ) ) ;
#32957 = CARTESIAN_POINT ( 'NONE',  ( -11.13714165684778301, 8.138643170880696331, 4.037354935646943588 ) ) ;
#32958 = VECTOR ( 'NONE', #48450, 1000.000000000000000 ) ;
#32959 = DIRECTION ( 'NONE',  ( 0.000000000000000000, 0.000000000000000000, 1.000000000000000000 ) ) ;
#32960 = CARTESIAN_POINT ( 'NONE',  ( -1.314022807222072098, 6.554273999800675377, 41.36949670402924539 ) ) ;
#32961 = DIRECTION ( 'NONE',  ( -1.000000000000000000, -0.000000000000000000, -0.000000000000000000 ) ) ;
#32962 = AXIS2_PLACEMENT_3D ( 'NONE', #36179, #57639, #41112 ) ;
#32963 = CARTESIAN_POINT ( 'NONE',  ( 90.66938301215044760, 21.90914557174533073, 84.57376703108099036 ) ) ;
#32964 = AXIS2_PLACEMENT_3D ( 'NONE', #38601, #59354, #27690 ) ;
#32965 = ADVANCED_FACE ( 'NONE', ( #55660 ), #39830, .T. ) ;
#32966 = VERTEX_POINT ( 'NONE', #18375 ) ;
#32968 = VECTOR ( 'NONE', #58131, 1000.000000000000000 ) ;
#32967 = DIRECTION ( 'NONE',  ( 0.9946643182127709037, -0.1031644031355968688, -9.691922193658267032E-15 ) ) ;
#32969 = CARTESIAN_POINT ( 'NONE',  ( -189.2826425734429563, 107.1493800926106275, -14.39297977970899112 ) ) ;
#32971 = EDGE_CURVE ( 'NONE', #23803, #5602, #18988, .T. ) ;
#32970 = CARTESIAN_POINT ( 'NONE',  ( -126.8005235842505840, 47.09307471149451629, 18.73398224919106880 ) ) ;
#32972 = CARTESIAN_POINT ( 'NONE',  ( -166.9992034932275828, 82.01285191063138313, -37.84924264257025328 ) ) ;
#32973 = CARTESIAN_POINT ( 'NONE',  ( -180.5370160906538786, 95.78117245680181213, 90.87545911180488645 ) ) ;
#32974 = EDGE_LOOP ( 'NONE', ( #48410, #17502, #34063, #23660 ) ) ;
#32975 = PLANE ( 'NONE',  #66103 ) ;
#32976 = CARTESIAN_POINT ( 'NONE',  ( -21.44923284420521625, -47.00251590192956286, 26.66469104408689006 ) ) ;
#32977 = CARTESIAN_POINT ( 'NONE',  ( 201.9721407532274782, 104.3507814346148024, -9.982163974892198866 ) ) ;
#32978 = CARTESIAN_POINT ( 'NONE',  ( -1.866625526081663322, 7.583073082893625028, -65.18153374896648700 ) ) ;
#32979 = CARTESIAN_POINT ( 'NONE',  ( -452.6627218934913230, 0.000000000000000000, -6.938893903907228378E-15 ) ) ;
#32980 = ORIENTED_EDGE ( 'NONE', *, *, #31218, .T. ) ;
#32981 = DIRECTION ( 'NONE',  ( -1.000000000000000000, 0.000000000000000000, 0.000000000000000000 ) ) ;
#32982 = CARTESIAN_POINT ( 'NONE',  ( 80.15818551272217007, 18.36718314243336181, 14.19107730079274887 ) ) ;
#32983 = B_SPLINE_CURVE_WITH_KNOTS ( 'NONE', 3,
 ( #46340, #25608, #68501, #3108, #36841, #46006, #41770, #35455, #15037, #24570, #41079, #58280, #24908, #36493, #10101, #52657, #8736, #25940, #67818, #31556, #47372, #20651, #67472, #19267, #62540, #10435, #43480, #37870, #48390, #5509, #934, #59317, #21008, #26963, #52994, #16753, #42786, #11130, #63910, #64957, #226, #58620, #58968, #43824, #47719, #37173 ),
 .UNSPECIFIED., .F., .F.,
 ( 4, 2, 2, 2, 2, 2, 2, 2, 2, 2, 2, 2, 2, 2, 2, 2, 2, 2, 2, 2, 2, 2, 4 ),
 ( 6.938893903907228378E-18, 0.003192770216278346951, 0.003990962770347930219, 0.004789155324417513487, 0.006385540432556660942, 0.007183732986626248547, 0.007981925540695836152, 0.009578310648835011362, 0.01037650320290461198, 0.01117469575697421086, 0.01197288831104380974, 0.01277108086511340862, 0.01436746597325258383, 0.01596385108139175904, 0.01676204363546133710, 0.01756023618953091170, 0.01835842874360048976, 0.01915662129767006783, 0.02075300640580923089, 0.02234939151394839396, 0.02394577662208756050, 0.02474396917615714203, 0.02554216173022672010 ),
 .UNSPECIFIED. ) ;
#32984 = CARTESIAN_POINT ( 'NONE',  ( -95.20053778133916467, 30.43887292928078381, 35.49128386806113866 ) ) ;
#32985 = PLANE ( 'NONE',  #35957 ) ;
#32987 = ORIENTED_EDGE ( 'NONE', *, *, #26149, .T. ) ;
#32986 = CARTESIAN_POINT ( 'NONE',  ( 114.6797682035588934, 32.10876583290006892, 4.200831402737990494 ) ) ;
#32988 = FACE_OUTER_BOUND ( 'NONE', #48887, .T. ) ;
#32989 = ORIENTED_EDGE ( 'NONE', *, *, #44454, .F. ) ;
#32990 = VERTEX_POINT ( 'NONE', #39370 ) ;
#32991 = CARTESIAN_POINT ( 'NONE',  ( -42.02161712141799654, -16.09918303830819397, 0.000000000000000000 ) ) ;
#32992 = PRESENTATION_LAYER_ASSIGNMENT (  '', '', ( #34171 ) ) ;
#32993 = LINE ( 'NONE', #54430, #54024 ) ;
#32994 = CIRCLE ( 'NONE', #47593, 30.00000000000000000 ) ;
#32996 = ORIENTED_EDGE ( 'NONE', *, *, #32181, .T. ) ;
#32995 = CARTESIAN_POINT ( 'NONE',  ( 157.4703587214989113, 57.65129005721575339, -89.81328548006499091 ) ) ;
#32997 = CARTESIAN_POINT ( 'NONE',  ( 45.57199999999999562, 0.000000000000000000, 0.000000000000000000 ) ) ;
#32998 = DIRECTION ( 'NONE',  ( -0.9989930665413144784, -0.04486483035051863633, 2.500042656554809847E-16 ) ) ;
#32999 = LINE ( 'NONE', #54084, #33928 ) ;
#33000 = VECTOR ( 'NONE', #57366, 1000.000000000000000 ) ;
#33001 = EDGE_LOOP ( 'NONE', ( #46038, #62130, #29048, #44251 ) ) ;
#33002 = EDGE_CURVE ( 'NONE', #39573, #64962, #38099, .T. ) ;
#33003 = CARTESIAN_POINT ( 'NONE',  ( 60.58000000000000540, -36.09918303830819752, 15.41169613715280562 ) ) ;
#33004 = AXIS2_PLACEMENT_3D ( 'NONE', #34702, #17454, #66374 ) ;
#33005 = VECTOR ( 'NONE', #53463, 1000.000000000000000 ) ;
#33006 = EDGE_CURVE ( 'NONE', #16361, #30638, #6657, .T. ) ;
#33007 = CARTESIAN_POINT ( 'NONE',  ( -32.41627406084104734, 9.753381371531506971, -8.520735355804967881 ) ) ;
#33008 = CARTESIAN_POINT ( 'NONE',  ( 156.7474413564702616, 57.09079859174879346, -89.83946617008655267 ) ) ;
#33009 = CIRCLE ( 'NONE', #21802, 65.00000000000000000 ) ;
#33010 = CARTESIAN_POINT ( 'NONE',  ( 126.4633682455862100, 38.28837286275645369, 65.14279228220068774 ) ) ;
#33011 = ORIENTED_EDGE ( 'NONE', *, *, #25744, .F. ) ;
#33012 = ORIENTED_EDGE ( 'NONE', *, *, #24708, .T. ) ;
#33013 = ORIENTED_EDGE ( 'NONE', *, *, #37162, .T. ) ;
#33014 = DIRECTION ( 'NONE',  ( 1.000000000000000000, 0.000000000000000000, -0.000000000000000000 ) ) ;
#33015 = CARTESIAN_POINT ( 'NONE',  ( -50.00000000000001421, -19.99999999999996447, 2.000000000000015543 ) ) ;
#33016 = DIRECTION ( 'NONE',  ( -1.000000000000000000, 0.000000000000000000, 0.000000000000000000 ) ) ;
#33017 = DIRECTION ( 'NONE',  ( 0.000000000000000000, 1.000000000000000000, 0.000000000000000000 ) ) ;
#33018 = CARTESIAN_POINT ( 'NONE',  ( 42.02161712141799654, -16.09918303830818687, 0.000000000000000000 ) ) ;
#33019 = DIRECTION ( 'NONE',  ( -0.000000000000000000, -0.000000000000000000, -1.000000000000000000 ) ) ;
#33020 = EDGE_CURVE ( 'NONE', #65087, #44762, #54203, .T. ) ;
#33021 = CARTESIAN_POINT ( 'NONE',  ( -447.6627218934913230, 399.9999999999997726, 103.5502958579881891 ) ) ;
#33022 = CARTESIAN_POINT ( 'NONE',  ( -47.97412431374925035, 13.93110604348564685, 89.00688050077388880 ) ) ;
#33023 = DIRECTION ( 'NONE',  ( 1.000000000000000000, 0.000000000000000000, 0.000000000000000000 ) ) ;
#33024 = ADVANCED_FACE ( 'NONE', ( #329 ), #21782, .F. ) ;
#33025 = ORIENTED_EDGE ( 'NONE', *, *, #24226, .F. ) ;
#33026 = CARTESIAN_POINT ( 'NONE',  ( -97.72846716802192191, 31.64568465353664806, -90.23871114884526889 ) ) ;
#33027 = EDGE_LOOP ( 'NONE', ( #15411, #23045, #20838, #2132 ) ) ;
#33028 = ORIENTED_EDGE ( 'NONE', *, *, #47177, .F. ) ;
#33029 = CARTESIAN_POINT ( 'NONE',  ( 184.3941060377212011, 82.01604625189465025, 30.06399996121712093 ) ) ;
#33030 = ADVANCED_FACE ( 'NONE', ( #50647 ), #2470, .F. ) ;
#33031 = DIRECTION ( 'NONE',  ( 0.000000000000000000, 0.000000000000000000, 1.000000000000000000 ) ) ;
#33032 = CARTESIAN_POINT ( 'NONE',  ( -31.43908319763710679, -170.0000000000000000, -50.31719736520186359 ) ) ;
#33033 = CARTESIAN_POINT ( 'NONE',  ( -38.61120365219831996, 10.87907113164045469, -94.14611914679960591 ) ) ;
#33034 = CARTESIAN_POINT ( 'NONE',  ( 22.15926701483428829, 7.796117250416236821, 41.47971552668069251 ) ) ;
#33035 = EDGE_CURVE ( 'NONE', #41523, #43949, #23923, .T. ) ;
#33036 = LINE ( 'NONE', #16845, #64100 ) ;
#33037 = DIRECTION ( 'NONE',  ( -1.000000000000000000, 0.000000000000000000, 0.000000000000000000 ) ) ;
#33038 = VERTEX_POINT ( 'NONE', #45375 ) ;
#33039 = CARTESIAN_POINT ( 'NONE',  ( -317.6627218934913230, 394.9999999999997158, -11.44970414201176823 ) ) ;
#33040 = CARTESIAN_POINT ( 'NONE',  ( 0.000000000000000000, 65.13282190615278466, -9.999999999999998224 ) ) ;
#33041 = VERTEX_POINT ( 'NONE', #15357 ) ;
#33042 = CARTESIAN_POINT ( 'NONE',  ( 2.644994884459111795, -7.710515798486388128, -9.417753204360273855 ) ) ;
#33043 = PRESENTATION_STYLE_ASSIGNMENT (( #5007 ) ) ;
#33044 = EDGE_LOOP ( 'NONE', ( #56135, #55933, #27293, #488, #50805, #50628, #30712, #37175, #45505 ) ) ;
#33045 = CARTESIAN_POINT ( 'NONE',  ( -83.12901536265223967, 24.07178615860086168, 43.95099611738770307 ) ) ;
#33046 = DIRECTION ( 'NONE',  ( 1.000000000000000000, 0.000000000000000000, 0.000000000000000000 ) ) ;
#33047 = DIRECTION ( 'NONE',  ( 0.000000000000000000, 0.000000000000000000, 1.000000000000000000 ) ) ;
#33048 = CARTESIAN_POINT ( 'NONE',  ( -28.13852122803040956, 9.072484007196644384, 57.80876482626037216 ) ) ;
#33049 = CIRCLE ( 'NONE', #3881, 243.4957430088094839 ) ;
#33050 = CARTESIAN_POINT ( 'NONE',  ( 128.0848616812662613, 38.04676222636084049, -11.86342996178354703 ) ) ;
#33051 = EDGE_CURVE ( 'NONE', #46092, #28503, #52295, .T. ) ;
#33052 = ORIENTED_EDGE ( 'NONE', *, *, #65129, .F. ) ;
#33053 = PRESENTATION_LAYER_ASSIGNMENT (  '', '', ( #63384 ) ) ;
#33054 = ORIENTED_EDGE ( 'NONE', *, *, #9525, .T. ) ;
#33055 = ADVANCED_FACE ( 'NONE', ( #68476 ), #66853, .F. ) ;
#33056 = EDGE_CURVE ( 'NONE', #62663, #28396, #57922, .T. ) ;
#33057 = EDGE_CURVE ( 'NONE', #26875, #10843, #25917, .T. ) ;
#33058 = CYLINDRICAL_SURFACE ( 'NONE', #6486, 89.99999999999998579 ) ;
#33059 = EDGE_LOOP ( 'NONE', ( #63319, #46185, #54568, #7983 ) ) ;
#33060 = CARTESIAN_POINT ( 'NONE',  ( -190.6985136298601731, 109.1272424661242582, -95.00000000000133582 ) ) ;
#33061 = CARTESIAN_POINT ( 'NONE',  ( 188.0298970627777635, 87.42051935455698697, -94.54416634815818554 ) ) ;
#33062 = VECTOR ( 'NONE', #41019, 1000.000000000000000 ) ;
#33063 = CARTESIAN_POINT ( 'NONE',  ( 206.3125232506203304, 108.5822159704962075, 44.04308254722315041 ) ) ;
#33064 = DIRECTION ( 'NONE',  ( -1.000000000000000000, 0.000000000000000000, 0.000000000000000000 ) ) ;
#33065 = AXIS2_PLACEMENT_3D ( 'NONE', #63758, #64091, #15566 ) ;
#33066 = CARTESIAN_POINT ( 'NONE',  ( 196.9999999999999716, 6.000000000000000000, -3.000000000000030198 ) ) ;
#33067 = CIRCLE ( 'NONE', #2740, 10.00000000000000178 ) ;
#33068 = ORIENTED_EDGE ( 'NONE', *, *, #38565, .F. ) ;
#33069 = CARTESIAN_POINT ( 'NONE',  ( -125.4481990864045287, 46.20056605584957765, -76.75825448869764500 ) ) ;
#33070 = ORIENTED_EDGE ( 'NONE', *, *, #69568, .T. ) ;
#33071 = EDGE_LOOP ( 'NONE', ( #40800, #12718, #17154, #40366, #61054, #60187, #47581, #50760, #5984 ) ) ;
#33072 = DIRECTION ( 'NONE',  ( 0.6234898018587319291, 0.7818314824680311359, 0.000000000000000000 ) ) ;
#33073 = DIRECTION ( 'NONE',  ( 1.000000000000000000, 0.000000000000000000, 0.000000000000000000 ) ) ;
#33074 = DIRECTION ( 'NONE',  ( -0.000000000000000000, -0.000000000000000000, -1.000000000000000000 ) ) ;
#33075 = CARTESIAN_POINT ( 'NONE',  ( 6.000000000000000000, 19.07878402833891229, -5.000000000000000888 ) ) ;
#33076 = DIRECTION ( 'NONE',  ( 1.000000000000000000, 0.000000000000000000, 0.000000000000000000 ) ) ;
#33077 = ORIENTED_EDGE ( 'NONE', *, *, #52632, .F. ) ;
#33078 = CARTESIAN_POINT ( 'NONE',  ( 79.23200707685333555, 17.02828389812517429, 11.62992474421185385 ) ) ;
#33079 = ORIENTED_EDGE ( 'NONE', *, *, #16439, .F. ) ;
#33080 = CARTESIAN_POINT ( 'NONE',  ( -71.26675986148646302, 19.63956187826085298, 39.16646718081778289 ) ) ;
#33081 = ORIENTED_EDGE ( 'NONE', *, *, #30143, .T. ) ;
#33082 = PLANE ( 'NONE',  #68999 ) ;
#33083 = EDGE_LOOP ( 'NONE', ( #4405, #50747, #18574, #32184 ) ) ;
#33084 = CARTESIAN_POINT ( 'NONE',  ( 422.4999999999999432, -18.06806526123148160, 378.0000000000000000 ) ) ;
#33085 = PLANE ( 'NONE',  #30570 ) ;
#33086 = DIRECTION ( 'NONE',  ( 0.000000000000000000, -1.000000000000000000, 0.000000000000000000 ) ) ;
#33087 = ORIENTED_EDGE ( 'NONE', *, *, #9062, .T. ) ;
#33088 = FACE_OUTER_BOUND ( 'NONE', #68951, .T. ) ;
#33089 = DIRECTION ( 'NONE',  ( 1.000000000000000000, 0.000000000000000000, 0.000000000000000000 ) ) ;
#33090 = EDGE_CURVE ( 'NONE', #16235, #29084, #13710, .T. ) ;
#33091 = CARTESIAN_POINT ( 'NONE',  ( 280.0000000000000000, 21.42428528562853529, 4.999999999999990230 ) ) ;
#33092 = AXIS2_PLACEMENT_3D ( 'NONE', #61737, #35018, #55419 ) ;
#33093 = PLANE ( 'NONE',  #64574 ) ;
#33094 = CARTESIAN_POINT ( 'NONE',  ( -129.6165111262478149, 48.99406349865698473, -22.08429765273019996 ) ) ;
#33095 = LINE ( 'NONE', #54173, #35680 ) ;
#33096 = FACE_OUTER_BOUND ( 'NONE', #44226, .T. ) ;
#33097 = B_SPLINE_CURVE_WITH_KNOTS ( 'NONE', 3,
 ( #69233, #9472, #31961, #57660, #279, #15776, #14739, #63962, #37222, #52376, #68556, #10489, #52705, #4871, #5559, #48444, #58331, #20709, #4197, #10149, #26340, #25661, #47093, #4533, #20359, #36894, #37574, #48113, #30933, #42837, #26682, #21065, #53388, #31611, #41826, #63281, #42165, #67028 ),
 .UNSPECIFIED., .F., .F.,
 ( 4, 2, 2, 2, 2, 2, 2, 2, 2, 2, 2, 2, 2, 2, 2, 2, 2, 2, 4 ),
 ( 1.551583845779545699E-17, 0.001559859933532273648, 0.003119719867064531683, 0.004679579800596789067, 0.006239439734129047753, 0.007799299667661305571, 0.008579229634427429710, 0.009359159601193552114, 0.01091901953472580039, 0.01169894950149191065, 0.01247887946825801918, 0.01403873940179021888, 0.01559859933532241859, 0.01715845926885461656, 0.01871831920238681626, 0.02027817913591901597, 0.02183803906945121567, 0.02339789900298341538, 0.02495775893651561508 ),
 .UNSPECIFIED. ) ;
#33098 = ORIENTED_EDGE ( 'NONE', *, *, #65770, .T. ) ;
#33099 = FACE_OUTER_BOUND ( 'NONE', #31015, .T. ) ;
#33100 = DIRECTION ( 'NONE',  ( 1.000000000000000000, 0.000000000000000000, 0.000000000000000000 ) ) ;
#33101 = ORIENTED_EDGE ( 'NONE', *, *, #61939, .T. ) ;
#33102 = FACE_BOUND ( 'NONE', #24465, .T. ) ;
#33103 = CARTESIAN_POINT ( 'NONE',  ( 76.57571471437145760, 0.000000000000000000, -30.00000000000000000 ) ) ;
#33104 = CIRCLE ( 'NONE', #55598, 10.00000000000000000 ) ;
#33105 = CARTESIAN_POINT ( 'NONE',  ( -180.2188652555596491, 96.98354576637423463, 62.72563788181442845 ) ) ;
#33106 = CARTESIAN_POINT ( 'NONE',  ( -447.6627218934913230, 394.9999999999998295, 108.5502958579881181 ) ) ;
#33107 = CARTESIAN_POINT ( 'NONE',  ( 23.81581464765719502, -7.603089679099516829, 0.000000000000000000 ) ) ;
#33108 = CARTESIAN_POINT ( 'NONE',  ( -81.90760111942957167, 24.66532273091449667, 17.85392087365031344 ) ) ;
#33109 = CARTESIAN_POINT ( 'NONE',  ( -12.99999999999999645, 10.00000000000000000, -33.00000000000000000 ) ) ;
#33110 = CARTESIAN_POINT ( 'NONE',  ( 114.4903733860909654, 21.88945422885941028, -2.223679814509753161 ) ) ;
#33111 = EDGE_CURVE ( 'NONE', #1423, #25478, #9389, .T. ) ;
#33112 = CARTESIAN_POINT ( 'NONE',  ( -125.6703656163502529, 47.55170550253217954, -76.75825448869768763 ) ) ;
#33113 = EDGE_CURVE ( 'NONE', #50267, #7537, #9738, .T. ) ;
#33114 = AXIS2_PLACEMENT_3D ( 'NONE', #25572, #56889, #56525 ) ;
#33115 = CARTESIAN_POINT ( 'NONE',  ( 41.71033659965589635, -1.250000000000021982, 13.79046340968178619 ) ) ;
#33117 = ADVANCED_FACE ( 'NONE', ( #35163 ), #20620, .T. ) ;
#33116 = CARTESIAN_POINT ( 'NONE',  ( 163.7607557204680404, 62.71181783708028235, 14.18050344063046886 ) ) ;
#33118 = CARTESIAN_POINT ( 'NONE',  ( 42.79263376053064860, 9.891365420389709229, -90.11595853705047432 ) ) ;
#33119 = ORIENTED_EDGE ( 'NONE', *, *, #46593, .F. ) ;
#33121 = VECTOR ( 'NONE', #49069, 1000.000000000000114 ) ;
#33120 = CARTESIAN_POINT ( 'NONE',  ( 209.3223706822284100, 190.0000000000000000, 31.44247402469554942 ) ) ;
#33122 = ORIENTED_EDGE ( 'NONE', *, *, #32472, .F. ) ;
#33123 = CARTESIAN_POINT ( 'NONE',  ( -444.1126562889743923, 394.7876926391177790, 94.27943548784956818 ) ) ;
#33124 = EDGE_CURVE ( 'NONE', #14014, #16854, #8087, .T. ) ;
#33125 = CARTESIAN_POINT ( 'NONE',  ( 81.04027388895737261, 18.64386073872847760, -65.14085334647751324 ) ) ;
#33126 = CARTESIAN_POINT ( 'NONE',  ( 103.6609592836012439, 27.04873813663200721, 94.41228810559154283 ) ) ;
#33127 = CARTESIAN_POINT ( 'NONE',  ( -143.2498117110515352, 60.33382252735061257, 60.92286773224797969 ) ) ;
#33128 = CARTESIAN_POINT ( 'NONE',  ( 69.49862690228275142, 14.27023134440515051, -20.17942441373172358 ) ) ;
#33129 = CARTESIAN_POINT ( 'NONE',  ( -24.32776401346968242, 9.546905915310563984, -40.38412230395840652 ) ) ;
#33130 = CARTESIAN_POINT ( 'NONE',  ( 211.7634543339367781, 118.4123239814494610, -95.00000000000133582 ) ) ;
#33131 = CARTESIAN_POINT ( 'NONE',  ( -73.58789645738433194, 21.51976592945687727, -90.76835761085054344 ) ) ;
#33132 = CARTESIAN_POINT ( 'NONE',  ( -125.4463376280758666, 47.40387005565908396, -23.05918939656154265 ) ) ;
#33133 = VERTEX_POINT ( 'NONE', #4454 ) ;
#33134 = VERTEX_POINT ( 'NONE', #4115 ) ;
#33135 = CARTESIAN_POINT ( 'NONE',  ( 33.46033188299907835, 8.722678254080102889, 59.67493974660781930 ) ) ;
#33136 = CARTESIAN_POINT ( 'NONE',  ( -8.651394114442540584, -32.28678521934651258, 6.893343212288941757 ) ) ;
#33137 = CARTESIAN_POINT ( 'NONE',  ( -66.97713359923307053, -33.64188291209072190, 41.38025477438755928 ) ) ;
#33138 = CARTESIAN_POINT ( 'NONE',  ( 442.3372781065083359, 370.0000000000043201, 108.5502958579838833 ) ) ;
#33139 = PRODUCT_DEFINITION_CONTEXT ( 'detailed design', #62394, 'design' ) ;
#33140 = DIRECTION ( 'NONE',  ( -0.000000000000000000, -1.000000000000000000, -0.000000000000000000 ) ) ;
#33141 = VERTEX_POINT ( 'NONE', #56623 ) ;
#33142 = EDGE_CURVE ( 'NONE', #28536, #30662, #36815, .T. ) ;
#33143 = CARTESIAN_POINT ( 'NONE',  ( 94.11733320392089297, 23.18939451097127957, 9.873858910156306123 ) ) ;
#33144 = CARTESIAN_POINT ( 'NONE',  ( -14.32241591711280115, 7.401556312061830845, 68.21502159609927674 ) ) ;
#33145 = CARTESIAN_POINT ( 'NONE',  ( -81.00507684688699328, 23.22613445438386748, -8.640849626975995790 ) ) ;
#33146 = FACE_OUTER_BOUND ( 'NONE', #65775, .T. ) ;
#33147 = CARTESIAN_POINT ( 'NONE',  ( 42.49453823366105354, 8.831814337191476127, -9.438221642302703884 ) ) ;
#33148 = CARTESIAN_POINT ( 'NONE',  ( 211.7419975634644800, 116.5322580952101674, -19.63582788492490394 ) ) ;
#33149 = FACE_BOUND ( 'NONE', #3253, .T. ) ;
#33150 = EDGE_CURVE ( 'NONE', #56752, #43605, #40374, .T. ) ;
#33151 = CARTESIAN_POINT ( 'NONE',  ( -61.86403937395562025, 16.61416349803655734, -39.56707441162413375 ) ) ;
#33152 = VECTOR ( 'NONE', #67704, 1000.000000000000000 ) ;
#33153 = ORIENTED_EDGE ( 'NONE', *, *, #56875, .T. ) ;
#33154 = CARTESIAN_POINT ( 'NONE',  ( -109.6829043543429236, 37.85329552808669717, -95.00000000000133582 ) ) ;
#33155 = CARTESIAN_POINT ( 'NONE',  ( 93.32756701508621688, 22.89083686918420568, -39.91087544770613249 ) ) ;
#33156 = AXIS2_PLACEMENT_3D ( 'NONE', #13056, #66522, #18314 ) ;
#33157 = DIRECTION ( 'NONE',  ( -0.000000000000000000, 1.000000000000000000, -0.000000000000000000 ) ) ;
#33158 = DIRECTION ( 'NONE',  ( -0.000000000000000000, 1.000000000000000000, -0.000000000000000000 ) ) ;
#33159 = FACE_OUTER_BOUND ( 'NONE', #12894, .T. ) ;
#33160 = LINE ( 'NONE', #18022, #28850 ) ;
#33161 = AXIS2_PLACEMENT_3D ( 'NONE', #46168, #30692, #35631 ) ;
#33162 = AXIS2_PLACEMENT_3D ( 'NONE', #46291, #57893, #67769 ) ;
#33163 = ORIENTED_EDGE ( 'NONE', *, *, #39086, .T. ) ;
#33164 = CARTESIAN_POINT ( 'NONE',  ( 55.76066037845578194, 11.10616952318092032, 8.503228194878166946 ) ) ;
#33165 = CARTESIAN_POINT ( 'NONE',  ( 10.55634918610403084, 0.000000000000000000, 2.000000000000000000 ) ) ;
#33166 = VERTEX_POINT ( 'NONE', #58257 ) ;
#33167 = ORIENTED_EDGE ( 'NONE', *, *, #9454, .F. ) ;
#33168 = VECTOR ( 'NONE', #33544, 1000.000000000000227 ) ;
#33169 = CARTESIAN_POINT ( 'NONE',  ( 5.799999999999999822, 8.000000000000000000, 0.000000000000000000 ) ) ;
#33170 = DIRECTION ( 'NONE',  ( -1.020422603260505347E-14, 1.000000000000000000, 5.551115123125782702E-17 ) ) ;
#33171 = CARTESIAN_POINT ( 'NONE',  ( 107.2672065034543039, 27.52931006625852817, 30.22273792253545466 ) ) ;
#33172 = VERTEX_POINT ( 'NONE', #25581 ) ;
#33173 = ORIENTED_EDGE ( 'NONE', *, *, #56278, .T. ) ;
#33174 = CARTESIAN_POINT ( 'NONE',  ( -0.2727178028659107412, 0.000000000000000000, 0.000000000000000000 ) ) ;
#33175 = CARTESIAN_POINT ( 'NONE',  ( 157.9121974517528599, 59.27335488206247760, 29.40946747225336821 ) ) ;
#33176 = CARTESIAN_POINT ( 'NONE',  ( -156.0204364459164594, 71.27041535366184632, -65.42916888645565621 ) ) ;
#33177 = PRODUCT_RELATED_PRODUCT_CATEGORY ( 'part', '', ( #8064 ) ) ;
#33178 = CARTESIAN_POINT ( 'NONE',  ( 70.51583798635768119, 15.57951509147424041, 10.22650159239598544 ) ) ;
#33179 = CARTESIAN_POINT ( 'NONE',  ( 64.08056813503694116, 12.89932471814516290, 3.125053320693556313E-16 ) ) ;
#33180 = EDGE_CURVE ( 'NONE', #10664, #41218, #31533, .T. ) ;
#33181 = LINE ( 'NONE', #17335, #59244 ) ;
#33182 = EDGE_CURVE ( 'NONE', #24540, #14371, #4793, .T. ) ;
#33183 = CARTESIAN_POINT ( 'NONE',  ( 39.40195752203891999, 9.424259417798149130, 44.91383430596327742 ) ) ;
#33184 = CARTESIAN_POINT ( 'NONE',  ( -41.31727360890708667, -62.59299402909810084, 0.000000000000000000 ) ) ;
#33185 = DIRECTION ( 'NONE',  ( -0.000000000000000000, -0.000000000000000000, -1.000000000000000000 ) ) ;
#33186 = CARTESIAN_POINT ( 'NONE',  ( 63.42461771757965039, 12.76763389977390695, -89.40979201309708913 ) ) ;
#33187 = CARTESIAN_POINT ( 'NONE',  ( 88.27986429602357532, 19.99062825313306391, 83.57789623867044781 ) ) ;
#33189 = ORIENTED_EDGE ( 'NONE', *, *, #28030, .F. ) ;
#33188 = FACE_OUTER_BOUND ( 'NONE', #18720, .T. ) ;
#33190 = VERTEX_POINT ( 'NONE', #7753 ) ;
#33191 = ORIENTED_EDGE ( 'NONE', *, *, #66589, .F. ) ;
#33192 = CARTESIAN_POINT ( 'NONE',  ( -15.26524495591509556, 7.490231452641286758, -17.05327951355247151 ) ) ;
#33193 = CARTESIAN_POINT ( 'NONE',  ( -54.08504625707234226, 14.42374043447185272, 45.27053657996511049 ) ) ;
#33194 = DIRECTION ( 'NONE',  ( -1.000000000000000000, 0.000000000000000000, 0.000000000000000000 ) ) ;
#33195 = DIRECTION ( 'NONE',  ( -0.000000000000000000, 1.000000000000000000, -0.000000000000000000 ) ) ;
#33196 = EDGE_CURVE ( 'NONE', #13211, #7345, #30240, .T. ) ;
#33197 = CARTESIAN_POINT ( 'NONE',  ( -59.58556642339446086, 16.99097764963621771, -36.72105999418167244 ) ) ;
#33198 = CARTESIAN_POINT ( 'NONE',  ( -14.84452950307166219, 8.460866451887694595, -18.72723383062862368 ) ) ;
#33199 = DIRECTION ( 'NONE',  ( -0.000000000000000000, -0.000000000000000000, -1.000000000000000000 ) ) ;
#33200 = CARTESIAN_POINT ( 'NONE',  ( 410.0000000000000000, 0.000000000000000000, 380.0000000000000000 ) ) ;
#33201 = ORIENTED_EDGE ( 'NONE', *, *, #42084, .F. ) ;
#33202 = CIRCLE ( 'NONE', #25384, 74.95140232871122521 ) ;
#33203 = CYLINDRICAL_SURFACE ( 'NONE', #34039, 72.99999999999998579 ) ;
#33204 = EDGE_LOOP ( 'NONE', ( #49834, #56468, #51894, #56685, #28472 ) ) ;
#33205 = ADVANCED_FACE ( 'NONE', ( #45725, #27274, #33275, #64928, #42760, #26597, #65629, #5139, #16722, #37146, #43105, #195, #27977, #11435, #65268, #59976, #5482, #21312, #58589, #64575, #1250, #22702, #10408, #22010, #31877, #64222, #38181, #69494, #49420, #53305, #48033, #6167, #32907, #16035, #59621, #37487 ), #44142, .T. ) ;
#33206 = ORIENTED_EDGE ( 'NONE', *, *, #7463, .F. ) ;
#33207 = ADVANCED_FACE ( 'NONE', ( #26936 ), #54702, .F. ) ;
#33208 = CARTESIAN_POINT ( 'NONE',  ( -62.97854483871554976, -16.08424353203763957, 40.00000000000003553 ) ) ;
#33209 = AXIS2_PLACEMENT_3D ( 'NONE', #24659, #57009, #46437 ) ;
#33210 = CARTESIAN_POINT ( 'NONE',  ( -60.12227522086160292, 17.14774203938726416, -90.87396971807878288 ) ) ;
#33211 = DIRECTION ( 'NONE',  ( 0.000000000000000000, 0.000000000000000000, -1.000000000000000000 ) ) ;
#33212 = LINE ( 'NONE', #55344, #55444 ) ;
#33213 = AXIS2_PLACEMENT_3D ( 'NONE', #51899, #3709, #68097 ) ;
#33214 = VECTOR ( 'NONE', #440, 1000.000000000000000 ) ;
#33215 = CARTESIAN_POINT ( 'NONE',  ( -108.9136445001389575, 36.28030794288191885, 14.68305003638678841 ) ) ;
#33216 = LINE ( 'NONE', #39191, #56176 ) ;
#33217 = AXIS2_PLACEMENT_3D ( 'NONE', #69211, #41111, #26316 ) ;
#33218 = CARTESIAN_POINT ( 'NONE',  ( 141.2801018238827453, 47.29457739955285689, -15.57642269469550200 ) ) ;
#33219 = VERTEX_POINT ( 'NONE', #54344 ) ;
#33220 = ORIENTED_EDGE ( 'NONE', *, *, #52083, .F. ) ;
#33221 = VECTOR ( 'NONE', #50142, 1000.000000000000000 ) ;
#33222 = ORIENTED_EDGE ( 'NONE', *, *, #65793, .T. ) ;
#33223 = CARTESIAN_POINT ( 'NONE',  ( 86.62931800182293784, -170.0000000000000000, -8.977013608448027426 ) ) ;
#33224 = AXIS2_PLACEMENT_3D ( 'NONE', #5407, #37070, #5739 ) ;
#33225 = CARTESIAN_POINT ( 'NONE',  ( -157.0079874970173250, 72.18249880494039417, -15.19463801503674460 ) ) ;
#33226 = CARTESIAN_POINT ( 'NONE',  ( 39.40195752203892710, 8.409560354027375340, -77.46436805589148378 ) ) ;
#33227 = DIRECTION ( 'NONE',  ( 0.000000000000000000, -0.9999993111447558203, 0.001173758924898823551 ) ) ;
#33228 = APPLICATION_CONTEXT ( 'automotive_design' ) ;
#33229 = CARTESIAN_POINT ( 'NONE',  ( -38.54881010929333485, 10.86689971295296431, 66.99878871782735246 ) ) ;
#33230 = CARTESIAN_POINT ( 'NONE',  ( -8.000000000000000000, -3.098204225878183671, -9.184209322808126075 ) ) ;
#33231 = ORIENTED_EDGE ( 'NONE', *, *, #41778, .F. ) ;
#33232 = CARTESIAN_POINT ( 'NONE',  ( 63.01563776193091826, 12.67277567978498709, -62.56524142263340593 ) ) ;
#33233 = CARTESIAN_POINT ( 'NONE',  ( -154.6171773099879658, 68.63761944777705537, 70.56064342458570593 ) ) ;
#33234 = CARTESIAN_POINT ( 'NONE',  ( -177.2385321673937142, 68.86478131554724769, 432.4362760962258108 ) ) ;
#33235 = CARTESIAN_POINT ( 'NONE',  ( -4.071369321747702053, 7.682719369516287422, -36.40674159414955113 ) ) ;
#33236 = LINE ( 'NONE', #27240, #62330 ) ;
#33237 = CARTESIAN_POINT ( 'NONE',  ( -82.53770812813171176, 23.83403279300014432, -49.04362026007095920 ) ) ;
#33239 = EDGE_CURVE ( 'NONE', #14014, #45637, #48714, .T. ) ;
#33238 = DIRECTION ( 'NONE',  ( -0.000000000000000000, 0.000000000000000000, 1.000000000000000000 ) ) ;
#33240 = CARTESIAN_POINT ( 'NONE',  ( 0.000000000000000000, 0.000000000000000000, 170.0000000000000000 ) ) ;
#33241 = CARTESIAN_POINT ( 'NONE',  ( 12.03194517566456412, 6.409266703743583982, -63.35348225446327319 ) ) ;
#33242 = B_SPLINE_CURVE_WITH_KNOTS ( 'NONE', 3,
 ( #40247, #19473, #8238, #25116, #8592, #2965, #36350, #40933, #20169, #34972, #30040, #57803, #13516, #9622, #52178, #14547, #29686, #35666, #51502, #36007, #24072, #56416, #62392, #51151, #67339, #45515, #14883, #66999, #24425, #24765, #45867, #67678, #57120, #46548, #62036, #19127, #30731, #40581, #31084, #14207, #30380, #51832, #3641 ),
 .UNSPECIFIED., .F., .F.,
 ( 4, 2, 2, 2, 2, 2, 2, 2, 2, 2, 2, 2, 1, 2, 2, 2, 2, 2, 2, 2, 2, 4 ),
 ( 0.02390068823634511341, 0.02538837671117072023, 0.02613222094858352190, 0.02687606518599632011, 0.02836375366082194427, 0.02985144213564756843, 0.03059528637306038745, 0.03133913061047320647, 0.03282681908529885145, 0.03431450756012450337, 0.03580219603495014835, 0.03654604027236297431, 0.03728988450977580027, 0.03803372874718861929, 0.03877757298460144525, 0.04026526145942713186, 0.04175294993425281154, 0.04324063840907849815, 0.04398448264649133799, 0.04472832688390418476, 0.04621601535872985056, 0.04770370383355551636 ),
 .UNSPECIFIED. ) ;
#33243 = VERTEX_POINT ( 'NONE', #48363 ) ;
#33244 = FACE_OUTER_BOUND ( 'NONE', #4484, .T. ) ;
#33245 = CARTESIAN_POINT ( 'NONE',  ( -133.3958821919892728, 51.63629593114584537, -69.77245200765010225 ) ) ;
#33246 = DIRECTION ( 'NONE',  ( -1.000000000000000000, 0.000000000000000000, 0.000000000000000000 ) ) ;
#33247 = LINE ( 'NONE', #43425, #4282 ) ;
#33248 = DIRECTION ( 'NONE',  ( -1.734723475976805517E-15, 0.000000000000000000, 1.000000000000000000 ) ) ;
#33249 = ORIENTED_EDGE ( 'NONE', *, *, #4241, .T. ) ;
#33250 = ORIENTED_EDGE ( 'NONE', *, *, #31124, .T. ) ;
#33251 = LINE ( 'NONE', #54685, #31398 ) ;
#33252 = DIRECTION ( 'NONE',  ( -0.9195277725514544587, 0.3930250316539148359, 5.102127870520019688E-18 ) ) ;
#33253 = ORIENTED_EDGE ( 'NONE', *, *, #66326, .T. ) ;
#33254 = CIRCLE ( 'NONE', #52375, 5.000000000000004441 ) ;
#33255 = ORIENTED_EDGE ( 'NONE', *, *, #68983, .F. ) ;
#33256 = CARTESIAN_POINT ( 'NONE',  ( 174.1251613516845111, 71.84747073139213569, -40.87395508819982126 ) ) ;
#33257 = LINE ( 'NONE', #21991, #22346 ) ;
#33258 = VERTEX_POINT ( 'NONE', #553 ) ;
#33259 = DIRECTION ( 'NONE',  ( 0.000000000000000000, 0.000000000000000000, 1.000000000000000000 ) ) ;
#33260 = CARTESIAN_POINT ( 'NONE',  ( 136.1215428813736992, 43.99260314811117212, 56.69008934874803174 ) ) ;
#33261 = CARTESIAN_POINT ( 'NONE',  ( -77.02372450489323796, 21.70271995013165167, -49.93720601098491585 ) ) ;
#33262 = DIRECTION ( 'NONE',  ( 0.000000000000000000, 0.000000000000000000, -1.000000000000000000 ) ) ;
#33263 = VECTOR ( 'NONE', #58905, 1000.000000000000000 ) ;
#33265 = DIRECTION ( 'NONE',  ( -2.312964634635743450E-16, 0.000000000000000000, -1.000000000000000000 ) ) ;
#33264 = VECTOR ( 'NONE', #56607, 1000.000000000000000 ) ;
#33266 = CARTESIAN_POINT ( 'NONE',  ( -189.2442476610617916, 107.0963225822736007, 38.85773244000630910 ) ) ;
#33267 = AXIS2_PLACEMENT_3D ( 'NONE', #16779, #26654, #48091 ) ;
#33268 = ADVANCED_BREP_SHAPE_REPRESENTATION ( '', ( #17922, #66832 ), #59007 ) ;
#33269 = VECTOR ( 'NONE', #18388, 1000.000000000000000 ) ;
#33270 = EDGE_CURVE ( 'NONE', #69128, #24965, #22356, .T. ) ;
#33271 = ORIENTED_EDGE ( 'NONE', *, *, #62086, .F. ) ;
#33272 = CARTESIAN_POINT ( 'NONE',  ( 113.8568724296587789, 30.58972477291343850, -50.01180695322363334 ) ) ;
#33273 = AXIS2_PLACEMENT_3D ( 'NONE', #52736, #20388, #43208 ) ;
#33274 = EDGE_CURVE ( 'NONE', #10310, #24054, #37011, .T. ) ;
#33275 = FACE_BOUND ( 'NONE', #5491, .T. ) ;
#33276 = CARTESIAN_POINT ( 'NONE',  ( 41.80536115778105000, 8.734184316430663841, -50.22851050661703454 ) ) ;
#33277 = CARTESIAN_POINT ( 'NONE',  ( -167.4844853368928170, 82.52074065752736942, -74.01054566969028770 ) ) ;
#33279 = ORIENTED_EDGE ( 'NONE', *, *, #49191, .T. ) ;
#33278 = CARTESIAN_POINT ( 'NONE',  ( -129.5125723098807384, 48.92280137375520610, 85.23347960619950925 ) ) ;
#33280 = LINE ( 'NONE', #22015, #34214 ) ;
#33281 = ADVANCED_FACE ( 'NONE', ( #11101 ), #32564, .T. ) ;
#33282 = VERTEX_POINT ( 'NONE', #53992 ) ;
#33283 = CARTESIAN_POINT ( 'NONE',  ( -130.6002960060536395, 49.67125682092491701, 32.26042931784617451 ) ) ;
#33284 = CARTESIAN_POINT ( 'NONE',  ( 60.74750367560238828, -24.13405452624855130, 43.58025477438756212 ) ) ;
#33285 = PLANE ( 'NONE',  #45604 ) ;
#33286 = CARTESIAN_POINT ( 'NONE',  ( 89.87840278991589571, 21.62393877508910833, 30.44804967038920651 ) ) ;
#33287 = CARTESIAN_POINT ( 'NONE',  ( -5.000000000000058620, -31.11269837220806878, 0.000000000000000000 ) ) ;
#33288 = DIRECTION ( 'NONE',  ( 0.6234898018587318180, 0.7818314824680311359, -0.000000000000000000 ) ) ;
#33289 = CARTESIAN_POINT ( 'NONE',  ( 92.19920907511534836, 21.39700525884450855, -75.21216531110735559 ) ) ;
#33290 = CARTESIAN_POINT ( 'NONE',  ( -28.53262343748519214, 9.132042770041840285, -89.57910440806035979 ) ) ;
#33291 = CARTESIAN_POINT ( 'NONE',  ( 311.9975424824652350, 170.0000000000000284, 380.0000000000001137 ) ) ;
#33292 = ORIENTED_EDGE ( 'NONE', *, *, #22308, .T. ) ;
#33293 = EDGE_CURVE ( 'NONE', #22683, #48695, #7135, .T. ) ;
#33294 = VERTEX_POINT ( 'NONE', #38896 ) ;
#33295 = ADVANCED_FACE ( 'NONE', ( #39242 ), #44859, .F. ) ;
#33296 = CARTESIAN_POINT ( 'NONE',  ( 46.90222083990963853, 9.503928413859240365, 37.65402312257223372 ) ) ;
#33297 = PLANE ( 'NONE',  #46400 ) ;
#33298 = DIRECTION ( 'NONE',  ( -0.000000000000000000, -1.000000000000000000, 0.000000000000000000 ) ) ;
#33299 = DIRECTION ( 'NONE',  ( 0.000000000000000000, 1.000000000000000000, 0.000000000000000000 ) ) ;
#33300 = CARTESIAN_POINT ( 'NONE',  ( 211.7318474105134669, 118.3631723164074714, -46.44534482335959069 ) ) ;
#33301 = CARTESIAN_POINT ( 'NONE',  ( -78.19438069111004097, 23.21811806230640585, -76.96000122218163142 ) ) ;
#33302 = FACE_OUTER_BOUND ( 'NONE', #46489, .T. ) ;
#33303 = CARTESIAN_POINT ( 'NONE',  ( 157.4703587214989398, -170.0000000000000000, -16.77963370867396975 ) ) ;
#33304 = CARTESIAN_POINT ( 'NONE',  ( 162.6190874793280727, 61.76782592053313437, -75.92743616221932257 ) ) ;
#33305 = PRODUCT_DEFINITION_SHAPE ( 'NONE', 'NONE',  #69603 ) ;
#33306 = ORIENTED_EDGE ( 'NONE', *, *, #6341, .F. ) ;
#33307 = CARTESIAN_POINT ( 'NONE',  ( -23.93933407965396043, 9.495050561681672718, 11.36750298520080626 ) ) ;
#33308 = ORIENTED_EDGE ( 'NONE', *, *, #29254, .F. ) ;
#33309 = AXIS2_PLACEMENT_3D ( 'NONE', #32771, #16241, #16928 ) ;
#33310 = CARTESIAN_POINT ( 'NONE',  ( 444.9999999999999432, -35.00000000000000000, 2.000000000000000000 ) ) ;
#33311 = CARTESIAN_POINT ( 'NONE',  ( -84.20019048342901158, 24.50704008690495428, 86.53502039815329283 ) ) ;
#33312 = CARTESIAN_POINT ( 'NONE',  ( -4.250000000000000000, 5.204748896376250699E-16, -9.500000000000000000 ) ) ;
#33313 = CARTESIAN_POINT ( 'NONE',  ( 133.4058733589413066, 42.32720528873923627, 29.51034083899532590 ) ) ;
#33314 = CARTESIAN_POINT ( 'NONE',  ( 8.000000000000007105, 249.8719672152120381, 94.99999999999866418 ) ) ;
#33315 = AXIS2_PLACEMENT_3D ( 'NONE', #62463, #58214, #63497 ) ;
#33316 = DIRECTION ( 'NONE',  ( -0.000000000000000000, 1.000000000000000000, -0.000000000000000000 ) ) ;
#33317 = DIRECTION ( 'NONE',  ( -0.9989930665413144784, -0.04486483035051863633, 2.500042656554809847E-16 ) ) ;
#33318 = AXIS2_PLACEMENT_3D ( 'NONE', #17029, #39552, #38499 ) ;
#33319 = DIRECTION ( 'NONE',  ( -0.000000000000000000, -0.000000000000000000, -1.000000000000000000 ) ) ;
#33320 = DIRECTION ( 'NONE',  ( -0.5508969814521065267, 0.8345732537212999791, 0.000000000000000000 ) ) ;
#33321 = DIRECTION ( 'NONE',  ( -1.000000000000000000, 0.000000000000000000, 0.000000000000000000 ) ) ;
#33322 = ORIENTED_EDGE ( 'NONE', *, *, #3794, .T. ) ;
#33323 = VERTEX_POINT ( 'NONE', #56490 ) ;
#33324 = CARTESIAN_POINT ( 'NONE',  ( 56.52205390515079131, 12.28646189164058988, 67.94243928922777798 ) ) ;
#33325 = DIRECTION ( 'NONE',  ( -1.000000000000000000, 0.000000000000000000, 0.000000000000000000 ) ) ;
#33326 = DIRECTION ( 'NONE',  ( 0.000000000000000000, 0.000000000000000000, -1.000000000000000000 ) ) ;
#33327 = CARTESIAN_POINT ( 'NONE',  ( -23.03840347525633447, -9.707315041312391202, 0.000000000000000000 ) ) ;
#33328 = CARTESIAN_POINT ( 'NONE',  ( 6.800000000000000711, 0.000000000000000000, 0.000000000000000000 ) ) ;
#33329 = CARTESIAN_POINT ( 'NONE',  ( 87.30556659420746257, 20.71715946144239950, 83.42470827707606418 ) ) ;
#33330 = VECTOR ( 'NONE', #26037, 1000.000000000000000 ) ;
#33331 = ORIENTED_EDGE ( 'NONE', *, *, #2380, .F. ) ;
#33332 = DIRECTION ( 'NONE',  ( 1.000000000000000000, 9.950807539071918675E-15, 9.950807539071956540E-15 ) ) ;
#33333 = CYLINDRICAL_SURFACE ( 'NONE', #43032, 5.000000000000018652 ) ;
#33334 = CARTESIAN_POINT ( 'NONE',  ( -127.6861178856153174, 47.68458428355327072, 18.57198835803803050 ) ) ;
#33335 = CARTESIAN_POINT ( 'NONE',  ( -125.8938041572051389, -170.0000000000000000, 3.775397282693376155 ) ) ;
#33336 = ITEM_DEFINED_TRANSFORMATION ( 'NONE', 'NONE', #34433,  #66832 ) ;
#33337 = CARTESIAN_POINT ( 'NONE',  ( -133.2787743207941276, 52.78950725740544669, -41.07782338636832975 ) ) ;
#33338 = ORIENTED_EDGE ( 'NONE', *, *, #41605, .F. ) ;
#33339 = CARTESIAN_POINT ( 'NONE',  ( -119.5576859660651508, 42.46117483543971360, -46.43479381264184980 ) ) ;
#33340 = CARTESIAN_POINT ( 'NONE',  ( 0.000000000000000000, 0.000000000000000000, 0.000000000000000000 ) ) ;
#33341 = CARTESIAN_POINT ( 'NONE',  ( -419.7337897053568554, 394.9999999999998863, -113.5207719538772579 ) ) ;
#33342 = CARTESIAN_POINT ( 'NONE',  ( -6.843910203392210789, 7.836697961436722260, -62.31111058179082818 ) ) ;
#33343 = PLANE ( 'NONE',  #15576 ) ;
#33344 = ORIENTED_EDGE ( 'NONE', *, *, #68283, .F. ) ;
#33345 = CARTESIAN_POINT ( 'NONE',  ( 163.8779926341230748, 64.12131166777415103, -93.39151763476601786 ) ) ;
#33346 = CARTESIAN_POINT ( 'NONE',  ( 197.6145711261845008, 97.10888456119690204, -46.37243094951851674 ) ) ;
#33347 = B_SPLINE_CURVE_WITH_KNOTS ( 'NONE', 3,
 ( #11566, #47911, #54478, #28461 ),
 .UNSPECIFIED., .F., .F.,
 ( 4, 4 ),
 ( 0.1259919275528358640, 0.1829744153748747437 ),
 .UNSPECIFIED. ) ;
#33348 = CARTESIAN_POINT ( 'NONE',  ( -101.3502439362134879, 33.43728945125134544, 30.56238026629964466 ) ) ;
#33349 = CARTESIAN_POINT ( 'NONE',  ( 22.80839748737787787, 6.826915557457470030, -45.67001842980409521 ) ) ;
#33351 = ORIENTED_EDGE ( 'NONE', *, *, #51773, .F. ) ;
#33350 = CARTESIAN_POINT ( 'NONE',  ( 113.4402889550712672, 31.50582881646777622, 17.06772458018410177 ) ) ;
#33352 = CARTESIAN_POINT ( 'NONE',  ( -10.96274578891778084, 22.46815979931508167, 0.000000000000000000 ) ) ;
#33353 = ADVANCED_FACE ( 'NONE', ( #40278 ), #23755, .F. ) ;
#33354 = ORIENTED_EDGE ( 'NONE', *, *, #20149, .T. ) ;
#33355 = VERTEX_POINT ( 'NONE', #7228 ) ;
#33356 = AXIS2_PLACEMENT_3D ( 'NONE', #45056, #29574, #17993 ) ;
#33357 = DIRECTION ( 'NONE',  ( 1.000000000000000000, 0.000000000000000000, 0.000000000000000000 ) ) ;
#33358 = EDGE_CURVE ( 'NONE', #22095, #32423, #66342, .T. ) ;
#33359 = CARTESIAN_POINT ( 'NONE',  ( -35.47785446961778177, 11.31170061832250973, -90.17238499101478055 ) ) ;
#33360 = VECTOR ( 'NONE', #32961, 1000.000000000000000 ) ;
#33362 = ORIENTED_EDGE ( 'NONE', *, *, #60960, .T. ) ;
#33361 = CARTESIAN_POINT ( 'NONE',  ( -10.24974837193994581, 8.069704751038630164, -62.64850511569373737 ) ) ;
#33363 = DIRECTION ( 'NONE',  ( 0.6234898018587431423, -0.7818314824680220321, 0.000000000000000000 ) ) ;
#33364 = EDGE_CURVE ( 'NONE', #8399, #21982, #24459, .T. ) ;
#33365 = LINE ( 'NONE', #49863, #46408 ) ;
#33366 = DIRECTION ( 'NONE',  ( -0.000000000000000000, 1.000000000000000000, -0.000000000000000000 ) ) ;
#33367 = AXIS2_PLACEMENT_3D ( 'NONE', #52188, #56783, #24436 ) ;
#33368 = VERTEX_POINT ( 'NONE', #29043 ) ;
#33369 = AXIS2_PLACEMENT_3D ( 'NONE', #63669, #54108, #5934 ) ;
#33370 = DIRECTION ( 'NONE',  ( 1.000000000000000000, 0.000000000000000000, 0.000000000000000000 ) ) ;
#33371 = AXIS2_PLACEMENT_3D ( 'NONE', #33003, #32319, #65725 ) ;
#33372 = CARTESIAN_POINT ( 'NONE',  ( -38.92726670956013635, 10.94099576009806718, -16.46139659267618427 ) ) ;
#33373 = CARTESIAN_POINT ( 'NONE',  ( -174.7903139851460423, 90.53182997092832807, 45.64566177438910444 ) ) ;
#33374 = CARTESIAN_POINT ( 'NONE',  ( 0.000000000000000000, 0.000000000000000000, 0.000000000000000000 ) ) ;
#33375 = CARTESIAN_POINT ( 'NONE',  ( 20.74185656603722450, 7.717159106492281317, 58.70619541278092157 ) ) ;
#33376 = EDGE_CURVE ( 'NONE', #58488, #66136, #5562, .T. ) ;
#33378 = ORIENTED_EDGE ( 'NONE', *, *, #26592, .T. ) ;
#33377 = B_SPLINE_CURVE_WITH_KNOTS ( 'NONE', 3,
 ( #37540, #69206, #48415, #21706, #31579, #4842, #21362, #42809, #16441, #956, #64277, #58991, #64626, #603, #11152, #47742, #15746, #37195, #53359, #17112, #11487, #53015, #37895, #59675, #26312, #59340, #54398, #5869, #32617, #5195, #22408, #32960, #21030, #43155, #42475, #26650, #248, #48085, #54044, #43848, #22059, #27325, #63935, #58640, #48766 ),
 .UNSPECIFIED., .F., .F.,
 ( 4, 2, 2, 1, 2, 2, 2, 2, 2, 2, 2, 2, 2, 2, 2, 2, 2, 2, 2, 2, 2, 2, 4 ),
 ( 0.02348395315094740227, 0.02495010856601299204, 0.02568318627354578693, 0.02641626398107858181, 0.02714934168861137670, 0.02788241939614417159, 0.02934857481120974748, 0.03008165251874254584, 0.03081473022627534419, 0.03228088564134092009, 0.03301396334887372191, 0.03374704105640652374, 0.03521319647147211351, 0.03667935188653771716, 0.03741242959407050511, 0.03814550730160329306, 0.03961166271666886896, 0.04107781813173444485, 0.04254397354680002075, 0.04327705125433281563, 0.04401012896186559664, 0.04547628437693117254, 0.04694243979199674843 ),
 .UNSPECIFIED. ) ;
#33379 = VERTEX_POINT ( 'NONE', #68396 ) ;
#33380 = ORIENTED_EDGE ( 'NONE', *, *, #57132, .T. ) ;
#33381 = DIRECTION ( 'NONE',  ( 1.000000000000000000, 0.000000000000000000, -0.000000000000000000 ) ) ;
#33382 = CARTESIAN_POINT ( 'NONE',  ( -104.7956873821848944, 35.21322275870666374, 4.105111570260970844 ) ) ;
#33383 = CARTESIAN_POINT ( 'NONE',  ( -35.38560449531984631, 10.27249159032102099, -49.19954030868971984 ) ) ;
#33384 = DIRECTION ( 'NONE',  ( -0.000000000000000000, 1.000000000000000000, -0.000000000000000000 ) ) ;
#33385 = DIRECTION ( 'NONE',  ( 1.000000000000000000, 0.000000000000000000, -2.921639538487254261E-16 ) ) ;
#33386 = CARTESIAN_POINT ( 'NONE',  ( 260.0716287634991204, 189.9999999999999432, -91.28179539054374914 ) ) ;
#33387 = CARTESIAN_POINT ( 'NONE',  ( -71.17846906053300415, 20.67346400882179935, -16.26539829717355801 ) ) ;
#33388 = CARTESIAN_POINT ( 'NONE',  ( 81.04675113612957205, 17.59091904316105826, 69.08915744240043466 ) ) ;
#33389 = ORIENTED_EDGE ( 'NONE', *, *, #37546, .F. ) ;
#33390 = CARTESIAN_POINT ( 'NONE',  ( -4.999999999999971578, 15.55634918610403084, 85.00100000000000477 ) ) ;
#33391 = DIRECTION ( 'NONE',  ( -0.000000000000000000, -1.000000000000000000, -0.000000000000000000 ) ) ;
#33392 = CARTESIAN_POINT ( 'NONE',  ( 207.4867844023103487, 110.2451255333963474, -63.69630056086449343 ) ) ;
#33393 = DIRECTION ( 'NONE',  ( 0.000000000000000000, 0.000000000000000000, -1.000000000000000000 ) ) ;
#33394 = CARTESIAN_POINT ( 'NONE',  ( -71.21970990337015905, 19.62334883444992428, 10.04748825087579434 ) ) ;
#33395 = CARTESIAN_POINT ( 'NONE',  ( -118.4470345550925714, 42.96051736048244152, 63.92217194901178345 ) ) ;
#33396 = CARTESIAN_POINT ( 'NONE',  ( -49.62489392740901906, 13.29305723289024499, 5.791284796356666043 ) ) ;
#33397 = CARTESIAN_POINT ( 'NONE',  ( 0.3194001229790404128, 3.115132258388582542, -8.000000000000000000 ) ) ;
#33398 = CARTESIAN_POINT ( 'NONE',  ( -3.318518101603030068, -7.321656987762886537, -9.499999999999994671 ) ) ;
#33399 = ORIENTED_EDGE ( 'NONE', *, *, #36290, .T. ) ;
#33400 = CIRCLE ( 'NONE', #26663, 24.99999999999985434 ) ;
#33401 = DIRECTION ( 'NONE',  ( 0.000000000000000000, -1.000000000000000000, 0.000000000000000000 ) ) ;
#33402 = CARTESIAN_POINT ( 'NONE',  ( -190.6985136298601731, 109.1272424661242582, 87.66052266422059347 ) ) ;
#33403 = ORIENTED_EDGE ( 'NONE', *, *, #37677, .T. ) ;
#33404 = FACE_OUTER_BOUND ( 'NONE', #12919, .T. ) ;
#33405 = CARTESIAN_POINT ( 'NONE',  ( -1.118033988749894458, 0.000000000000000000, 0.000000000000000000 ) ) ;
#33406 = ORIENTED_EDGE ( 'NONE', *, *, #68760, .F. ) ;
#33407 = CARTESIAN_POINT ( 'NONE',  ( -82.32931163805224628, 23.75065981441939655, 31.36902022954703995 ) ) ;
#33408 = CARTESIAN_POINT ( 'NONE',  ( -27.49195330402087833, 9.993776132065308460, -76.04372912499586334 ) ) ;
#33409 = CARTESIAN_POINT ( 'NONE',  ( 46.23304607317103176, 10.41544405387738514, 34.30787760119516605 ) ) ;
#33410 = CARTESIAN_POINT ( 'NONE',  ( -29.04258984626622819, 9.210213971636685315, 57.44998931435969780 ) ) ;
#33411 = CARTESIAN_POINT ( 'NONE',  ( -146.1142527948576060, 61.35394402951020254, 18.06864745197337285 ) ) ;
#33412 = VECTOR ( 'NONE', #3907, 1000.000000000000000 ) ;
#33413 = ORIENTED_EDGE ( 'NONE', *, *, #67973, .F. ) ;
#33414 = VERTEX_POINT ( 'NONE', #35702 ) ;
#33415 = DIRECTION ( 'NONE',  ( -0.3930250316539148359, -0.9195277725514544587, 0.000000000000000000 ) ) ;
#33416 = EDGE_LOOP ( 'NONE', ( #50860, #68782, #16368, #28426 ) ) ;
#33417 = CARTESIAN_POINT ( 'NONE',  ( 31.91383250562745388, 8.564461488296997160, -15.78690365252851535 ) ) ;
#33418 = CARTESIAN_POINT ( 'NONE',  ( -68.06184294702700299, -31.38946074233465211, 41.38025477438755928 ) ) ;
#33419 = EDGE_CURVE ( 'NONE', #21145, #18591, #46234, .T. ) ;
#33420 = CARTESIAN_POINT ( 'NONE',  ( 140.1490313966874908, 46.55482389929059650, 86.60343140016868801 ) ) ;
#33421 = VECTOR ( 'NONE', #38018, 1000.000000000000000 ) ;
#33422 = CARTESIAN_POINT ( 'NONE',  ( 197.6319840686292082, 98.73992647122672395, -95.00000000000133582 ) ) ;
#33423 = CARTESIAN_POINT ( 'NONE',  ( 61.62594073580572740, -21.79346734964916266, 41.38025477438755928 ) ) ;
#33424 = EDGE_CURVE ( 'NONE', #44801, #24394, #52552, .T. ) ;
#33425 = AXIS2_PLACEMENT_3D ( 'NONE', #64151, #27552, #11369 ) ;
#33426 = ORIENTED_EDGE ( 'NONE', *, *, #53257, .T. ) ;
#33427 = CARTESIAN_POINT ( 'NONE',  ( -120.1497954511983721, 42.82624472369558788, -74.10732019003926041 ) ) ;
#33428 = ORIENTED_EDGE ( 'NONE', *, *, #5268, .T. ) ;
#33429 = ORIENTED_EDGE ( 'NONE', *, *, #64103, .T. ) ;
#33430 = CARTESIAN_POINT ( 'NONE',  ( 10.55634918610396511, -46.66904755831214402, 2.000000000000000000 ) ) ;
#33431 = DIRECTION ( 'NONE',  ( -1.000000000000000000, 0.000000000000000000, 0.000000000000000000 ) ) ;
#33432 = DIRECTION ( 'NONE',  ( -1.850371928290090422E-16, 1.000000000000000000, 1.110223024625156171E-16 ) ) ;
#33433 = CARTESIAN_POINT ( 'NONE',  ( 136.7507824285648894, 44.38599729999915411, 17.08875733851226997 ) ) ;
#33434 = CARTESIAN_POINT ( 'NONE',  ( -13.24252603915608617, 63.63674649211943546, 170.0000000000000000 ) ) ;
#33435 = VERTEX_POINT ( 'NONE', #8964 ) ;
#33436 = EDGE_CURVE ( 'NONE', #29969, #48053, #14603, .T. ) ;
#33437 = DIRECTION ( 'NONE',  ( -1.000000000000000000, 0.000000000000000000, 0.000000000000000000 ) ) ;
#33438 = ORIENTED_EDGE ( 'NONE', *, *, #63141, .F. ) ;
#33439 = ADVANCED_FACE ( 'NONE', ( #26169 ), #9997, .T. ) ;
#33440 = CARTESIAN_POINT ( 'NONE',  ( 10.55634918610403084, 4.999999999999969802, 85.00100000000000477 ) ) ;
#33441 = ORIENTED_EDGE ( 'NONE', *, *, #11513, .T. ) ;
#33442 = CARTESIAN_POINT ( 'NONE',  ( 129.8795108792701569, 39.07419932312295430, -90.84173050637812707 ) ) ;
#33443 = EDGE_LOOP ( 'NONE', ( #56650, #56536 ) ) ;
#33444 = FACE_OUTER_BOUND ( 'NONE', #45481, .T. ) ;
#33445 = EDGE_CURVE ( 'NONE', #30796, #45847, #1109, .T. ) ;
#33446 = CARTESIAN_POINT ( 'NONE',  ( 90.91465859190772392, 20.92790537681857543, 4.207571972591185983 ) ) ;
#33447 = DIRECTION ( 'NONE',  ( -1.387778780781446169E-16, 1.000000000000000000, 3.469446951953615421E-17 ) ) ;
#33448 = EDGE_LOOP ( 'NONE', ( #13310, #55794, #66940, #1089 ) ) ;
#33449 = CIRCLE ( 'NONE', #51426, 5.000000000000004441 ) ;
#33450 = DIRECTION ( 'NONE',  ( 0.000000000000000000, 1.000000000000000000, 0.000000000000000000 ) ) ;
#33451 =( LENGTH_UNIT ( ) NAMED_UNIT ( * ) SI_UNIT ( .MILLI., .METRE. ) );
#33452 = AXIS2_PLACEMENT_3D ( 'NONE', #947, #31330, #22749 ) ;
#33453 = CARTESIAN_POINT ( 'NONE',  ( 32.89501968360929851, 8.663558833820822258, 41.17552703169613437 ) ) ;
#33454 = CARTESIAN_POINT ( 'NONE',  ( -178.5848962563133568, 94.99295350784007042, -37.04987916691930394 ) ) ;
#33455 = FACE_OUTER_BOUND ( 'NONE', #24898, .T. ) ;
#33456 = CARTESIAN_POINT ( 'NONE',  ( 16.78635691501517613, 0.000000000000000000, -41.68900338898716740 ) ) ;
#33457 = CARTESIAN_POINT ( 'NONE',  ( -417.6627218934913230, 399.9999999999998295, 78.55029585798814651 ) ) ;
#33458 = EDGE_CURVE ( 'NONE', #7475, #28498, #50524, .T. ) ;
#33459 = VERTEX_POINT ( 'NONE', #114 ) ;
#33460 = CARTESIAN_POINT ( 'NONE',  ( 140.0820590176526252, 46.51134312115247127, -74.55802468919154080 ) ) ;
#33461 = VECTOR ( 'NONE', #66656, 1000.000000000000227 ) ;
#33462 = CARTESIAN_POINT ( 'NONE',  ( 26.11269837220809364, 15.55634918610396866, 85.00100000000000477 ) ) ;
#33463 = EDGE_LOOP ( 'NONE', ( #51270, #62486 ) ) ;
#33464 = ADVANCED_FACE ( 'NONE', ( #5051 ), #38451, .T. ) ;
#33465 = ADVANCED_FACE ( 'NONE', ( #54618 ), #32826, .F. ) ;
#33466 = FACE_BOUND ( 'NONE', #22016, .T. ) ;
#33467 = AXIS2_PLACEMENT_3D ( 'NONE', #28955, #24016, #66254 ) ;
#33468 = CARTESIAN_POINT ( 'NONE',  ( -0.3249717932738296899, 6.518578686837487979, -69.27445299358225839 ) ) ;
#33469 = FILL_AREA_STYLE ('',( #43986 ) ) ;
#33470 = CARTESIAN_POINT ( 'NONE',  ( -144.3939084932120807, 61.25241660819418144, -9.976470740476594656 ) ) ;
#33471 = CARTESIAN_POINT ( 'NONE',  ( -125.8938041572051389, 47.69968343338778283, -49.91370389823397602 ) ) ;
#33472 = CARTESIAN_POINT ( 'NONE',  ( -2.869721780807576561, 7.625909776230886727, 43.26631488255254254 ) ) ;
#33473 = CARTESIAN_POINT ( 'NONE',  ( 5.799999999999999822, 4.618802153517004960, 7.999999999999998224 ) ) ;
#33474 = CARTESIAN_POINT ( 'NONE',  ( 113.7669346082183495, 21.75174821959686255, 3.303877464828373078 ) ) ;
#33475 = CARTESIAN_POINT ( 'NONE',  ( -7.330587818645180498, 7.867004275019543691, -8.573520141480125645 ) ) ;
#33476 = CARTESIAN_POINT ( 'NONE',  ( -14.93280618462406828, 8.469244267267917792, 40.02294218869200648 ) ) ;
#33477 = CARTESIAN_POINT ( 'NONE',  ( 117.0065308422768453, 32.13872219870569324, 7.015794843079218523 ) ) ;
#33478 = CARTESIAN_POINT ( 'NONE',  ( 410.0000000000000000, 2.000000000000001776, -90.00000000000000000 ) ) ;
#33479 = VERTEX_POINT ( 'NONE', #32137 ) ;
#33480 = DIRECTION ( 'NONE',  ( 1.387778780781446169E-16, -1.000000000000000000, -3.469446951953615421E-17 ) ) ;
#33481 = EDGE_LOOP ( 'NONE', ( #50958, #66320, #42674, #36788 ) ) ;
#33482 = PLANE ( 'NONE',  #13825 ) ;
#33483 = CARTESIAN_POINT ( 'NONE',  ( 86.62931800182293784, 20.48449268398423939, -77.66611478937542756 ) ) ;
#33484 = CARTESIAN_POINT ( 'NONE',  ( 102.7475671010530220, 26.65887778672039587, 90.36044456738673603 ) ) ;
#33485 = DIRECTION ( 'NONE',  ( 0.000000000000000000, 0.000000000000000000, 1.000000000000000000 ) ) ;
#33486 = CARTESIAN_POINT ( 'NONE',  ( -15.14442107647020563, 7.478650287766785532, 89.63505923903740324 ) ) ;
#33487 = CARTESIAN_POINT ( 'NONE',  ( -26.88234027341226096, 9.904106450608203716, -48.79416700654920902 ) ) ;
#33488 = CYLINDRICAL_SURFACE ( 'NONE', #49003, 7.500000000000013323 ) ;
#33489 = CARTESIAN_POINT ( 'NONE',  ( -72.44920908684991900, 21.11636224409796370, -92.10391607065253083 ) ) ;
#33490 = LINE ( 'NONE', #34183, #55462 ) ;
#33491 = ORIENTED_EDGE ( 'NONE', *, *, #16721, .F. ) ;
#33492 = ORIENTED_EDGE ( 'NONE', *, *, #13101, .F. ) ;
#33493 = CARTESIAN_POINT ( 'NONE',  ( 31.90247004928964358, 8.563336936370815167, 63.75499471202854096 ) ) ;
#33494 = CARTESIAN_POINT ( 'NONE',  ( 26.12852347772543737, 70.00000000000000000, 129.5802547743875550 ) ) ;
#33495 = CARTESIAN_POINT ( 'NONE',  ( -61.29635759142615115, 21.66977272663494958, 170.0000000000000000 ) ) ;
#33496 = CARTESIAN_POINT ( 'NONE',  ( -167.0073208999198755, 82.02183861952781285, 60.81400106796706240 ) ) ;
#33497 = FACE_OUTER_BOUND ( 'NONE', #24272, .T. ) ;
#33498 = CARTESIAN_POINT ( 'NONE',  ( -46.66904755831212981, -10.55634918610397222, 0.000000000000000000 ) ) ;
#33499 = EDGE_LOOP ( 'NONE', ( #10904, #11007 ) ) ;
#33500 = CARTESIAN_POINT ( 'NONE',  ( 94.11595392909971736, 23.18887043179185170, 10.88183017804118435 ) ) ;
#33501 = CARTESIAN_POINT ( 'NONE',  ( 23.09590709048884349, 7.852755081912510704, -41.31320969520013620 ) ) ;
#33502 = CARTESIAN_POINT ( 'NONE',  ( -86.10361028793438720, 25.29528064050656866, -16.77258119596484320 ) ) ;
#33503 = CARTESIAN_POINT ( 'NONE',  ( -81.96414466956503020, 24.68804580838119733, -89.55477965345060909 ) ) ;
#33504 = FACE_OUTER_BOUND ( 'NONE', #15986, .T. ) ;
#33505 = CARTESIAN_POINT ( 'NONE',  ( 209.5118425285948831, 113.1852661712287471, -11.22590986498565790 ) ) ;
#33506 = ADVANCED_FACE ( 'NONE', ( #15615 ), #64841, .F. ) ;
#33507 = FACE_BOUND ( 'NONE', #44068, .T. ) ;
#33508 = CARTESIAN_POINT ( 'NONE',  ( -62.15324028806258383, 16.70091357159900980, -40.25091533774048003 ) ) ;
#33509 = AXIS2_PLACEMENT_3D ( 'NONE', #31413, #31078, #9616 ) ;
#33510 = EDGE_CURVE ( 'NONE', #39103, #49065, #33662, .T. ) ;
#33511 = VERTEX_POINT ( 'NONE', #59889 ) ;
#33512 = CIRCLE ( 'NONE', #58198, 21.99999999999998579 ) ;
#33513 = CARTESIAN_POINT ( 'NONE',  ( 132.0249343950657135, 41.49728247212333798, 17.49763525730703506 ) ) ;
#33514 = LINE ( 'NONE', #6053, #32749 ) ;
#33515 = LINE ( 'NONE', #6761, #38630 ) ;
#33516 = FACE_OUTER_BOUND ( 'NONE', #26408, .T. ) ;
#33517 = CARTESIAN_POINT ( 'NONE',  ( 154.0293889979056701, 55.02370422818217577, 3.384461364915644754 ) ) ;
#33518 = CARTESIAN_POINT ( 'NONE',  ( -1.224646799147352468E-15, 16.00000000000000000, 6.196318915105386793 ) ) ;
#33519 = AXIS2_PLACEMENT_3D ( 'NONE', #43718, #38818, #54978 ) ;
#33520 = EDGE_LOOP ( 'NONE', ( #48650, #60012, #41861, #25296 ) ) ;
#33522 = ADVANCED_FACE ( 'NONE', ( #37751 ), #64491, .T. ) ;
#33521 = DIRECTION ( 'NONE',  ( -1.000000000000000000, 0.000000000000000000, 0.000000000000000000 ) ) ;
#33523 = DIRECTION ( 'NONE',  ( -1.000000000000000000, 0.000000000000000000, 0.000000000000000000 ) ) ;
#33524 = ORIENTED_EDGE ( 'NONE', *, *, #39470, .F. ) ;
#33525 = ADVANCED_FACE ( 'NONE', ( #16302 ), #59540, .F. ) ;
#33526 = AXIS2_PLACEMENT_3D ( 'NONE', #47898, #27839, #10963 ) ;
#33527 = EDGE_LOOP ( 'NONE', ( #35583, #45930, #54888, #18130 ) ) ;
#33528 = CARTESIAN_POINT ( 'NONE',  ( -27.00000000000000355, 26.99999999999999645, 12.00000000000000000 ) ) ;
#33529 = LINE ( 'NONE', #56017, #62324 ) ;
#33530 = CARTESIAN_POINT ( 'NONE',  ( 106.6228877857910788, 27.24245963308693419, 43.69709372667754366 ) ) ;
#33531 = VERTEX_POINT ( 'NONE', #47953 ) ;
#33532 = EDGE_CURVE ( 'NONE', #8631, #50694, #52757, .T. ) ;
#33533 = VERTEX_POINT ( 'NONE', #65186 ) ;
#33534 = CARTESIAN_POINT ( 'NONE',  ( -7.825402957745087207, -170.0000000000000000, 45.11558103944722120 ) ) ;
#33535 = CARTESIAN_POINT ( 'NONE',  ( 162.8034185388970911, 63.22443559329414597, 31.61437189098316480 ) ) ;
#33536 = PLANE ( 'NONE',  #68704 ) ;
#33537 = CARTESIAN_POINT ( 'NONE',  ( -742.9236288613935812, -685.7537703392392814, 10.00000000000000000 ) ) ;
#33538 = CARTESIAN_POINT ( 'NONE',  ( 4.339467034331195627, 6.732211846623388674, -9.500000000000003553 ) ) ;
#33539 = CARTESIAN_POINT ( 'NONE',  ( -49.43836229152576323, 14.28302414152159727, -47.71376574487467792 ) ) ;
#33540 = CARTESIAN_POINT ( 'NONE',  ( -49.44484229820454857, 14.28460989390479341, 15.97695875002632881 ) ) ;
#33541 = CARTESIAN_POINT ( 'NONE',  ( -128.9863978264384912, 49.78205252558954896, -8.732497812272862703 ) ) ;
#33542 = CARTESIAN_POINT ( 'NONE',  ( 0.000000000000000000, 0.000000000000000000, 41.38025477438755928 ) ) ;
#33543 = CARTESIAN_POINT ( 'NONE',  ( 70.05403699894507952, 14.41597870224753208, -94.18588356900310998 ) ) ;
#33544 = DIRECTION ( 'NONE',  ( -0.2225209339563184452, 0.9749279121818226201, 0.000000000000000000 ) ) ;
#33546 = ORIENTED_EDGE ( 'NONE', *, *, #47955, .F. ) ;
#33545 = DIRECTION ( 'NONE',  ( -0.000000000000000000, -0.000000000000000000, -1.000000000000000000 ) ) ;
#33547 = ORIENTED_EDGE ( 'NONE', *, *, #43310, .F. ) ;
#33548 = ADVANCED_FACE ( 'NONE', ( #37067 ), #42348, .F. ) ;
#33549 = EDGE_CURVE ( 'NONE', #476, #2404, #42626, .T. ) ;
#33550 = ORIENTED_EDGE ( 'NONE', *, *, #2246, .T. ) ;
#33551 = CARTESIAN_POINT ( 'NONE',  ( -13.47680110791658237, 7.324966777230637049, -21.02899547893517607 ) ) ;
#33552 = CARTESIAN_POINT ( 'NONE',  ( -167.7367320859366941, 82.78554475141790192, 86.78082447994947302 ) ) ;
#33553 = CARTESIAN_POINT ( 'NONE',  ( -47.61380558691495679, 12.81230778489787880, -14.88474268100918607 ) ) ;
#33554 = CARTESIAN_POINT ( 'NONE',  ( -5.066666666666671759, 8.000000000000000000, -11.86666666666666536 ) ) ;
#33555 = EDGE_CURVE ( 'NONE', #7326, #18961, #58507, .T. ) ;
#33556 = CARTESIAN_POINT ( 'NONE',  ( -62.50103539982530521, 17.85731685071835173, -43.72722077931214812 ) ) ;
#33557 = CARTESIAN_POINT ( 'NONE',  ( -61.36325649057843634, 43.03793052543095854, 41.38025477438755928 ) ) ;
#33558 = VECTOR ( 'NONE', #20688, 1000.000000000000000 ) ;
#33559 = CARTESIAN_POINT ( 'NONE',  ( 50.98853755884148597, 388.0000000000071054, 96.05029585798814651 ) ) ;
#33560 = DIRECTION ( 'NONE',  ( 0.000000000000000000, 0.000000000000000000, -1.000000000000000000 ) ) ;
#33561 = VERTEX_POINT ( 'NONE', #824 ) ;
#33562 = CARTESIAN_POINT ( 'NONE',  ( 109.9975424824652634, 295.6904194069557548, 539.5330678552892323 ) ) ;
#33563 = EDGE_LOOP ( 'NONE', ( #69427, #56370, #19780, #21316 ) ) ;
#33564 = ORIENTED_EDGE ( 'NONE', *, *, #12225, .F. ) ;
#33565 = AXIS2_PLACEMENT_3D ( 'NONE', #44127, #6151, #32548 ) ;
#33566 = DIRECTION ( 'NONE',  ( 0.000000000000000000, 0.000000000000000000, -1.000000000000000000 ) ) ;
#33567 = SURFACE_STYLE_USAGE ( .BOTH. , #17004 ) ;
#33568 = CARTESIAN_POINT ( 'NONE',  ( -29.23649411797835995, 10.25826775638764943, 84.22912791894023599 ) ) ;
#33569 = CARTESIAN_POINT ( 'NONE',  ( -94.79534239005252516, 29.13842790650044279, -43.05777683239141140 ) ) ;
#33570 =( GEOMETRIC_REPRESENTATION_CONTEXT ( 3 ) GLOBAL_UNCERTAINTY_ASSIGNED_CONTEXT ( ( #60643 ) ) GLOBAL_UNIT_ASSIGNED_CONTEXT ( ( #59043, #43203, #21759 ) ) REPRESENTATION_CONTEXT ( 'NONE', 'WORKASPACE' ) );
#33571 = CARTESIAN_POINT ( 'NONE',  ( 7.533997733929802543, -64.93035244659006366, 41.38025477438755928 ) ) ;
#33572 = CARTESIAN_POINT ( 'NONE',  ( 0.000000000000000000, 0.000000000000000000, 5.000000000000000000 ) ) ;
#33573 = CARTESIAN_POINT ( 'NONE',  ( 136.9654665832767932, 44.52067472585215313, -9.849378322202888114 ) ) ;
#33574 = ORIENTED_EDGE ( 'NONE', *, *, #56822, .T. ) ;
#33575 = EDGE_LOOP ( 'NONE', ( #16044, #57389 ) ) ;
#33576 = ORIENTED_EDGE ( 'NONE', *, *, #22711, .T. ) ;
#33577 = DIRECTION ( 'NONE',  ( -0.000000000000000000, -0.000000000000000000, -1.000000000000000000 ) ) ;
#33578 = CARTESIAN_POINT ( 'NONE',  ( -14.32241591711281714, 7.401556312061831733, 14.52592041517191035 ) ) ;
#33579 = DIRECTION ( 'NONE',  ( 0.000000000000000000, -1.000000000000000000, 0.000000000000000000 ) ) ;
#33580 = CARTESIAN_POINT ( 'NONE',  ( 56.30011474572733476, 11.21470186335419150, -19.72478589053048381 ) ) ;
#33581 = CARTESIAN_POINT ( 'NONE',  ( 259.4165763529819060, -27.00000000000000355, 138.9999999999999716 ) ) ;
#33582 = CARTESIAN_POINT ( 'NONE',  ( 0.000000000000000000, 2.755455298081544778E-15, -22.50000000000000000 ) ) ;
#33583 = ORIENTED_EDGE ( 'NONE', *, *, #53481, .F. ) ;
#33584 = DIRECTION ( 'NONE',  ( -1.000000000000000000, 0.000000000000000000, 0.000000000000000000 ) ) ;
#33585 = CARTESIAN_POINT ( 'NONE',  ( -157.0069704378501569, 70.81086990254190994, 65.64755214383821169 ) ) ;
#33586 = CARTESIAN_POINT ( 'NONE',  ( -0.5178428571329642960, 7.532057582089303871, -41.21203124799237116 ) ) ;
#33587 = CARTESIAN_POINT ( 'NONE',  ( 26.99999999999999645, 26.99999999999999645, 0.000000000000000000 ) ) ;
#33588 = DIRECTION ( 'NONE',  ( -1.000000000000000000, 0.000000000000000000, 0.000000000000000000 ) ) ;
#33589 = CARTESIAN_POINT ( 'NONE',  ( 32.06997139192793611, -56.95813133885440038, 43.58025477438756212 ) ) ;
#33590 = FACE_BOUND ( 'NONE', #10914, .T. ) ;
#33591 = DIRECTION ( 'NONE',  ( -1.000000000000000000, 0.000000000000000000, 0.000000000000000000 ) ) ;
#33592 = EDGE_CURVE ( 'NONE', #45368, #3161, #10326, .T. ) ;
#33593 = EDGE_LOOP ( 'NONE', ( #39521, #63928, #65761, #60754, #34653, #40843, #17737, #5753, #17597 ) ) ;
#33594 = DIRECTION ( 'NONE',  ( 1.000000000000000000, -0.000000000000000000, -0.000000000000000000 ) ) ;
#33595 = CARTESIAN_POINT ( 'NONE',  ( -132.2199390322348620, 50.80243550247267592, -65.19852263477184806 ) ) ;
#33596 = CARTESIAN_POINT ( 'NONE',  ( -103.2061297292849531, 34.38496953192503724, -76.81632396160040344 ) ) ;
#33597 = CARTESIAN_POINT ( 'NONE',  ( 45.90693067088658808, 9.344800815249323378, -66.19927155725260093 ) ) ;
#33598 = CARTESIAN_POINT ( 'NONE',  ( -18.89790202299208133, 62.20684691518606257, 3.061616997868437868E-16 ) ) ;
#33599 = ORIENTED_EDGE ( 'NONE', *, *, #4239, .F. ) ;
#33600 = ORIENTED_EDGE ( 'NONE', *, *, #62973, .F. ) ;
#33602 = EDGE_CURVE ( 'NONE', #46713, #38519, #48625, .T. ) ;
#33601 = CARTESIAN_POINT ( 'NONE',  ( -126.7195977354785867, 47.03939704596392346, -88.63674059282946871 ) ) ;
#33603 = CARTESIAN_POINT ( 'NONE',  ( 176.5082832158485360, 74.10150673151672152, 84.54631382975011888 ) ) ;
#33604 = ORIENTED_EDGE ( 'NONE', *, *, #14075, .F. ) ;
#33605 = EDGE_LOOP ( 'NONE', ( #12992, #1256, #46559, #44480, #63874, #5723 ) ) ;
#33606 = CARTESIAN_POINT ( 'NONE',  ( 175.8963338753314360, 73.51705463274393537, -38.30295033125676696 ) ) ;
#33607 = DIRECTION ( 'NONE',  ( 0.000000000000000000, 0.000000000000000000, 1.000000000000000000 ) ) ;
#33608 = EDGE_CURVE ( 'NONE', #13157, #25409, #68491, .T. ) ;
#33609 = DIRECTION ( 'NONE',  ( -0.000000000000000000, -0.000000000000000000, 1.000000000000000000 ) ) ;
#33610 = ORIENTED_EDGE ( 'NONE', *, *, #36250, .F. ) ;
#33612 = LINE ( 'NONE', #17407, #2026 ) ;
#33611 = CIRCLE ( 'NONE', #49291, 89.99999999999998579 ) ;
#33613 = VECTOR ( 'NONE', #19147, 1000.000000000000000 ) ;
#33614 = EDGE_CURVE ( 'NONE', #62679, #46362, #30294, .T. ) ;
#33615 = CARTESIAN_POINT ( 'NONE',  ( 140.4641697461913168, 46.75994457266056514, 67.44143240493572478 ) ) ;
#33616 = CARTESIAN_POINT ( 'NONE',  ( -78.19460645047367109, 22.14203592077027949, -50.11545063171791270 ) ) ;
#33617 = CARTESIAN_POINT ( 'NONE',  ( -27.00000000000000355, 26.99999999999999289, 15.00000000000000000 ) ) ;
#33618 = AXIS2_PLACEMENT_3D ( 'NONE', #18277, #61535, #24261 ) ;
#33619 = CARTESIAN_POINT ( 'NONE',  ( 88.53517449242353621, 20.08005703101045114, -36.06378951590050974 ) ) ;
#33620 = CARTESIAN_POINT ( 'NONE',  ( -48.34250119710922888, 14.01879126850789348, -19.23099893068116373 ) ) ;
#33621 = EDGE_LOOP ( 'NONE', ( #17613, #36413, #62866, #50306 ) ) ;
#33622 = CARTESIAN_POINT ( 'NONE',  ( 116.0773578185793298, 31.67580513411749621, -48.16155069270497080 ) ) ;
#33623 = CARTESIAN_POINT ( 'NONE',  ( -71.42546113164834765, 20.75891408601219368, 13.09244254408361741 ) ) ;
#33624 = CARTESIAN_POINT ( 'NONE',  ( -142.0729208125266894, 59.40063722436774896, -41.17521488854814748 ) ) ;
#33625 = CARTESIAN_POINT ( 'NONE',  ( 107.3013380801407521, 388.0000000000076739, 96.05029585798752123 ) ) ;
#33627 = VERTEX_POINT ( 'NONE', #54255 ) ;
#33626 = CARTESIAN_POINT ( 'NONE',  ( -121.3504824331598826, 43.57435154345014894, 85.83401817385978916 ) ) ;
#33628 = CARTESIAN_POINT ( 'NONE',  ( 55.76255201544532270, 12.13275766515751641, 8.496681876347771833 ) ) ;
#33629 = ORIENTED_EDGE ( 'NONE', *, *, #2977, .T. ) ;
#33630 = CARTESIAN_POINT ( 'NONE',  ( 6.400000000000000355, -4.618802153517012954, -8.000000000000001776 ) ) ;
#33631 = CARTESIAN_POINT ( 'NONE',  ( -55.05276343752909440, 14.68156374112638929, -23.37177340799619785 ) ) ;
#33632 = DIRECTION ( 'NONE',  ( -5.551115123125781716E-16, 0.000000000000000000, -1.000000000000000000 ) ) ;
#33633 = EDGE_CURVE ( 'NONE', #62233, #37433, #48981, .T. ) ;
#33634 = ADVANCED_FACE ( 'NONE', ( #33880 ), #6786, .T. ) ;
#33635 = CARTESIAN_POINT ( 'NONE',  ( 181.0840389613909736, 78.60582251573003987, -24.38050707541595230 ) ) ;
#33636 = CARTESIAN_POINT ( 'NONE',  ( 139.6359093656973585, 45.02518919224741012, -11.89209978307138904 ) ) ;
#33637 = DIRECTION ( 'NONE',  ( 0.000000000000000000, 0.000000000000000000, 1.000000000000000000 ) ) ;
#33638 = CARTESIAN_POINT ( 'NONE',  ( 93.33480479917545836, 21.81892021443993457, -66.76901901691363150 ) ) ;
#33639 = CARTESIAN_POINT ( 'NONE',  ( -28.14167211390615009, 9.073095087475770981, -89.75665694410322715 ) ) ;
#33640 = CARTESIAN_POINT ( 'NONE',  ( 2.005731055991735623, 188.0000000000000000, 0.000000000000000000 ) ) ;
#33641 = ORIENTED_EDGE ( 'NONE', *, *, #60011, .T. ) ;
#33642 = APPLICATION_CONTEXT ( 'automotive_design' ) ;
#33643 = VERTEX_POINT ( 'NONE', #17337 ) ;
#33644 = CARTESIAN_POINT ( 'NONE',  ( 42.49453823366106775, 8.831814337191479680, 44.25087953862465184 ) ) ;
#33645 = CARTESIAN_POINT ( 'NONE',  ( 0.4964154566687890013, 4.996589667937373136, 7.345652830558761615 ) ) ;
#33646 = CARTESIAN_POINT ( 'NONE',  ( 433.3728120124415568, 394.9999999999999432, 99.58582976392126795 ) ) ;
#33647 = VECTOR ( 'NONE', #30864, 1000.000000000000000 ) ;
#33648 = DIRECTION ( 'NONE',  ( -1.000000000000000000, 0.000000000000000000, 0.000000000000000000 ) ) ;
#33649 = CARTESIAN_POINT ( 'NONE',  ( 210.5008983495071959, 116.4753531594350733, -39.06839114615122099 ) ) ;
#33650 = CARTESIAN_POINT ( 'NONE',  ( 110.2429982417149290, 28.88204397445231209, -77.76698815611739235 ) ) ;
#33651 = CARTESIAN_POINT ( 'NONE',  ( -105.8879439778144587, 34.65133284149109727, 58.27111540278865931 ) ) ;
#33652 = CARTESIAN_POINT ( 'NONE',  ( -24.33435124463266419, 8.532637995283115728, -40.40188971294399778 ) ) ;
#33653 = DIRECTION ( 'NONE',  ( 0.5407162030609372616, -0.6444004775717707689, 0.5407162030609374836 ) ) ;
#33654 = ORIENTED_EDGE ( 'NONE', *, *, #27685, .T. ) ;
#33655 = CARTESIAN_POINT ( 'NONE',  ( -30.94745021534355800, 10.53010394565407637, 18.37190381572551345 ) ) ;
#33656 = ORIENTED_EDGE ( 'NONE', *, *, #64022, .T. ) ;
#33657 = CARTESIAN_POINT ( 'NONE',  ( -24.53636015449790264, 60.58612729876396941, 41.38025477438755928 ) ) ;
#33658 = DIRECTION ( 'NONE',  ( -0.000000000000000000, 1.000000000000000000, -0.000000000000000000 ) ) ;
#33659 = CARTESIAN_POINT ( 'NONE',  ( -1.333402737265964699, 0.000000000000000000, -9.910703160737465822 ) ) ;
#33660 = DIRECTION ( 'NONE',  ( 0.000000000000000000, 0.000000000000000000, 1.000000000000000000 ) ) ;
#33661 = LINE ( 'NONE', #38222, #23162 ) ;
#33662 = CIRCLE ( 'NONE', #17934, 65.00000000000000000 ) ;
#33663 = CARTESIAN_POINT ( 'NONE',  ( -102.2801239173131194, -170.0000000000000000, 30.51907450641510522 ) ) ;
#33664 = LINE ( 'NONE', #61759, #24804 ) ;
#33665 = VECTOR ( 'NONE', #41638, 1000.000000000000000 ) ;
#33666 = CARTESIAN_POINT ( 'NONE',  ( -166.2425995121691642, 81.22826102820870631, 94.99999999999866418 ) ) ;
#33667 = CARTESIAN_POINT ( 'NONE',  ( 209.0273569836735419, 112.4716286368275462, 84.24349562760866661 ) ) ;
#33668 = CARTESIAN_POINT ( 'NONE',  ( 0.000000000000000000, 70.00000000000000000, 0.000000000000000000 ) ) ;
#33669 = ORIENTED_EDGE ( 'NONE', *, *, #18421, .T. ) ;
#33670 = CARTESIAN_POINT ( 'NONE',  ( 55.52751777340357364, 12.08567914268656374, 64.64719063402279176 ) ) ;
#33671 = CARTESIAN_POINT ( 'NONE',  ( 0.000000000000000000, 0.000000000000000000, 0.000000000000000000 ) ) ;
#33672 = LINE ( 'NONE', #20245, #63439 ) ;
#33673 = EDGE_CURVE ( 'NONE', #49905, #65743, #17977, .T. ) ;
#33675 = EDGE_CURVE ( 'NONE', #41480, #46223, #28238, .T. ) ;
#33674 = CARTESIAN_POINT ( 'NONE',  ( -439.4229916354184411, 388.0000000000020464, 96.05029585799300662 ) ) ;
#33676 = CARTESIAN_POINT ( 'NONE',  ( 56.48035995027075273, 49.34540444547854321, 43.58025477438756212 ) ) ;
#33677 = CARTESIAN_POINT ( 'NONE',  ( 133.8566784816069060, 42.60093787723652525, -9.178760341931967659 ) ) ;
#33678 = EDGE_CURVE ( 'NONE', #12095, #17473, #55725, .T. ) ;
#33679 = ORIENTED_EDGE ( 'NONE', *, *, #63110, .F. ) ;
#33680 = DIRECTION ( 'NONE',  ( -0.9108602745606089179, -0.4127148655274876510, 7.475994222889548834E-15 ) ) ;
#33681 = VECTOR ( 'NONE', #37313, 1000.000000000000000 ) ;
#33682 = LINE ( 'NONE', #2020, #40791 ) ;
#33683 = LINE ( 'NONE', #37549, #36530 ) ;
#33684 = CARTESIAN_POINT ( 'NONE',  ( -165.7690020878297901, 80.74028011998679233, -43.72344623212075021 ) ) ;
#33685 = CARTESIAN_POINT ( 'NONE',  ( -165.6309143132208987, 79.16027303391220471, 91.58517648874418171 ) ) ;
#33686 = VERTEX_POINT ( 'NONE', #4295 ) ;
#33687 = CARTESIAN_POINT ( 'NONE',  ( -125.8938041572051105, 46.49392987655492959, -49.91370389823397602 ) ) ;
#33688 = PLANE ( 'NONE',  #49827 ) ;
#33689 = DIRECTION ( 'NONE',  ( 0.5128992774059071280, -0.8584487936018655452, 0.000000000000000000 ) ) ;
#33690 = CARTESIAN_POINT ( 'NONE',  ( -0.7211439451572416726, 7.539282923622936394, -67.34605877822407649 ) ) ;
#33691 = ADVANCED_FACE ( 'NONE', ( #29630 ), #30677, .F. ) ;
#33692 = DIRECTION ( 'NONE',  ( -0.000000000000000000, -0.000000000000000000, -1.000000000000000000 ) ) ;
#33693 = ORIENTED_EDGE ( 'NONE', *, *, #5184, .T. ) ;
#33694 = CARTESIAN_POINT ( 'NONE',  ( -61.76386578474846090, 17.63453064612501109, 7.588056654894035802 ) ) ;
#33695 = CARTESIAN_POINT ( 'NONE',  ( 198.8687991397276278, 98.67887821384414337, -48.55222848310017270 ) ) ;
#33696 = EDGE_CURVE ( 'NONE', #10168, #53714, #35951, .T. ) ;
#33697 = CARTESIAN_POINT ( 'NONE',  ( -95.86163447241558799, 30.75089131639703410, 34.10712415686030852 ) ) ;
#33698 = AXIS2_PLACEMENT_3D ( 'NONE', #22901, #12350, #38032 ) ;
#33699 = CARTESIAN_POINT ( 'NONE',  ( 22.81270948571150115, 6.827178363529887939, -40.37925852579917319 ) ) ;
#33701 = ORIENTED_EDGE ( 'NONE', *, *, #48713, .F. ) ;
#33700 = CARTESIAN_POINT ( 'NONE',  ( 111.1829448509513298, 30.43012797723691776, 17.72218487494545514 ) ) ;
#33702 = LINE ( 'NONE', #44225, #35086 ) ;
#33703 = EDGE_LOOP ( 'NONE', ( #21854, #52340, #18228, #65805 ) ) ;
#33704 = ORIENTED_EDGE ( 'NONE', *, *, #8735, .F. ) ;
#33705 = CARTESIAN_POINT ( 'NONE',  ( -71.37402418445427088, 19.67651958824263048, -17.54144548817878402 ) ) ;
#33706 = DIRECTION ( 'NONE',  ( 1.850169831522831466E-16, -1.000000000000000000, 5.551115123125781470E-17 ) ) ;
#33708 = EDGE_LOOP ( 'NONE', ( #37221, #10559, #22264, #4797 ) ) ;
#33707 = CARTESIAN_POINT ( 'NONE',  ( -13.29455179262033226, 8.319166883236668752, -74.90053121910786160 ) ) ;
#33709 = CARTESIAN_POINT ( 'NONE',  ( 164.4615316623334991, 63.29763980349832764, 34.18048905360906531 ) ) ;
#33710 = DIRECTION ( 'NONE',  ( 1.000000000000000000, 0.000000000000000000, 0.000000000000000000 ) ) ;
#33711 = VECTOR ( 'NONE', #7822, 1000.000000000000000 ) ;
#33712 = DIRECTION ( 'NONE',  ( 1.387778780781445922E-16, -1.000000000000000000, -1.232595164407830946E-32 ) ) ;
#33713 = EDGE_LOOP ( 'NONE', ( #58397, #2500 ) ) ;
#33714 = CYLINDRICAL_SURFACE ( 'NONE', #24392, 65.00000000000000000 ) ;
#33715 = CARTESIAN_POINT ( 'NONE',  ( -38.55214349681828168, 10.86754840574842262, -18.40125661905821630 ) ) ;
#33716 = CARTESIAN_POINT ( 'NONE',  ( 113.4402889550712530, 31.50582881646776912, 43.91227517064776009 ) ) ;
#33717 = CARTESIAN_POINT ( 'NONE',  ( -131.2955621888335713, 51.38237199780174080, 6.050075014823135255 ) ) ;
#33718 = CARTESIAN_POINT ( 'NONE',  ( 23.03546163277112413, 7.848986635155161373, 66.30567845553197515 ) ) ;
#33719 = ORIENTED_EDGE ( 'NONE', *, *, #5392, .T. ) ;
#33720 = ORIENTED_EDGE ( 'NONE', *, *, #47604, .T. ) ;
#33721 = VERTEX_POINT ( 'NONE', #8184 ) ;
#33722 = CARTESIAN_POINT ( 'NONE',  ( 211.0271454480929663, 115.4465235294104986, -93.48507865360365088 ) ) ;
#33723 = FACE_OUTER_BOUND ( 'NONE', #63549, .T. ) ;
#33724 = PLANE ( 'NONE',  #59390 ) ;
#33725 = CARTESIAN_POINT ( 'NONE',  ( -35.99019277275121453, 10.38248800679341954, -36.83593714842513123 ) ) ;
#33726 = CARTESIAN_POINT ( 'NONE',  ( -95.72254973812390233, 29.57223513374536594, 88.01148943108383094 ) ) ;
#33727 = DIRECTION ( 'NONE',  ( 0.6579387259397136978, -0.7530714660036099684, 5.102127870520022769E-18 ) ) ;
#33728 = CARTESIAN_POINT ( 'NONE',  ( -190.6985136298601731, 109.1272424661242582, -46.56223028809779407 ) ) ;
#33729 = CARTESIAN_POINT ( 'NONE',  ( -72.21889834709580214, 21.03534256744169539, -11.90770200485403940 ) ) ;
#33730 = EDGE_LOOP ( 'NONE', ( #69044, #61629, #55979, #9881, #59599, #26907, #13597, #65941, #23383, #10402, #50581, #53161 ) ) ;
#33731 = CYLINDRICAL_SURFACE ( 'NONE', #59053, 10.00000000000000178 ) ;
#33732 = VERTEX_POINT ( 'NONE', #25413 ) ;
#33733 = CARTESIAN_POINT ( 'NONE',  ( 32.46582151331404731, 7.608418548522502434, 40.29821503774315516 ) ) ;
#33734 =( LENGTH_UNIT ( ) NAMED_UNIT ( * ) SI_UNIT ( .MILLI., .METRE. ) );
#33735 = ORIENTED_EDGE ( 'NONE', *, *, #60585, .F. ) ;
#33736 = CARTESIAN_POINT ( 'NONE',  ( 188.2988323915788271, 86.21831227955478028, 38.87825967812030825 ) ) ;
#33737 = CARTESIAN_POINT ( 'NONE',  ( 6.375108774214766072E-14, 31.11269837220806167, 85.00100000000000477 ) ) ;
#33738 = DIRECTION ( 'NONE',  ( -0.000000000000000000, -0.000000000000000000, 1.000000000000000000 ) ) ;
#33739 = CARTESIAN_POINT ( 'NONE',  ( -51.35181696773307891, 13.72007042346227479, 4.431000077818415761 ) ) ;
#33740 = VECTOR ( 'NONE', #46529, 1000.000000000000000 ) ;
#33741 = LINE ( 'NONE', #6647, #20273 ) ;
#33742 = EDGE_CURVE ( 'NONE', #15020, #21961, #25753, .T. ) ;
#33743 = CARTESIAN_POINT ( 'NONE',  ( 163.1370549780984049, 63.50181104276889243, -75.40761482696586882 ) ) ;
#33744 = ORIENTED_EDGE ( 'NONE', *, *, #37619, .T. ) ;
#33745 = DIRECTION ( 'NONE',  ( 0.000000000000000000, -1.000000000000000000, 0.000000000000000000 ) ) ;
#33746 = CARTESIAN_POINT ( 'NONE',  ( 204.6977192012829789, -170.0000000000000000, -43.82593103262159673 ) ) ;
#33747 = ORIENTED_EDGE ( 'NONE', *, *, #34300, .T. ) ;
#33748 = FACE_OUTER_BOUND ( 'NONE', #3894, .T. ) ;
#33749 = DIRECTION ( 'NONE',  ( 0.7071067811865475727, 2.220446049250312341E-16, -0.7071067811865474617 ) ) ;
#33750 = DIRECTION ( 'NONE',  ( -0.000000000000000000, -1.000000000000000000, 0.000000000000000000 ) ) ;
#33751 = ORIENTED_EDGE ( 'NONE', *, *, #26684, .F. ) ;
#33752 = DIRECTION ( 'NONE',  ( -1.850169831522831466E-16, 1.000000000000000000, 1.110223024625156294E-16 ) ) ;
#33754 = EDGE_CURVE ( 'NONE', #38092, #59735, #63024, .T. ) ;
#33753 = CARTESIAN_POINT ( 'NONE',  ( -36.84489839129265931, -53.54860840895233309, 170.0000000000000000 ) ) ;
#33755 = CARTESIAN_POINT ( 'NONE',  ( 39.89582146299186860, 9.488756994579086168, 44.91383430596328452 ) ) ;
#33756 = ADVANCED_FACE ( 'NONE', ( #24371 ), #56719, .F. ) ;
#33757 = VERTEX_POINT ( 'NONE', #47184 ) ;
#33758 = EDGE_CURVE ( 'NONE', #39418, #44574, #11181, .T. ) ;
#33759 = VERTEX_POINT ( 'NONE', #14151 ) ;
#33760 = CARTESIAN_POINT ( 'NONE',  ( -30.26163486738143860, 23.53144966999699150, 13.32819397642332859 ) ) ;
#33761 = ORIENTED_EDGE ( 'NONE', *, *, #14611, .T. ) ;
#33762 = CARTESIAN_POINT ( 'NONE',  ( -55.05276343752910151, -170.0000000000000000, -69.56087458892355357 ) ) ;
#33763 = DIRECTION ( 'NONE',  ( 1.000000000000000000, 0.000000000000000000, -0.000000000000000000 ) ) ;
#33764 = CARTESIAN_POINT ( 'NONE',  ( 141.3354458183166287, 47.33100220280247328, 90.10713329041466579 ) ) ;
#33765 = FACE_OUTER_BOUND ( 'NONE', #43865, .T. ) ;
#33766 = DIRECTION ( 'NONE',  ( 1.000000000000000000, 0.000000000000000000, 0.000000000000000000 ) ) ;
#33767 = ORIENTED_EDGE ( 'NONE', *, *, #18062, .T. ) ;
#33768 = EDGE_CURVE ( 'NONE', #17316, #2210, #3945, .T. ) ;
#33769 = LINE ( 'NONE', #23220, #2081 ) ;
#33770 = ORIENTED_EDGE ( 'NONE', *, *, #65510, .T. ) ;
#33771 = ORIENTED_EDGE ( 'NONE', *, *, #41333, .F. ) ;
#33772 = CARTESIAN_POINT ( 'NONE',  ( -422.6627218934913230, 399.9999999999997726, 113.5502958579881891 ) ) ;
#33773 = LINE ( 'NONE', #11957, #13727 ) ;
#33774 = CARTESIAN_POINT ( 'NONE',  ( 412.3372781065085633, 219.4906275429376308, -146.4497041420117682 ) ) ;
#33775 = CARTESIAN_POINT ( 'NONE',  ( 139.3067271572849677, 44.81402783181202665, -65.20950923262978449 ) ) ;
#33776 = CARTESIAN_POINT ( 'NONE',  ( 0.000000000000000000, 0.000000000000000000, 40.00000000000003553 ) ) ;
#33777 = VERTEX_POINT ( 'NONE', #40530 ) ;
#33778 = VERTEX_POINT ( 'NONE', #46848 ) ;
#33779 = CARTESIAN_POINT ( 'NONE',  ( 65.33961467711179694, 13.12780797910698816, 34.48241823980619358 ) ) ;
#33780 = ORIENTED_EDGE ( 'NONE', *, *, #27751, .F. ) ;
#33781 = FACE_OUTER_BOUND ( 'NONE', #44217, .T. ) ;
#33782 = ORIENTED_EDGE ( 'NONE', *, *, #68309, .T. ) ;
#33783 = DIRECTION ( 'NONE',  ( -0.000000000000000000, 1.000000000000000000, -0.000000000000000000 ) ) ;
#33784 = CIRCLE ( 'NONE', #58467, 21.99999999999998579 ) ;
#33785 = CARTESIAN_POINT ( 'NONE',  ( 93.70675391435744928, 21.95852801827565770, 7.872820059410217119 ) ) ;
#33786 = CARTESIAN_POINT ( 'NONE',  ( -1.683356153843273750, 65.34430428700410687, 41.38025477438755928 ) ) ;
#33787 = ORIENTED_EDGE ( 'NONE', *, *, #68677, .F. ) ;
#33788 = DIRECTION ( 'NONE',  ( 1.000000000000000000, 0.000000000000000000, 0.000000000000000000 ) ) ;
#33789 = DIRECTION ( 'NONE',  ( 1.000000000000000000, 0.000000000000000000, 0.000000000000000000 ) ) ;
#33790 = CARTESIAN_POINT ( 'NONE',  ( 36.98541457540710553, 9.120571655722420346, 44.53055877612269597 ) ) ;
#33791 = CARTESIAN_POINT ( 'NONE',  ( 66.30230369578305272, 14.49551544185123753, 30.56703610697686102 ) ) ;
#33792 = CARTESIAN_POINT ( 'NONE',  ( -125.8938041572051105, 46.49392987655492959, -23.06915330777029638 ) ) ;
#33793 = CARTESIAN_POINT ( 'NONE',  ( -146.3604280344345909, 61.55502468262317706, -89.18082157871309334 ) ) ;
#33794 = CARTESIAN_POINT ( 'NONE',  ( 133.3996297101683979, 41.14871796345731525, -62.86786152285935003 ) ) ;
#33795 = EDGE_LOOP ( 'NONE', ( #25504, #53996 ) ) ;
#33796 = PLANE ( 'NONE',  #2847 ) ;
#33797 = PLANE ( 'NONE',  #66981 ) ;
#33798 = VERTEX_POINT ( 'NONE', #13799 ) ;
#33799 = DIRECTION ( 'NONE',  ( -1.000000000000000000, 0.000000000000000000, 0.000000000000000000 ) ) ;
#33800 = CARTESIAN_POINT ( 'NONE',  ( -0.5183605925911991541, 6.525266619725957007, -71.47052751656273983 ) ) ;
#33801 = CARTESIAN_POINT ( 'NONE',  ( -37.37206033059242571, 11.66494618096613145, 33.12183574046159151 ) ) ;
#33802 = CARTESIAN_POINT ( 'NONE',  ( -144.7530445311634821, 61.54314312182905411, -21.27383361102199189 ) ) ;
#33803 = PLANE ( 'NONE',  #7623 ) ;
#33804 = EDGE_CURVE ( 'NONE', #8775, #2294, #24717, .T. ) ;
#33805 = CYLINDRICAL_SURFACE ( 'NONE', #54616, 7.500000000000013323 ) ;
#33806 = DIRECTION ( 'NONE',  ( 0.000000000000000000, 0.000000000000000000, 1.000000000000000000 ) ) ;
#33807 = CARTESIAN_POINT ( 'NONE',  ( 114.9668435325539235, 21.99239968880144502, -0.6609596067687202314 ) ) ;
#33808 = CARTESIAN_POINT ( 'NONE',  ( -2.873329055852802405, 7.626065826870667586, -21.72791809929673690 ) ) ;
#33809 = CARTESIAN_POINT ( 'NONE',  ( -11.13714165684777946, 8.138643170880698108, 30.88190552611061435 ) ) ;
#33810 = CARTESIAN_POINT ( 'NONE',  ( 116.1021807117071631, 31.68810634233422263, 14.97497448979273571 ) ) ;
#33811 = LINE ( 'NONE', #28532, #23059 ) ;
#33812 = ORIENTED_EDGE ( 'NONE', *, *, #46043, .T. ) ;
#33813 = CARTESIAN_POINT ( 'NONE',  ( -101.8140949286062380, 33.67224128592402366, -35.01457726497591239 ) ) ;
#33814 = ORIENTED_EDGE ( 'NONE', *, *, #60180, .T. ) ;
#33815 = CARTESIAN_POINT ( 'NONE',  ( -19.56458807131831890, -15.75959024859417390, 3.061616997868437868E-16 ) ) ;
#33816 = CARTESIAN_POINT ( 'NONE',  ( 79.13041963748371188, 18.04952109592811382, -70.68632447848128209 ) ) ;
#33817 = CARTESIAN_POINT ( 'NONE',  ( 104.1111664609392022, 27.24250349207208899, 86.46839379475228782 ) ) ;
#33818 = CARTESIAN_POINT ( 'NONE',  ( -48.12872802574198516, -43.70867239603780519, 0.000000000000000000 ) ) ;
#33819 = CARTESIAN_POINT ( 'NONE',  ( -15.55634918610403439, 2.818925648462311528E-14, 2.000000000000001776 ) ) ;
#33820 = CONICAL_SURFACE ( 'NONE', #57410, 74.95140232871122521, 0.8777644062502172329 ) ;
#33821 = PRODUCT_DEFINITION_SHAPE ( 'NONE', 'NONE',  #69637 ) ;
#33822 = CARTESIAN_POINT ( 'NONE',  ( 0.000000000000000000, 0.000000000000000000, 5.000000000000000888 ) ) ;
#33823 = AXIS2_PLACEMENT_3D ( 'NONE', #51844, #3657, #8604 ) ;
#33824 = CARTESIAN_POINT ( 'NONE',  ( -1.224646799147352468E-15, 16.00000000000000000, 6.196318915105386793 ) ) ;
#33825 = CARTESIAN_POINT ( 'NONE',  ( -118.8691191306315460, 43.21907118237575673, -12.92847206412439220 ) ) ;
#33826 = EDGE_LOOP ( 'NONE', ( #60897, #18023, #62818, #1868, #2311, #21539, #57896 ) ) ;
#33827 = EDGE_LOOP ( 'NONE', ( #59627, #22118, #20286, #23676 ) ) ;
#33829 = EDGE_CURVE ( 'NONE', #30922, #35779, #25826, .T. ) ;
#33828 = DIRECTION ( 'NONE',  ( -1.000000000000000000, -0.000000000000000000, -0.000000000000000000 ) ) ;
#33830 = DIRECTION ( 'NONE',  ( -1.807017991507219923E-16, 1.727686100818908852E-16, 1.000000000000000000 ) ) ;
#33832 = CARTESIAN_POINT ( 'NONE',  ( 46.47744650267831190, 9.435478116178785513, -94.18279426279515576 ) ) ;
#33831 = AXIS2_PLACEMENT_3D ( 'NONE', #54621, #11360, #22622 ) ;
#33833 =( NAMED_UNIT ( * ) PLANE_ANGLE_UNIT ( ) SI_UNIT ( $, .RADIAN. ) );
#33834 = CARTESIAN_POINT ( 'NONE',  ( -125.8938041572051389, -170.0000000000000000, 38.11994787315708777 ) ) ;
#33835 = EDGE_CURVE ( 'NONE', #68286, #21636, #65827, .T. ) ;
#33836 = AXIS2_PLACEMENT_3D ( 'NONE', #59122, #64763, #1094 ) ;
#33837 = CARTESIAN_POINT ( 'NONE',  ( -15.55634918610403439, 2.818925648462311528E-14, 0.000000000000000000 ) ) ;
#33838 = EDGE_LOOP ( 'NONE', ( #8654, #27814 ) ) ;
#33839 = CARTESIAN_POINT ( 'NONE',  ( 87.59078297315400619, 20.81577753000345155, 2.914042839113803129 ) ) ;
#33840 = CARTESIAN_POINT ( 'NONE',  ( 23.23965501943000334, 7.861749956303022202, -44.00267626036002611 ) ) ;
#33841 = CARTESIAN_POINT ( 'NONE',  ( 15.78827728214693416, 7.507518794609588042, 56.85925826316891829 ) ) ;
#33842 = DIRECTION ( 'NONE',  ( -1.000000000000000000, 0.000000000000000000, 0.000000000000000000 ) ) ;
#33843 = DIRECTION ( 'NONE',  ( 0.9510565162951545304, -0.3090169943749447312, 5.102127870520021228E-18 ) ) ;
#33844 = FACE_BOUND ( 'NONE', #44590, .T. ) ;
#33845 = CARTESIAN_POINT ( 'NONE',  ( 161.7006237583813117, 62.31514460450498660, 57.54382807939717992 ) ) ;
#33846 = EDGE_CURVE ( 'NONE', #3228, #964, #52471, .T. ) ;
#33847 = ORIENTED_EDGE ( 'NONE', *, *, #22312, .F. ) ;
#33848 = CARTESIAN_POINT ( 'NONE',  ( 20.00000000000000000, 0.000000000000000000, -5.000000000000000888 ) ) ;
#33849 = DIRECTION ( 'NONE',  ( -0.000000000000000000, -0.000000000000000000, -1.000000000000000000 ) ) ;
#33850 = DIRECTION ( 'NONE',  ( 0.000000000000000000, 1.000000000000000000, 0.000000000000000000 ) ) ;
#33851 = CARTESIAN_POINT ( 'NONE',  ( -20.63749999999999929, 0.000000000000000000, 0.000000000000000000 ) ) ;
#33852 = CARTESIAN_POINT ( 'NONE',  ( 153.4268936273268196, 54.57409659828383752, 3.743913822929773705 ) ) ;
#33853 = ADVANCED_FACE ( 'NONE', ( #46493, #19420 ), #2908, .T. ) ;
#33854 = EDGE_CURVE ( 'NONE', #35286, #49653, #41233, .T. ) ;
#33855 = DIRECTION ( 'NONE',  ( 0.000000000000000000, 0.000000000000000000, 1.000000000000000000 ) ) ;
#33856 = ORIENTED_EDGE ( 'NONE', *, *, #28493, .F. ) ;
#33857 = DIRECTION ( 'NONE',  ( 1.000000000000000000, 0.000000000000000000, -0.000000000000000000 ) ) ;
#33858 = LINE ( 'NONE', #11339, #58550 ) ;
#33859 = ORIENTED_EDGE ( 'NONE', *, *, #7636, .T. ) ;
#33860 = CARTESIAN_POINT ( 'NONE',  ( -24.51966494718108081, 5.470267094204372960, 3.061616997868437868E-16 ) ) ;
#33861 = ORIENTED_EDGE ( 'NONE', *, *, #67999, .T. ) ;
#33862 = PLANE ( 'NONE',  #22973 ) ;
#33863 = FACE_OUTER_BOUND ( 'NONE', #21575, .T. ) ;
#33864 = CARTESIAN_POINT ( 'NONE',  ( 89.88147981065576175, 21.62466191578946706, -63.39067841512786572 ) ) ;
#33865 = ORIENTED_EDGE ( 'NONE', *, *, #2659, .F. ) ;
#33866 = AXIS2_PLACEMENT_3D ( 'NONE', #25208, #68115, #15670 ) ;
#33867 = ORIENTED_EDGE ( 'NONE', *, *, #48903, .T. ) ;
#33868 = CARTESIAN_POINT ( 'NONE',  ( 39.89582146299186860, 9.488756994579084392, 71.75838489642696061 ) ) ;
#33869 = LINE ( 'NONE', #23663, #61809 ) ;
#33870 = CARTESIAN_POINT ( 'NONE',  ( -151.2511071212631464, 67.00426547928869070, -61.84963319502005419 ) ) ;
#33871 = CARTESIAN_POINT ( 'NONE',  ( 69.35866309798980467, 15.27376159675663736, 14.47800203215017056 ) ) ;
#33872 = CARTESIAN_POINT ( 'NONE',  ( 0.000000000000000000, 0.000000000000000000, 0.000000000000000000 ) ) ;
#33873 = AXIS2_PLACEMENT_3D ( 'NONE', #46661, #20275, #9382 ) ;
#33874 = ORIENTED_EDGE ( 'NONE', *, *, #16969, .T. ) ;
#33875 = PRODUCT_DEFINITION_SHAPE ( 'NONE', 'NONE',  #69607 ) ;
#33876 = AXIS2_PLACEMENT_3D ( 'NONE', #11275, #65104, #21831 ) ;
#33877 = VECTOR ( 'NONE', #2596, 1000.000000000000000 ) ;
#33878 =( LENGTH_UNIT ( ) NAMED_UNIT ( * ) SI_UNIT ( .MILLI., .METRE. ) );
#33879 = CARTESIAN_POINT ( 'NONE',  ( -48.70883077256302585, 14.10659259062419046, 6.964640123796999482 ) ) ;
#33880 = FACE_OUTER_BOUND ( 'NONE', #55166, .T. ) ;
#33881 = CARTESIAN_POINT ( 'NONE',  ( -156.4859261060826157, 71.69908252863689313, -93.24215537093068917 ) ) ;
#33882 = CARTESIAN_POINT ( 'NONE',  ( 113.4351684956570239, 30.38657459074491030, -23.38094634528284743 ) ) ;
#33883 = CARTESIAN_POINT ( 'NONE',  ( 93.28163122584956568, 21.79878316975275965, 94.43086186953131289 ) ) ;
#33885 = ORIENTED_EDGE ( 'NONE', *, *, #25827, .T. ) ;
#33884 = PLANE ( 'NONE',  #16333 ) ;
#33886 = ORIENTED_EDGE ( 'NONE', *, *, #27631, .T. ) ;
#33887 = STYLED_ITEM ( 'NONE', ( #10610 ), #16524 ) ;
#33888 = ORIENTED_EDGE ( 'NONE', *, *, #5526, .T. ) ;
#33889 = CARTESIAN_POINT ( 'NONE',  ( 0.000000000000000000, 0.000000000000000000, 41.38025477438755928 ) ) ;
#33890 = CARTESIAN_POINT ( 'NONE',  ( 169.9999999999999716, 3.680555555555560243, 4.000000000000000000 ) ) ;
#33891 = CARTESIAN_POINT ( 'NONE',  ( -49.62489392740900485, 13.29305723289023966, -21.05326579410700560 ) ) ;
#33892 = EDGE_CURVE ( 'NONE', #2402, #37212, #4622, .T. ) ;
#33893 = LINE ( 'NONE', #9924, #22040 ) ;
#33894 = CARTESIAN_POINT ( 'NONE',  ( -38.45778834351242637, 11.87434869453506892, 67.21600681512579456 ) ) ;
#33895 = CARTESIAN_POINT ( 'NONE',  ( -27.75784411156621090, 18.62216926092103009, 6.893342936425399081 ) ) ;
#33896 = CARTESIAN_POINT ( 'NONE',  ( -71.96390573417174608, 19.88067451234327621, -66.05669224067524681 ) ) ;
#33897 = CARTESIAN_POINT ( 'NONE',  ( -7.825402957745083654, 6.891034867348166060, 30.11558103944718923 ) ) ;
#33899 = ORIENTED_EDGE ( 'NONE', *, *, #24503, .T. ) ;
#33898 = ADVANCED_FACE ( 'NONE', ( #53828 ), #47872, .T. ) ;
#33900 = CARTESIAN_POINT ( 'NONE',  ( 26.11269837220806167, -6.375108774214766072E-14, 2.000000000000001776 ) ) ;
#33901 = ORIENTED_EDGE ( 'NONE', *, *, #19860, .T. ) ;
#33902 = EDGE_LOOP ( 'NONE', ( #17342, #63373, #15000, #33701 ) ) ;
#33903 = CARTESIAN_POINT ( 'NONE',  ( -142.0070007485041117, 59.34878529741514086, 11.10676733467697730 ) ) ;
#33904 = CARTESIAN_POINT ( 'NONE',  ( -61.00567534907362699, 17.40801984996452489, -91.82290913100322882 ) ) ;
#33905 = CARTESIAN_POINT ( 'NONE',  ( -38.02163356681019479, 11.78964455120423693, 94.99999999999866418 ) ) ;
#33906 = CARTESIAN_POINT ( 'NONE',  ( 110.2429982417149432, 29.99119854320847267, -24.07788697519002596 ) ) ;
#33907 = DIRECTION ( 'NONE',  ( -0.2225209339563042066, -0.9749279121818259508, 0.000000000000000000 ) ) ;
#33908 = LINE ( 'NONE', #7173, #35944 ) ;
#33909 = CARTESIAN_POINT ( 'NONE',  ( 135.6793972494602940, 43.71805072851429230, -23.96845213928238039 ) ) ;
#33910 = EDGE_LOOP ( 'NONE', ( #18586, #36846, #16402, #50042 ) ) ;
#33911 = ADVANCED_FACE ( 'NONE', ( #26086 ), #58094, .T. ) ;
#33912 = VERTEX_POINT ( 'NONE', #9915 ) ;
#33913 = ORIENTED_EDGE ( 'NONE', *, *, #45998, .T. ) ;
#33914 = EDGE_CURVE ( 'NONE', #48508, #48281, #50490, .T. ) ;
#33915 = DIRECTION ( 'NONE',  ( 0.7071067811865474617, 0.000000000000000000, -0.7071067811865476838 ) ) ;
#33916 = DIRECTION ( 'NONE',  ( -0.000000000000000000, 1.000000000000000000, -0.000000000000000000 ) ) ;
#33917 = CARTESIAN_POINT ( 'NONE',  ( 31.90184941268615759, 7.552181687745349592, -70.20641173465664053 ) ) ;
#33918 = CARTESIAN_POINT ( 'NONE',  ( 59.72897338775215559, 11.93428797217974768, -23.12208266423090919 ) ) ;
#33919 = EDGE_CURVE ( 'NONE', #49926, #47377, #69336, .T. ) ;
#33920 = UNCERTAINTY_MEASURE_WITH_UNIT (LENGTH_MEASURE( 1.000000000000000082E-05 ), #53424, 'distance_accuracy_value', 'NONE');
#33921 = VECTOR ( 'NONE', #45436, 1000.000000000000000 ) ;
#33922 = EDGE_CURVE ( 'NONE', #48751, #11163, #4968, .T. ) ;
#33923 = CARTESIAN_POINT ( 'NONE',  ( -54.57280099357649306, 14.55288945003959888, 30.31732777293113656 ) ) ;
#33924 = DIRECTION ( 'NONE',  ( 1.000000000000000000, 0.000000000000000000, 0.000000000000000000 ) ) ;
#33925 = VERTEX_POINT ( 'NONE', #65102 ) ;
#33926 = CARTESIAN_POINT ( 'NONE',  ( -58.76099769480629220, 16.75353773354895281, -63.03723493735800787 ) ) ;
#33927 = DIRECTION ( 'NONE',  ( -1.000000000000000000, -4.565061778886334783E-18, 0.000000000000000000 ) ) ;
#33928 = VECTOR ( 'NONE', #5570, 1000.000000000000000 ) ;
#33929 = CARTESIAN_POINT ( 'NONE',  ( -0.5658006089934872751, 7.533733779014707643, -44.86461209534569861 ) ) ;
#33930 = CYLINDRICAL_SURFACE ( 'NONE', #10491, 21.00000000000000355 ) ;
#33931 = CARTESIAN_POINT ( 'NONE',  ( -168.7187482717114051, 82.35796501763486788, 5.386810785733501028 ) ) ;
#33932 = DIRECTION ( 'NONE',  ( 1.661094098900087138E-16, 0.6427876096865404731, -0.7660444431189771253 ) ) ;
#33933 = FACE_BOUND ( 'NONE', #63687, .T. ) ;
#33934 = CARTESIAN_POINT ( 'NONE',  ( -189.3696967735686485, 107.2697815289672718, 90.68589341612421606 ) ) ;
#33935 = VECTOR ( 'NONE', #19877, 1000.000000000000000 ) ;
#33936 = EDGE_CURVE ( 'NONE', #34238, #61056, #68977, .T. ) ;
#33937 = VECTOR ( 'NONE', #26690, 1000.000000000000000 ) ;
#33938 = ORIENTED_EDGE ( 'NONE', *, *, #24887, .F. ) ;
#33939 = CARTESIAN_POINT ( 'NONE',  ( 277.7789859651024358, 21.53699436807884027, 4.491592093615985881 ) ) ;
#33940 = CARTESIAN_POINT ( 'NONE',  ( -127.6861178856153174, 47.68458428355325651, -61.96166341335298000 ) ) ;
#33941 = CYLINDRICAL_SURFACE ( 'NONE', #63535, 7.500000000000013323 ) ;
#33942 = ADVANCED_FACE ( 'NONE', ( #377 ), #43279, .F. ) ;
#33943 = CARTESIAN_POINT ( 'NONE',  ( 0.000000000000000000, 0.000000000000000000, 43.58025477438756212 ) ) ;
#33944 = EDGE_CURVE ( 'NONE', #68395, #27359, #67209, .T. ) ;
#33945 = DIRECTION ( 'NONE',  ( 0.000000000000000000, 1.000000000000000000, 0.000000000000000000 ) ) ;
#33946 = ORIENTED_EDGE ( 'NONE', *, *, #9008, .F. ) ;
#33947 = DIRECTION ( 'NONE',  ( -0.000000000000000000, 0.000000000000000000, -1.000000000000000000 ) ) ;
#33948 = CARTESIAN_POINT ( 'NONE',  ( 178.9572806431051788, 76.48101739820698697, 83.28229297188985925 ) ) ;
#33949 = ORIENTED_EDGE ( 'NONE', *, *, #10636, .F. ) ;
#33950 = ORIENTED_EDGE ( 'NONE', *, *, #57470, .T. ) ;
#33951 = CARTESIAN_POINT ( 'NONE',  ( 173.7246046907419554, 71.47482343504563573, -42.25086531254567745 ) ) ;
#33952 = CARTESIAN_POINT ( 'NONE',  ( 150.4722669492348643, 53.65054032737663192, 34.19824095576758083 ) ) ;
#33953 = LINE ( 'NONE', #44495, #11089 ) ;
#33954 = ORIENTED_EDGE ( 'NONE', *, *, #11242, .T. ) ;
#33955 = CARTESIAN_POINT ( 'NONE',  ( 111.1865443042261603, 30.43181341527237649, 56.50051719710833709 ) ) ;
#33956 = CARTESIAN_POINT ( 'NONE',  ( -178.2381786520593607, 93.01028335822124404, 16.96567094477213189 ) ) ;
#33957 = CARTESIAN_POINT ( 'NONE',  ( 324.1677456657756125, 2.000000000000000000, -123.1183350412580779 ) ) ;
#33958 = FACE_OUTER_BOUND ( 'NONE', #11421, .T. ) ;
#33959 = FACE_OUTER_BOUND ( 'NONE', #54815, .T. ) ;
#33960 = CARTESIAN_POINT ( 'NONE',  ( -47.55316895016325418, 13.83165595246916801, -15.36910518223855426 ) ) ;
#33961 = ORIENTED_EDGE ( 'NONE', *, *, #34428, .F. ) ;
#33962 = CARTESIAN_POINT ( 'NONE',  ( -123.4416615615273258, 44.90042688650401459, -8.477572847294975844 ) ) ;
#33963 = CARTESIAN_POINT ( 'NONE',  ( -71.22896441287282698, 20.69091426169409687, 10.07455366818023279 ) ) ;
#33964 = CARTESIAN_POINT ( 'NONE',  ( -145.5195986658808920, 62.16746116576787529, -48.66889029199882799 ) ) ;
#33965 = LINE ( 'NONE', #33625, #45517 ) ;
#33967 = VERTEX_POINT ( 'NONE', #64056 ) ;
#33966 = CARTESIAN_POINT ( 'NONE',  ( -133.3249632897631614, 51.58572645347020824, 90.73949300795004547 ) ) ;
#33968 = CARTESIAN_POINT ( 'NONE',  ( 79.92465405224848496, 17.24122384219593940, -39.92366204608148195 ) ) ;
#33969 = AXIS2_PLACEMENT_3D ( 'NONE', #66841, #2116, #7736 ) ;
#33970 = VERTEX_POINT ( 'NONE', #15867 ) ;
#33971 = AXIS2_PLACEMENT_3D ( 'NONE', #31979, #33014, #49167 ) ;
#33972 = DIRECTION ( 'NONE',  ( -1.000000000000000000, 0.000000000000000000, 0.000000000000000000 ) ) ;
#33973 = CARTESIAN_POINT ( 'NONE',  ( 86.14890207173841929, 20.31981596387579714, 44.71208757247934074 ) ) ;
#33974 = LINE ( 'NONE', #66693, #18638 ) ;
#33975 = CARTESIAN_POINT ( 'NONE',  ( 93.43270425363546394, 22.93046121381056324, 34.04559475132371205 ) ) ;
#33976 = CONICAL_SURFACE ( 'NONE', #3643, 74.95140232871122521, 0.8777644062502172329 ) ;
#33977 = CARTESIAN_POINT ( 'NONE',  ( 134.7770330630252715, 41.98246829846534922, -9.221158025336912090 ) ) ;
#33978 = FACE_OUTER_BOUND ( 'NONE', #24443, .T. ) ;
#33979 = CARTESIAN_POINT ( 'NONE',  ( 20.11619980831799737, 7.685075536026321430, -90.56824105099134670 ) ) ;
#33980 = ADVANCED_FACE ( 'NONE', ( #53137 ), #64754, .F. ) ;
#33981 = CARTESIAN_POINT ( 'NONE',  ( -35.00000000000000000, 0.000000000000000000, 30.00000000000000000 ) ) ;
#33982 = ORIENTED_EDGE ( 'NONE', *, *, #28376, .F. ) ;
#33984 = ORIENTED_EDGE ( 'NONE', *, *, #58575, .F. ) ;
#33983 = B_SPLINE_CURVE_WITH_KNOTS ( 'NONE', 3,
 ( #37645, #48185, #47850, #4604, #69316, #21468, #21142, #42585, #64041, #11, #56571, #36501, #29838, #20316, #8393, #18942, #24580, #8747, #41780, #25951, #25268, #14694 ),
 .UNSPECIFIED., .F., .F.,
 ( 4, 2, 2, 2, 2, 2, 2, 2, 2, 2, 4 ),
 ( 9.309503074677274191E-17, 0.001318139496345288294, 0.001977209244517854486, 0.002636278992690420462, 0.003954418489035491265, 0.005272557985380562501, 0.005931627733553119369, 0.006590697481725675370, 0.007908836978070793444, 0.009226976474415910651, 0.01054511597076102612 ),
 .UNSPECIFIED. ) ;
#33985 = FACE_OUTER_BOUND ( 'NONE', #28491, .T. ) ;
#33986 = CIRCLE ( 'NONE', #3649, 5.000000000000004441 ) ;
#33987 = CYLINDRICAL_SURFACE ( 'NONE', #52033, 7.500000000000013323 ) ;
#33988 = CARTESIAN_POINT ( 'NONE',  ( -59.94154301275570873, 45.09516516490385385, 170.0000000000000000 ) ) ;
#33989 = DIRECTION ( 'NONE',  ( -3.081487911019579554E-32, -1.000000000000000000, -3.469446951953612956E-17 ) ) ;
#33990 = CARTESIAN_POINT ( 'NONE',  ( 204.6977192012829505, 108.0580384837234931, -51.32593103262161094 ) ) ;
#33991 = CARTESIAN_POINT ( 'NONE',  ( -30.62628708973388569, 68.47330165179126027, 170.0000000000000000 ) ) ;
#33992 = LINE ( 'NONE', #38924, #38189 ) ;
#33993 = CARTESIAN_POINT ( 'NONE',  ( -23.95096213915836714, 8.481591526885946308, -42.32845173688443907 ) ) ;
#33994 = DIRECTION ( 'NONE',  ( 0.000000000000000000, 0.000000000000000000, -1.000000000000000000 ) ) ;
#33995 = EDGE_CURVE ( 'NONE', #10801, #41137, #11273, .T. ) ;
#33996 = ORIENTED_EDGE ( 'NONE', *, *, #14295, .T. ) ;
#33997 = ORIENTED_EDGE ( 'NONE', *, *, #28759, .F. ) ;
#33998 = CARTESIAN_POINT ( 'NONE',  ( 51.39999999999999858, 5.616230220889761452E-16, -4.171999999999999709 ) ) ;
#33999 = CYLINDRICAL_SURFACE ( 'NONE', #12833, 7.500000000000020428 ) ;
#34000 = EDGE_CURVE ( 'NONE', #39038, #62258, #15535, .T. ) ;
#34001 = CARTESIAN_POINT ( 'NONE',  ( -85.34215807311493052, 24.97769003780924280, 68.19029523188604003 ) ) ;
#34002 = CARTESIAN_POINT ( 'NONE',  ( 126.3681350380371242, 38.23508791628619718, 37.50295032406403095 ) ) ;
#34003 = CARTESIAN_POINT ( 'NONE',  ( 8.000000000000007105, 249.8719672152120381, 94.99999999999866418 ) ) ;
#34004 = EDGE_CURVE ( 'NONE', #17967, #47060, #14537, .T. ) ;
#34005 = CARTESIAN_POINT ( 'NONE',  ( 64.97411640938653932, -37.36411256620218069, 41.38025477438755928 ) ) ;
#34006 = CARTESIAN_POINT ( 'NONE',  ( -101.8187363387487210, 33.67461140603126779, -23.17002667451226472 ) ) ;
#34007 = CARTESIAN_POINT ( 'NONE',  ( 57.57684776206770749, 12.50442334002048206, 32.14292840263019002 ) ) ;
#34008 = CARTESIAN_POINT ( 'NONE',  ( 35.07461521969879215, 7.885994798980979326, 84.96838794907451131 ) ) ;
#34009 = CARTESIAN_POINT ( 'NONE',  ( 22.07550062443481664, 11.73338281062075872, 0.000000000000000000 ) ) ;
#34010 = ORIENTED_EDGE ( 'NONE', *, *, #36472, .F. ) ;
#34011 = CARTESIAN_POINT ( 'NONE',  ( -34.39004539972345498, 0.000000000000000000, -9.999999999999998224 ) ) ;
#34012 = PLANE ( 'NONE',  #36318 ) ;
#34013 = CARTESIAN_POINT ( 'NONE',  ( -190.4966031023458299, 108.8421921967458701, -37.93375413894162307 ) ) ;
#34014 = DIRECTION ( 'NONE',  ( 1.000000000000000000, -0.000000000000000000, -0.000000000000000000 ) ) ;
#34015 = CARTESIAN_POINT ( 'NONE',  ( -109.7078892845591298, 36.71702188566217018, -68.28782286830018222 ) ) ;
#34016 = CARTESIAN_POINT ( 'NONE',  ( -96.04542865839948718, 29.72476396586411340, -92.00996532311685883 ) ) ;
#34017 = ORIENTED_EDGE ( 'NONE', *, *, #54356, .F. ) ;
#34018 = AXIS2_PLACEMENT_3D ( 'NONE', #28938, #66238, #2203 ) ;
#34019 = DIRECTION ( 'NONE',  ( 9.540529038762972043E-15, -4.297659324423976752E-15, 0.9999999999999997780 ) ) ;
#34020 = CARTESIAN_POINT ( 'NONE',  ( -189.9554299271397895, 108.0836897899587825, -12.03754007755143718 ) ) ;
#34021 = DIRECTION ( 'NONE',  ( -4.314083075427411048E-32, -1.000000000000000000, -6.123233995736762338E-17 ) ) ;
#34022 = EDGE_CURVE ( 'NONE', #54476, #41255, #5994, .T. ) ;
#34023 = CARTESIAN_POINT ( 'NONE',  ( 299.8372781065085064, 399.9999999999998863, -33.94970414201181796 ) ) ;
#34024 = DIRECTION ( 'NONE',  ( -0.000000000000000000, 1.000000000000000000, -0.000000000000000000 ) ) ;
#34025 = ORIENTED_EDGE ( 'NONE', *, *, #62001, .F. ) ;
#34026 = LINE ( 'NONE', #65336, #47000 ) ;
#34027 = VECTOR ( 'NONE', #15374, 1000.000000000000000 ) ;
#34028 = CARTESIAN_POINT ( 'NONE',  ( -3.244108878396733786, 6.635632329121485817, -10.11498957647276598 ) ) ;
#34029 = ADVANCED_FACE ( 'NONE', ( #48893 ), #60578, .T. ) ;
#34030 = DIRECTION ( 'NONE',  ( 0.000000000000000000, 0.000000000000000000, 1.000000000000000000 ) ) ;
#34031 = VECTOR ( 'NONE', #52675, 1000.000000000000114 ) ;
#34032 = CARTESIAN_POINT ( 'NONE',  ( 0.000000000000000000, 0.000000000000000000, 0.000000000000000000 ) ) ;
#34033 = VECTOR ( 'NONE', #23014, 1000.000000000000000 ) ;
#34034 = DIRECTION ( 'NONE',  ( -0.000000000000000000, -0.000000000000000000, -1.000000000000000000 ) ) ;
#34035 = ORIENTED_EDGE ( 'NONE', *, *, #15008, .T. ) ;
#34036 = CARTESIAN_POINT ( 'NONE',  ( 164.1849564601154441, 64.37948657927526597, -93.96497455420622202 ) ) ;
#34037 = CYLINDRICAL_SURFACE ( 'NONE', #37303, 10.00000000000000178 ) ;
#34038 = CARTESIAN_POINT ( 'NONE',  ( 447.3372781065086770, 400.0000000000066507, -146.4497041420121093 ) ) ;
#34039 = AXIS2_PLACEMENT_3D ( 'NONE', #841, #7162, #59910 ) ;
#34040 = CARTESIAN_POINT ( 'NONE',  ( 16.76400266940279948, 6.533513613209221305, -50.47150667450311090 ) ) ;
#34042 = EDGE_LOOP ( 'NONE', ( #53893, #20034 ) ) ;
#34041 = CARTESIAN_POINT ( 'NONE',  ( 10.55634918610409656, 31.11269837220803325, 0.000000000000000000 ) ) ;
#34043 = CARTESIAN_POINT ( 'NONE',  ( 61.09275639403235658, 12.23448398202910248, 30.04748534290944662 ) ) ;
#34044 = EDGE_LOOP ( 'NONE', ( #10699, #16595, #61976, #38311 ) ) ;
#34045 = ORIENTED_EDGE ( 'NONE', *, *, #36081, .T. ) ;
#34046 = CARTESIAN_POINT ( 'NONE',  ( -125.4859928193505567, 46.22544753638531034, -88.60280507916128556 ) ) ;
#34047 = CARTESIAN_POINT ( 'NONE',  ( -78.66644367742111399, -170.0000000000000000, 64.76275173013681297 ) ) ;
#34049 = ORIENTED_EDGE ( 'NONE', *, *, #12471, .F. ) ;
#34048 = CARTESIAN_POINT ( 'NONE',  ( -11.78188048797445298, 8.190559674012732216, -76.13891883678253691 ) ) ;
#34050 = CARTESIAN_POINT ( 'NONE',  ( 35.39413431650373099, 0.000000000000000000, -9.999999999999998224 ) ) ;
#34051 = DIRECTION ( 'NONE',  ( 0.000000000000000000, 1.000000000000000000, 0.000000000000000000 ) ) ;
#34052 = FACE_BOUND ( 'NONE', #36444, .T. ) ;
#34053 = PRODUCT_RELATED_PRODUCT_CATEGORY ( 'part', '', ( #66481 ) ) ;
#34054 = EDGE_LOOP ( 'NONE', ( #7642, #69282 ) ) ;
#34055 = CARTESIAN_POINT ( 'NONE',  ( 207.2640160519426615, 111.6867652229576322, -77.72071523413366378 ) ) ;
#34056 = EDGE_CURVE ( 'NONE', #15985, #4944, #64399, .T. ) ;
#34057 = CARTESIAN_POINT ( 'NONE',  ( -109.6829043543429236, -170.0000000000000000, -95.00000000000133582 ) ) ;
#34058 = EDGE_CURVE ( 'NONE', #49097, #5706, #59113, .T. ) ;
#34060 = CARTESIAN_POINT ( 'NONE',  ( -179.2210908201800805, 95.76260491022611632, 42.71376849300861522 ) ) ;
#34059 = CIRCLE ( 'NONE', #19593, 54.99999999999995026 ) ;
#34061 = CARTESIAN_POINT ( 'NONE',  ( 132.9453095272139365, 42.04754713161464252, 71.35489142945908725 ) ) ;
#34062 = CARTESIAN_POINT ( 'NONE',  ( 16.27775141556968919, 7.523247835309962106, 56.85925826316893961 ) ) ;
#34063 = ORIENTED_EDGE ( 'NONE', *, *, #56296, .F. ) ;
#34064 = VERTEX_POINT ( 'NONE', #2139 ) ;
#34065 = ORIENTED_EDGE ( 'NONE', *, *, #8831, .F. ) ;
#34066 = VECTOR ( 'NONE', #65480, 1000.000000000000000 ) ;
#34067 = LINE ( 'NONE', #55509, #39593 ) ;
#34068 = DIRECTION ( 'NONE',  ( 0.9989930665413143673, 0.04486483035051862939, 0.000000000000000000 ) ) ;
#34069 = DIRECTION ( 'NONE',  ( 0.9909497617679332571, 0.1342332658176667581, 2.500042656554810340E-16 ) ) ;
#34070 = AXIS2_PLACEMENT_3D ( 'NONE', #43819, #28352, #7946 ) ;
#34071 = CARTESIAN_POINT ( 'NONE',  ( -35.17600017528511813, 10.23461991275926941, -49.32454204471093107 ) ) ;
#34072 = CARTESIAN_POINT ( 'NONE',  ( -98.59957010994544646, 30.95006567008976717, 85.16634146005831951 ) ) ;
#34073 = CARTESIAN_POINT ( 'NONE',  ( -7.916219337932451694, 0.000000000000000000, 6.110112224316693208 ) ) ;
#34074 = VECTOR ( 'NONE', #4028, 1000.000000000000000 ) ;
#34075 = DIRECTION ( 'NONE',  ( -1.469488203625031485E-16, 2.022576995815118308E-16, 1.000000000000000000 ) ) ;
#34076 = CARTESIAN_POINT ( 'NONE',  ( -61.68940124183719576, 17.61226241086874467, 94.99999999999866418 ) ) ;
#34077 = EDGE_CURVE ( 'NONE', #3372, #8866, #41524, .T. ) ;
#34078 = ORIENTED_EDGE ( 'NONE', *, *, #31696, .T. ) ;
#34080 = DIRECTION ( 'NONE',  ( 0.000000000000000000, 0.000000000000000000, 1.000000000000000000 ) ) ;
#34079 = VECTOR ( 'NONE', #58998, 1000.000000000000000 ) ;
#34081 = VERTEX_POINT ( 'NONE', #60165 ) ;
#34082 = CARTESIAN_POINT ( 'NONE',  ( 36.76746179515745183, 8.081433644308903652, 44.44018405963787188 ) ) ;
#34083 = AXIS2_PLACEMENT_3D ( 'NONE', #47152, #48512, #32026 ) ;
#34084 = DIRECTION ( 'NONE',  ( 0.000000000000000000, 0.000000000000000000, 1.000000000000000000 ) ) ;
#34085 = ADVANCED_FACE ( 'NONE', ( #11984, #33455 ), #12335, .T. ) ;
#34086 = FACE_OUTER_BOUND ( 'NONE', #55774, .T. ) ;
#34087 = CARTESIAN_POINT ( 'NONE',  ( 0.7145311798163268557, -9.237604307034018802, 5.946466066724412554E-16 ) ) ;
#34088 = EDGE_CURVE ( 'NONE', #62698, #26121, #23088, .T. ) ;
#34089 = CARTESIAN_POINT ( 'NONE',  ( 60.00000000000000000, 7.347880794884118356E-15, -5.000000000000000000 ) ) ;
#34090 = CARTESIAN_POINT ( 'NONE',  ( 0.000000000000000000, 0.000000000000000000, 25.00000000000007816 ) ) ;
#34091 = CARTESIAN_POINT ( 'NONE',  ( -8.314488422519710653, 7.931352979988683494, -50.41807073194384969 ) ) ;
#34092 = AXIS2_PLACEMENT_3D ( 'NONE', #23785, #56133, #6901 ) ;
#34093 = CARTESIAN_POINT ( 'NONE',  ( 151.6192474229129630, 53.24103268919210308, -48.32307074035101380 ) ) ;
#34094 = DIRECTION ( 'NONE',  ( 0.000000000000000000, -1.000000000000000000, 0.000000000000000000 ) ) ;
#34095 = VERTEX_POINT ( 'NONE', #19688 ) ;
#34096 = DIRECTION ( 'NONE',  ( -0.000000000000000000, -1.000000000000000000, -0.000000000000000000 ) ) ;
#34097 = CARTESIAN_POINT ( 'NONE',  ( -439.4229916354184979, 400.0000000000065370, -133.9497041420121377 ) ) ;
#34098 = ORIENTED_EDGE ( 'NONE', *, *, #29858, .T. ) ;
#34099 = LINE ( 'NONE', #50268, #34227 ) ;
#34100 = DIRECTION ( 'NONE',  ( 1.000000000000000000, 1.387778780781448634E-16, -1.387778780781445676E-15 ) ) ;
#34101 = DIRECTION ( 'NONE',  ( -0.000000000000000000, 1.000000000000000000, -0.000000000000000000 ) ) ;
#34102 = EDGE_LOOP ( 'NONE', ( #6876, #6628 ) ) ;
#34103 = CARTESIAN_POINT ( 'NONE',  ( -86.10361028793440141, 25.29528064050660419, 36.91651998496248410 ) ) ;
#34104 = CARTESIAN_POINT ( 'NONE',  ( -10.46803069297985900, 7.077485182625207649, -62.73931412836061838 ) ) ;
#34105 = CARTESIAN_POINT ( 'NONE',  ( 41.80372346091801461, 9.750024116765237281, 44.52309710506295204 ) ) ;
#34106 = CARTESIAN_POINT ( 'NONE',  ( 140.0614732283738704, 45.29930344725071478, -47.74382409638028690 ) ) ;
#34107 = ORIENTED_EDGE ( 'NONE', *, *, #58658, .T. ) ;
#34108 = CARTESIAN_POINT ( 'NONE',  ( -125.0000000000000000, 0.000000000000000000, -10.00000000000000000 ) ) ;
#34109 = VERTEX_POINT ( 'NONE', #35175 ) ;
#34110 = LINE ( 'NONE', #1750, #39073 ) ;
#34111 = DIRECTION ( 'NONE',  ( -0.000000000000000000, -0.000000000000000000, -1.000000000000000000 ) ) ;
#34112 = CARTESIAN_POINT ( 'NONE',  ( -5.417282889646091171, 7.753782747238993522, 17.87817252730139828 ) ) ;
#34113 = CARTESIAN_POINT ( 'NONE',  ( -1.328627985309865034, 7.561890325089884790, 60.70477836359661694 ) ) ;
#34114 = EDGE_CURVE ( 'NONE', #35973, #13434, #38416, .T. ) ;
#34115 = CARTESIAN_POINT ( 'NONE',  ( 198.4963257495732023, 99.83071316188434707, -93.29099697683768966 ) ) ;
#34116 = CARTESIAN_POINT ( 'NONE',  ( -452.6627218934859798, 400.0000000000064801, -146.4497041420121377 ) ) ;
#34117 = ORIENTED_EDGE ( 'NONE', *, *, #21529, .F. ) ;
#34118 = STYLED_ITEM ( 'NONE', ( #30037 ), #41410 ) ;
#34119 = CARTESIAN_POINT ( 'NONE',  ( -36.11269837220804391, 20.55634918610408945, 85.00100000000000477 ) ) ;
#34120 = ORIENTED_EDGE ( 'NONE', *, *, #11262, .T. ) ;
#34121 = CARTESIAN_POINT ( 'NONE',  ( 164.6406716478537646, 63.44801348349338355, -18.99558380653978418 ) ) ;
#34122 = DIRECTION ( 'NONE',  ( -0.000000000000000000, 0.000000000000000000, 1.000000000000000000 ) ) ;
#34123 = CIRCLE ( 'NONE', #7146, 24.99999999999985434 ) ;
#34124 = CARTESIAN_POINT ( 'NONE',  ( 63.98009977735161158, 12.89803120691696314, 56.70387718321437376 ) ) ;
#34125 = CARTESIAN_POINT ( 'NONE',  ( 136.1310312718402429, 42.81430973242788696, -63.20608120636161686 ) ) ;
#34126 = DIRECTION ( 'NONE',  ( 1.000000000000000000, 0.000000000000000000, 0.000000000000000000 ) ) ;
#34127 = CIRCLE ( 'NONE', #22863, 4.999999999999997335 ) ;
#34128 = ORIENTED_EDGE ( 'NONE', *, *, #59778, .F. ) ;
#34129 = AXIS2_PLACEMENT_3D ( 'NONE', #37251, #58702, #53767 ) ;
#34130 = VERTEX_POINT ( 'NONE', #24293 ) ;
#34131 = VECTOR ( 'NONE', #51507, 1000.000000000000000 ) ;
#34132 = CARTESIAN_POINT ( 'NONE',  ( 10.83046137699561484, 6.392429922561258415, 43.16356064574667073 ) ) ;
#34133 = ORIENTED_EDGE ( 'NONE', *, *, #69229, .F. ) ;
#34134 = CARTESIAN_POINT ( 'NONE',  ( -61.52143283897137138, 16.51181063611438304, -73.36460479103185151 ) ) ;
#34135 = DIRECTION ( 'NONE',  ( 1.000000000000000000, 0.000000000000000000, 0.000000000000000000 ) ) ;
#34136 = AXIS2_PLACEMENT_3D ( 'NONE', #49217, #22503, #33064 ) ;
#34137 = B_SPLINE_CURVE_WITH_KNOTS ( 'NONE', 3,
 ( #15766, #21725, #27697, #64298, #47768, #43175, #42500, #49138 ),
 .UNSPECIFIED., .F., .F.,
 ( 4, 2, 2, 4 ),
 ( 0.004673709593152181735, 0.005837709341827665953, 0.007001709090503150171, 0.009329708587854116872 ),
 .UNSPECIFIED. ) ;
#34138 = ORIENTED_EDGE ( 'NONE', *, *, #68835, .T. ) ;
#34139 = CARTESIAN_POINT ( 'NONE',  ( -147.3641864666714980, 62.38213854487952403, -76.35815727694746613 ) ) ;
#34140 = CARTESIAN_POINT ( 'NONE',  ( 89.21005684773506061, 20.31770592753387206, 3.321479991859375591 ) ) ;
#34141 = EDGE_CURVE ( 'NONE', #35908, #45811, #14421, .T. ) ;
#34142 = DIRECTION ( 'NONE',  ( -0.000000000000000000, -0.000000000000000000, -1.000000000000000000 ) ) ;
#34143 = ORIENTED_EDGE ( 'NONE', *, *, #65424, .T. ) ;
#34144 = DIRECTION ( 'NONE',  ( 1.000000000000000000, 0.000000000000000000, -0.000000000000000000 ) ) ;
#34145 = ADVANCED_FACE ( 'NONE', ( #34845 ), #19000, .F. ) ;
#34146 = CARTESIAN_POINT ( 'NONE',  ( 62.38471166598394291, 13.55946638994290154, 83.52142562900598932 ) ) ;
#34147 = CARTESIAN_POINT ( 'NONE',  ( 37.46876540261052924, 9.179568636624026112, 30.16313010050332011 ) ) ;
#34148 = CARTESIAN_POINT ( 'NONE',  ( -180.6158171975815208, 97.47361786002628037, -42.53633187762700629 ) ) ;
#34149 = ADVANCED_FACE ( 'NONE', ( #19340 ), #40796, .T. ) ;
#34150 = CARTESIAN_POINT ( 'NONE',  ( -133.3392045760936639, 51.59583146030205825, -16.62341006324014359 ) ) ;
#34151 = CARTESIAN_POINT ( 'NONE',  ( -143.7563954441272926, 59.45082218538873065, -91.18228907187790355 ) ) ;
#34152 = APPLICATION_CONTEXT ( 'automotive_design' ) ;
#34153 = DIRECTION ( 'NONE',  ( 0.000000000000000000, 0.000000000000000000, -1.000000000000000000 ) ) ;
#34154 = EDGE_LOOP ( 'NONE', ( #61818, #62423, #15451, #58308 ) ) ;
#34155 = CARTESIAN_POINT ( 'NONE',  ( 141.2801018238827169, 47.29457739955284268, -69.26552387562287549 ) ) ;
#34156 = DIRECTION ( 'NONE',  ( 0.000000000000000000, 0.000000000000000000, 1.000000000000000000 ) ) ;
#34157 = ORIENTED_EDGE ( 'NONE', *, *, #46843, .F. ) ;
#34158 = EDGE_CURVE ( 'NONE', #61600, #28307, #47354, .T. ) ;
#34159 = CARTESIAN_POINT ( 'NONE',  ( -157.0079874970173250, 72.18249880494042259, -42.03918860550044911 ) ) ;
#34160 = CARTESIAN_POINT ( 'NONE',  ( 208.5884523568772124, 113.6152425727545108, -10.55554601564709749 ) ) ;
#34161 = CARTESIAN_POINT ( 'NONE',  ( -33.85171821065139852, 11.02091558840053942, 44.83441027425075731 ) ) ;
#34162 = CARTESIAN_POINT ( 'NONE',  ( -169.1041038606267080, 82.76530082651281361, -48.56111750552656048 ) ) ;
#34163 = CARTESIAN_POINT ( 'NONE',  ( 86.62931800182293784, -170.0000000000000000, -43.32156419891173016 ) ) ;
#34164 = CARTESIAN_POINT ( 'NONE',  ( -13.72143910172259318, 7.346845691402125844, -91.95266834806231770 ) ) ;
#34165 = CARTESIAN_POINT ( 'NONE',  ( -50.13771638889892301, 13.41835215703893702, -63.87468226647597902 ) ) ;
#34166 = CARTESIAN_POINT ( 'NONE',  ( -0.5783162822156591165, 7.534184941292927817, -14.12672653011558488 ) ) ;
#34167 = CARTESIAN_POINT ( 'NONE',  ( -15.32584732649904247, 8.506915958926390076, 38.10398657133274014 ) ) ;
#34168 = CARTESIAN_POINT ( 'NONE',  ( 117.6865880453675999, 32.48051379280607165, 9.211411928219352063 ) ) ;
#34169 = DIRECTION ( 'NONE',  ( 0.000000000000000000, 1.000000000000000000, 0.000000000000000000 ) ) ;
#34170 = ORIENTED_EDGE ( 'NONE', *, *, #20278, .F. ) ;
#34171 = STYLED_ITEM ( 'NONE', ( #12653 ), #41867 ) ;
#34172 = CARTESIAN_POINT ( 'NONE',  ( -94.83794676023109105, 30.26879337035744655, -41.45177952449644465 ) ) ;
#34173 = ORIENTED_EDGE ( 'NONE', *, *, #68780, .F. ) ;
#34174 = DIRECTION ( 'NONE',  ( -0.6910626489868685329, 0.7227948638273878901, 0.000000000000000000 ) ) ;
#34175 = EDGE_CURVE ( 'NONE', #3914, #18610, #31973, .T. ) ;
#34176 = CARTESIAN_POINT ( 'NONE',  ( 84.27937148876360141, 19.69225537006224869, -77.29251801931836496 ) ) ;
#34177 = LINE ( 'NONE', #28896, #20365 ) ;
#34178 = CARTESIAN_POINT ( 'NONE',  ( 432.4999999999999432, -18.06806526123148160, 380.0000000000000000 ) ) ;
#34179 = CARTESIAN_POINT ( 'NONE',  ( -2.999999999999994227, 0.000000000000000000, -20.30000000000000071 ) ) ;
#34180 = DIRECTION ( 'NONE',  ( 0.000000000000000000, 0.000000000000000000, -1.000000000000000000 ) ) ;
#34181 = AXIS2_PLACEMENT_3D ( 'NONE', #11391, #11054, #53946 ) ;
#34182 = CARTESIAN_POINT ( 'NONE',  ( 56.31655686453512288, 12.24428004209404897, -93.43573692067893433 ) ) ;
#34183 = CARTESIAN_POINT ( 'NONE',  ( -25.87147652227456263, 70.00000000000000000, 129.5802547743875550 ) ) ;
#34184 = VERTEX_POINT ( 'NONE', #36567 ) ;
#34185 = CONICAL_SURFACE ( 'NONE', #21798, 8.000000000000000000, 1.047197551196600296 ) ;
#34186 = VERTEX_POINT ( 'NONE', #42522 ) ;
#34187 = B_SPLINE_CURVE_WITH_KNOTS ( 'NONE', 3,
 ( #3293, #23706, #66628, #13499, #66982, #18424, #45850, #39877, #34956, #8223, #29671, #13158, #34623, #67325, #56061, #7876, #51133, #40230, #51484, #2949, #29326, #45497, #24751, #14193, #8917, #19111, #51819, #62018, #13837, #35300, #42970, #52509, #21525, #5006, #41956, #63418, #69373, #26472, #15222, #58463, #14869, #53177, #3982, #68, #36688, #47221, #9256, #4661, #53529, #58135, #9951, #31407, #46891, #64441, #25793, #52837, #52165, #15911, #31069, #25452, #47909, #5358, #4332, #63065, #36337, #26812, #37025, #26123, #16251 ),
 .UNSPECIFIED., .F., .F.,
 ( 4, 2, 2, 2, 2, 2, 1, 2, 2, 2, 2, 2, 2, 2, 2, 2, 2, 2, 2, 2, 2, 2, 2, 2, 2, 2, 2, 2, 2, 2, 2, 2, 2, 2, 4 ),
 ( 0.000000000000000000, 0.001221101243989660551, 0.001831651865984463287, 0.002442202487979266024, 0.003663303731968859788, 0.004273854353963660140, 0.004884404975958460925, 0.005494955597953261710, 0.006105506219948060760, 0.007326607463937678810, 0.007937158085932474391, 0.008547708707927269972, 0.009768809951916843787, 0.01098991119590641587, 0.01221101243989598968, 0.01343211368388556523, 0.01465321492787513905, 0.01709541741585432484, 0.01831651865984389171, 0.01953761990383345165, 0.02197982239181260622, 0.02320092363580220085, 0.02442202487979178854, 0.02564312612378137970, 0.02686422736777097434, 0.02930642985575018095, 0.03174863234372939103, 0.03296973358771899260, 0.03358028420971379685, 0.03419083483170859417, 0.03541193607569825125, 0.03602248669769304856, 0.03663303731968785282, 0.03785413856367740582, 0.03907523980766696575 ),
 .UNSPECIFIED. ) ;
#34188 = CARTESIAN_POINT ( 'NONE',  ( -447.6627218934913799, 0.000000000000000000, -116.4497041420118393 ) ) ;
#34189 = CARTESIAN_POINT ( 'NONE',  ( 175.5493994043409032, 73.18740965572595769, 68.72061911442422399 ) ) ;
#34190 = CARTESIAN_POINT ( 'NONE',  ( 43.35276089251598819, 8.955376472641077612, -90.37929691252209352 ) ) ;
#34191 = CARTESIAN_POINT ( 'NONE',  ( 102.7983318509014623, 26.68040613344513545, 62.90955133405510935 ) ) ;
#34192 = AXIS2_PLACEMENT_3D ( 'NONE', #15084, #10833, #69566 ) ;
#34193 = CARTESIAN_POINT ( 'NONE',  ( -166.5742238910466142, 81.57147158222490191, -19.03685731792293012 ) ) ;
#34194 = DIRECTION ( 'NONE',  ( -0.000000000000000000, -0.000000000000000000, -1.000000000000000000 ) ) ;
#34195 = ORIENTED_EDGE ( 'NONE', *, *, #57690, .F. ) ;
#34196 = CARTESIAN_POINT ( 'NONE',  ( 88.98820631332498010, 21.30618275724810573, 3.231923812655122852 ) ) ;
#34197 = CARTESIAN_POINT ( 'NONE',  ( -14.66033866466834645, 7.432913330382390882, 61.36269437948495664 ) ) ;
#34198 = CARTESIAN_POINT ( 'NONE',  ( 12.91653430408660874, 7.431946598423014194, 57.41795537130889215 ) ) ;
#34199 = LINE ( 'NONE', #23639, #18341 ) ;
#34200 = DIRECTION ( 'NONE',  ( -0.000000000000000000, -0.9989683093773507050, -0.04541273895899305274 ) ) ;
#34201 = FACE_BOUND ( 'NONE', #32816, .T. ) ;
#34202 = ORIENTED_EDGE ( 'NONE', *, *, #13292, .F. ) ;
#34203 = CARTESIAN_POINT ( 'NONE',  ( 13.24564585880038514, 63.65041531508843065, 43.58025477438756923 ) ) ;
#34204 = CARTESIAN_POINT ( 'NONE',  ( 0.000000000000000000, 0.000000000000000000, -9.500000000000000000 ) ) ;
#34205 = LINE ( 'NONE', #61622, #61091 ) ;
#34206 = CARTESIAN_POINT ( 'NONE',  ( -178.2328124332056234, 94.56955476227571467, 5.969047184286479180 ) ) ;
#34207 = CARTESIAN_POINT ( 'NONE',  ( 206.2957331585309362, 110.2946564621822887, 56.17913581376664212 ) ) ;
#34208 = CARTESIAN_POINT ( 'NONE',  ( 84.74140601443113496, 18.78541996275572856, -62.90364757930472450 ) ) ;
#34209 = ORIENTED_EDGE ( 'NONE', *, *, #54445, .T. ) ;
#34210 = CARTESIAN_POINT ( 'NONE',  ( 197.1975259970232344, 98.19639476549652102, -43.49939252954278146 ) ) ;
#34211 = VERTEX_POINT ( 'NONE', #291 ) ;
#34212 = CARTESIAN_POINT ( 'NONE',  ( 108.7067726706416977, 29.28183711776652132, -89.72851832208228018 ) ) ;
#34213 = ORIENTED_EDGE ( 'NONE', *, *, #44792, .F. ) ;
#34214 = VECTOR ( 'NONE', #49425, 1000.000000000000000 ) ;
#34215 = LINE ( 'NONE', #1865, #53222 ) ;
#34216 = DIRECTION ( 'NONE',  ( 1.604841615724182364E-15, 1.000000000000000000, 0.000000000000000000 ) ) ;
#34217 = LINE ( 'NONE', #28585, #6626 ) ;
#34218 = ORIENTED_EDGE ( 'NONE', *, *, #10925, .T. ) ;
#34219 = VERTEX_POINT ( 'NONE', #53750 ) ;
#34220 = CARTESIAN_POINT ( 'NONE',  ( 38.91493890549797641, 8.346224043800601677, -23.77526687496409963 ) ) ;
#34221 = DIRECTION ( 'NONE',  ( 0.000000000000000000, -1.000000000000000000, 0.000000000000000000 ) ) ;
#34222 = CARTESIAN_POINT ( 'NONE',  ( -155.7457403566965297, 71.01814553754120141, -73.35110919937355334 ) ) ;
#34223 = CARTESIAN_POINT ( 'NONE',  ( 66.94365390260637128, 14.65531706601758977, 4.074685676838114112 ) ) ;
#34224 = CARTESIAN_POINT ( 'NONE',  ( 152.6804161981488619, 55.27286404993338209, 4.288696971359757804 ) ) ;
#34225 = VERTEX_POINT ( 'NONE', #10162 ) ;
#34226 = VECTOR ( 'NONE', #40058, 1000.000000000000227 ) ;
#34227 = VECTOR ( 'NONE', #28819, 1000.000000000000000 ) ;
#34228 = ADVANCED_FACE ( 'NONE', ( #53522 ), #31624, .F. ) ;
#34229 = SURFACE_STYLE_USAGE ( .BOTH. , #51096 ) ;
#34230 = LINE ( 'NONE', #44059, #26421 ) ;
#34231 = VECTOR ( 'NONE', #13873, 1000.000000000000114 ) ;
#34232 = CARTESIAN_POINT ( 'NONE',  ( -133.3220917939969183, 52.82057604964899866, -14.49950751745602950 ) ) ;
#34233 = LINE ( 'NONE', #12075, #13879 ) ;
#34234 = CARTESIAN_POINT ( 'NONE',  ( 115.7746371641014775, 31.52600568297705408, -11.48978713420478925 ) ) ;
#34235 = CARTESIAN_POINT ( 'NONE',  ( 94.12361176368516169, 22.11573381981098052, 90.45082768725070821 ) ) ;
#34237 = ORIENTED_EDGE ( 'NONE', *, *, #4740, .F. ) ;
#34236 = FACE_OUTER_BOUND ( 'NONE', #37786, .T. ) ;
#34238 = VERTEX_POINT ( 'NONE', #15108 ) ;
#34239 = ADVANCED_FACE ( 'NONE', ( #9835 ), #15791, .F. ) ;
#34240 = VERTEX_POINT ( 'NONE', #15456 ) ;
#34241 = CARTESIAN_POINT ( 'NONE',  ( 42.70988075781782101, 8.862408058333491212, 3.820616178905913873 ) ) ;
#34242 = CARTESIAN_POINT ( 'NONE',  ( -180.6289110087067797, 97.48982472183162429, 92.17219495999866297 ) ) ;
#34243 = LINE ( 'NONE', #2233, #4196 ) ;
#34244 = CARTESIAN_POINT ( 'NONE',  ( 104.3805245147141676, 26.26278144139197934, -21.28214446120828285 ) ) ;
#34245 = CARTESIAN_POINT ( 'NONE',  ( 198.4017331595409246, 98.09114638179336509, 5.778807527766608665 ) ) ;
#34246 = CARTESIAN_POINT ( 'NONE',  ( -55.05276343752909440, 15.72344139423349141, -35.21632399845986328 ) ) ;
#34247 = DIRECTION ( 'NONE',  ( -1.000000000000000000, 0.000000000000000000, 0.000000000000000000 ) ) ;
#34248 = CARTESIAN_POINT ( 'NONE',  ( -72.20490592113145567, 19.96451062593610004, -65.62012688376218250 ) ) ;
#34249 = CARTESIAN_POINT ( 'NONE',  ( 8.000000000000007105, 249.8719672152120381, -95.00000000000133582 ) ) ;
#34250 = ORIENTED_EDGE ( 'NONE', *, *, #13961, .F. ) ;
#34251 = DIRECTION ( 'NONE',  ( -1.000000000000000000, -1.776356839400250465E-15, 0.000000000000000000 ) ) ;
#34252 = VERTEX_POINT ( 'NONE', #11192 ) ;
#34253 = ORIENTED_EDGE ( 'NONE', *, *, #63113, .F. ) ;
#34254 = EDGE_CURVE ( 'NONE', #69216, #49946, #64052, .T. ) ;
#34255 = DIRECTION ( 'NONE',  ( 0.000000000000000000, 1.232595164407830672E-32, 1.000000000000000000 ) ) ;
#34256 = CARTESIAN_POINT ( 'NONE',  ( 181.0840389613909736, 80.03940679743416808, -78.06960825634331513 ) ) ;
#34257 = CARTESIAN_POINT ( 'NONE',  ( -166.2053056899075045, 81.18967388993343093, 35.40543396571913348 ) ) ;
#34258 = CARTESIAN_POINT ( 'NONE',  ( -99.98930671699736195, 31.63190627461932891, -49.67157807265856917 ) ) ;
#34259 = FACE_OUTER_BOUND ( 'NONE', #31937, .T. ) ;
#34260 = DIRECTION ( 'NONE',  ( 0.000000000000000000, 0.000000000000000000, 1.000000000000000000 ) ) ;
#34261 = CARTESIAN_POINT ( 'NONE',  ( 140.4641697461913168, 46.75994457266055093, -13.09221936645533368 ) ) ;
#34262 = EDGE_LOOP ( 'NONE', ( #22427, #31431, #17283, #59089 ) ) ;
#34263 = VERTEX_POINT ( 'NONE', #38993 ) ;
#34264 = EDGE_LOOP ( 'NONE', ( #17482, #61432 ) ) ;
#34265 = VECTOR ( 'NONE', #37585, 1000.000000000000000 ) ;
#34266 = FACE_OUTER_BOUND ( 'NONE', #10510, .T. ) ;
#34267 = DIRECTION ( 'NONE',  ( 2.437361367520478414E-16, 5.563118268672117023E-17, 1.000000000000000000 ) ) ;
#34268 = LINE ( 'NONE', #13839, #17646 ) ;
#34269 = CARTESIAN_POINT ( 'NONE',  ( 93.85477471612979627, 23.08982334209078147, -95.00000000000133582 ) ) ;
#34270 = VECTOR ( 'NONE', #14140, 1000.000000000000000 ) ;
#34271 = DIRECTION ( 'NONE',  ( -1.000000000000000000, 0.000000000000000000, 0.000000000000000000 ) ) ;
#34272 = CARTESIAN_POINT ( 'NONE',  ( 199.9103251464699440, 101.6434290204575603, 69.33018220824747857 ) ) ;
#34273 = ORIENTED_EDGE ( 'NONE', *, *, #46385, .F. ) ;
#34274 = LINE ( 'NONE', #56070, #5323 ) ;
#34275 = CIRCLE ( 'NONE', #66872, 60.00000000000000000 ) ;
#34276 = CARTESIAN_POINT ( 'NONE',  ( -60.98168946575806615, 17.40090852531920618, -64.94124262262964464 ) ) ;
#34277 = CARTESIAN_POINT ( 'NONE',  ( 197.2199163281727863, 98.22431253015348318, -71.33388331724441400 ) ) ;
#34278 = CARTESIAN_POINT ( 'NONE',  ( -179.5178913137216909, 94.54206947403388028, -38.25780915961179574 ) ) ;
#34279 = CARTESIAN_POINT ( 'NONE',  ( 102.8066580714140485, 25.59117171226998266, 9.258329190121406427 ) ) ;
#34280 = CARTESIAN_POINT ( 'NONE',  ( -170.2801941679961146, 84.02053682015869640, 4.523125458188938630 ) ) ;
#34281 = CARTESIAN_POINT ( 'NONE',  ( -173.1211646369891355, 88.63826465341151106, -22.86740657428632773 ) ) ;
#34282 = FACE_BOUND ( 'NONE', #16921, .T. ) ;
#34284 = CARTESIAN_POINT ( 'NONE',  ( -189.3456113063706709, 107.2364438114461791, 93.44106408251658991 ) ) ;
#34283 = B_SPLINE_CURVE_WITH_KNOTS ( 'NONE', 3,
 ( #49531, #44263, #66104, #62185, #35813, #15043, #56565, #36498, #14690, #24913, #4148, #8742, #51303, #67477, #46699, #35461, #20312, #57950 ),
 .UNSPECIFIED., .F., .F.,
 ( 4, 2, 2, 2, 2, 2, 2, 2, 4 ),
 ( 0.01368524652304596405, 0.01545087154706958552, 0.01721649657109320872, 0.02074774661914039961, 0.02251337164316399506, 0.02427899666718758703, 0.02604462169121118595, 0.02692743420322298367, 0.02781024671523478140 ),
 .UNSPECIFIED. ) ;
#34285 = CIRCLE ( 'NONE', #54481, 498.0000000000000000 ) ;
#34286 = VECTOR ( 'NONE', #58225, 1000.000000000000000 ) ;
#34287 = CARTESIAN_POINT ( 'NONE',  ( -0.5780275525703854056, 6.527356703336898214, 62.51425872000311301 ) ) ;
#34288 = ORIENTED_EDGE ( 'NONE', *, *, #36705, .F. ) ;
#34289 = FACE_OUTER_BOUND ( 'NONE', #34295, .T. ) ;
#34290 = CYLINDRICAL_SURFACE ( 'NONE', #18402, 89.99999999999997158 ) ;
#34291 = LINE ( 'NONE', #39215, #16327 ) ;
#34292 = DIRECTION ( 'NONE',  ( -1.000000000000000000, 0.000000000000000000, 0.000000000000000000 ) ) ;
#34293 = CARTESIAN_POINT ( 'NONE',  ( 59.72647370436682479, 12.96353798836696214, -63.32053846355550775 ) ) ;
#34294 = ADVANCED_FACE ( 'NONE', ( #59722 ), #6266, .F. ) ;
#34295 = EDGE_LOOP ( 'NONE', ( #63046, #228, #68307, #37874 ) ) ;
#34296 = DIRECTION ( 'NONE',  ( 0.000000000000000000, 0.000000000000000000, -1.000000000000000000 ) ) ;
#34297 = DIRECTION ( 'NONE',  ( -0.000000000000000000, 1.000000000000000000, -0.000000000000000000 ) ) ;
#34298 = ORIENTED_EDGE ( 'NONE', *, *, #62017, .T. ) ;
#34299 = B_SPLINE_CURVE_WITH_KNOTS ( 'NONE', 3,
 ( #66634, #6488, #33230, #60646, #12818, #34630 ),
 .UNSPECIFIED., .F., .F.,
 ( 4, 2, 4 ),
 ( 0.008240550023493531037, 0.01057684187039406240, 0.01291313371729459550 ),
 .UNSPECIFIED. ) ;
#34300 = EDGE_CURVE ( 'NONE', #66403, #11659, #27723, .T. ) ;
#34301 = EDGE_LOOP ( 'NONE', ( #68255, #11469 ) ) ;
#34302 = CARTESIAN_POINT ( 'NONE',  ( 173.6718135456487175, 71.42581476597410983, -42.54376570200113150 ) ) ;
#34303 = CARTESIAN_POINT ( 'NONE',  ( 150.4542242713869484, 53.63744268572195750, 39.57349238810517988 ) ) ;
#34304 = CARTESIAN_POINT ( 'NONE',  ( 64.16679220703369424, 10.37413986118183828, 40.00000000000003553 ) ) ;
#34305 = EDGE_LOOP ( 'NONE', ( #15002, #35007, #32833, #56878 ) ) ;
#34306 = FACE_OUTER_BOUND ( 'NONE', #44891, .T. ) ;
#34307 = DIRECTION ( 'NONE',  ( 1.000000000000000000, 0.000000000000000000, 0.000000000000000000 ) ) ;
#34308 = CARTESIAN_POINT ( 'NONE',  ( -0.7215816834507559063, 6.532459459468096696, 8.353057134836445741 ) ) ;
#34309 = CARTESIAN_POINT ( 'NONE',  ( -55.05276343752910151, -170.0000000000000000, -77.06087458892358200 ) ) ;
#34310 = CARTESIAN_POINT ( 'NONE',  ( -28.13128612339709278, 10.08889185338652972, -9.223690606770793110 ) ) ;
#34311 = CARTESIAN_POINT ( 'NONE',  ( -51.34542473642584781, 14.75635007918830155, -22.39598248981539541 ) ) ;
#34312 = EDGE_CURVE ( 'NONE', #65175, #10742, #22413, .T. ) ;
#34313 = VERTEX_POINT ( 'NONE', #7329 ) ;
#34314 = EDGE_CURVE ( 'NONE', #57172, #58537, #40511, .T. ) ;
#34315 = LINE ( 'NONE', #39924, #7611 ) ;
#34316 = CIRCLE ( 'NONE', #43261, 245.3095347406802205 ) ;
#34317 = CARTESIAN_POINT ( 'NONE',  ( -75.43495400358860081, 22.18831810339350952, 4.301192105811935562 ) ) ;
#34318 = CARTESIAN_POINT ( 'NONE',  ( 73.57152302639913444, -14.62167909564502821, 170.0000000000000000 ) ) ;
#34319 = CARTESIAN_POINT ( 'NONE',  ( -166.3205068063721512, 81.30869308872871670, -72.23115024874353196 ) ) ;
#34320 = CIRCLE ( 'NONE', #3987, 246.3582898394607525 ) ;
#34322 = EDGE_LOOP ( 'NONE', ( #51514, #39923, #30551, #6113 ) ) ;
#34321 = CARTESIAN_POINT ( 'NONE',  ( -123.1591800884025218, 44.71875343686618010, 84.80057340962032697 ) ) ;
#34323 = CARTESIAN_POINT ( 'NONE',  ( 82.34195123877070444, 18.00239921638038965, -37.16307426115260171 ) ) ;
#34324 = EDGE_CURVE ( 'NONE', #7572, #56265, #35880, .T. ) ;
#34325 = AXIS2_PLACEMENT_3D ( 'NONE', #4922, #25015, #20759 ) ;
#34326 = VECTOR ( 'NONE', #40253, 1000.000000000000000 ) ;
#34327 = ORIENTED_EDGE ( 'NONE', *, *, #2055, .T. ) ;
#34328 = PLANE ( 'NONE',  #10996 ) ;
#34329 = CARTESIAN_POINT ( 'NONE',  ( 80.71682498289315788, 18.54204664833076066, 41.85293259918689301 ) ) ;
#34330 = DIRECTION ( 'NONE',  ( 1.000000000000000000, 0.000000000000000000, 0.000000000000000000 ) ) ;
#34331 = AXIS2_PLACEMENT_3D ( 'NONE', #66474, #39725, #2787 ) ;
#34333 = FACE_OUTER_BOUND ( 'NONE', #29924, .T. ) ;
#34332 = VECTOR ( 'NONE', #10077, 1000.000000000000000 ) ;
#34334 = SHAPE_REPRESENTATION ( 'cutting blade', ( #66832 ), #6181 ) ;
#34335 = CARTESIAN_POINT ( 'NONE',  ( 311.9975424824652350, 172.0000000000000284, 418.0000000000000568 ) ) ;
#34336 = CARTESIAN_POINT ( 'NONE',  ( 6.400000000000000355, 4.618802153517001408, -8.000000000000000000 ) ) ;
#34337 = CARTESIAN_POINT ( 'NONE',  ( 0.000000000000000000, 0.000000000000000000, 0.000000000000000000 ) ) ;
#34338 = AXIS2_PLACEMENT_3D ( 'NONE', #38100, #53916, #117 ) ;
#34339 = DIRECTION ( 'NONE',  ( -1.000000000000000000, -0.000000000000000000, -0.000000000000000000 ) ) ;
#34340 = ORIENTED_EDGE ( 'NONE', *, *, #38178, .T. ) ;
#34341 = VERTEX_POINT ( 'NONE', #17159 ) ;
#34342 = EDGE_CURVE ( 'NONE', #40287, #32688, #38632, .T. ) ;
#34343 = CARTESIAN_POINT ( 'NONE',  ( 102.8066580714140343, 25.59117171227001464, 62.94743037104881722 ) ) ;
#34344 = CARTESIAN_POINT ( 'NONE',  ( 162.7921669283190909, 61.91024532638674316, 58.46359787650868611 ) ) ;
#34346 = EDGE_CURVE ( 'NONE', #39218, #30581, #20446, .T. ) ;
#34345 = CARTESIAN_POINT ( 'NONE',  ( -12.99999999999999822, 84.99999999999998579, 82.99999999999998579 ) ) ;
#34347 = EDGE_CURVE ( 'NONE', #16942, #53544, #67132, .T. ) ;
#34348 = EDGE_CURVE ( 'NONE', #7089, #59608, #13985, .T. ) ;
#34349 = DIRECTION ( 'NONE',  ( -0.000000000000000000, -0.000000000000000000, -1.000000000000000000 ) ) ;
#34350 = CARTESIAN_POINT ( 'NONE',  ( 26.53820713381362140, 51.95411424136508316, 27.58472369392174173 ) ) ;
#34351 = CARTESIAN_POINT ( 'NONE',  ( -109.5142642360664667, 36.61018064014777451, 62.81589927390022865 ) ) ;
#34352 = CYLINDRICAL_SURFACE ( 'NONE', #39598, 7.500000000000020428 ) ;
#34353 = DIRECTION ( 'NONE',  ( -0.8160245890732938934, -0.5780171883497599028, 0.000000000000000000 ) ) ;
#34354 = ORIENTED_EDGE ( 'NONE', *, *, #22526, .F. ) ;
#34355 = ORIENTED_EDGE ( 'NONE', *, *, #46120, .T. ) ;
#34356 = VERTEX_POINT ( 'NONE', #45653 ) ;
#34357 = DIRECTION ( 'NONE',  ( -0.000000000000000000, 0.000000000000000000, -1.000000000000000000 ) ) ;
#34358 = CARTESIAN_POINT ( 'NONE',  ( -74.60184650407219920, 20.81479667884462614, 85.29625918890103264 ) ) ;
#34359 = LINE ( 'NONE', #6566, #35224 ) ;
#34360 = CARTESIAN_POINT ( 'NONE',  ( 130.7457207912710828, 40.74300766298683385, 30.17037958794855257 ) ) ;
#34361 = CARTESIAN_POINT ( 'NONE',  ( 106.6944765335652647, -21.67660392622676824, -3.765493530430633395 ) ) ;
#34362 = DIRECTION ( 'NONE',  ( -0.000000000000000000, 1.000000000000000000, -0.000000000000000000 ) ) ;
#34363 = CARTESIAN_POINT ( 'NONE',  ( -95.63694837622350065, 30.64472169584720618, -12.17974421549104314 ) ) ;
#34364 = CARTESIAN_POINT ( 'NONE',  ( 57.39233401791016576, 12.46575990788836918, 42.29982551114518685 ) ) ;
#34365 = DIRECTION ( 'NONE',  ( 1.000000000000000000, 0.000000000000000000, 0.000000000000000000 ) ) ;
#34366 = CARTESIAN_POINT ( 'NONE',  ( 447.3372781065085633, 400.0000000000000568, -116.4497041420118393 ) ) ;
#34367 = ORIENTED_EDGE ( 'NONE', *, *, #12858, .T. ) ;
#34368 = LINE ( 'NONE', #44905, #42984 ) ;
#34369 = DIRECTION ( 'NONE',  ( 1.000000000000000000, 0.000000000000000000, -0.000000000000000000 ) ) ;
#34370 = CARTESIAN_POINT ( 'NONE',  ( -15.27594996066616773, 8.502079791899641137, 9.781629159753414626 ) ) ;
#34371 = CARTESIAN_POINT ( 'NONE',  ( 0.000000000000000000, 0.000000000000000000, 170.0000000000000000 ) ) ;
#34372 = CARTESIAN_POINT ( 'NONE',  ( -102.7456062648101636, 33.01749955571779083, -76.85912785543966663 ) ) ;
#34373 = CARTESIAN_POINT ( 'NONE',  ( 126.4757069339777473, 38.29528077539270470, -18.03564317929428285 ) ) ;
#34374 = AXIS2_PLACEMENT_3D ( 'NONE', #21930, #64504, #15628 ) ;
#34375 = B_SPLINE_CURVE_WITH_KNOTS ( 'NONE', 3,
 ( #58777, #49611, #5331, #22546, #387, #26786, #42612, #37675 ),
 .UNSPECIFIED., .F., .F.,
 ( 4, 2, 2, 4 ),
 ( 0.01336725832182610388, 0.01453745201803767137, 0.01570764571424923886, 0.01804803310667237384 ),
 .UNSPECIFIED. ) ;
#34376 = EDGE_LOOP ( 'NONE', ( #28690, #58528, #4717, #17806, #29869, #58844, #17165, #4716 ) ) ;
#34377 = AXIS2_PLACEMENT_3D ( 'NONE', #37527, #16424, #54388 ) ;
#34378 = DIRECTION ( 'NONE',  ( -0.4127148655274873734, 0.9108602745606090290, 7.557850055494265064E-15 ) ) ;
#34379 = CARTESIAN_POINT ( 'NONE',  ( -189.5325095384513929, 107.4952257375067290, -13.13692968654411786 ) ) ;
#34380 = CARTESIAN_POINT ( 'NONE',  ( 447.3372781065086201, 217.8591479523844612, 78.55029585798806124 ) ) ;
#34381 = CARTESIAN_POINT ( 'NONE',  ( -447.6627218934889925, 395.0000000000064801, -141.4497041420092387 ) ) ;
#34382 = CARTESIAN_POINT ( 'NONE',  ( -167.9337388826115784, 81.53346785675708475, 86.55874306617425873 ) ) ;
#34383 = ORIENTED_EDGE ( 'NONE', *, *, #60993, .F. ) ;
#34385 = CARTESIAN_POINT ( 'NONE',  ( 23.09119322872580682, 7.852465917941087170, -95.00000000000133582 ) ) ;
#34384 = VECTOR ( 'NONE', #34014, 1000.000000000000000 ) ;
#34386 = VECTOR ( 'NONE', #31345, 1000.000000000000227 ) ;
#34387 = PRODUCT_DEFINITION_FORMATION_WITH_SPECIFIED_SOURCE ( 'ANY', '', #5169, .NOT_KNOWN. ) ;
#34388 = CARTESIAN_POINT ( 'NONE',  ( -142.0081215801269536, 58.07066293384865929, -15.76809686950948830 ) ) ;
#34389 = CIRCLE ( 'NONE', #22005, 2.999999999999981792 ) ;
#34390 = CARTESIAN_POINT ( 'NONE',  ( -2.873329055852807290, 7.626065826870673803, -75.41701928022413881 ) ) ;
#34391 = EDGE_CURVE ( 'NONE', #29060, #29497, #51282, .T. ) ;
#34392 = VECTOR ( 'NONE', #24388, 1000.000000000000000 ) ;
#34393 = CARTESIAN_POINT ( 'NONE',  ( 6.526941389886392386, -24.13294503563501436, 0.000000000000000000 ) ) ;
#34394 = VERTEX_POINT ( 'NONE', #36134 ) ;
#34395 = DIRECTION ( 'NONE',  ( -0.000000000000000000, -0.000000000000000000, -1.000000000000000000 ) ) ;
#34396 = CARTESIAN_POINT ( 'NONE',  ( 197.3707490726350215, 96.80690576410104597, -42.19351181672752205 ) ) ;
#34397 = DIRECTION ( 'NONE',  ( -1.000000000000000000, 0.000000000000000000, 0.000000000000000000 ) ) ;
#34398 = CARTESIAN_POINT ( 'NONE',  ( 19.75784582661440680, 6.660183274347837745, -36.65081142605392728 ) ) ;
#34400 = EDGE_LOOP ( 'NONE', ( #57429, #11520, #69271, #48123 ) ) ;
#34399 = CARTESIAN_POINT ( 'NONE',  ( 110.7167338301703694, 30.21148223254618159, 17.76666361527367499 ) ) ;
#34401 = EDGE_CURVE ( 'NONE', #3129, #3906, #31410, .T. ) ;
#34402 = CARTESIAN_POINT ( 'NONE',  ( 57.39083379741711610, 11.43779987330584724, 32.32724278055570721 ) ) ;
#34403 = EDGE_CURVE ( 'NONE', #28975, #4035, #65091, .T. ) ;
#34404 = EDGE_LOOP ( 'NONE', ( #27853, #4715 ) ) ;
#34406 = ORIENTED_EDGE ( 'NONE', *, *, #62455, .F. ) ;
#34405 = EDGE_CURVE ( 'NONE', #33323, #39735, #41503, .T. ) ;
#34407 = CARTESIAN_POINT ( 'NONE',  ( 173.8623159076320235, 72.97967239795021044, 34.76400434874135215 ) ) ;
#34408 = CARTESIAN_POINT ( 'NONE',  ( 18.21423326326598158, 6.590134686181414736, -62.74990453328492634 ) ) ;
#34409 = ADVANCED_FACE ( 'NONE', ( #67803 ), #67461, .F. ) ;
#34411 = ORIENTED_EDGE ( 'NONE', *, *, #48102, .F. ) ;
#34410 = CARTESIAN_POINT ( 'NONE',  ( -8.800520192024519517, 7.964629484975260354, -77.21523971768127126 ) ) ;
#34412 = CARTESIAN_POINT ( 'NONE',  ( -94.82531008173683063, 30.26290669250042598, 90.82179001772281879 ) ) ;
#34413 = DIRECTION ( 'NONE',  ( 0.000000000000000000, -0.000000000000000000, -1.000000000000000000 ) ) ;
#34414 = CARTESIAN_POINT ( 'NONE',  ( -71.15374617000811952, 20.66492714610676273, -42.60528795093121346 ) ) ;
#34415 = ORIENTED_EDGE ( 'NONE', *, *, #49796, .F. ) ;
#34416 = B_SPLINE_CURVE_WITH_KNOTS ( 'NONE', 3,
 ( #55024, #37454, #5453, #11769, #17393, #43421 ),
 .UNSPECIFIED., .F., .F.,
 ( 4, 2, 4 ),
 ( 0.01291313371729459203, 0.01525081363757309870, 0.01758849355785160537 ),
 .UNSPECIFIED. ) ;
#34417 = CARTESIAN_POINT ( 'NONE',  ( 206.3053863259450509, 110.3084416756849464, -63.29990767306989596 ) ) ;
#34418 = VECTOR ( 'NONE', #49613, 1000.000000000000227 ) ;
#34419 = DIRECTION ( 'NONE',  ( -0.000000000000000000, 1.000000000000000000, -0.000000000000000000 ) ) ;
#34420 = DIRECTION ( 'NONE',  ( 0.000000000000000000, 0.000000000000000000, -1.000000000000000000 ) ) ;
#34421 = CARTESIAN_POINT ( 'NONE',  ( 128.0540543950622805, 39.18660671946771146, 68.63333648139733612 ) ) ;
#34422 = DIRECTION ( 'NONE',  ( -0.8595065975201763298, 0.000000000000000000, 0.5111246509603011301 ) ) ;
#34423 = ORIENTED_EDGE ( 'NONE', *, *, #58455, .F. ) ;
#34424 = VERTEX_POINT ( 'NONE', #9058 ) ;
#34425 = AXIS2_PLACEMENT_3D ( 'NONE', #27849, #49286, #7091 ) ;
#34426 = VERTEX_POINT ( 'NONE', #2398 ) ;
#34428 = EDGE_CURVE ( 'NONE', #135, #2857, #23856, .T. ) ;
#34427 = CARTESIAN_POINT ( 'NONE',  ( -15.55634918610403439, 2.818925648462311528E-14, 85.00100000000000477 ) ) ;
#34429 = EDGE_CURVE ( 'NONE', #2074, #28747, #1074, .T. ) ;
#34430 = AXIS2_PLACEMENT_3D ( 'NONE', #51331, #62213, #54226 ) ;
#34431 = CARTESIAN_POINT ( 'NONE',  ( -29.49715792695969085, 42.41725740634736042, 26.66469066592268788 ) ) ;
#34432 = CARTESIAN_POINT ( 'NONE',  ( 5.799999999999999822, -4.618802153517012954, -8.000000000000001776 ) ) ;
#34433 = AXIS2_PLACEMENT_3D ( 'NONE', #43508, #64985, #64283 ) ;
#34434 = EDGE_CURVE ( 'NONE', #36808, #26715, #62849, .T. ) ;
#34435 = CARTESIAN_POINT ( 'NONE',  ( -142.4991775570125583, 58.45550857435407011, 40.94546928456825441 ) ) ;
#34436 = CARTESIAN_POINT ( 'NONE',  ( 18.07314801315404296, -17.44990292519077002, 0.000000000000000000 ) ) ;
#34437 = CARTESIAN_POINT ( 'NONE',  ( -78.66644367742111399, 23.39876645725285798, -8.270900041254197532 ) ) ;
#34438 = VECTOR ( 'NONE', #3185, 1000.000000000000000 ) ;
#34439 = ORIENTED_EDGE ( 'NONE', *, *, #49851, .T. ) ;
#34440 = CARTESIAN_POINT ( 'NONE',  ( 83.60262962804348774, 18.41036205028015615, 57.19024780777382944 ) ) ;
#34442 = ORIENTED_EDGE ( 'NONE', *, *, #37088, .F. ) ;
#34441 = B_SPLINE_CURVE_WITH_KNOTS ( 'NONE', 3,
 ( #10969, #32435, #41951, #63414, #47905, #21188, #63062, #27143, #42635, #37022, #20152, #36683, #41603, #58460, #36332, #20837, #33825, #48928, #6393, #60895, #43660, #414, #1823, #7448, #28904, #65488, #39115, #44011, #23282, #21867, #27845, #44728, #39444, #38049, #65139, #49993, #17647, #27490, #59494, #43312, #770, #28545, #64788, #33132, #49281, #54566 ),
 .UNSPECIFIED., .F., .F.,
 ( 4, 2, 2, 2, 2, 2, 2, 2, 2, 2, 2, 2, 2, 2, 2, 2, 2, 2, 2, 2, 2, 2, 4 ),
 ( 7.152448122690996019E-18, 0.003192770216278319195, 0.003990962770347897259, 0.004789155324417473589, 0.006385540432556618441, 0.007183732986626203444, 0.007981925540695787580, 0.009578310648834957586, 0.01037650320290455300, 0.01117469575697414667, 0.01197288831104374382, 0.01277108086511333750, 0.01436746597325252658, 0.01596385108139171741, 0.01676204363546130241, 0.01756023618953088741, 0.01835842874360046895, 0.01915662129767005395, 0.02075300640580922049, 0.02234939151394838702, 0.02394577662208755703, 0.02474396917615713856, 0.02554216173022672010 ),
 .UNSPECIFIED. ) ;
#34444 = VECTOR ( 'NONE', #22130, 1000.000000000000000 ) ;
#34443 = CARTESIAN_POINT ( 'NONE',  ( 31.96227686234411181, 7.558148489540045922, 36.43275077287186292 ) ) ;
#34445 = FILL_AREA_STYLE ('',( #51644 ) ) ;
#34446 = CARTESIAN_POINT ( 'NONE',  ( 20.89850557012432830, 13.94239061780435662, 3.061616997868437868E-16 ) ) ;
#34447 = CARTESIAN_POINT ( 'NONE',  ( 19.62566184736079578, 15.48655536434876900, 0.000000000000000000 ) ) ;
#34448 = CARTESIAN_POINT ( 'NONE',  ( -21.27554331373000096, 61.43430442924864820, 0.000000000000000000 ) ) ;
#34449 = DIRECTION ( 'NONE',  ( 1.000000000000000000, 0.000000000000000000, 0.000000000000000000 ) ) ;
#34450 = CARTESIAN_POINT ( 'NONE',  ( -48.99162761293256096, 13.13973062091724664, 6.548506681903217164 ) ) ;
#34451 = CARTESIAN_POINT ( 'NONE',  ( 50.98853755884148597, 395.0000000000004547, 101.0502958579881465 ) ) ;
#34452 = ORIENTED_EDGE ( 'NONE', *, *, #58933, .F. ) ;
#34453 = CARTESIAN_POINT ( 'NONE',  ( -102.2801239173131052, 32.78103895658057354, -88.70367844590326456 ) ) ;
#34454 = DIRECTION ( 'NONE',  ( -1.000000000000000000, -0.000000000000000000, -0.000000000000000000 ) ) ;
#34455 = ORIENTED_EDGE ( 'NONE', *, *, #42106, .F. ) ;
#34456 = LINE ( 'NONE', #29160, #522 ) ;
#34457 = FACE_OUTER_BOUND ( 'NONE', #58753, .T. ) ;
#34458 = DIRECTION ( 'NONE',  ( 0.000000000000000000, -1.000000000000000000, 0.000000000000000000 ) ) ;
#34459 = VERTEX_POINT ( 'NONE', #4468 ) ;
#34460 = CARTESIAN_POINT ( 'NONE',  ( 65.33961433650038941, -13.12780791729416840, 34.48241795236666007 ) ) ;
#34461 = CARTESIAN_POINT ( 'NONE',  ( 150.7770046255792238, 53.87214803240240713, -67.07469974738161511 ) ) ;
#34462 = CARTESIAN_POINT ( 'NONE',  ( -38.87848244732137459, 10.93141945332450327, 36.73303816849150394 ) ) ;
#34463 = CARTESIAN_POINT ( 'NONE',  ( 140.1999945597798671, 45.38880890490928977, -47.53303235619388545 ) ) ;
#34464 = ORIENTED_EDGE ( 'NONE', *, *, #18905, .F. ) ;
#34465 =( NAMED_UNIT ( * ) PLANE_ANGLE_UNIT ( ) SI_UNIT ( $, .RADIAN. ) );
#34466 = CARTESIAN_POINT ( 'NONE',  ( -121.5677746760273834, 43.71038933438993013, 44.26482168794601790 ) ) ;
#34467 = VERTEX_POINT ( 'NONE', #26611 ) ;
#34468 = CARTESIAN_POINT ( 'NONE',  ( 31.90247004928964358, 8.563336936370816943, -16.77865705936252994 ) ) ;
#34469 = CARTESIAN_POINT ( 'NONE',  ( -55.05276343752909440, 15.72344139423348430, 30.31732777293113301 ) ) ;
#34470 = CARTESIAN_POINT ( 'NONE',  ( -7.330587818645180498, 7.867004275019547244, 18.27103044898354156 ) ) ;
#34471 = CARTESIAN_POINT ( 'NONE',  ( 135.4635403382140737, 43.58489979881251486, 83.36700200578437148 ) ) ;
#34472 = PRODUCT ( 'Part1', 'Part1', '', ( #43074 ) ) ;
#34473 = CARTESIAN_POINT ( 'NONE',  ( 200.2036606579482338, 102.0234725140079632, -91.49788894171744857 ) ) ;
#34474 = AXIS2_PLACEMENT_3D ( 'NONE', #64683, #27035, #52732 ) ;
#34475 = EDGE_CURVE ( 'NONE', #36282, #52894, #40394, .T. ) ;
#34476 = DIRECTION ( 'NONE',  ( 0.000000000000000000, 0.000000000000000000, 1.000000000000000000 ) ) ;
#34477 = VERTEX_POINT ( 'NONE', #31543 ) ;
#34478 = CARTESIAN_POINT ( 'NONE',  ( 163.1495034066983862, 62.20479872133083887, -11.85475170272490608 ) ) ;
#34479 = FACE_BOUND ( 'NONE', #61649, .T. ) ;
#34480 = CIRCLE ( 'NONE', #15371, 185.0000000000000000 ) ;
#34481 = CARTESIAN_POINT ( 'NONE',  ( 70.45466089417031696, 14.52203022703029944, 65.14393066459052761 ) ) ;
#34482 = CARTESIAN_POINT ( 'NONE',  ( -129.8719378883314164, 50.39084145585431429, -89.73039419715394160 ) ) ;
#34483 = LINE ( 'NONE', #54861, #20603 ) ;
#34484 = AXIS2_PLACEMENT_3D ( 'NONE', #67601, #51761, #67952 ) ;
#34485 = ORIENTED_EDGE ( 'NONE', *, *, #59443, .F. ) ;
#34486 = LINE ( 'NONE', #64689, #11658 ) ;
#34487 = EDGE_CURVE ( 'NONE', #5133, #55571, #52980, .T. ) ;
#34488 = CARTESIAN_POINT ( 'NONE',  ( 164.9700808964341547, 65.04346068891115351, -16.49089399958545954 ) ) ;
#34489 = CARTESIAN_POINT ( 'NONE',  ( 57.16566366493297835, 11.64445456857528782, 27.58472369370708321 ) ) ;
#34490 = ORIENTED_EDGE ( 'NONE', *, *, #63779, .T. ) ;
#34491 = CONICAL_SURFACE ( 'NONE', #9771, 65.00000000000000000, 0.7853981633974497223 ) ;
#34492 = CARTESIAN_POINT ( 'NONE',  ( 67.55199883153196083, 14.80832170058782360, 58.16522213638270955 ) ) ;
#34493 = CARTESIAN_POINT ( 'NONE',  ( 0.000000000000000000, 0.000000000000000000, 0.000000000000000000 ) ) ;
#34494 = EDGE_CURVE ( 'NONE', #54444, #8166, #60695, .T. ) ;
#34495 = EDGE_CURVE ( 'NONE', #33912, #9782, #43119, .T. ) ;
#34496 = EDGE_LOOP ( 'NONE', ( #13657, #16247 ) ) ;
#34497 = CARTESIAN_POINT ( 'NONE',  ( -144.9287131874381771, 60.39056348581542721, -63.19771770627043139 ) ) ;
#34498 = CARTESIAN_POINT ( 'NONE',  ( 0.000000000000000000, 0.000000000000000000, 10.00000000000000000 ) ) ;
#34499 = EDGE_CURVE ( 'NONE', #23153, #12593, #52306, .T. ) ;
#34500 = DIRECTION ( 'NONE',  ( 1.000000000000000000, 0.000000000000000000, 0.000000000000000000 ) ) ;
#34501 = VERTEX_POINT ( 'NONE', #36479 ) ;
#34502 = DIRECTION ( 'NONE',  ( 0.4738686624729966379, 0.8805955318567391110, -1.096041457762183139E-16 ) ) ;
#34503 = CARTESIAN_POINT ( 'NONE',  ( 67.88615656271203136, 14.89310733039355306, 85.25998462581451065 ) ) ;
#34504 = CARTESIAN_POINT ( 'NONE',  ( -74.75133697335806460, 5.472689625386069068, 41.38025477438755928 ) ) ;
#34505 = CARTESIAN_POINT ( 'NONE',  ( 80.15818551272215586, 18.36718314243335470, -12.65347328967094498 ) ) ;
#34506 = CARTESIAN_POINT ( 'NONE',  ( -129.3963145237380843, 48.84337839101544176, -8.933155718294752745 ) ) ;
#34507 = CARTESIAN_POINT ( 'NONE',  ( 151.6351261592328967, 53.25263237790400694, 68.47247492333102059 ) ) ;
#34508 = CARTESIAN_POINT ( 'NONE',  ( 126.5710838895481345, 37.19597237024179037, -72.16778413864886943 ) ) ;
#34509 = EDGE_LOOP ( 'NONE', ( #69003, #17140, #45484, #15824 ) ) ;
#34510 = CARTESIAN_POINT ( 'NONE',  ( -96.77705718164443738, 31.18700926299571208, 69.98325796537412202 ) ) ;
#34511 = CARTESIAN_POINT ( 'NONE',  ( -14.84452950307166219, 8.460866451887699924, 61.80641794076242945 ) ) ;
#34512 = ORIENTED_EDGE ( 'NONE', *, *, #52639, .T. ) ;
#34513 = CARTESIAN_POINT ( 'NONE',  ( -156.8728827992624417, 72.05711009495558983, -43.75528730729580218 ) ) ;
#34514 = CARTESIAN_POINT ( 'NONE',  ( 417.3372781065086770, 0.000000000000000000, 113.5502958579881749 ) ) ;
#34515 = FACE_OUTER_BOUND ( 'NONE', #7376, .T. ) ;
#34516 = FACE_OUTER_BOUND ( 'NONE', #41727, .T. ) ;
#34517 = CARTESIAN_POINT ( 'NONE',  ( -10.71904918402348805, 7.096480526292664237, -89.67472281983359039 ) ) ;
#34518 = ADVANCED_FACE ( 'NONE', ( #9750 ), #48050, .T. ) ;
#34519 = DIRECTION ( 'NONE',  ( -1.232595164407830946E-32, -1.000000000000000000, 1.479221584281239571E-31 ) ) ;
#34520 = LINE ( 'NONE', #23263, #64235 ) ;
#34521 = CARTESIAN_POINT ( 'NONE',  ( -10.69547592951791160, 8.103864096836391084, 30.67361113490947488 ) ) ;
#34522 = CARTESIAN_POINT ( 'NONE',  ( -62.30100056228381078, 16.74548393487071607, 12.96427395586250952 ) ) ;
#34523 = VERTEX_POINT ( 'NONE', #63557 ) ;
#34524 = AXIS2_PLACEMENT_3D ( 'NONE', #53085, #48151, #15481 ) ;
#34525 = B_SPLINE_CURVE_WITH_KNOTS ( 'NONE', 3,
 ( #55958, #28879, #29220, #51373, #50331, #3190 ),
 .UNSPECIFIED., .F., .F.,
 ( 4, 2, 4 ),
 ( 1.095770181082984128E-06, 0.03239442681617709513, 0.06478775786217309818 ),
 .UNSPECIFIED. ) ;
#34526 = CARTESIAN_POINT ( 'NONE',  ( -94.83091526606385457, 30.26550147229321652, -43.53056186647030756 ) ) ;
#34527 = ORIENTED_EDGE ( 'NONE', *, *, #21419, .F. ) ;
#34528 = CARTESIAN_POINT ( 'NONE',  ( -20.63749999999999574, 0.000000000000000000, -23.97499999999999787 ) ) ;
#34529 = CARTESIAN_POINT ( 'NONE',  ( 0.000000000000000000, 0.000000000000000000, 18.50000000000000000 ) ) ;
#34530 = VECTOR ( 'NONE', #61850, 1000.000000000000000 ) ;
#34531 = CARTESIAN_POINT ( 'NONE',  ( 46.70715146412977248, 9.472433765546997009, 62.54244382710503913 ) ) ;
#34532 = CARTESIAN_POINT ( 'NONE',  ( -65.36598343705435354, 0.000000000000000000, 41.38025477438755928 ) ) ;
#34533 = CARTESIAN_POINT ( 'NONE',  ( -14.91909499790562954, 7.457200389278945352, 93.82548247898083105 ) ) ;
#34534 = CONICAL_SURFACE ( 'NONE', #43474, 73.43826238111391547, 0.6747409422235518539 ) ;
#34535 = DIRECTION ( 'NONE',  ( 1.000000000000000000, -0.000000000000000000, 0.000000000000000000 ) ) ;
#34537 = VECTOR ( 'NONE', #2082, 999.9999999999998863 ) ;
#34536 = CARTESIAN_POINT ( 'NONE',  ( 133.8566784816069344, -170.0000000000000000, 37.01034083899534721 ) ) ;
#34538 = FACE_OUTER_BOUND ( 'NONE', #52695, .T. ) ;
#34539 = EDGE_LOOP ( 'NONE', ( #62675, #57214, #4573, #24456 ) ) ;
#34540 = ORIENTED_EDGE ( 'NONE', *, *, #5931, .T. ) ;
#34541 = LINE ( 'NONE', #19375, #50025 ) ;
#34542 = CARTESIAN_POINT ( 'NONE',  ( 15.55634918610403261, 4.999999999999969802, 0.000000000000000000 ) ) ;
#34543 = DIRECTION ( 'NONE',  ( -0.000000000000000000, -0.000000000000000000, -1.000000000000000000 ) ) ;
#34544 = CARTESIAN_POINT ( 'NONE',  ( 106.6322547488295243, 28.34756922280614688, 57.36455916318408299 ) ) ;
#34545 = AXIS2_PLACEMENT_3D ( 'NONE', #54980, #18748, #12781 ) ;
#34546 = CARTESIAN_POINT ( 'NONE',  ( 110.2429982417149574, -170.0000000000000000, -89.61153874658103291 ) ) ;
#34547 = CARTESIAN_POINT ( 'NONE',  ( 59.72647370436681769, 12.96353798836696747, -9.631437282628132479 ) ) ;
#34548 = VERTEX_POINT ( 'NONE', #63898 ) ;
#34549 = CARTESIAN_POINT ( 'NONE',  ( 86.62931800182293784, 20.48449268398422518, 2.867536982015617575 ) ) ;
#34550 = EDGE_CURVE ( 'NONE', #14016, #40816, #25595, .T. ) ;
#34551 = CARTESIAN_POINT ( 'NONE',  ( -7.825402957745083654, 6.891034867348165172, 56.96013162991089018 ) ) ;
#34552 = LINE ( 'NONE', #55282, #52919 ) ;
#34553 = B_SPLINE_CURVE_WITH_KNOTS ( 'NONE', 3,
 ( #11755, #44103, #17380, #56072, #13511, #18436, #24066, #56410, #45862, #45158, #1557, #19121, #7889, #17750, #1927, #66638, #7187, #55366, #28645, #61687, #50449, #23386, #50786, #34277, #23019, #29335, #39891, #40241, #66994, #51144, #6833, #50098, #2607, #8232, #61348, #62030, #60649, #2269, #40576, #45510, #67333, #2960, #44471, #23716, #13167, #66305, #65952, #18092, #34635, #44824 ),
 .UNSPECIFIED., .F., .F.,
 ( 4, 2, 2, 2, 2, 2, 2, 2, 2, 2, 2, 2, 2, 2, 2, 2, 2, 2, 2, 2, 2, 2, 2, 2, 4 ),
 ( 0.03296461860586797493, 0.03492857779726588757, 0.03689253698866380021, 0.03885649618006171979, 0.04082045537145963243, 0.04278441456285754507, 0.04376639415855652221, 0.04474837375425549935, 0.04573035334995447648, 0.04671233294565345362, 0.04720332274350291790, 0.04769431254135237525, 0.04867629213705129687, 0.04965827173275022544, 0.05064025132844915400, 0.05162223092414808256, 0.05260421051984700419, 0.05358619011554593276, 0.05456816971124485438, 0.05555014930694378295, 0.05653212890264271151, 0.05849608809404054782, 0.06046004728543838413, 0.06242400647683622739, 0.06438796566823407064 ),
 .UNSPECIFIED. ) ;
#34554 = DIRECTION ( 'NONE',  ( 1.000000000000000000, 0.000000000000000000, 0.000000000000000000 ) ) ;
#34555 = CARTESIAN_POINT ( 'NONE',  ( 205.5105258529713126, 107.4632495673648123, -9.514488831477544650 ) ) ;
#34556 = FACE_BOUND ( 'NONE', #11519, .T. ) ;
#34557 = EDGE_CURVE ( 'NONE', #56752, #2801, #32170, .T. ) ;
#34558 = EDGE_CURVE ( 'NONE', #29614, #23236, #47358, .T. ) ;
#34559 = ADVANCED_FACE ( 'NONE', ( #16050 ), #68815, .T. ) ;
#34560 = VERTEX_POINT ( 'NONE', #32240 ) ;
#34561 = DIRECTION ( 'NONE',  ( -2.612346171088249236E-15, -1.000000000000000000, 7.216449660063517513E-16 ) ) ;
#34562 = DIRECTION ( 'NONE',  ( -1.000000000000000000, 0.000000000000000000, 0.000000000000000000 ) ) ;
#34563 = CARTESIAN_POINT ( 'NONE',  ( 33.31166872005965729, 8.707041209322234465, -74.34829994818775845 ) ) ;
#34564 = CARTESIAN_POINT ( 'NONE',  ( -5.066666666666671759, 8.000000000000000000, -11.86666666666666536 ) ) ;
#34565 = CARTESIAN_POINT ( 'NONE',  ( 210.6584452238134588, 116.7138338345753965, 58.97358617813433312 ) ) ;
#34566 = CARTESIAN_POINT ( 'NONE',  ( 81.57482918025354479, 17.75786713398421313, -64.61972240065618678 ) ) ;
#34567 = AXIS2_PLACEMENT_3D ( 'NONE', #8506, #39466, #66567 ) ;
#34568 = ORIENTED_EDGE ( 'NONE', *, *, #4817, .F. ) ;
#34569 = CARTESIAN_POINT ( 'NONE',  ( -20.63749999999999574, 2.877919977996280320E-15, 23.50000000000000000 ) ) ;
#34570 = CARTESIAN_POINT ( 'NONE',  ( 201.5987353083855567, 103.8544727311227263, -50.66920982680341012 ) ) ;
#34571 = VERTEX_POINT ( 'NONE', #5496 ) ;
#34573 = DIRECTION ( 'NONE',  ( 0.000000000000000000, -1.000000000000000000, 0.000000000000000000 ) ) ;
#34572 = CIRCLE ( 'NONE', #43519, 30.00000000000000000 ) ;
#34574 = ORIENTED_EDGE ( 'NONE', *, *, #25659, .T. ) ;
#34575 = CARTESIAN_POINT ( 'NONE',  ( -81.01337222286376516, 23.22902179892324881, -76.59940889876602910 ) ) ;
#34576 = DIRECTION ( 'NONE',  ( -0.000000000000000000, 1.000000000000000000, -0.000000000000000000 ) ) ;
#34577 = CARTESIAN_POINT ( 'NONE',  ( 92.21252738308862718, 22.47457138983957137, -75.19816570723047278 ) ) ;
#34578 = EDGE_CURVE ( 'NONE', #62629, #21254, #35932, .T. ) ;
#34579 = EDGE_LOOP ( 'NONE', ( #22086, #8798, #43925, #47959 ) ) ;
#34580 = AXIS2_PLACEMENT_3D ( 'NONE', #30639, #35572, #13763 ) ;
#34581 = EDGE_CURVE ( 'NONE', #56862, #22146, #262, .T. ) ;
#34582 = VERTEX_POINT ( 'NONE', #24032 ) ;
#34583 = CARTESIAN_POINT ( 'NONE',  ( 43.14565945994675644, 9.942782559600560788, 57.75492960358775463 ) ) ;
#34584 = CARTESIAN_POINT ( 'NONE',  ( -130.2647544212423725, 131.3624518482485541, 10.00000000000000000 ) ) ;
#34585 = CIRCLE ( 'NONE', #33467, 35.00000000000000000 ) ;
#34586 = CARTESIAN_POINT ( 'NONE',  ( 21.42484406671928454, 6.746536496442160136, 5.716369911633448986 ) ) ;
#34587 = ORIENTED_EDGE ( 'NONE', *, *, #62001, .T. ) ;
#34588 = AXIS2_PLACEMENT_3D ( 'NONE', #21830, #10582, #15868 ) ;
#34589 = DIRECTION ( 'NONE',  ( 1.000000000000000000, 0.000000000000000000, 0.000000000000000000 ) ) ;
#34590 = AXIS2_PLACEMENT_3D ( 'NONE', #61991, #52811, #14163 ) ;
#34591 = CARTESIAN_POINT ( 'NONE',  ( -47.65155309726505806, 13.85482731128120193, 9.734102492370531934 ) ) ;
#34592 = CARTESIAN_POINT ( 'NONE',  ( -132.0738857626834317, 51.93126104279146915, -19.82589294571803507 ) ) ;
#34593 = CARTESIAN_POINT ( 'NONE',  ( 111.1767565371974484, 29.31586421952250632, -24.03438127329443219 ) ) ;
#34594 = CARTESIAN_POINT ( 'NONE',  ( 88.90509360958570539, 20.20992759522961180, 83.74746512799291054 ) ) ;
#34596 = EDGE_LOOP ( 'NONE', ( #46212, #40074 ) ) ;
#34595 = CARTESIAN_POINT ( 'NONE',  ( -166.4833234777584323, 81.47689702327105010, -92.37364644444049588 ) ) ;
#34597 = ORIENTED_EDGE ( 'NONE', *, *, #31510, .T. ) ;
#34598 = VERTEX_POINT ( 'NONE', #54004 ) ;
#34599 = CARTESIAN_POINT ( 'NONE',  ( 46.90222083990963853, 9.503928413859236812, 10.80947253210855052 ) ) ;
#34600 = DIRECTION ( 'NONE',  ( 0.000000000000000000, 0.000000000000000000, 1.000000000000000000 ) ) ;
#34601 = DIRECTION ( 'NONE',  ( -1.000000000000000000, 0.000000000000000000, 0.000000000000000000 ) ) ;
#34602 = CARTESIAN_POINT ( 'NONE',  ( 103.0026233023293116, 25.67408295205788349, -18.60120070009467241 ) ) ;
#34603 = CARTESIAN_POINT ( 'NONE',  ( 199.3743599161302882, 99.31857334527873604, 15.17104788207974231 ) ) ;
#34604 = CARTESIAN_POINT ( 'NONE',  ( 199.9883293275698293, 101.7441989053914426, 84.55131181239630678 ) ) ;
#34605 = CARTESIAN_POINT ( 'NONE',  ( 0.000000000000000000, 0.000000000000000000, 41.38025477438755928 ) ) ;
#34606 = DIRECTION ( 'NONE',  ( 0.000000000000000000, 0.000000000000000000, 1.000000000000000000 ) ) ;
#34607 = CARTESIAN_POINT ( 'NONE',  ( -14.55425570676091773, 7.423011834016146615, 40.93716450737882440 ) ) ;
#34608 = ORIENTED_EDGE ( 'NONE', *, *, #32544, .T. ) ;
#34609 = CARTESIAN_POINT ( 'NONE',  ( 8.478575283864733692, 7.382882227715640511, -14.47795047564284410 ) ) ;
#34610 = EDGE_LOOP ( 'NONE', ( #4921, #48815, #34865, #46157 ) ) ;
#34612 = VERTEX_POINT ( 'NONE', #32922 ) ;
#34611 = B_SPLINE_CURVE_WITH_KNOTS ( 'NONE', 3,
 ( #35846, #9111, #52363, #9804, #4179, #63267, #31264, #25980, #18970, #51336, #38247, #48780, #68867, #59008, #58317, #21046, #16101, #63950, #64293, #43517, #16455, #5883, #10136, #59690, #58657, #10476, #22076, #42149, #42494, #10826, #26325, #37909, #42822, #64996, #6238, #47412, #11502, #31593, #27342, #59355, #37556, #16789, #20690, #21721, #32977, #53375, #53033, #47762, #4859, #11166 ),
 .UNSPECIFIED., .F., .F.,
 ( 4, 2, 2, 2, 2, 2, 2, 2, 2, 2, 2, 2, 2, 2, 2, 2, 2, 2, 2, 2, 2, 2, 2, 2, 4 ),
 ( 0.03296461860586794718, 0.03492857779726583900, 0.03689253698866373082, 0.03885649618006162265, 0.04082045537145951447, 0.04278441456285740629, 0.04376639415855634874, 0.04474837375425529118, 0.04573035334995423362, 0.04671233294565317606, 0.04720332274350264035, 0.04769431254135211157, 0.04867629213705104707, 0.04965827173274998951, 0.05064025132844893196, 0.05162223092414787440, 0.05260421051984681684, 0.05358619011554575928, 0.05456816971124470173, 0.05555014930694364417, 0.05653212890264258661, 0.05849608809404044374, 0.06046004728543829393, 0.06242400647683614412, 0.06438796566823400125 ),
 .UNSPECIFIED. ) ;
#34613 = CARTESIAN_POINT ( 'NONE',  ( -148.0058283997321098, 64.22864592525512251, 4.024936692211257494 ) ) ;
#34614 = DIRECTION ( 'NONE',  ( -1.000000000000000000, 0.000000000000000000, 0.000000000000000000 ) ) ;
#34615 = CARTESIAN_POINT ( 'NONE',  ( -165.7690020878297901, 80.74028011998679233, 36.81020553927029226 ) ) ;
#34616 = CARTESIAN_POINT ( 'NONE',  ( 0.000000000000000000, 0.000000000000000000, -5.000000000000000000 ) ) ;
#34617 = CARTESIAN_POINT ( 'NONE',  ( -31.43908319763710679, 10.61114334766713796, -89.00629854612920155 ) ) ;
#34618 = CARTESIAN_POINT ( 'NONE',  ( 14.81290967676422277, 7.477658233646010899, -50.47154902647776709 ) ) ;
#34619 = DIRECTION ( 'NONE',  ( -0.000000000000000000, 1.000000000000000000, -0.000000000000000000 ) ) ;
#34620 = VERTEX_POINT ( 'NONE', #22023 ) ;
#34621 = ORIENTED_EDGE ( 'NONE', *, *, #34802, .T. ) ;
#34622 = AXIS2_PLACEMENT_3D ( 'NONE', #49024, #6124, #55722 ) ;
#34623 = CARTESIAN_POINT ( 'NONE',  ( 188.5871124577482192, 88.04033245483464043, 90.77543754304032575 ) ) ;
#34624 = CARTESIAN_POINT ( 'NONE',  ( -7.825402957745083654, 6.891034867348166060, 3.271030448983516692 ) ) ;
#34625 = PLANE ( 'NONE',  #25591 ) ;
#34626 = CARTESIAN_POINT ( 'NONE',  ( 58.09607305250595743, 11.58497620657515270, -22.05889382308176039 ) ) ;
#34627 = VECTOR ( 'NONE', #10130, 1000.000000000000227 ) ;
#34628 = UNCERTAINTY_MEASURE_WITH_UNIT (LENGTH_MEASURE( 1.000000000000000082E-05 ), #27587, 'distance_accuracy_value', 'NONE');
#34629 = CARTESIAN_POINT ( 'NONE',  ( -5.999999999999998224, 19.07878402833891229, -5.000000000000000000 ) ) ;
#34630 = CARTESIAN_POINT ( 'NONE',  ( -8.000000000000000000, 0.000000000000000000, -9.500000000000000000 ) ) ;
#34631 = VERTEX_POINT ( 'NONE', #45128 ) ;
#34632 = COLOUR_RGB ( '',0.7921568627450980005, 0.8196078431372548767, 0.9333333333333333481 ) ;
#34633 = CARTESIAN_POINT ( 'NONE',  ( 46.51377856795992471, 10.46037936279324576, -67.53287648513382635 ) ) ;
#34634 = CARTESIAN_POINT ( 'NONE',  ( -60.64199216239840240, 17.30050036439948258, -74.56797183276353280 ) ) ;
#34635 = CARTESIAN_POINT ( 'NONE',  ( 204.3091227790963558, 107.5190503136783065, -63.17048162308529413 ) ) ;
#34636 = CARTESIAN_POINT ( 'NONE',  ( -177.1539090641757923, 91.73101548694627638, -35.87291332312106817 ) ) ;
#34637 = LINE ( 'NONE', #62033, #7138 ) ;
#34638 = CARTESIAN_POINT ( 'NONE',  ( -165.7689197919845014, 79.30072199592277116, 12.98792212612636732 ) ) ;
#34639 = CARTESIAN_POINT ( 'NONE',  ( -61.68940124183720286, -170.0000000000000000, 94.99999999999866418 ) ) ;
#34640 = FACE_BOUND ( 'NONE', #26110, .T. ) ;
#34641 = CARTESIAN_POINT ( 'NONE',  ( 133.8566784816069344, 42.60093787723652525, 56.35489142945903751 ) ) ;
#34642 = ADVANCED_FACE ( 'NONE', ( #5833 ), #43464, .F. ) ;
#34643 = AXIS2_PLACEMENT_3D ( 'NONE', #5759, #64165, #65212 ) ;
#34644 = ADVANCED_FACE ( 'NONE', ( #24384 ), #66608, .F. ) ;
#34645 = CARTESIAN_POINT ( 'NONE',  ( -5.871577929436014642, 6.771181646175757685, 71.71801545187251747 ) ) ;
#34646 = VERTEX_POINT ( 'NONE', #48728 ) ;
#34647 = CARTESIAN_POINT ( 'NONE',  ( 276.9485791615414314, 21.63883785544751603, -3.974247539526118533 ) ) ;
#34648 = EDGE_CURVE ( 'NONE', #64675, #34426, #61656, .T. ) ;
#34649 = CARTESIAN_POINT ( 'NONE',  ( 157.4703587214989113, 58.92748579479258808, 56.25401806271706562 ) ) ;
#34650 = DIRECTION ( 'NONE',  ( -0.8160245890732938934, -0.5780171883497599028, 0.000000000000000000 ) ) ;
#34651 = LINE ( 'NONE', #56086, #24482 ) ;
#34652 = DIRECTION ( 'NONE',  ( 0.3090169943749582759, -0.9510565162951499785, 0.000000000000000000 ) ) ;
#34653 = ORIENTED_EDGE ( 'NONE', *, *, #68543, .F. ) ;
#34654 = FACE_OUTER_BOUND ( 'NONE', #67611, .T. ) ;
#34655 = ORIENTED_EDGE ( 'NONE', *, *, #44042, .F. ) ;
#34656 = VERTEX_POINT ( 'NONE', #66272 ) ;
#34657 = DIRECTION ( 'NONE',  ( 1.000000000000000000, 0.000000000000000000, 0.000000000000000000 ) ) ;
#34658 = CARTESIAN_POINT ( 'NONE',  ( 151.7783534118502189, 54.60545177578661935, 41.79957158508126014 ) ) ;
#34659 = CARTESIAN_POINT ( 'NONE',  ( -15.55634918610396866, 31.11269837220809009, 2.000000000000001776 ) ) ;
#34660 = EDGE_CURVE ( 'NONE', #68705, #67501, #24588, .T. ) ;
#34661 = ORIENTED_EDGE ( 'NONE', *, *, #45920, .T. ) ;
#34662 = FACE_OUTER_BOUND ( 'NONE', #9877, .T. ) ;
#34663 = CARTESIAN_POINT ( 'NONE',  ( -180.4654253355436992, 95.69358270527506249, 9.926583934681923793 ) ) ;
#34664 = CARTESIAN_POINT ( 'NONE',  ( -1.314022807222076983, 6.554273999800675377, 14.52494611356557641 ) ) ;
#34665 = DIRECTION ( 'NONE',  ( 0.000000000000000000, -0.7071067811865475727, 0.7071067811865475727 ) ) ;
#34666 = CARTESIAN_POINT ( 'NONE',  ( 150.1480464045414180, 52.17471502308665521, 92.38535431822143096 ) ) ;
#34667 = DIRECTION ( 'NONE',  ( -0.9749279121818259508, 0.2225209339563041788, 0.000000000000000000 ) ) ;
#34668 = VERTEX_POINT ( 'NONE', #36658 ) ;
#34669 = VECTOR ( 'NONE', #6594, 1000.000000000000114 ) ;
#34670 = CARTESIAN_POINT ( 'NONE',  ( 112.5721302457195208, 29.97407549554797868, -36.27765895070014324 ) ) ;
#34671 = CARTESIAN_POINT ( 'NONE',  ( -71.23176719684943237, 20.69188312694498677, 12.09344324661407377 ) ) ;
#34672 = CARTESIAN_POINT ( 'NONE',  ( 43.35980717318838629, 8.957244490220878319, -36.74440757935403923 ) ) ;
#34673 = VECTOR ( 'NONE', #62219, 1000.000000000000000 ) ;
#34674 = DIRECTION ( 'NONE',  ( -0.000000000000000000, -0.000000000000000000, -1.000000000000000000 ) ) ;
#34676 = ORIENTED_EDGE ( 'NONE', *, *, #613, .T. ) ;
#34675 = FACE_OUTER_BOUND ( 'NONE', #31428, .T. ) ;
#34677 = PLANE ( 'NONE',  #21827 ) ;
#34678 = MECHANICAL_DESIGN_GEOMETRIC_PRESENTATION_REPRESENTATION (  '', ( #5476 ), #4339 ) ;
#34679 = ORIENTED_EDGE ( 'NONE', *, *, #14219, .F. ) ;
#34680 = DIRECTION ( 'NONE',  ( 0.000000000000000000, 0.000000000000000000, 1.000000000000000000 ) ) ;
#34681 = CARTESIAN_POINT ( 'NONE',  ( 84.97658021689284169, 19.92447159015899416, 29.89253886502025637 ) ) ;
#34682 = DIRECTION ( 'NONE',  ( -1.850371928290090422E-16, 1.000000000000000000, 1.110223024625156294E-16 ) ) ;
#34683 = LINE ( 'NONE', #62441, #45167 ) ;
#34684 = CARTESIAN_POINT ( 'NONE',  ( 140.4897729434290454, 45.57634363643752806, -13.13958130089202392 ) ) ;
#34685 = DIRECTION ( 'NONE',  ( -0.9510565162951500895, -0.3090169943749583314, 5.102127870520021999E-18 ) ) ;
#34686 = CARTESIAN_POINT ( 'NONE',  ( -180.6158171975815492, 97.47361786002628037, -15.69178128716336040 ) ) ;
#34687 = CARTESIAN_POINT ( 'NONE',  ( -154.6171773099879658, 68.63761944777705537, -36.81755893726905526 ) ) ;
#34688 = ORIENTED_EDGE ( 'NONE', *, *, #59678, .F. ) ;
#34689 = ORIENTED_EDGE ( 'NONE', *, *, #65166, .F. ) ;
#34690 = LINE ( 'NONE', #23776, #5743 ) ;
#34691 = CARTESIAN_POINT ( 'NONE',  ( 164.9697211531229755, 63.72502658717164792, 63.45721136982654542 ) ) ;
#34692 = CARTESIAN_POINT ( 'NONE',  ( -21.77424096535250442, 54.12382820593439448, 27.58472315868181468 ) ) ;
#34693 = DIRECTION ( 'NONE',  ( -1.000000000000000000, 0.000000000000000000, 0.000000000000000000 ) ) ;
#34694 = EDGE_CURVE ( 'NONE', #19637, #54242, #47527, .T. ) ;
#34695 = CARTESIAN_POINT ( 'NONE',  ( 187.8959968237854525, 85.77553094678185630, -46.87483139314726088 ) ) ;
#34696 = CARTESIAN_POINT ( 'NONE',  ( -104.5827168854524558, 33.96561401163047833, 57.71033412352771563 ) ) ;
#34697 = DIRECTION ( 'NONE',  ( 0.000000000000000000, -1.000000000000000000, 0.000000000000000000 ) ) ;
#34698 = DIRECTION ( 'NONE',  ( 0.000000000000000000, -0.000000000000000000, 1.000000000000000000 ) ) ;
#34699 = ORIENTED_EDGE ( 'NONE', *, *, #48332, .F. ) ;
#34700 = ORIENTED_EDGE ( 'NONE', *, *, #15175, .F. ) ;
#34701 = VERTEX_POINT ( 'NONE', #56732 ) ;
#34702 = CARTESIAN_POINT ( 'NONE',  ( 309.8720357909272707, 172.0000000000000284, 536.6193948016162949 ) ) ;
#34703 = FACE_OUTER_BOUND ( 'NONE', #67148, .T. ) ;
#34704 = CARTESIAN_POINT ( 'NONE',  ( -5.000000000000000000, 5.000000000000000000, 85.00100000000000477 ) ) ;
#34705 = CARTESIAN_POINT ( 'NONE',  ( 132.2818448028687897, 41.65267246304672000, 29.67398922120065663 ) ) ;
#34706 = CARTESIAN_POINT ( 'NONE',  ( 412.0000000000000000, 192.0000000000000000, 378.0000000000000000 ) ) ;
#34707 = CARTESIAN_POINT ( 'NONE',  ( -55.05276343752909440, 15.72344139423348430, 30.31732777293113301 ) ) ;
#34708 = CARTESIAN_POINT ( 'NONE',  ( -99.99439884168255332, 32.75762661251356889, -8.511024296776820819 ) ) ;
#34709 = CARTESIAN_POINT ( 'NONE',  ( 59.29474530993685732, 12.86968658439547930, 43.82944600131264679 ) ) ;
#34710 = CARTESIAN_POINT ( 'NONE',  ( 37.45083697588171390, 8.163195152810535760, 83.83898265753474277 ) ) ;
#34711 = VERTEX_POINT ( 'NONE', #57418 ) ;
#34712 = CARTESIAN_POINT ( 'NONE',  ( -4.180838820196604466, 65.23214221112780820, 43.58025477438756212 ) ) ;
#34713 = CARTESIAN_POINT ( 'NONE',  ( 442.3372781065085633, 400.0000000000000568, -136.4497041420118251 ) ) ;
#34714 = CARTESIAN_POINT ( 'NONE',  ( -14.33060720034883673, 8.412649192293191192, 7.006307883328436681 ) ) ;
#34715 = CARTESIAN_POINT ( 'NONE',  ( -144.9287131874381771, 60.39056348581540590, 17.33593406512061819 ) ) ;
#34716 = PLANE ( 'NONE',  #14128 ) ;
#34717 = CARTESIAN_POINT ( 'NONE',  ( 197.3685896092616474, 96.80423329231983587, 61.92891938233814386 ) ) ;
#34718 = EDGE_CURVE ( 'NONE', #62968, #4994, #3956, .T. ) ;
#34719 = CARTESIAN_POINT ( 'NONE',  ( 127.4992165631961569, 38.87141012667720474, -20.68911966244177947 ) ) ;
#34720 = AXIS2_PLACEMENT_3D ( 'NONE', #62411, #35689, #24096 ) ;
#34721 = ORIENTED_EDGE ( 'NONE', *, *, #37731, .T. ) ;
#34722 = EDGE_CURVE ( 'NONE', #8386, #12944, #3269, .T. ) ;
#34723 = CARTESIAN_POINT ( 'NONE',  ( 126.3580464630938707, 38.22944795020833908, -43.82392713467700673 ) ) ;
#34724 = CARTESIAN_POINT ( 'NONE',  ( -38.80621516088653067, 11.94263260276895622, -41.34864224206805261 ) ) ;
#34725 = DIRECTION ( 'NONE',  ( 0.7530714660036099684, 0.6579387259397138088, -0.000000000000000000 ) ) ;
#34726 = AXIS2_PLACEMENT_3D ( 'NONE', #56250, #54849, #8065 ) ;
#34727 = CARTESIAN_POINT ( 'NONE',  ( -188.6739852773920347, 108.2139733222100517, -43.81670758250005093 ) ) ;
#34728 = ORIENTED_EDGE ( 'NONE', *, *, #17928, .T. ) ;
#34729 = CARTESIAN_POINT ( 'NONE',  ( -4.613603609464498767, -74.86839895266049894, 170.0000000000000000 ) ) ;
#34730 = B_SPLINE_CURVE_WITH_KNOTS ( 'NONE', 3,
 ( #10420, #37499, #25594, #4467, #58953, #51960, #47357, #20632, #46679, #26610, #19964, #3770, #25243, #15015, #63897, #62868, #63556, #31542, #14668, #52979, #4802, #15365, #41415, #68813, #36133, #30861, #47029, #20291, #48049, #5152, #36828, #52305, #26266, #58604, #36478, #69504, #52643, #4125, #15708, #20990, #68486, #21324, #41755, #57930, #9749, #31212, #25926, #58266 ),
 .UNSPECIFIED., .F., .F.,
 ( 4, 2, 2, 2, 2, 2, 2, 2, 2, 2, 2, 2, 2, 2, 2, 2, 2, 2, 2, 2, 2, 2, 2, 4 ),
 ( 0.02554216173022674438, 0.02715505844859233270, 0.02796150680777515288, 0.02876795516695797306, 0.03038085188532354056, 0.03199374860368910806, 0.03360664532205467903, 0.03441309368123745410, 0.03521954204042023612, 0.03602599039960301119, 0.03683243875878579321, 0.03844533547715135030, 0.03925178383633415313, 0.04005823219551694903, 0.04086468055469975186, 0.04167112891388255469, 0.04247757727306535058, 0.04328402563224814648, 0.04489692235061378683, 0.04650981906897942025, 0.04731626742816222309, 0.04812271578734503286, 0.04973561250571071485, 0.05134850922407639684 ),
 .UNSPECIFIED. ) ;
#34731 = CARTESIAN_POINT ( 'NONE',  ( -36.11269837220812207, -31.11269837220801193, 2.000000000000001776 ) ) ;
#34732 = CARTESIAN_POINT ( 'NONE',  ( 204.6977192012829505, 108.0580384837234931, 2.363170148305746565 ) ) ;
#34733 = CARTESIAN_POINT ( 'NONE',  ( 159.9309212402495461, 60.87908227903663771, 83.50715383507403544 ) ) ;
#34734 = EDGE_CURVE ( 'NONE', #8399, #33379, #22074, .T. ) ;
#34735 = VERTEX_POINT ( 'NONE', #43641 ) ;
#34736 = CARTESIAN_POINT ( 'NONE',  ( -56.96436614829622869, 16.24647150911285820, 3.716444753663429523 ) ) ;
#34737 = CARTESIAN_POINT ( 'NONE',  ( 5.799999999999999822, 8.000000000000000000, 0.000000000000000000 ) ) ;
#34738 = CARTESIAN_POINT ( 'NONE',  ( -72.99999999999998579, 0.000000000000000000, 85.00000000000000000 ) ) ;
#34739 = EDGE_CURVE ( 'NONE', #46954, #30352, #32755, .T. ) ;
#34740 = ADVANCED_FACE ( 'NONE', ( #53502 ), #21846, .T. ) ;
#34741 = LINE ( 'NONE', #7992, #53907 ) ;
#34742 = CARTESIAN_POINT ( 'NONE',  ( 79.14129363775930415, 17.00055658855363205, 9.874494824056680997 ) ) ;
#34744 = ORIENTED_EDGE ( 'NONE', *, *, #55497, .T. ) ;
#34743 = DIRECTION ( 'NONE',  ( -0.000000000000000000, -0.000000000000000000, 1.000000000000000000 ) ) ;
#34745 = CARTESIAN_POINT ( 'NONE',  ( 58.09607305250595033, 11.58497620657515803, 31.63020735784560600 ) ) ;
#34746 = EDGE_LOOP ( 'NONE', ( #34945, #42625 ) ) ;
#34747 = VERTEX_POINT ( 'NONE', #58437 ) ;
#34748 = CARTESIAN_POINT ( 'NONE',  ( -171.4943428135323131, 86.82484920477511992, 18.84716997149836359 ) ) ;
#34749 = DIRECTION ( 'NONE',  ( 0.000000000000000000, 0.000000000000000000, 1.000000000000000000 ) ) ;
#34751 = ORIENTED_EDGE ( 'NONE', *, *, #43644, .T. ) ;
#34750 = CARTESIAN_POINT ( 'NONE',  ( -14.56631729561072319, 8.434645566888200108, -66.43805081226972220 ) ) ;
#34752 = CARTESIAN_POINT ( 'NONE',  ( -95.25262505162312721, 30.46326104480063890, 94.40935392145755145 ) ) ;
#34754 = AXIS2_PLACEMENT_3D ( 'NONE', #43120, #63899, #16051 ) ;
#34753 = CARTESIAN_POINT ( 'NONE',  ( -24.61094659556677655, 9.585225265507407499, 40.82880548562345524 ) ) ;
#34755 = FACE_BOUND ( 'NONE', #62358, .T. ) ;
#34756 = VERTEX_POINT ( 'NONE', #20816 ) ;
#34757 = CARTESIAN_POINT ( 'NONE',  ( 211.7357196141372242, 118.3691710715567211, -68.06136091401778287 ) ) ;
#34758 = CYLINDRICAL_SURFACE ( 'NONE', #15125, 7.500000000000013323 ) ;
#34759 = CARTESIAN_POINT ( 'NONE',  ( 0.000000000000000000, 70.00000000000000000, 0.000000000000000000 ) ) ;
#34760 = LINE ( 'NONE', #55867, #6666 ) ;
#34761 = DIRECTION ( 'NONE',  ( -0.000000000000000000, 1.000000000000000000, -0.000000000000000000 ) ) ;
#34762 = ORIENTED_EDGE ( 'NONE', *, *, #7165, .F. ) ;
#34763 = VECTOR ( 'NONE', #29202, 1000.000000000000114 ) ;
#34764 = VERTEX_POINT ( 'NONE', #21497 ) ;
#34765 = ORIENTED_EDGE ( 'NONE', *, *, #44143, .F. ) ;
#34766 = LINE ( 'NONE', #6978, #62076 ) ;
#34767 = VECTOR ( 'NONE', #62404, 1000.000000000000000 ) ;
#34768 = CARTESIAN_POINT ( 'NONE',  ( 111.9975424824652634, 295.8720703627916464, 535.5371946177799600 ) ) ;
#34769 = CARTESIAN_POINT ( 'NONE',  ( -52.34571669801462690, 13.97238103161367562, -89.40772904822969736 ) ) ;
#34770 = EDGE_CURVE ( 'NONE', #28864, #35305, #55043, .T. ) ;
#34771 = DIRECTION ( 'NONE',  ( -0.000000000000000000, -0.000000000000000000, -1.000000000000000000 ) ) ;
#34772 = CARTESIAN_POINT ( 'NONE',  ( -15.55634918610408945, -31.11269837220804035, 0.000000000000000000 ) ) ;
#34773 = DIRECTION ( 'NONE',  ( 0.000000000000000000, 0.000000000000000000, -1.000000000000000000 ) ) ;
#34774 = CARTESIAN_POINT ( 'NONE',  ( -71.97171223898807568, 20.94894057408424359, -12.35306980544747546 ) ) ;
#34775 = VERTEX_POINT ( 'NONE', #16915 ) ;
#34776 = CARTESIAN_POINT ( 'NONE',  ( -108.6622665321723105, 37.28993738537006664, 34.07158365272115219 ) ) ;
#34777 = EDGE_LOOP ( 'NONE', ( #69038, #52836, #23194, #33938 ) ) ;
#34778 = EDGE_CURVE ( 'NONE', #40870, #23153, #27121, .T. ) ;
#34779 = CARTESIAN_POINT ( 'NONE',  ( 36.31593203568480277, 8.028139509847019184, 30.57375986728627026 ) ) ;
#34780 = CARTESIAN_POINT ( 'NONE',  ( -10.00000000000000178, 35.26862320190615208, 5.000000000000000000 ) ) ;
#34781 = ORIENTED_EDGE ( 'NONE', *, *, #12227, .F. ) ;
#34782 = CARTESIAN_POINT ( 'NONE',  ( 183.1910712700538397, 80.76073941711160842, 44.01936912216330455 ) ) ;
#34783 = CARTESIAN_POINT ( 'NONE',  ( 6.400000000000000355, -9.237604307034033013, -1.753283555911559014E-16 ) ) ;
#34784 = PRESENTATION_STYLE_ASSIGNMENT (( #66805 ) ) ;
#34785 = CARTESIAN_POINT ( 'NONE',  ( -123.6618353044034535, 46.23845779494349273, 57.78952661695447546 ) ) ;
#34786 = CARTESIAN_POINT ( 'NONE',  ( -47.80193682758676488, 12.85650137125659143, 8.992210446493192677 ) ) ;
#34787 = CARTESIAN_POINT ( 'NONE',  ( 151.1607415860635797, 52.90668588398090577, -47.71061066794121075 ) ) ;
#34788 = ORIENTED_EDGE ( 'NONE', *, *, #1349, .F. ) ;
#34789 = DIRECTION ( 'NONE',  ( -0.7071067811865476838, -1.110223024625156294E-16, -0.7071067811865474617 ) ) ;
#34790 = LINE ( 'NONE', #34097, #61096 ) ;
#34791 = ORIENTED_EDGE ( 'NONE', *, *, #69395, .T. ) ;
#34792 = FACE_OUTER_BOUND ( 'NONE', #20930, .T. ) ;
#34793 = CARTESIAN_POINT ( 'NONE',  ( 64.99999999999998579, 0.000000000000000000, -1.127570259384924454E-14 ) ) ;
#34794 = PLANE ( 'NONE',  #61128 ) ;
#34795 = VERTEX_POINT ( 'NONE', #42615 ) ;
#34796 = EDGE_CURVE ( 'NONE', #65969, #42777, #48911, .T. ) ;
#34797 = CARTESIAN_POINT ( 'NONE',  ( 14.59045944429442443, -20.30070179093305427, 0.000000000000000000 ) ) ;
#34798 = DIRECTION ( 'NONE',  ( 0.000000000000000000, 1.000000000000000000, -0.000000000000000000 ) ) ;
#34799 = CARTESIAN_POINT ( 'NONE',  ( -97.49219489034499020, 30.41416107059308871, -21.46345111338298750 ) ) ;
#34800 = ADVANCED_FACE ( 'NONE', ( #38376 ), #42275, .T. ) ;
#34801 = CARTESIAN_POINT ( 'NONE',  ( -25.80058235236790765, 8.733375263008326783, 69.53065690646717201 ) ) ;
#34802 = EDGE_CURVE ( 'NONE', #60780, #8669, #15546, .T. ) ;
#34803 = VERTEX_POINT ( 'NONE', #21170 ) ;
#34804 = ADVANCED_FACE ( 'NONE', ( #5661 ), #48216, .T. ) ;
#34805 = CIRCLE ( 'NONE', #57290, 65.00000000000000000 ) ;
#34806 = CARTESIAN_POINT ( 'NONE',  ( -85.23209958216042992, 26.02162889534598733, -92.67245568390785593 ) ) ;
#34807 = CARTESIAN_POINT ( 'NONE',  ( -123.6619986853277879, 45.04188181212061437, 45.28385183707185746 ) ) ;
#34808 = EDGE_LOOP ( 'NONE', ( #13074, #37648, #47388, #61345 ) ) ;
#34809 = CARTESIAN_POINT ( 'NONE',  ( 173.0237957311180708, 69.97204739562489806, -91.14091141288837150 ) ) ;
#34810 = CARTESIAN_POINT ( 'NONE',  ( 184.3941060377211443, 82.01604625189460762, 3.219449370753451944 ) ) ;
#34811 = CARTESIAN_POINT ( 'NONE',  ( 61.28323125814100081, 21.66484633135460669, 170.0000000000000000 ) ) ;
#34812 = CARTESIAN_POINT ( 'NONE',  ( -1.224646799147352468E-15, 16.00000000000000000, 6.196318915105386793 ) ) ;
#34813 = DIRECTION ( 'NONE',  ( -1.000000000000000000, 0.000000000000000000, 0.000000000000000000 ) ) ;
#34814 = DIRECTION ( 'NONE',  ( -1.000000000000000000, 0.000000000000000000, 0.000000000000000000 ) ) ;
#34815 = AXIS2_PLACEMENT_3D ( 'NONE', #45547, #55403, #3000 ) ;
#34816 = ORIENTED_EDGE ( 'NONE', *, *, #61409, .F. ) ;
#34817 = CARTESIAN_POINT ( 'NONE',  ( 164.4615316623334991, 63.29763980349831343, -19.50861212731829752 ) ) ;
#34818 = DIRECTION ( 'NONE',  ( -1.000000000000000000, -0.000000000000000000, -0.000000000000000000 ) ) ;
#34819 = CARTESIAN_POINT ( 'NONE',  ( 70.38121440378671423, 14.50253793787158685, 65.63465686359772633 ) ) ;
#34820 = LINE ( 'NONE', #56257, #33264 ) ;
#34821 = CARTESIAN_POINT ( 'NONE',  ( 0.000000000000000000, 200.0000000000000000, 0.000000000000000000 ) ) ;
#34822 = EDGE_CURVE ( 'NONE', #29971, #33511, #56160, .T. ) ;
#34823 = EDGE_CURVE ( 'NONE', #35154, #64522, #15737, .T. ) ;
#34824 = AXIS2_PLACEMENT_3D ( 'NONE', #51764, #51076, #40172 ) ;
#34825 = ADVANCED_FACE ( 'NONE', ( #59820 ), #32417, .T. ) ;
#34826 = ORIENTED_EDGE ( 'NONE', *, *, #9536, .T. ) ;
#34827 = ADVANCED_FACE ( 'NONE', ( #15882 ), #58780, .T. ) ;
#34828 = CARTESIAN_POINT ( 'NONE',  ( 159.2325040199866919, 60.31699144791974021, -9.434136353667053498 ) ) ;
#34829 = CARTESIAN_POINT ( 'NONE',  ( 65.00000000000000000, 0.000000000000000000, 15.70156211871650775 ) ) ;
#34830 = EDGE_LOOP ( 'NONE', ( #2726, #19893, #11416, #11316 ) ) ;
#34831 = CARTESIAN_POINT ( 'NONE',  ( -452.6627218934859798, 400.0000000000064801, -146.4497041420121377 ) ) ;
#34832 = DIRECTION ( 'NONE',  ( 1.000000000000000000, 0.000000000000000000, 0.000000000000000000 ) ) ;
#34833 = B_SPLINE_CURVE_WITH_KNOTS ( 'NONE', 3,
 ( #62326, #35603, #57061, #56354, #8175, #30323, #30670, #19071, #8529, #51777, #29976, #52117, #25056, #51439, #3250, #67964, #3935, #61293, #19765, #41224, #25406, #39833, #57747, #4960, #36293, #20794, #68308, #32043, #58087, #26424, #9558, #58759, #42260, #9906, #41907, #27099, #63017, #15178, #31023, #53131, #42921, #52789, #14819 ),
 .UNSPECIFIED., .F., .F.,
 ( 4, 2, 2, 2, 2, 2, 2, 2, 1, 2, 2, 2, 2, 2, 2, 2, 2, 2, 2, 2, 2, 4 ),
 ( 0.000000000000000000, 0.001465684626643313062, 0.002198526939964969701, 0.002931369253286626123, 0.004397053879929952412, 0.005862738506573278267, 0.007328423133216604123, 0.008061265446538276591, 0.008794107759859948192, 0.009526950073181621528, 0.01025979238650329313, 0.01172547701314665541, 0.01319116163979001770, 0.01465684626643337998, 0.01538968857975506026, 0.01612253089307674053, 0.01758821551972008027, 0.01905390014636342694, 0.01978674245968510548, 0.02051958477300678402, 0.02198526939965014457, 0.02345095402629350512 ),
 .UNSPECIFIED. ) ;
#34834 = ORIENTED_EDGE ( 'NONE', *, *, #24955, .F. ) ;
#34835 = CARTESIAN_POINT ( 'NONE',  ( -142.3178993725748853, 58.31327888234795864, -66.94886755203597772 ) ) ;
#34837 = DIRECTION ( 'NONE',  ( -0.000000000000000000, -0.000000000000000000, 1.000000000000000000 ) ) ;
#34836 = AXIS2_PLACEMENT_3D ( 'NONE', #58267, #10085, #10770 ) ;
#34838 = FACE_OUTER_BOUND ( 'NONE', #49341, .T. ) ;
#34839 = LINE ( 'NONE', #8089, #51888 ) ;
#34840 = ORIENTED_EDGE ( 'NONE', *, *, #64498, .F. ) ;
#34841 = CARTESIAN_POINT ( 'NONE',  ( -101.8187363387486641, 33.67461140603122516, 3.674523915951410480 ) ) ;
#34842 = CARTESIAN_POINT ( 'NONE',  ( 65.60747156646080214, 14.32439394919076570, 83.95651089761803121 ) ) ;
#34843 = CARTESIAN_POINT ( 'NONE',  ( 152.6567222595844555, 55.25503842111547925, -91.54794413222496985 ) ) ;
#34844 = CARTESIAN_POINT ( 'NONE',  ( 79.33384730094455506, 18.11203072455033336, -18.23467331857458262 ) ) ;
#34845 = FACE_OUTER_BOUND ( 'NONE', #16971, .T. ) ;
#34846 = CARTESIAN_POINT ( 'NONE',  ( 0.000000000000000000, 0.000000000000000000, 85.00100000000000477 ) ) ;
#34847 = CARTESIAN_POINT ( 'NONE',  ( 131.6189313563687620, 40.08924984825279125, -63.19450288702588381 ) ) ;
#34848 = ORIENTED_EDGE ( 'NONE', *, *, #59243, .F. ) ;
#34849 = CARTESIAN_POINT ( 'NONE',  ( 181.0840389613909736, 78.60582251573003987, 56.15314469597509373 ) ) ;
#34850 = CARTESIAN_POINT ( 'NONE',  ( -31.11269837220804035, 20.55634918610408945, 0.000000000000000000 ) ) ;
#34851 = ORIENTED_EDGE ( 'NONE', *, *, #39110, .F. ) ;
#34852 = CIRCLE ( 'NONE', #29218, 25.12245591505646303 ) ;
#34853 = LINE ( 'NONE', #39087, #28389 ) ;
#34854 = DIRECTION ( 'NONE',  ( 0.7071067811865475727, 0.000000000000000000, 0.7071067811865475727 ) ) ;
#34855 = CARTESIAN_POINT ( 'NONE',  ( -34.74563762132952860, 11.17960945723135779, 44.45265738134296640 ) ) ;
#34856 = DIRECTION ( 'NONE',  ( -0.000000000000000000, 1.000000000000000000, -0.000000000000000000 ) ) ;
#34857 = DIRECTION ( 'NONE',  ( -0.000000000000000000, -0.000000000000000000, -1.000000000000000000 ) ) ;
#34858 = CARTESIAN_POINT ( 'NONE',  ( -52.68007207639882239, 14.05813534436550682, -76.67980032479178476 ) ) ;
#34859 = CARTESIAN_POINT ( 'NONE',  ( -0.7076388175553618431, 7.538734751903870546, -18.48788273639771162 ) ) ;
#34860 = CARTESIAN_POINT ( 'NONE',  ( 173.7227242028390606, 71.47307702680406294, 8.499494705527911975 ) ) ;
#34861 = CARTESIAN_POINT ( 'NONE',  ( -62.45356936877016807, 16.79156452995240301, 9.731492733239218040 ) ) ;
#34862 = ORIENTED_EDGE ( 'NONE', *, *, #54121, .T. ) ;
#34863 = ADVANCED_FACE ( 'NONE', ( #6007 ), #37679, .F. ) ;
#34864 = CARTESIAN_POINT ( 'NONE',  ( -99.98584758882476820, 32.75338129098884110, -49.67063086737493904 ) ) ;
#34865 = ORIENTED_EDGE ( 'NONE', *, *, #24252, .F. ) ;
#34866 = CARTESIAN_POINT ( 'NONE',  ( 102.8111940033034273, 25.59308899183601582, -69.22529567365751291 ) ) ;
#34867 = CARTESIAN_POINT ( 'NONE',  ( 46.23113030541875190, 10.41513832761375902, -13.16521276663865692 ) ) ;
#34868 = CARTESIAN_POINT ( 'NONE',  ( 43.14356474118744700, 8.925336319666904217, 57.73968773710988245 ) ) ;
#34869 = CYLINDRICAL_SURFACE ( 'NONE', #23393, 65.36598343705435354 ) ;
#34870 = FACE_OUTER_BOUND ( 'NONE', #21902, .T. ) ;
#34871 = VECTOR ( 'NONE', #61029, 1000.000000000000000 ) ;
#34872 = LINE ( 'NONE', #28542, #56879 ) ;
#34873 = CARTESIAN_POINT ( 'NONE',  ( -173.1211646369891071, 87.12891641440859303, -22.86740657428632773 ) ) ;
#34874 = CARTESIAN_POINT ( 'NONE',  ( -166.3188283541502415, 79.86268666707375985, 61.99536074306163869 ) ) ;
#34875 = ORIENTED_EDGE ( 'NONE', *, *, #9851, .F. ) ;
#34876 = ORIENTED_EDGE ( 'NONE', *, *, #22726, .T. ) ;
#34877 = EDGE_CURVE ( 'NONE', #26757, #2801, #22458, .T. ) ;
#34878 = CARTESIAN_POINT ( 'NONE',  ( 447.3372781065085633, 365.0000000000001137, -146.4497041420116261 ) ) ;
#34879 = DIRECTION ( 'NONE',  ( -0.000000000000000000, 0.000000000000000000, -1.000000000000000000 ) ) ;
#34880 = CARTESIAN_POINT ( 'NONE',  ( 44.67156470120503542, 9.152591717284639827, -91.40705571865771617 ) ) ;
#34881 = CARTESIAN_POINT ( 'NONE',  ( -171.5023337025455135, 86.83681590836893349, 57.83153322340911018 ) ) ;
#34882 = LINE ( 'NONE', #2864, #8316 ) ;
#34883 = EDGE_CURVE ( 'NONE', #8997, #64350, #13395, .T. ) ;
#34884 = EDGE_CURVE ( 'NONE', #46252, #36977, #49973, .T. ) ;
#34885 = AXIS2_PLACEMENT_3D ( 'NONE', #4399, #21260, #58881 ) ;
#34886 = CARTESIAN_POINT ( 'NONE',  ( 61.33840119549017089, 13.32121602003047123, -23.69023232728272887 ) ) ;
#34887 = ORIENTED_EDGE ( 'NONE', *, *, #48732, .F. ) ;
#34888 = DIRECTION ( 'NONE',  ( -0.3090169943749582759, 0.9510565162951499785, 0.000000000000000000 ) ) ;
#34889 = CARTESIAN_POINT ( 'NONE',  ( 22.72762739171800561, 7.830015800126072456, -40.14245491239596930 ) ) ;
#34890 = CARTESIAN_POINT ( 'NONE',  ( -81.67992981004168485, 23.49232121719082400, -22.64303255023387962 ) ) ;
#34891 = DIRECTION ( 'NONE',  ( -0.000000000000000000, -0.000000000000000000, -1.000000000000000000 ) ) ;
#34892 = FACE_BOUND ( 'NONE', #18667, .T. ) ;
#34893 = EDGE_LOOP ( 'NONE', ( #54601, #15487, #2088, #30322 ) ) ;
#34894 = EDGE_LOOP ( 'NONE', ( #50116, #14143, #18917, #61790 ) ) ;
#34895 = LINE ( 'NONE', #34203, #62727 ) ;
#34896 = FACE_OUTER_BOUND ( 'NONE', #66373, .T. ) ;
#34897 = FACE_OUTER_BOUND ( 'NONE', #60291, .T. ) ;
#34898 = CARTESIAN_POINT ( 'NONE',  ( -2.645453300864630819E-14, -10.55634918610403439, 2.000000000000001776 ) ) ;
#34899 = CARTESIAN_POINT ( 'NONE',  ( 23.26352157766197948, 6.855087657142792779, 91.89523032385697832 ) ) ;
#34900 = AXIS2_PLACEMENT_3D ( 'NONE', #48835, #682, #58129 ) ;
#34901 = EDGE_CURVE ( 'NONE', #55648, #42077, #48958, .T. ) ;
#34902 = CARTESIAN_POINT ( 'NONE',  ( 80.72161230109723817, 17.48902961068032980, -74.81300800374665982 ) ) ;
#34903 = ORIENTED_EDGE ( 'NONE', *, *, #17864, .F. ) ;
#34904 = ADVANCED_FACE ( 'NONE', ( #44707 ), #12698, .T. ) ;
#34905 = DIRECTION ( 'NONE',  ( -0.000000000000000000, -0.000000000000000000, -1.000000000000000000 ) ) ;
#34906 = CARTESIAN_POINT ( 'NONE',  ( 197.3700262219430783, 98.41176242030789467, -42.19614285301155832 ) ) ;
#34907 = VERTEX_POINT ( 'NONE', #55602 ) ;
#34908 = CARTESIAN_POINT ( 'NONE',  ( 396.6937511374966334, 500.0000000000000000, -51.64566090791306863 ) ) ;
#34909 = ORIENTED_EDGE ( 'NONE', *, *, #30050, .F. ) ;
#34910 = CARTESIAN_POINT ( 'NONE',  ( -82.32931163805226049, 23.75065981441938234, -76.00918213230767151 ) ) ;
#34911 = CARTESIAN_POINT ( 'NONE',  ( -55.53456145826333312, 15.85318253404851063, -23.37177340799620140 ) ) ;
#34912 = CARTESIAN_POINT ( 'NONE',  ( 90.51709546286272712, 21.85407654229979357, -76.58433341987911547 ) ) ;
#34913 = ORIENTED_EDGE ( 'NONE', *, *, #41139, .F. ) ;
#34914 = ORIENTED_EDGE ( 'NONE', *, *, #2945, .F. ) ;
#34915 = LINE ( 'NONE', #40871, #35259 ) ;
#34916 = CARTESIAN_POINT ( 'NONE',  ( -108.5076394317819677, 37.20503715172082337, -91.99933385091648574 ) ) ;
#34917 = CARTESIAN_POINT ( 'NONE',  ( 22.89634831467701659, 6.832298124325686395, 13.07552592342019260 ) ) ;
#34918 = ORIENTED_EDGE ( 'NONE', *, *, #7336, .F. ) ;
#34919 = CARTESIAN_POINT ( 'NONE',  ( 5.799999999999999822, 4.618802153517004960, 7.999999999999998224 ) ) ;
#34920 = CARTESIAN_POINT ( 'NONE',  ( 180.2494929075577375, 79.18888319146951460, -63.06960825634327961 ) ) ;
#34921 = CARTESIAN_POINT ( 'NONE',  ( -129.3970594949620363, 50.06339481638100608, -22.21707316791037456 ) ) ;
#34922 = DIRECTION ( 'NONE',  ( -0.9216045519012663334, 0.000000000000000000, 0.3881301971180111110 ) ) ;
#34923 = CARTESIAN_POINT ( 'NONE',  ( 79.37778929114111293, 18.12554302172300780, -41.34262384610868679 ) ) ;
#34925 = ORIENTED_EDGE ( 'NONE', *, *, #14558, .T. ) ;
#34924 = FACE_OUTER_BOUND ( 'NONE', #31727, .T. ) ;
#34926 = ORIENTED_EDGE ( 'NONE', *, *, #64905, .T. ) ;
#34927 = VECTOR ( 'NONE', #24419, 1000.000000000000000 ) ;
#34928 = VERTEX_POINT ( 'NONE', #55961 ) ;
#34929 = CARTESIAN_POINT ( 'NONE',  ( 46.90141780929663895, 9.503798448769785523, 10.06464778740114774 ) ) ;
#34930 = CARTESIAN_POINT ( 'NONE',  ( 98.48662049252141060, -156.6058287036421177, 10.00000000000000000 ) ) ;
#34931 = CARTESIAN_POINT ( 'NONE',  ( -51.13073217147959326, 13.66490163179657102, -9.474297845703558707 ) ) ;
#34932 = FACE_OUTER_BOUND ( 'NONE', #40517, .T. ) ;
#34933 = CARTESIAN_POINT ( 'NONE',  ( 140.1272987153004124, 45.34167505388539610, -93.07698992894040657 ) ) ;
#34934 = CARTESIAN_POINT ( 'NONE',  ( -26.06927550048145292, 8.771279580068128467, -91.25299760957113904 ) ) ;
#34935 = CARTESIAN_POINT ( 'NONE',  ( 211.8616541147234784, 118.5646031478490414, 88.16756572905163125 ) ) ;
#34936 = EDGE_CURVE ( 'NONE', #40674, #4244, #62897, .T. ) ;
#34938 = DIRECTION ( 'NONE',  ( -0.000000000000000000, 1.000000000000000000, -0.000000000000000000 ) ) ;
#34937 = VECTOR ( 'NONE', #28686, 1000.000000000000000 ) ;
#34939 = CARTESIAN_POINT ( 'NONE',  ( 6.933333333333335347, 0.000000000000000000, 43.13333333333333286 ) ) ;
#34940 = CARTESIAN_POINT ( 'NONE',  ( -10.23867141318105922, 7.059827648235817321, 30.49746343403691995 ) ) ;
#34941 = VERTEX_POINT ( 'NONE', #6719 ) ;
#34942 = EDGE_CURVE ( 'NONE', #62736, #16812, #67444, .T. ) ;
#34943 = CARTESIAN_POINT ( 'NONE',  ( 8.480977594057447888, 7.382886909400594000, -17.88117617556033423 ) ) ;
#34944 = ORIENTED_EDGE ( 'NONE', *, *, #47265, .F. ) ;
#34945 = ORIENTED_EDGE ( 'NONE', *, *, #19013, .T. ) ;
#34946 = DIRECTION ( 'NONE',  ( -1.000000000000000000, 0.000000000000000000, 0.000000000000000000 ) ) ;
#34947 = CARTESIAN_POINT ( 'NONE',  ( 184.5867277229703518, 83.68414666546580349, -63.93399993165346729 ) ) ;
#34948 = CARTESIAN_POINT ( 'NONE',  ( -38.31648305663216547, 11.84679862791310079, 94.41515645623105968 ) ) ;
#34949 = CARTESIAN_POINT ( 'NONE',  ( 0.06730325657896543690, -1.557442666625494576, 8.000000000000000000 ) ) ;
#34950 = CARTESIAN_POINT ( 'NONE',  ( 141.9165763529819344, 192.0000000000000000, 129.0000000000000000 ) ) ;
#34951 = PLANE ( 'NONE',  #55138 ) ;
#34952 = LINE ( 'NONE', #14864, #67438 ) ;
#34953 = CARTESIAN_POINT ( 'NONE',  ( 131.6189313563687335, 40.08924984825279125, -36.34995229656220772 ) ) ;
#34954 = EDGE_LOOP ( 'NONE', ( #4773, #43606, #61868, #34078 ) ) ;
#34955 = ORIENTED_EDGE ( 'NONE', *, *, #24640, .T. ) ;
#34956 = CARTESIAN_POINT ( 'NONE',  ( 188.3569538602032480, 87.78382372060060845, 92.37220588221737216 ) ) ;
#34957 = LINE ( 'NONE', #2597, #18447 ) ;
#34958 = DIRECTION ( 'NONE',  ( -1.850169831522831466E-16, 1.000000000000000000, 1.110223024625156294E-16 ) ) ;
#34959 = CARTESIAN_POINT ( 'NONE',  ( -27.48703802937314933, 8.975952825337623509, -63.28273934099161124 ) ) ;
#34960 = ADVANCED_FACE ( 'NONE', ( #60535 ), #8112, .T. ) ;
#34961 = EDGE_CURVE ( 'NONE', #31797, #39615, #19103, .T. ) ;
#34962 = B_SPLINE_CURVE_WITH_KNOTS ( 'NONE', 3,
 ( #26900, #16345, #54666, #1560, #38143, #48326, #6494, #21618, #15996, #22668, #21965, #160, #59583, #59249, #32525, #53953, #11399, #44107, #17383, #38862, #32873, #54305, #6127, #27589, #49028, #34279, #50790, #55368, #34969, #18438, #55728, #18095, #3301, #2962, #56769, #35310, #29338, #19124, #29683, #61350, #40578, #2609, #1930, #60652 ),
 .UNSPECIFIED., .F., .F.,
 ( 4, 2, 2, 2, 2, 2, 2, 2, 2, 2, 2, 2, 2, 2, 2, 2, 2, 2, 2, 2, 2, 4 ),
 ( 0.000000000000000000, 0.001533942663855616256, 0.003067885327711232513, 0.004601827991566848769, 0.005368799323494655162, 0.006135770655422460688, 0.007669713319278092557, 0.008436684651205906757, 0.009203655983133721824, 0.01073759864698933982, 0.01150456997891714794, 0.01227154131084495781, 0.01303851264277276420, 0.01380548397470057233, 0.01533942663855619552, 0.01687336930241181698, 0.01840731196626744018, 0.01994125463012305990, 0.02070822596205087324, 0.02147519729397868657, 0.02300913995783434793, 0.02454308262169001276 ),
 .UNSPECIFIED. ) ;
#34963 = CARTESIAN_POINT ( 'NONE',  ( -439.4229916354182706, 394.9999999999998295, 91.05029585798840230 ) ) ;
#34964 = ORIENTED_EDGE ( 'NONE', *, *, #48079, .T. ) ;
#34965 = CARTESIAN_POINT ( 'NONE',  ( 283.3030319151914682, 21.67621409537481014, -3.767785295203601059 ) ) ;
#34966 = CARTESIAN_POINT ( 'NONE',  ( -56.01329802674224112, 15.98369420723829570, -77.01488154601142355 ) ) ;
#34967 = PLANE ( 'NONE',  #4584 ) ;
#34968 = CARTESIAN_POINT ( 'NONE',  ( 277.4947172190871925, -21.56856595115426600, 4.339532581985733550 ) ) ;
#34969 = CARTESIAN_POINT ( 'NONE',  ( 103.1567541746301657, 25.73937982110325606, 7.758240586775330350 ) ) ;
#34970 = CARTESIAN_POINT ( 'NONE',  ( -30.94745021534356511, 10.53010394565407637, 72.06100499665291181 ) ) ;
#34971 = CARTESIAN_POINT ( 'NONE',  ( -24.02131509525290554, -34.12171010297063845, 13.79046340968177908 ) ) ;
#34972 = CARTESIAN_POINT ( 'NONE',  ( -50.52927270563906603, 13.51486287463704450, 58.65938854185318263 ) ) ;
#34973 = B_SPLINE_CURVE_WITH_KNOTS ( 'NONE', 3,
 ( #12026, #66214, #65494, #44371, #11311, #33137 ),
 .UNSPECIFIED., .F., .F.,
 ( 4, 2, 4 ),
 ( 0.03218938496963297952, 0.06469835385212996393, 0.09720732273462692752 ),
 .UNSPECIFIED. ) ;
#34974 = CARTESIAN_POINT ( 'NONE',  ( -1.728570918131774325, 6.570609986804655023, 60.08533143854203473 ) ) ;
#34975 = ORIENTED_EDGE ( 'NONE', *, *, #12627, .F. ) ;
#34976 = CARTESIAN_POINT ( 'NONE',  ( 277.4892320395364322, 21.56923944770097279, -4.336110802034249367 ) ) ;
#34977 = CIRCLE ( 'NONE', #63030, 24.99999999999985434 ) ;
#34978 = CARTESIAN_POINT ( 'NONE',  ( -128.9925397612932443, 48.56800623462826394, -76.09213246840596412 ) ) ;
#34979 = FACE_OUTER_BOUND ( 'NONE', #20614, .T. ) ;
#34980 = CARTESIAN_POINT ( 'NONE',  ( -56.44201257846630426, 32.26641783793562723, 43.58025477438756923 ) ) ;
#34981 = CARTESIAN_POINT ( 'NONE',  ( -0.3508015596286013227, 7.526244656639662800, 90.60611482011238138 ) ) ;
#34982 = AXIS2_PLACEMENT_3D ( 'NONE', #9281, #30744, #2288 ) ;
#34983 = EDGE_LOOP ( 'NONE', ( #51339, #51678, #23267, #27879 ) ) ;
#34984 = CARTESIAN_POINT ( 'NONE',  ( -7.347286611336974360, -4.995646404165295706, -0.4969600502617599891 ) ) ;
#34985 = EDGE_LOOP ( 'NONE', ( #46586, #31261, #7264, #62934 ) ) ;
#34986 = VECTOR ( 'NONE', #48544, 1000.000000000000000 ) ;
#34987 = VECTOR ( 'NONE', #37351, 999.9999999999998863 ) ;
#34988 = ORIENTED_EDGE ( 'NONE', *, *, #40030, .F. ) ;
#34989 = FACE_OUTER_BOUND ( 'NONE', #35392, .T. ) ;
#34990 = CARTESIAN_POINT ( 'NONE',  ( 150.5538013146980347, 53.70974888488126453, 39.82180283041768831 ) ) ;
#34991 = CARTESIAN_POINT ( 'NONE',  ( 0.000000000000000000, 0.000000000000000000, 41.38025477438755928 ) ) ;
#34992 = VERTEX_POINT ( 'NONE', #65829 ) ;
#34993 = DIRECTION ( 'NONE',  ( -1.000000000000000000, 0.000000000000000000, 0.000000000000000000 ) ) ;
#34994 = CARTESIAN_POINT ( 'NONE',  ( -176.3791001330699260, 90.82833141237287577, 18.24710418921203114 ) ) ;
#34995 = CARTESIAN_POINT ( 'NONE',  ( -3.857727530059801513, 6.665032499723451132, 17.14034259272734317 ) ) ;
#34996 = CIRCLE ( 'NONE', #38342, 243.4957430088094839 ) ;
#34997 = PLANE ( 'NONE',  #10685 ) ;
#34998 = CARTESIAN_POINT ( 'NONE',  ( 0.000000000000000000, 0.000000000000000000, 0.000000000000000000 ) ) ;
#34999 = CARTESIAN_POINT ( 'NONE',  ( -23.93933407965395688, 9.495050561681670942, -15.47704760526285916 ) ) ;
#35000 = CARTESIAN_POINT ( 'NONE',  ( 140.0614732283738704, 45.29930344725075031, 5.945277084547093693 ) ) ;
#35001 = ORIENTED_EDGE ( 'NONE', *, *, #22596, .T. ) ;
#35002 = CARTESIAN_POINT ( 'NONE',  ( 116.9200705848630264, 32.09536795999728298, -39.96847962606891258 ) ) ;
#35003 = CARTESIAN_POINT ( 'NONE',  ( -71.57660578921959882, 20.81129687646278725, 13.57068704725283581 ) ) ;
#35004 = LINE ( 'NONE', #67371, #38275 ) ;
#35005 = DIRECTION ( 'NONE',  ( -0.000000000000000000, 1.000000000000000000, -0.000000000000000000 ) ) ;
#35007 = ORIENTED_EDGE ( 'NONE', *, *, #40793, .F. ) ;
#35006 = CARTESIAN_POINT ( 'NONE',  ( 50.98853755884157835, 388.0000000000065370, -128.9497041420121946 ) ) ;
#35008 = CARTESIAN_POINT ( 'NONE',  ( 80.16939877002759829, 17.31693935407228935, -39.47914003811105488 ) ) ;
#35009 = ADVANCED_FACE ( 'NONE', ( #2151 ), #58404, .T. ) ;
#35010 = ORIENTED_EDGE ( 'NONE', *, *, #59382, .F. ) ;
#35011 = FACE_BOUND ( 'NONE', #230, .T. ) ;
#35012 = CARTESIAN_POINT ( 'NONE',  ( 82.73618382051373032, 19.18661415186669572, 43.62715597890617403 ) ) ;
#35013 = DIRECTION ( 'NONE',  ( 1.000000000000000000, -0.000000000000000000, 0.000000000000000000 ) ) ;
#35014 = CARTESIAN_POINT ( 'NONE',  ( 442.3372781065086201, 0.000000000000000000, 103.5502958579881749 ) ) ;
#35015 = EDGE_CURVE ( 'NONE', #58406, #52035, #18318, .T. ) ;
#35016 = CARTESIAN_POINT ( 'NONE',  ( -124.3331814159187587, 45.47486189329072204, 57.62516324564902703 ) ) ;
#35017 = CARTESIAN_POINT ( 'NONE',  ( -86.16710354151695128, 26.41338104675949694, -15.53640633945776273 ) ) ;
#35018 = DIRECTION ( 'NONE',  ( -0.000000000000000000, -0.000000000000000000, -1.000000000000000000 ) ) ;
#35019 = ADVANCED_FACE ( 'NONE', ( #18673 ), #29562, .F. ) ;
#35020 = CARTESIAN_POINT ( 'NONE',  ( -1.148430018225575555, 500.0000000000000000, -0.000000000000000000 ) ) ;
#35021 = VERTEX_POINT ( 'NONE', #17262 ) ;
#35022 = VERTEX_POINT ( 'NONE', #12349 ) ;
#35023 = EDGE_CURVE ( 'NONE', #46840, #6856, #3392, .T. ) ;
#35024 = VECTOR ( 'NONE', #2193, 1000.000000000000000 ) ;
#35025 = CARTESIAN_POINT ( 'NONE',  ( 108.3906473026529653, 28.03385344351494268, 71.23839387606832929 ) ) ;
#35026 = CARTESIAN_POINT ( 'NONE',  ( 164.6406716478538215, 63.44801348349341197, 61.53806796485126540 ) ) ;
#35027 = CARTESIAN_POINT ( 'NONE',  ( -189.4223925288096666, 107.3427006758676043, 66.98796678033512819 ) ) ;
#35028 = VECTOR ( 'NONE', #57227, 1000.000000000000000 ) ;
#35029 = FACE_OUTER_BOUND ( 'NONE', #36607, .T. ) ;
#35030 = DIRECTION ( 'NONE',  ( -0.000000000000000000, 1.000000000000000000, -0.000000000000000000 ) ) ;
#35031 = LINE ( 'NONE', #19538, #18360 ) ;
#35032 = VERTEX_POINT ( 'NONE', #2839 ) ;
#35033 = PRODUCT_DEFINITION_SHAPE ( 'NONE', 'NONE',  #69585 ) ;
#35034 = EDGE_LOOP ( 'NONE', ( #44784, #31255, #57016, #44090 ) ) ;
#35035 = ORIENTED_EDGE ( 'NONE', *, *, #18126, .F. ) ;
#35036 = VECTOR ( 'NONE', #9315, 1000.000000000000000 ) ;
#35037 = MECHANICAL_DESIGN_GEOMETRIC_PRESENTATION_REPRESENTATION (  '', ( #24951 ), #57476 ) ;
#35038 = FACE_OUTER_BOUND ( 'NONE', #39589, .T. ) ;
#35039 = CARTESIAN_POINT ( 'NONE',  ( -73.83891297820638044, 20.54113601143295753, 85.85888820351974005 ) ) ;
#35040 = DIRECTION ( 'NONE',  ( 0.000000000000000000, 0.000000000000000000, 1.000000000000000000 ) ) ;
#35041 = EDGE_CURVE ( 'NONE', #30746, #30581, #25344, .T. ) ;
#35042 = CARTESIAN_POINT ( 'NONE',  ( 67.55134213333077753, 13.77030723107741039, -49.21396399478243922 ) ) ;
#35043 = CARTESIAN_POINT ( 'NONE',  ( 211.9975424824652066, 190.0000000000000284, 276.7368757365948682 ) ) ;
#35044 = CARTESIAN_POINT ( 'NONE',  ( -58.33157376762796531, 16.63098604184963847, 44.56701505676580410 ) ) ;
#35045 = CARTESIAN_POINT ( 'NONE',  ( -96.45303203827903360, 31.03218867996497821, -10.92221250935651966 ) ) ;
#35046 = DIRECTION ( 'NONE',  ( -0.8191520442889886899, 1.003171929053520926E-16, 0.5735764363510506003 ) ) ;
#35047 = CARTESIAN_POINT ( 'NONE',  ( 31.89767103975184881, 7.551769522480730856, 90.89116849545793286 ) ) ;
#35048 = ITEM_DEFINED_TRANSFORMATION ( 'NONE', 'NONE', #54521,  #66832 ) ;
#35049 = ORIENTED_EDGE ( 'NONE', *, *, #28369, .F. ) ;
#35050 = DIRECTION ( 'NONE',  ( -0.000000000000000000, -0.000000000000000000, -1.000000000000000000 ) ) ;
#35051 = CARTESIAN_POINT ( 'NONE',  ( -102.2801239173131052, 32.78103895658057354, -76.85912785543962400 ) ) ;
#35052 = CARTESIAN_POINT ( 'NONE',  ( -189.7987719395349018, 107.8653664616570467, -39.23015726446638496 ) ) ;
#35053 = DIRECTION ( 'NONE',  ( -0.000000000000000000, 1.000000000000000000, -0.000000000000000000 ) ) ;
#35054 = CARTESIAN_POINT ( 'NONE',  ( 22.90619343622340764, 7.840927939412482672, -18.58827641307582468 ) ) ;
#35055 = CARTESIAN_POINT ( 'NONE',  ( 201.6034029841262338, 102.1956603101140644, 70.39772623200110502 ) ) ;
#35056 = EDGE_LOOP ( 'NONE', ( #7696, #57667, #16248, #51724 ) ) ;
#35057 = CARTESIAN_POINT ( 'NONE',  ( 133.4058733589413919, 42.32720528873925048, -51.02331093239570237 ) ) ;
#35058 = CARTESIAN_POINT ( 'NONE',  ( -38.87871322265797858, 11.95691939779334767, -41.83587164630765187 ) ) ;
#35059 = CARTESIAN_POINT ( 'NONE',  ( -1.201657407838099433E-15, -7.124194613927628872, -3.660532965668815919 ) ) ;
#35060 = CARTESIAN_POINT ( 'NONE',  ( -165.6130566995026356, 79.14211131649287267, 92.14615457014019739 ) ) ;
#35061 = VERTEX_POINT ( 'NONE', #51717 ) ;
#35062 = CARTESIAN_POINT ( 'NONE',  ( 126.3681350380370958, 38.23508791628619008, 10.65839973360038684 ) ) ;
#35063 = CARTESIAN_POINT ( 'NONE',  ( -149.2910611247328063, 63.99625741915658494, -7.968279941028271196 ) ) ;
#35064 = DIRECTION ( 'NONE',  ( 0.000000000000000000, 0.000000000000000000, -1.000000000000000000 ) ) ;
#35065 = VERTEX_POINT ( 'NONE', #24650 ) ;
#35066 = CARTESIAN_POINT ( 'NONE',  ( 150.1360066839118304, 53.40685429604861412, 92.17743685337597981 ) ) ;
#35067 = EDGE_LOOP ( 'NONE', ( #335, #25530, #38676, #6039 ) ) ;
#35068 = CARTESIAN_POINT ( 'NONE',  ( -62.29496909743954092, 17.79481128341708285, 12.93814815294244269 ) ) ;
#35069 = CARTESIAN_POINT ( 'NONE',  ( 127.4750938923429402, 37.70245908594343121, 33.06177329601652559 ) ) ;
#35070 = CARTESIAN_POINT ( 'NONE',  ( -155.7455325080991315, 71.01834415181987481, 42.39273526441780859 ) ) ;
#35071 = VECTOR ( 'NONE', #25988, 1000.000000000000000 ) ;
#35072 = CARTESIAN_POINT ( 'NONE',  ( 51.85299110299440173, 39.21848821248450179, 170.0000000000000000 ) ) ;
#35073 = CARTESIAN_POINT ( 'NONE',  ( 100.0000000000000284, 5.000000000000000000, 18.50000000000000000 ) ) ;
#35074 = VECTOR ( 'NONE', #3252, 1000.000000000000000 ) ;
#35076 = VERTEX_POINT ( 'NONE', #19354 ) ;
#35075 = LINE ( 'NONE', #13286, #63442 ) ;
#35077 = ADVANCED_FACE ( 'NONE', ( #8817 ), #56645, .F. ) ;
#35078 = CARTESIAN_POINT ( 'NONE',  ( 63.01563776193090405, 12.67277567978497643, 44.81296093922130552 ) ) ;
#35079 = EDGE_LOOP ( 'NONE', ( #41070, #50547, #46010, #12357 ) ) ;
#35080 = ORIENTED_EDGE ( 'NONE', *, *, #32737, .T. ) ;
#35081 = CARTESIAN_POINT ( 'NONE',  ( -166.7050147108375313, 81.70694330787516435, 15.40055725785405727 ) ) ;
#35082 = CARTESIAN_POINT ( 'NONE',  ( 17.72992212664810197, 6.570588738776104165, -77.11196272085689429 ) ) ;
#35084 = ORIENTED_EDGE ( 'NONE', *, *, #26149, .F. ) ;
#35083 = CARTESIAN_POINT ( 'NONE',  ( -132.9126122820979390, 52.52752252041128145, 62.30792293928088554 ) ) ;
#35085 = CARTESIAN_POINT ( 'NONE',  ( -96.88714137552827310, 31.24002647487883522, 86.48642051269072795 ) ) ;
#35086 = VECTOR ( 'NONE', #43182, 1000.000000000000000 ) ;
#35087 = FACE_BOUND ( 'NONE', #29132, .T. ) ;
#35088 = EDGE_LOOP ( 'NONE', ( #3450, #57049, #43356, #29822 ) ) ;
#35089 = CARTESIAN_POINT ( 'NONE',  ( 180.3998223972066910, 79.34418886440140284, -89.93734709859124621 ) ) ;
#35090 = EDGE_CURVE ( 'NONE', #66690, #47682, #14436, .T. ) ;
#35091 = CARTESIAN_POINT ( 'NONE',  ( 134.7720294983483598, 43.15885542353189663, 44.46810067847044223 ) ) ;
#35092 = CARTESIAN_POINT ( 'NONE',  ( 117.7442255600442422, 33.63739995216995737, 36.61229788494631521 ) ) ;
#35093 = CARTESIAN_POINT ( 'NONE',  ( -130.5904357464317229, 50.88938808445627160, 17.14299821243472977 ) ) ;
#35094 = CARTESIAN_POINT ( 'NONE',  ( 65.62985354949974237, 14.32996029952553840, -63.03137781880401036 ) ) ;
#35095 = ORIENTED_EDGE ( 'NONE', *, *, #63278, .T. ) ;
#35096 = VERTEX_POINT ( 'NONE', #30960 ) ;
#35097 = EDGE_CURVE ( 'NONE', #61600, #69216, #52406, .T. ) ;
#35098 = CARTESIAN_POINT ( 'NONE',  ( -145.3246383987844297, 62.00818849034183700, -21.69799560209030531 ) ) ;
#35099 = CARTESIAN_POINT ( 'NONE',  ( 209.9518228411288874, 0.000000000000000000, 31.43423095485942298 ) ) ;
#35100 = CYLINDRICAL_SURFACE ( 'NONE', #69232, 5.000000000000004441 ) ;
#35101 = CARTESIAN_POINT ( 'NONE',  ( -22.06416059020191867, 12.01293505575286602, 0.000000000000000000 ) ) ;
#35102 = CARTESIAN_POINT ( 'NONE',  ( -142.3393481102175713, 58.33014244976926932, 35.99748335774498287 ) ) ;
#35103 = CARTESIAN_POINT ( 'NONE',  ( -129.4098618459771615, 48.85263848239743822, 58.33566833192991652 ) ) ;
#35104 = CARTESIAN_POINT ( 'NONE',  ( -169.1005390226459042, 82.76152663947081578, -62.70965392198332466 ) ) ;
#35105 = VERTEX_POINT ( 'NONE', #8465 ) ;
#35106 = CARTESIAN_POINT ( 'NONE',  ( -447.6627218934912662, 369.9999999999998863, 108.5502958579877060 ) ) ;
#35107 = VERTEX_POINT ( 'NONE', #68583 ) ;
#35108 = DIRECTION ( 'NONE',  ( -1.000000000000000000, 0.000000000000000000, 0.000000000000000000 ) ) ;
#35109 = DIRECTION ( 'NONE',  ( -0.000000000000000000, -0.000000000000000000, -1.000000000000000000 ) ) ;
#35110 = EDGE_LOOP ( 'NONE', ( #42576, #32075, #39320, #52970, #67290, #49406, #26233 ) ) ;
#35111 = CARTESIAN_POINT ( 'NONE',  ( 0.000000000000000000, 0.000000000000000000, 41.41421356237313489 ) ) ;
#35112 = ADVANCED_FACE ( 'NONE', ( #13732 ), #20384, .T. ) ;
#35113 = CARTESIAN_POINT ( 'NONE',  ( 134.3182571105338923, 42.88121222759020412, 71.35489142945908725 ) ) ;
#35114 = DIRECTION ( 'NONE',  ( 0.000000000000000000, 0.000000000000000000, 1.000000000000000000 ) ) ;
#35115 = DIRECTION ( 'NONE',  ( -0.000000000000000000, -1.000000000000000000, -0.000000000000000000 ) ) ;
#35116 = DIRECTION ( 'NONE',  ( 0.000000000000000000, 1.000000000000000000, -0.000000000000000000 ) ) ;
#35117 = CARTESIAN_POINT ( 'NONE',  ( -15.13211202216340823, 8.488266782358833140, -44.62742559165378253 ) ) ;
#35118 = AXIS2_PLACEMENT_3D ( 'NONE', #66498, #17596, #39747 ) ;
#35119 = EDGE_CURVE ( 'NONE', #55226, #13226, #62625, .T. ) ;
#35120 = CARTESIAN_POINT ( 'NONE',  ( 152.8430172091322561, 54.14068524174418684, -49.53136367997995393 ) ) ;
#35121 = ORIENTED_EDGE ( 'NONE', *, *, #18356, .T. ) ;
#35122 = VECTOR ( 'NONE', #61491, 1000.000000000000114 ) ;
#35123 = CARTESIAN_POINT ( 'NONE',  ( -109.6829043543429236, 36.70322915510440254, -95.00000000000133582 ) ) ;
#35124 = ORIENTED_EDGE ( 'NONE', *, *, #69550, .T. ) ;
#35125 = DIRECTION ( 'NONE',  ( -0.000000000000000000, 1.000000000000000000, -0.000000000000000000 ) ) ;
#35126 = CARTESIAN_POINT ( 'NONE',  ( -62.50103539982530521, 17.85731685071834818, 63.65098158254257754 ) ) ;
#35127 = CARTESIAN_POINT ( 'NONE',  ( 185.0000000000000000, 0.000000000000000000, 0.000000000000000000 ) ) ;
#35128 = ORIENTED_EDGE ( 'NONE', *, *, #3444, .F. ) ;
#35129 = CARTESIAN_POINT ( 'NONE',  ( 44.01696072966022655, -47.84694004974146253, 170.0000000000000000 ) ) ;
#35130 = CARTESIAN_POINT ( 'NONE',  ( -10.23402954931276554, 7.059791383763807993, -62.65565335715368889 ) ) ;
#35131 = CARTESIAN_POINT ( 'NONE',  ( -37.38262509017738466, 10.64263598035110547, 42.31726256907158756 ) ) ;
#35132 = AXIS2_PLACEMENT_3D ( 'NONE', #6834, #53952, #11757 ) ;
#35133 = CARTESIAN_POINT ( 'NONE',  ( 0.000000000000000000, 0.000000000000000000, 0.000000000000000000 ) ) ;
#35134 = AXIS2_PLACEMENT_3D ( 'NONE', #47226, #64101, #20496 ) ;
#35135 = ORIENTED_EDGE ( 'NONE', *, *, #34770, .T. ) ;
#35136 = B_SPLINE_CURVE_WITH_KNOTS ( 'NONE', 3,
 ( #40494, #49646, #44742, #60564, #66559, #51059, #13426, #45075, #45781, #18348, #39810, #55991, #50706, #61264, #13087, #67256, #34889, #23976, #19042, #33501, #54929, #1474, #12381, #33840, #55281, #13764, #4258, #67587, #30300, #19734, #19386, #61945, #62991, #30641, #40844, #63340, #51414, #14464, #35222, #9882, #47149, #46116, #31335 ),
 .UNSPECIFIED., .F., .F.,
 ( 4, 2, 2, 2, 2, 2, 2, 2, 1, 2, 2, 2, 2, 2, 2, 2, 2, 2, 2, 2, 2, 4 ),
 ( 0.000000000000000000, 0.001466285743483476288, 0.002199428615225214323, 0.002932571486966952575, 0.004398857230450438187, 0.005865142973933924232, 0.007331428717417410278, 0.008064571589159153300, 0.008797714460900897190, 0.009530857332642639346, 0.01026400020438438324, 0.01173028594786784673, 0.01319657169135131022, 0.01466285743483477372, 0.01539600030657651587, 0.01612914317831826150, 0.01759542892180174581, 0.01906171466528523359, 0.01979485753702698095, 0.02052800040876873178, 0.02199428615225221609, 0.02346057189573570387 ),
 .UNSPECIFIED. ) ;
#35138 = AXIS2_PLACEMENT_3D ( 'NONE', #1267, #18147, #16740 ) ;
#35137 = DIRECTION ( 'NONE',  ( 0.000000000000000000, 0.000000000000000000, 1.000000000000000000 ) ) ;
#35139 = CARTESIAN_POINT ( 'NONE',  ( -156.9900125991010214, 72.16580261738671709, 64.47870932869700766 ) ) ;
#35140 = CARTESIAN_POINT ( 'NONE',  ( -118.6157340058429668, 41.88485941274766589, 39.95035298570361704 ) ) ;
#35141 = CARTESIAN_POINT ( 'NONE',  ( -59.57733000654214095, 15.94108165424593793, -48.71746015130258911 ) ) ;
#35142 = ORIENTED_EDGE ( 'NONE', *, *, #23228, .F. ) ;
#35143 = CARTESIAN_POINT ( 'NONE',  ( -180.5801285865472039, 97.42945596116102536, -69.85561729999363934 ) ) ;
#35144 = DIRECTION ( 'NONE',  ( -0.000000000000000000, -1.000000000000000000, -0.000000000000000000 ) ) ;
#35145 = CARTESIAN_POINT ( 'NONE',  ( 112.5721302457195634, 29.97407549554797868, 44.25599282069087081 ) ) ;
#35146 = DIRECTION ( 'NONE',  ( 1.000000000000000000, 0.000000000000000000, 0.000000000000000000 ) ) ;
#35147 = CARTESIAN_POINT ( 'NONE',  ( 2.700000000000004619, 0.000000000000000000, -25.00000000000000355 ) ) ;
#35148 = VERTEX_POINT ( 'NONE', #41166 ) ;
#35149 = CARTESIAN_POINT ( 'NONE',  ( 6.000000000000000000, 23.07878402833891229, -5.000000000000000000 ) ) ;
#35150 = CARTESIAN_POINT ( 'NONE',  ( 116.1021807117071774, 31.68810634233424395, -65.55867728159829255 ) ) ;
#35151 = CARTESIAN_POINT ( 'NONE',  ( 68.45098769362923008, 13.99935947269945480, 58.98388901208659263 ) ) ;
#35152 = CARTESIAN_POINT ( 'NONE',  ( 136.7690435008551333, 44.39743995805025634, 3.250471752906729517 ) ) ;
#35153 = DIRECTION ( 'NONE',  ( -0.000000000000000000, -0.000000000000000000, 1.000000000000000000 ) ) ;
#35154 = VERTEX_POINT ( 'NONE', #57342 ) ;
#35155 = EDGE_CURVE ( 'NONE', #34477, #19832, #43860, .T. ) ;
#35156 = LINE ( 'NONE', #25996, #26053 ) ;
#35157 = ORIENTED_EDGE ( 'NONE', *, *, #28276, .F. ) ;
#35158 = EDGE_CURVE ( 'NONE', #42059, #6090, #48819, .T. ) ;
#35159 = LINE ( 'NONE', #30582, #818 ) ;
#35160 = CARTESIAN_POINT ( 'NONE',  ( 127.0701306906838397, 37.47492071169578054, 87.48711923404823665 ) ) ;
#35161 = ORIENTED_EDGE ( 'NONE', *, *, #52093, .T. ) ;
#35162 = CARTESIAN_POINT ( 'NONE',  ( -145.9095871962850879, 61.18682730038540285, -62.57265054608006238 ) ) ;
#35163 = FACE_OUTER_BOUND ( 'NONE', #49742, .T. ) ;
#35164 = LINE ( 'NONE', #18645, #45013 ) ;
#35165 = CARTESIAN_POINT ( 'NONE',  ( 164.9534461562627712, 63.71129898458567453, -44.20161124359641036 ) ) ;
#35166 = AXIS2_PLACEMENT_3D ( 'NONE', #42104, #5505, #64600 ) ;
#35167 = ORIENTED_EDGE ( 'NONE', *, *, #64875, .T. ) ;
#35168 = DIRECTION ( 'NONE',  ( 0.000000000000000000, 0.000000000000000000, 1.000000000000000000 ) ) ;
#35169 = EDGE_CURVE ( 'NONE', #36960, #30847, #59045, .T. ) ;
#35170 = VECTOR ( 'NONE', #58310, 1000.000000000000000 ) ;
#35171 = EDGE_CURVE ( 'NONE', #25214, #20810, #42194, .T. ) ;
#35172 = CARTESIAN_POINT ( 'NONE',  ( 69.38831087449705137, 15.28150064080604942, 87.03339823595428015 ) ) ;
#35173 = CARTESIAN_POINT ( 'NONE',  ( -868.3301948030079984, -622.0000000000060254, 0.000000000000000000 ) ) ;
#35174 = CARTESIAN_POINT ( 'NONE',  ( -31.11269837220801193, 31.11269837220812207, 0.000000000000000000 ) ) ;
#35175 = CARTESIAN_POINT ( 'NONE',  ( 46.68054346512387554, 10.48734223171576829, -95.00000000000133582 ) ) ;
#35176 = VECTOR ( 'NONE', #28292, 999.9999999999998863 ) ;
#35177 = CARTESIAN_POINT ( 'NONE',  ( -142.6040384731713004, 58.53810651789324737, -93.02743765931519704 ) ) ;
#35178 = FACE_OUTER_BOUND ( 'NONE', #46830, .T. ) ;
#35180 = VERTEX_POINT ( 'NONE', #20737 ) ;
#35179 = EDGE_CURVE ( 'NONE', #242, #53998, #5918, .T. ) ;
#35181 = CARTESIAN_POINT ( 'NONE',  ( -100.4440683050664802, 32.98184228837414622, 72.15012103992511072 ) ) ;
#35182 = DIRECTION ( 'NONE',  ( 0.000000000000000000, 0.000000000000000000, 1.000000000000000000 ) ) ;
#35183 = ORIENTED_EDGE ( 'NONE', *, *, #24861, .T. ) ;
#35184 = VECTOR ( 'NONE', #5848, 1000.000000000000000 ) ;
#35185 = ADVANCED_FACE ( 'NONE', ( #5249 ), #53071, .T. ) ;
#35186 = EDGE_CURVE ( 'NONE', #22496, #49023, #13606, .T. ) ;
#35187 = CARTESIAN_POINT ( 'NONE',  ( -156.7435307435793845, 71.93726016406968427, -44.30516796381674283 ) ) ;
#35188 = CARTESIAN_POINT ( 'NONE',  ( 211.7357196141372526, 118.3691710715567353, -14.37225973309041827 ) ) ;
#35189 = CARTESIAN_POINT ( 'NONE',  ( -156.4960819023051499, 70.34114605623875605, -66.38289013128127181 ) ) ;
#35190 = DIRECTION ( 'NONE',  ( -0.000000000000000000, 0.000000000000000000, -1.000000000000000000 ) ) ;
#35191 = CARTESIAN_POINT ( 'NONE',  ( -47.55360235114366674, 12.79819361309569103, -70.07348629407573526 ) ) ;
#35192 = CARTESIAN_POINT ( 'NONE',  ( -4.506365319453812468, 7.705038994660875495, -22.80363844821005515 ) ) ;
#35193 = CARTESIAN_POINT ( 'NONE',  ( 179.0096185093687495, 76.53352131383243773, 2.743568850346190136 ) ) ;
#35194 = LINE ( 'NONE', #35547, #39933 ) ;
#35195 = VERTEX_POINT ( 'NONE', #18579 ) ;
#35196 = CARTESIAN_POINT ( 'NONE',  ( -101.3537077702550562, 33.43904726487055967, -35.05764247501280551 ) ) ;
#35197 = VERTEX_POINT ( 'NONE', #1012 ) ;
#35198 = CARTESIAN_POINT ( 'NONE',  ( 417.3372781065086201, 399.9999999999998863, 108.5502958579881891 ) ) ;
#35199 = B_SPLINE_CURVE_WITH_KNOTS ( 'NONE', 3,
 ( #32129, #41992, #58173, #106, #38088, #15610, #53906, #15949, #42341, #48617, #32474, #21231, #64133, #58849, #37394, #37059, #53565, #5045, #10320, #10661, #5727, #47595, #16632, #36727, #31783, #27186, #31108, #458, #5398, #20883, #21563, #52876, #25832, #63456, #9989, #26507, #58498, #4702, #21912, #42677, #43006, #53216, #43360, #37744 ),
 .UNSPECIFIED., .F., .F.,
 ( 4, 2, 2, 2, 2, 2, 2, 2, 2, 2, 2, 2, 2, 2, 2, 2, 2, 2, 2, 2, 2, 4 ),
 ( 0.02895403260893130923, 0.03071603688922217718, 0.03247804116951304165, 0.03424004544980391307, 0.03600204973009477755, 0.03776405401038564202, 0.03864505615053107773, 0.03952605829067650650, 0.04040706043082194221, 0.04128806257096737098, 0.04216906471111279975, 0.04305006685125822852, 0.04393106899140365729, 0.04481207113154909299, 0.04569307327169452176, 0.04657407541183995053, 0.04745507755198538624, 0.04833607969213081501, 0.05009808397242168643, 0.05186008825271255784, 0.05362209253300343620, 0.05714610109358520679 ),
 .UNSPECIFIED. ) ;
#35200 = EDGE_CURVE ( 'NONE', #34109, #31066, #39340, .T. ) ;
#35201 = CARTESIAN_POINT ( 'NONE',  ( 46.65860211212413589, 10.48377752989033951, -14.31619431203790960 ) ) ;
#35202 = LINE ( 'NONE', #67239, #14794 ) ;
#35203 = LINE ( 'NONE', #52744, #38988 ) ;
#35204 = CARTESIAN_POINT ( 'NONE',  ( 0.000000000000000000, 1.502314598737159031E-15, -8.000000000000000000 ) ) ;
#35205 = EDGE_CURVE ( 'NONE', #58006, #59279, #7690, .T. ) ;
#35206 = EDGE_CURVE ( 'NONE', #66816, #19283, #48244, .T. ) ;
#35207 = CARTESIAN_POINT ( 'NONE',  ( -107.0544991134679691, 36.41543129049374272, -21.45915251517910960 ) ) ;
#35208 = CARTESIAN_POINT ( 'NONE',  ( 447.3372781065086201, 0.000000000000000000, -146.4497041420118251 ) ) ;
#35209 = CARTESIAN_POINT ( 'NONE',  ( -165.6393662153604396, 79.16886183052815795, 65.77194331359760326 ) ) ;
#35210 = ORIENTED_EDGE ( 'NONE', *, *, #8894, .F. ) ;
#35211 = EDGE_LOOP ( 'NONE', ( #51419, #61501 ) ) ;
#35212 = DIRECTION ( 'NONE',  ( 0.000000000000000000, 0.000000000000000000, 1.000000000000000000 ) ) ;
#35213 = DIRECTION ( 'NONE',  ( -0.000000000000000000, -0.000000000000000000, 1.000000000000000000 ) ) ;
#35214 = CARTESIAN_POINT ( 'NONE',  ( 173.6710158776850506, 71.42507420636734139, -18.05732277655958384 ) ) ;
#35215 = CARTESIAN_POINT ( 'NONE',  ( 102.7414208686707582, 26.65627265923299305, 64.44516497733118854 ) ) ;
#35216 = CIRCLE ( 'NONE', #54254, 5.000000000000004441 ) ;
#35217 = CARTESIAN_POINT ( 'NONE',  ( -442.6627218934914367, 399.9999999999998863, -136.4497041420118251 ) ) ;
#35218 = MECHANICAL_DESIGN_GEOMETRIC_PRESENTATION_REPRESENTATION (  '', ( #65548 ), #18391 ) ;
#35219 = CARTESIAN_POINT ( 'NONE',  ( 55.51637278631173444, 12.08345311280959677, -16.88578774313057096 ) ) ;
#35220 = ORIENTED_EDGE ( 'NONE', *, *, #4239, .T. ) ;
#35221 = CARTESIAN_POINT ( 'NONE',  ( -64.61430802170492882, 7.070445451047392638, 40.00000000000003553 ) ) ;
#35222 = CARTESIAN_POINT ( 'NONE',  ( 18.20314211955701111, 7.596739727129572017, -50.13654653627244784 ) ) ;
#35223 = CARTESIAN_POINT ( 'NONE',  ( 15.29305096970402822, 7.491604910111008486, 71.85925826316895382 ) ) ;
#35224 = VECTOR ( 'NONE', #28012, 1000.000000000000000 ) ;
#35225 = FACE_BOUND ( 'NONE', #34404, .T. ) ;
#35226 = VECTOR ( 'NONE', #27192, 1000.000000000000114 ) ;
#35227 = VECTOR ( 'NONE', #4003, 1000.000000000000000 ) ;
#35228 = AXIS2_PLACEMENT_3D ( 'NONE', #7115, #22594, #50381 ) ;
#35229 = ORIENTED_EDGE ( 'NONE', *, *, #36903, .T. ) ;
#35230 = EDGE_LOOP ( 'NONE', ( #63760, #51300, #10857, #31546 ) ) ;
#35231 = DIRECTION ( 'NONE',  ( -1.000000000000000000, 0.000000000000000000, 0.000000000000000000 ) ) ;
#35232 = DIRECTION ( 'NONE',  ( -0.9639628606958512425, -0.2660368455666826670, 0.000000000000000000 ) ) ;
#35233 = CIRCLE ( 'NONE', #31867, 5.000000000000087930 ) ;
#35234 = LINE ( 'NONE', #46127, #63345 ) ;
#35235 = CARTESIAN_POINT ( 'NONE',  ( 50.71116719115956073, 28.84239711592981337, 27.58472315868180402 ) ) ;
#35236 = CARTESIAN_POINT ( 'NONE',  ( 15.12874021383972334, 6.480380938026408799, 83.72563133567338411 ) ) ;
#35237 = CARTESIAN_POINT ( 'NONE',  ( 83.38067517854670996, 18.33799117207140128, -76.93039019878386853 ) ) ;
#35238 = VERTEX_POINT ( 'NONE', #6633 ) ;
#35239 = LINE ( 'NONE', #13103, #42678 ) ;
#35240 = CARTESIAN_POINT ( 'NONE',  ( 203.9228889538744909, 106.9879579748728275, -51.29625234351511409 ) ) ;
#35241 = ORIENTED_EDGE ( 'NONE', *, *, #30736, .T. ) ;
#35242 = DIRECTION ( 'NONE',  ( -1.000000000000000000, 0.000000000000000000, 0.000000000000000000 ) ) ;
#35243 = ORIENTED_EDGE ( 'NONE', *, *, #40571, .T. ) ;
#35244 = EDGE_CURVE ( 'NONE', #23953, #17123, #65194, .T. ) ;
#35245 = DIRECTION ( 'NONE',  ( -1.000000000000000000, -0.000000000000000000, -0.000000000000000000 ) ) ;
#35246 = DIRECTION ( 'NONE',  ( -0.000000000000000000, -0.000000000000000000, -1.000000000000000000 ) ) ;
#35247 = CARTESIAN_POINT ( 'NONE',  ( 14.61870061263185150, 17.42188897416313154, -35.38129938736816626 ) ) ;
#35248 = ORIENTED_EDGE ( 'NONE', *, *, #36540, .F. ) ;
#35249 = ORIENTED_EDGE ( 'NONE', *, *, #30902, .T. ) ;
#35250 = DIRECTION ( 'NONE',  ( -0.000000000000000000, -0.000000000000000000, -1.000000000000000000 ) ) ;
#35251 = DIRECTION ( 'NONE',  ( 1.000000000000000000, 0.000000000000000000, 0.000000000000000000 ) ) ;
#35252 = CARTESIAN_POINT ( 'NONE',  ( 106.6181401479172166, 28.34160787025143335, 16.83688178611173214 ) ) ;
#35253 = EDGE_LOOP ( 'NONE', ( #21425, #9214, #68577, #55084, #57918, #8434, #34988, #65062, #42741, #59159, #4438, #27066 ) ) ;
#35254 = EDGE_CURVE ( 'NONE', #56777, #62166, #66334, .T. ) ;
#35255 = EDGE_CURVE ( 'NONE', #69403, #49926, #13541, .T. ) ;
#35256 = EDGE_CURVE ( 'NONE', #30847, #58924, #12969, .T. ) ;
#35257 = DIRECTION ( 'NONE',  ( 0.000000000000000000, 0.000000000000000000, 1.000000000000000000 ) ) ;
#35258 = CARTESIAN_POINT ( 'NONE',  ( 173.6737675136087660, 72.80308721038095143, -71.76398898605381760 ) ) ;
#35259 = VECTOR ( 'NONE', #56708, 1000.000000000000000 ) ;
#35260 = CARTESIAN_POINT ( 'NONE',  ( -442.6627218934913799, 394.9999999999998295, -125.1412729879898791 ) ) ;
#35261 = CARTESIAN_POINT ( 'NONE',  ( 110.7164744784864041, 29.10110206241302322, -9.077886975190001095 ) ) ;
#35262 = EDGE_CURVE ( 'NONE', #10027, #29060, #29137, .T. ) ;
#35263 = CARTESIAN_POINT ( 'NONE',  ( 79.54836217416617217, 18.17815803851260270, -45.80621361996720964 ) ) ;
#35264 = DIRECTION ( 'NONE',  ( 1.000000000000000000, 0.000000000000000000, -2.220446049250313081E-16 ) ) ;
#35265 = ORIENTED_EDGE ( 'NONE', *, *, #64555, .T. ) ;
#35266 = AXIS2_PLACEMENT_3D ( 'NONE', #20842, #25101, #4333 ) ;
#35267 = ORIENTED_EDGE ( 'NONE', *, *, #60222, .F. ) ;
#35268 = CIRCLE ( 'NONE', #15030, 65.36598343705435354 ) ;
#35269 = CARTESIAN_POINT ( 'NONE',  ( 46.50207827473962396, 9.439498081273464791, 8.140350865663473101 ) ) ;
#35270 = CARTESIAN_POINT ( 'NONE',  ( -6.214074258788039096, -32.84308722476502140, 6.893342931991226941 ) ) ;
#35271 = CARTESIAN_POINT ( 'NONE',  ( -452.6627218934861503, 370.0000000000064233, -146.4497041420121377 ) ) ;
#35272 = CARTESIAN_POINT ( 'NONE',  ( 122.2516123306975402, 190.0000000000000000, -21.28179539054375624 ) ) ;
#35273 = CARTESIAN_POINT ( 'NONE',  ( 128.9253503890652439, 38.52561778336672660, 4.509604327398147205 ) ) ;
#35274 = VECTOR ( 'NONE', #20151, 1000.000000000000000 ) ;
#35275 = PLANE ( 'NONE',  #5504 ) ;
#35276 = CARTESIAN_POINT ( 'NONE',  ( -836.0476379851789943, -568.5227338237882577, 10.00000000000000000 ) ) ;
#35277 = AXIS2_PLACEMENT_3D ( 'NONE', #12055, #49320, #38797 ) ;
#35278 = CARTESIAN_POINT ( 'NONE',  ( 211.3757499519976477, 117.8130818709823444, 40.13274018705065771 ) ) ;
#35279 = CARTESIAN_POINT ( 'NONE',  ( -81.23268307104839892, 24.39742801172154785, 57.71144102871279813 ) ) ;
#35280 = DIRECTION ( 'NONE',  ( 0.000000000000000000, 0.000000000000000000, 1.000000000000000000 ) ) ;
#35281 = ORIENTED_EDGE ( 'NONE', *, *, #66176, .T. ) ;
#35282 = AXIS2_PLACEMENT_3D ( 'NONE', #28489, #39055, #1767 ) ;
#35283 = CARTESIAN_POINT ( 'NONE',  ( 8.540564391411907152, 7.383006541823029067, -18.11898453561821398 ) ) ;
#35284 = ORIENTED_EDGE ( 'NONE', *, *, #29303, .T. ) ;
#35285 = LINE ( 'NONE', #23443, #63240 ) ;
#35286 = VERTEX_POINT ( 'NONE', #24568 ) ;
#35287 = FACE_OUTER_BOUND ( 'NONE', #22688, .T. ) ;
#35288 = CARTESIAN_POINT ( 'NONE',  ( 184.3879440808140373, 83.47316703125162007, -63.83297031623806816 ) ) ;
#35289 = CIRCLE ( 'NONE', #56464, 243.4957430088094839 ) ;
#35290 = CARTESIAN_POINT ( 'NONE',  ( -169.8972248494842745, 85.08697738648012887, 45.10824208028097360 ) ) ;
#35291 = CARTESIAN_POINT ( 'NONE',  ( -94.88380767928869375, 29.17964217339916289, -41.24520491189826288 ) ) ;
#35292 = EDGE_CURVE ( 'NONE', #34668, #13679, #30182, .T. ) ;
#35293 = CARTESIAN_POINT ( 'NONE',  ( -28.35957743809534648, 10.12373109553627337, 4.028907504916732663 ) ) ;
#35294 = FACE_OUTER_BOUND ( 'NONE', #37627, .T. ) ;
#35295 = CARTESIAN_POINT ( 'NONE',  ( 9.280894575734583540, 7.385644305345138605, -46.77988395504912944 ) ) ;
#35296 = EDGE_CURVE ( 'NONE', #36305, #6675, #41077, .T. ) ;
#35297 = CYLINDRICAL_SURFACE ( 'NONE', #48654, 7.500000000000020428 ) ;
#35298 = ORIENTED_EDGE ( 'NONE', *, *, #48882, .T. ) ;
#35299 = ORIENTED_EDGE ( 'NONE', *, *, #38351, .F. ) ;
#35300 = CARTESIAN_POINT ( 'NONE',  ( 185.5740152438940243, 84.73932458755626840, 84.48237900350213181 ) ) ;
#35301 = CARTESIAN_POINT ( 'NONE',  ( 50.98853755884139360, 388.0000000000071054, 91.05029585798797598 ) ) ;
#35302 = CARTESIAN_POINT ( 'NONE',  ( -452.6627218934913799, 0.000000000000000000, -111.4497041420118251 ) ) ;
#35303 = UNCERTAINTY_MEASURE_WITH_UNIT (LENGTH_MEASURE( 1.000000000000000082E-05 ), #55012, 'distance_accuracy_value', 'NONE');
#35304 = CARTESIAN_POINT ( 'NONE',  ( -34.39004539972345498, 0.000000000000000000, -5.000000000000000000 ) ) ;
#35305 = VERTEX_POINT ( 'NONE', #8025 ) ;
#35306 = DIRECTION ( 'NONE',  ( 0.000000000000000000, -1.000000000000000000, 0.000000000000000000 ) ) ;
#35307 = CARTESIAN_POINT ( 'NONE',  ( -62.30163634902122283, 17.79682011226254090, -71.54896639739239106 ) ) ;
#35308 = CARTESIAN_POINT ( 'NONE',  ( 176.6258282025054598, 74.21441092921637050, -76.60518865254823595 ) ) ;
#35309 = CARTESIAN_POINT ( 'NONE',  ( -173.9656771507954716, 88.06879734510549440, -34.71195716474998250 ) ) ;
#35310 = CARTESIAN_POINT ( 'NONE',  ( 106.4107271020440209, 27.14892220304137993, 3.815184072439286922 ) ) ;
#35311 = DIRECTION ( 'NONE',  ( -0.000000000000000000, -0.000000000000000000, 1.000000000000000000 ) ) ;
#35312 = CARTESIAN_POINT ( 'NONE',  ( 105.5071502593007722, 21.88997039781574472, 2.218170224452124195 ) ) ;
#35313 = CARTESIAN_POINT ( 'NONE',  ( -189.8133172329396814, 107.8858115918112901, 94.99999999999866418 ) ) ;
#35314 = VECTOR ( 'NONE', #12952, 1000.000000000000000 ) ;
#35315 = CARTESIAN_POINT ( 'NONE',  ( -3.868882431147342427, 6.665575841812235502, 58.08385180160794192 ) ) ;
#35316 = VERTEX_POINT ( 'NONE', #3785 ) ;
#35318 = CARTESIAN_POINT ( 'NONE',  ( 279.6684666882774195, 21.42428528562853174, 4.999999999999991118 ) ) ;
#35317 = COLOUR_RGB ( '',0.7921568627450980005, 0.8196078431372548767, 0.9333333333333333481 ) ;
#35319 = CARTESIAN_POINT ( 'NONE',  ( -128.1384526288949530, 47.98891607499722056, -76.42915334089175872 ) ) ;
#35320 = CARTESIAN_POINT ( 'NONE',  ( -109.7790042512818047, 37.90666514836944145, -69.65031332244757323 ) ) ;
#35321 = CARTESIAN_POINT ( 'NONE',  ( -48.04019567818504299, 12.91272349839804612, -40.04495495352035306 ) ) ;
#35322 = CARTESIAN_POINT ( 'NONE',  ( -64.18058723658653264, 10.37664328995176888, 41.38025477438755928 ) ) ;
#35323 = CARTESIAN_POINT ( 'NONE',  ( 7.762887554996211747E-14, 51.66904755831208718, 2.000000000000001776 ) ) ;
#35324 = AXIS2_PLACEMENT_3D ( 'NONE', #38146, #11402, #6131 ) ;
#35325 = ORIENTED_EDGE ( 'NONE', *, *, #6822, .T. ) ;
#35326 = VECTOR ( 'NONE', #49280, 1000.000000000000000 ) ;
#35327 = CARTESIAN_POINT ( 'NONE',  ( -6.774725108395958983, 24.06456107444435233, 0.000000000000000000 ) ) ;
#35328 = LINE ( 'NONE', #66660, #23732 ) ;
#35329 = ORIENTED_EDGE ( 'NONE', *, *, #24220, .T. ) ;
#35330 = ORIENTED_EDGE ( 'NONE', *, *, #6105, .F. ) ;
#35331 = EDGE_CURVE ( 'NONE', #35721, #60501, #48336, .T. ) ;
#35332 = VECTOR ( 'NONE', #45370, 1000.000000000000000 ) ;
#35333 = CARTESIAN_POINT ( 'NONE',  ( 178.1903523079567151, 75.72906488635189248, -50.65795404092384757 ) ) ;
#35334 = CARTESIAN_POINT ( 'NONE',  ( 150.2193536046551969, 53.46717047532150957, 34.97374097100669843 ) ) ;
#35335 = B_SPLINE_CURVE_WITH_KNOTS ( 'NONE', 3,
 ( #67693, #61704, #40946, #35327 ),
 .UNSPECIFIED., .F., .F.,
 ( 4, 4 ),
 ( 9.900409499073836656E-07, 0.05658314289920116785 ),
 .UNSPECIFIED. ) ;
#35336 = CARTESIAN_POINT ( 'NONE',  ( 0.000000000000000000, 0.000000000000000000, 0.000000000000000000 ) ) ;
#35337 = VERTEX_POINT ( 'NONE', #68499 ) ;
#35338 = DIRECTION ( 'NONE',  ( -0.9578262852211514300, 0.000000000000000000, -0.2873478855663451625 ) ) ;
#35339 = CARTESIAN_POINT ( 'NONE',  ( 122.2516123306975402, 190.0000000000000000, -91.28179539054376335 ) ) ;
#35340 = CARTESIAN_POINT ( 'NONE',  ( -5.416136198635860488, 6.745992685878680284, 3.664297029461999422 ) ) ;
#35341 = LINE ( 'NONE', #56800, #606 ) ;
#35342 = CARTESIAN_POINT ( 'NONE',  ( -84.53753601793931693, 25.73343139558518544, 33.22451195744211105 ) ) ;
#35343 = CARTESIAN_POINT ( 'NONE',  ( 156.3719388878481027, 56.80180099471265720, 83.17326589912873658 ) ) ;
#35344 = CARTESIAN_POINT ( 'NONE',  ( 141.2366329129481528, 46.06278879703612716, 8.803202109551088839 ) ) ;
#35345 = EDGE_CURVE ( 'NONE', #43782, #67945, #51636, .T. ) ;
#35346 = ORIENTED_EDGE ( 'NONE', *, *, #35179, .F. ) ;
#35347 = CARTESIAN_POINT ( 'NONE',  ( -836.0476379851789943, -568.5227338237882577, 0.000000000000000000 ) ) ;
#35348 = CARTESIAN_POINT ( 'NONE',  ( 99.99999999999997158, 0.000000000000000000, -25.00000000000000000 ) ) ;
#35349 = ADVANCED_FACE ( 'NONE', ( #14350 ), #19617, .F. ) ;
#35350 = CARTESIAN_POINT ( 'NONE',  ( 46.42281973867196854, 9.426811321855151249, -40.47057392414230037 ) ) ;
#35351 = EDGE_CURVE ( 'NONE', #55351, #28828, #35453, .T. ) ;
#35352 = DIRECTION ( 'NONE',  ( -1.000000000000000000, 0.000000000000000000, 0.000000000000000000 ) ) ;
#35354 = ORIENTED_EDGE ( 'NONE', *, *, #43789, .T. ) ;
#35353 = DIRECTION ( 'NONE',  ( -1.850169831522831466E-16, 1.000000000000000000, 1.110223024625156294E-16 ) ) ;
#35355 = CARTESIAN_POINT ( 'NONE',  ( 79.23200707685333555, 17.02828389812517074, -42.05917643671551787 ) ) ;
#35356 = ORIENTED_EDGE ( 'NONE', *, *, #8167, .F. ) ;
#35357 = EDGE_CURVE ( 'NONE', #29309, #17325, #64088, .T. ) ;
#35358 = ORIENTED_EDGE ( 'NONE', *, *, #50666, .F. ) ;
#35359 = DIRECTION ( 'NONE',  ( -0.000000000000000000, -0.000000000000000000, 1.000000000000000000 ) ) ;
#35360 = CARTESIAN_POINT ( 'NONE',  ( 79.19119222799093905, 18.06817527909836230, 38.20617424704751386 ) ) ;
#35361 = CARTESIAN_POINT ( 'NONE',  ( 197.6316695787931508, 97.13022718399025734, -68.13838693519056733 ) ) ;
#35362 = CARTESIAN_POINT ( 'NONE',  ( 10.55634918610403084, -3.079134169858832593E-14, 85.00100000000000477 ) ) ;
#35363 = DIRECTION ( 'NONE',  ( 1.000000000000000000, 0.000000000000000000, 0.000000000000000000 ) ) ;
#35364 = CARTESIAN_POINT ( 'NONE',  ( -81.90760111942957167, 24.66532273091449667, -8.990629716813376859 ) ) ;
#35365 = CARTESIAN_POINT ( 'NONE',  ( -175.9944734395086527, 91.92390745845763433, -8.426759268301923456 ) ) ;
#35366 = AXIS2_PLACEMENT_3D ( 'NONE', #32321, #31623, #57677 ) ;
#35367 = CARTESIAN_POINT ( 'NONE',  ( 204.6977192012829789, 108.0580384837234931, 17.36317014830577321 ) ) ;
#35368 = ORIENTED_EDGE ( 'NONE', *, *, #5567, .T. ) ;
#35369 = ORIENTED_EDGE ( 'NONE', *, *, #44601, .F. ) ;
#35370 = CARTESIAN_POINT ( 'NONE',  ( -104.5916564445180228, 35.10571011602407765, 18.32481510845080663 ) ) ;
#35371 = CARTESIAN_POINT ( 'NONE',  ( 15.78827728214693416, -170.0000000000000000, -89.20804527961313113 ) ) ;
#35372 = CARTESIAN_POINT ( 'NONE',  ( 0.000000000000000000, 0.000000000000000000, 170.0000000000000000 ) ) ;
#35373 = DIRECTION ( 'NONE',  ( 0.1342332658176667581, -0.9909497617679332571, 0.000000000000000000 ) ) ;
#35374 = CIRCLE ( 'NONE', #21895, 242.4895526022646379 ) ;
#35375 = DIRECTION ( 'NONE',  ( 0.000000000000000000, -0.000000000000000000, -1.000000000000000000 ) ) ;
#35376 = CARTESIAN_POINT ( 'NONE',  ( 19.10216788411014122, 6.629360741291162817, 30.78208475216976225 ) ) ;
#35377 = ADVANCED_FACE ( 'NONE', ( #13646 ), #52316, .F. ) ;
#35378 = CARTESIAN_POINT ( 'NONE',  ( -142.4962548760750281, 59.73493706050192031, 89.22523109323365986 ) ) ;
#35379 = ORIENTED_EDGE ( 'NONE', *, *, #53571, .T. ) ;
#35380 = ORIENTED_EDGE ( 'NONE', *, *, #3499, .T. ) ;
#35381 = VECTOR ( 'NONE', #39714, 1000.000000000000000 ) ;
#35382 = ORIENTED_EDGE ( 'NONE', *, *, #41809, .T. ) ;
#35383 = AXIS2_PLACEMENT_3D ( 'NONE', #36089, #19203, #20246 ) ;
#35384 = CARTESIAN_POINT ( 'NONE',  ( -72.74158548548088277, 20.15252735510585325, 86.99778511234599421 ) ) ;
#35385 = CARTESIAN_POINT ( 'NONE',  ( 173.9832054143776077, 71.71542822834034325, -95.00000000000133582 ) ) ;
#35386 = CARTESIAN_POINT ( 'NONE',  ( 66.94779593213118574, 13.61918177102166183, -36.82943163571080447 ) ) ;
#35387 = CARTESIAN_POINT ( 'NONE',  ( 69.72313848477121212, 27.50266661387133738, 41.38025477438755928 ) ) ;
#35388 = CARTESIAN_POINT ( 'NONE',  ( -25.87147652227456263, 100.0000000000000000, 77.58025477438755502 ) ) ;
#35389 = CARTESIAN_POINT ( 'NONE',  ( -37.93379515072631847, 11.77251734620209156, -73.44473663808183517 ) ) ;
#35390 = CARTESIAN_POINT ( 'NONE',  ( 56.52205390515081973, 12.28646189164058100, 41.09788869876410899 ) ) ;
#35391 = CARTESIAN_POINT ( 'NONE',  ( 43.73690422994441462, 9.012838840865988743, 84.97377783626691894 ) ) ;
#35392 = EDGE_LOOP ( 'NONE', ( #15726, #9791, #66613, #12051 ) ) ;
#35393 = CARTESIAN_POINT ( 'NONE',  ( -2.874437057892791803, 6.618922960888053098, -48.57289573616785816 ) ) ;
#35394 = DIRECTION ( 'NONE',  ( 0.000000000000000000, 0.000000000000000000, 1.000000000000000000 ) ) ;
#35395 = CARTESIAN_POINT ( 'NONE',  ( 31.11269837220800127, -26.11269837220812562, 0.000000000000000000 ) ) ;
#35396 = DIRECTION ( 'NONE',  ( 1.000000000000000000, 0.000000000000000000, 0.000000000000000000 ) ) ;
#35397 = CARTESIAN_POINT ( 'NONE',  ( 129.6961120139403647, 38.96846414226718736, -22.92345578965780462 ) ) ;
#35398 = CYLINDRICAL_SURFACE ( 'NONE', #35472, 7.500000000000027534 ) ;
#35399 = CARTESIAN_POINT ( 'NONE',  ( 6.400000000000000355, -4.618802153516998743, 7.999999999999998224 ) ) ;
#35400 = ORIENTED_EDGE ( 'NONE', *, *, #47714, .T. ) ;
#35401 = SHAPE_DEFINITION_REPRESENTATION ( #31558, #60409 ) ;
#35402 = PLANE ( 'NONE',  #38588 ) ;
#35403 = CARTESIAN_POINT ( 'NONE',  ( -33.12994257348896099, 10.89587983539684757, -50.12821252459180243 ) ) ;
#35404 = DIRECTION ( 'NONE',  ( 0.4738686624729966379, 0.8805955318567391110, -0.000000000000000000 ) ) ;
#35405 = CARTESIAN_POINT ( 'NONE',  ( 181.9411407973024950, 80.91291802046383452, -36.22505766587962484 ) ) ;
#35406 = ORIENTED_EDGE ( 'NONE', *, *, #58413, .F. ) ;
#35407 = ORIENTED_EDGE ( 'NONE', *, *, #21449, .F. ) ;
#35408 = ADVANCED_FACE ( 'NONE', ( #4139 ), #62537, .T. ) ;
#35409 = CARTESIAN_POINT ( 'NONE',  ( -29.04258984626622464, 9.210213971636679986, -23.08366245703133046 ) ) ;
#35410 = EDGE_CURVE ( 'NONE', #20839, #53439, #57318, .T. ) ;
#35411 = CARTESIAN_POINT ( 'NONE',  ( 200.8383807319521281, 102.8517715783673623, 3.418042344880998229 ) ) ;
#35412 = ORIENTED_EDGE ( 'NONE', *, *, #11242, .F. ) ;
#35413 = ADVANCED_FACE ( 'NONE', ( #51971 ), #25255, .F. ) ;
#35414 = CARTESIAN_POINT ( 'NONE',  ( 14.77197020583827580, -49.50853448602472895, 26.66469104408690427 ) ) ;
#35415 = ORIENTED_EDGE ( 'NONE', *, *, #49589, .T. ) ;
#35416 = CARTESIAN_POINT ( 'NONE',  ( -56.97556689808916275, 16.24958672959845885, 18.22614236532972498 ) ) ;
#35417 = CARTESIAN_POINT ( 'NONE',  ( 129.5193594945039308, 38.86618897895343139, 43.14722117905061083 ) ) ;
#35418 = AXIS2_PLACEMENT_3D ( 'NONE', #9575, #21491, #57412 ) ;
#35419 = EDGE_CURVE ( 'NONE', #33531, #13094, #47962, .T. ) ;
#35420 = CARTESIAN_POINT ( 'NONE',  ( -157.0069571479806996, 72.18154199622279066, 37.92026323496924789 ) ) ;
#35421 = DIRECTION ( 'NONE',  ( -1.000000000000000000, 0.000000000000000000, 0.000000000000000000 ) ) ;
#35422 = AXIS2_PLACEMENT_3D ( 'NONE', #17288, #49638, #65851 ) ;
#35424 = CARTESIAN_POINT ( 'NONE',  ( -20.55634918610400419, 15.55634918610405748, 0.000000000000000000 ) ) ;
#35423 = AXIS2_PLACEMENT_3D ( 'NONE', #62572, #58647, #30908 ) ;
#35426 = ORIENTED_EDGE ( 'NONE', *, *, #52318, .T. ) ;
#35425 = CARTESIAN_POINT ( 'NONE',  ( -31.11269837220801193, 31.11269837220812207, 85.00100000000000477 ) ) ;
#35427 = CARTESIAN_POINT ( 'NONE',  ( 55.56474667084417263, 11.06706367715628758, 38.30556224444529079 ) ) ;
#35428 = VECTOR ( 'NONE', #69055, 1000.000000000000114 ) ;
#35429 = ORIENTED_EDGE ( 'NONE', *, *, #17219, .T. ) ;
#35430 = ORIENTED_EDGE ( 'NONE', *, *, #11600, .F. ) ;
#35431 = CARTESIAN_POINT ( 'NONE',  ( -165.6208371326873419, 80.58821715390998008, 11.17930752570401332 ) ) ;
#35432 = VECTOR ( 'NONE', #10012, 1000.000000000000000 ) ;
#35433 = ADVANCED_FACE ( 'NONE', ( #56556 ), #62177, .F. ) ;
#35434 = CYLINDRICAL_SURFACE ( 'NONE', #67525, 7.500000000000020428 ) ;
#35435 = EDGE_CURVE ( 'NONE', #38900, #19572, #42736, .T. ) ;
#35437 = ORIENTED_EDGE ( 'NONE', *, *, #9138, .T. ) ;
#35436 = CARTESIAN_POINT ( 'NONE',  ( -131.6399667378751133, 51.62465701391631256, 69.81063530948696894 ) ) ;
#35438 = FACE_OUTER_BOUND ( 'NONE', #68611, .T. ) ;
#35439 = CARTESIAN_POINT ( 'NONE',  ( -71.57660578921959882, 20.81129687646280146, -40.11841413367452702 ) ) ;
#35440 = ORIENTED_EDGE ( 'NONE', *, *, #6019, .T. ) ;
#35441 = CARTESIAN_POINT ( 'NONE',  ( 175.0086665638700083, 74.06151034403055178, -93.01110694259065781 ) ) ;
#35442 = CARTESIAN_POINT ( 'NONE',  ( 136.1037846510193106, 43.98155406734453265, 44.18067958987710142 ) ) ;
#35443 = CARTESIAN_POINT ( 'NONE',  ( 123.4242852856285566, 0.000000000000000000, -20.00000000000000000 ) ) ;
#35444 = LINE ( 'NONE', #3431, #47089 ) ;
#35445 = CARTESIAN_POINT ( 'NONE',  ( 63.50537371531942910, 13.81987663608982331, -62.56524142263342014 ) ) ;
#35446 = ORIENTED_EDGE ( 'NONE', *, *, #61796, .F. ) ;
#35447 = ORIENTED_EDGE ( 'NONE', *, *, #6166, .T. ) ;
#35448 = CARTESIAN_POINT ( 'NONE',  ( 0.000000000000000000, 0.000000000000000000, 30.00000000000000000 ) ) ;
#35449 = CARTESIAN_POINT ( 'NONE',  ( -24.39004539972345498, 0.000000000000000000, -5.000000000000000000 ) ) ;
#35450 = DIRECTION ( 'NONE',  ( -0.000000000000000000, 1.000000000000000000, -0.000000000000000000 ) ) ;
#35451 = CARTESIAN_POINT ( 'NONE',  ( -55.05276343752910151, 14.68156374112637330, -88.90542517938719413 ) ) ;
#35452 = LINE ( 'NONE', #44351, #56754 ) ;
#35453 = LINE ( 'NONE', #9070, #24789 ) ;
#35454 = CARTESIAN_POINT ( 'NONE',  ( -146.5268141329886760, 61.69196909035590437, 45.10686021381179955 ) ) ;
#35455 = CARTESIAN_POINT ( 'NONE',  ( -121.5928001448269100, 44.91559452735375402, 44.28205460033795049 ) ) ;
#35456 = CARTESIAN_POINT ( 'NONE',  ( -172.3018509397888636, 86.22053936367348115, -61.58980725186435734 ) ) ;
#35457 = ORIENTED_EDGE ( 'NONE', *, *, #33608, .T. ) ;
#35458 = CARTESIAN_POINT ( 'NONE',  ( -109.4995148930278646, 37.75156937139183100, 35.92031809713896706 ) ) ;
#35459 = ORIENTED_EDGE ( 'NONE', *, *, #51461, .F. ) ;
#35460 = VECTOR ( 'NONE', #37850, 1000.000000000000000 ) ;
#35461 = CARTESIAN_POINT ( 'NONE',  ( -180.4790817662267557, 95.71028656509025723, -94.42029243692577722 ) ) ;
#35462 = CARTESIAN_POINT ( 'NONE',  ( 0.000000000000000000, 0.000000000000000000, 170.0000000000000000 ) ) ;
#35463 = ORIENTED_EDGE ( 'NONE', *, *, #29394, .F. ) ;
#35464 = DIRECTION ( 'NONE',  ( 0.000000000000000000, 0.000000000000000000, 1.000000000000000000 ) ) ;
#35465 = PLANE ( 'NONE',  #61428 ) ;
#35466 = DIRECTION ( 'NONE',  ( 0.000000000000000000, 0.000000000000000000, 1.000000000000000000 ) ) ;
#35468 = DIRECTION ( 'NONE',  ( -0.000000000000000000, 1.000000000000000000, -0.000000000000000000 ) ) ;
#35467 = VECTOR ( 'NONE', #48830, 1000.000000000000000 ) ;
#35469 = DIRECTION ( 'NONE',  ( 5.055952397801357946E-18, -6.848752866791659805E-19, -1.000000000000000000 ) ) ;
#35470 = CARTESIAN_POINT ( 'NONE',  ( 15.78827728214693416, -170.0000000000000000, 10.67015708224156079 ) ) ;
#35471 = PLANE ( 'NONE',  #60741 ) ;
#35472 = AXIS2_PLACEMENT_3D ( 'NONE', #8677, #68442, #25884 ) ;
#35473 = AXIS2_PLACEMENT_3D ( 'NONE', #15249, #41630, #52529 ) ;
#35474 = ORIENTED_EDGE ( 'NONE', *, *, #23599, .F. ) ;
#35475 = DIRECTION ( 'NONE',  ( 0.000000000000000000, 0.000000000000000000, 1.000000000000000000 ) ) ;
#35476 = ORIENTED_EDGE ( 'NONE', *, *, #48256, .F. ) ;
#35477 = LINE ( 'NONE', #30207, #10404 ) ;
#35478 = CARTESIAN_POINT ( 'NONE',  ( -62.06231780744546001, 17.72446026058427293, 67.34115632414402342 ) ) ;
#35479 = CARTESIAN_POINT ( 'NONE',  ( -189.2442476610617916, 107.0963225822736007, 12.01318184954264368 ) ) ;
#35480 = EDGE_LOOP ( 'NONE', ( #32727, #12807, #20507, #23481, #34049, #62747, #35708, #51964 ) ) ;
#35481 = DIRECTION ( 'NONE',  ( -0.000000000000000000, -1.000000000000000000, -0.000000000000000000 ) ) ;
#35482 = CARTESIAN_POINT ( 'NONE',  ( -57.15434679788744887, 15.25497255977697186, -89.20270284046692666 ) ) ;
#35483 = CARTESIAN_POINT ( 'NONE',  ( -37.79601571721867970, 10.72155118426296738, 41.70395869289448143 ) ) ;
#35484 = CARTESIAN_POINT ( 'NONE',  ( 135.4423125506058909, 42.39015362494584593, -50.85732353738030298 ) ) ;
#35485 = AXIS2_PLACEMENT_3D ( 'NONE', #10178, #47810, #59397 ) ;
#35486 =( REPRESENTATION_RELATIONSHIP ('NONE','NONE', #40274, #60409 ) REPRESENTATION_RELATIONSHIP_WITH_TRANSFORMATION ( #42283 )SHAPE_REPRESENTATION_RELATIONSHIP( ) );
#35487 = ORIENTED_EDGE ( 'NONE', *, *, #65928, .T. ) ;
#35488 =( NAMED_UNIT ( * ) SI_UNIT ( $, .STERADIAN. ) SOLID_ANGLE_UNIT ( ) );
#35489 = CARTESIAN_POINT ( 'NONE',  ( -156.7435307435793845, 71.93726016406968427, 63.07303439803798994 ) ) ;
#35490 = LINE ( 'NONE', #52686, #34627 ) ;
#35491 = CYLINDRICAL_SURFACE ( 'NONE', #27668, 30.00000000000000000 ) ;
#35492 = ORIENTED_EDGE ( 'NONE', *, *, #43892, .F. ) ;
#35493 = CARTESIAN_POINT ( 'NONE',  ( -175.9944734395087096, 91.92390745845763433, -62.11586044922930938 ) ) ;
#35494 = CARTESIAN_POINT ( 'NONE',  ( 134.2297964129789136, 42.82763724447237053, 83.20224964760393505 ) ) ;
#35495 = CARTESIAN_POINT ( 'NONE',  ( 117.7411475730015269, 32.50808475802734421, 36.56858284938125792 ) ) ;
#35496 = EDGE_CURVE ( 'NONE', #65265, #12369, #62880, .T. ) ;
#35497 = CARTESIAN_POINT ( 'NONE',  ( -55.05276343752909440, 15.72344139423347364, -62.06087458892354647 ) ) ;
#35498 = EDGE_CURVE ( 'NONE', #69361, #43260, #14633, .T. ) ;
#35499 = B_SPLINE_CURVE_WITH_KNOTS ( 'NONE', 3,
 ( #28785, #7330, #12254, #50927, #7681, #38994, #29128, #1700, #40026, #61486, #45296, #33717, #60778, #23158, #13306, #6622, #8016, #24208, #49874, #65728, #45654, #67133, #18921, #61815, #49514, #17517, #55147, #6973, #44607, #39335, #12602, #30509, #51283, #9751, #8375, #20635, #45992, #35093, #25928, #56905, #9059, #52307, #3098, #40708, #24557, #9405, #51962, #67462 ),
 .UNSPECIFIED., .F., .F.,
 ( 4, 2, 2, 2, 2, 2, 2, 2, 2, 2, 2, 2, 2, 2, 2, 2, 2, 2, 2, 2, 2, 2, 2, 4 ),
 ( 0.02554216173022672356, 0.02715505844859244372, 0.02796150680777527431, 0.02876795516695810837, 0.03038085188532369668, 0.03199374860368928153, 0.03360664532205487331, 0.03441309368123766227, 0.03521954204042045122, 0.03602599039960324712, 0.03683243875878603607, 0.03844533547715162092, 0.03925178383633440987, 0.04005823219551719883, 0.04086468055469999472, 0.04167112891388279061, 0.04247757727306557263, 0.04328402563224836852, 0.04489692235061398806, 0.04650981906897960760, 0.04731626742816241737, 0.04812271578734523408, 0.04973561250571080505, 0.05134850922407638296 ),
 .UNSPECIFIED. ) ;
#35500 = CARTESIAN_POINT ( 'NONE',  ( 0.000000000000000000, 0.000000000000000000, 40.00000000000003553 ) ) ;
#35501 = ORIENTED_EDGE ( 'NONE', *, *, #67054, .T. ) ;
#35502 = LINE ( 'NONE', #35149, #800 ) ;
#35503 = CARTESIAN_POINT ( 'NONE',  ( 114.6890011751076344, 30.99337387307412683, -64.20757585925009892 ) ) ;
#35504 = CARTESIAN_POINT ( 'NONE',  ( 67.55134213333079174, 13.77030723107741217, 58.16423836707232198 ) ) ;
#35505 = CARTESIAN_POINT ( 'NONE',  ( 141.0517870458593279, 47.14452711594498169, 12.29862548867962957 ) ) ;
#35506 = EDGE_CURVE ( 'NONE', #25468, #15010, #30423, .T. ) ;
#35507 = CARTESIAN_POINT ( 'NONE',  ( -84.49322488516129681, 0.000000000000000000, 43.58025477438756212 ) ) ;
#35508 = VERTEX_POINT ( 'NONE', #69517 ) ;
#35509 = CARTESIAN_POINT ( 'NONE',  ( 164.4760519199595592, 64.62478832434435105, -14.04941869432099644 ) ) ;
#35510 = ORIENTED_EDGE ( 'NONE', *, *, #51660, .F. ) ;
#35511 = VECTOR ( 'NONE', #65828, 1000.000000000000000 ) ;
#35512 = CYLINDRICAL_SURFACE ( 'NONE', #7567, 7.500000000000013323 ) ;
#35513 = CARTESIAN_POINT ( 'NONE',  ( 135.1687848281947879, 42.22135448245729350, 83.28891585102797990 ) ) ;
#35514 = EDGE_CURVE ( 'NONE', #28520, #53742, #10220, .T. ) ;
#35515 = AXIS2_PLACEMENT_3D ( 'NONE', #25952, #62552, #14362 ) ;
#35517 = ORIENTED_EDGE ( 'NONE', *, *, #51624, .T. ) ;
#35516 = DIRECTION ( 'NONE',  ( -0.000000000000000000, -0.000000000000000000, 1.000000000000000000 ) ) ;
#35518 = CARTESIAN_POINT ( 'NONE',  ( 164.0105905242218398, 64.23277447906895077, -47.30424189763910903 ) ) ;
#35519 = CARTESIAN_POINT ( 'NONE',  ( 86.62931800182293784, 19.42108912189599934, 17.86753698201564688 ) ) ;
#35520 = CARTESIAN_POINT ( 'NONE',  ( 164.3702714028688661, 63.22112480708620552, -40.67253380548667252 ) ) ;
#35521 = AXIS2_PLACEMENT_3D ( 'NONE', #41624, #32108, #5372 ) ;
#35522 = VECTOR ( 'NONE', #46568, 999.9999999999998863 ) ;
#35523 = ORIENTED_EDGE ( 'NONE', *, *, #17786, .F. ) ;
#35524 = AXIS2_PLACEMENT_3D ( 'NONE', #66741, #55824, #33680 ) ;
#35525 = CYLINDRICAL_SURFACE ( 'NONE', #31115, 75.31295361348102801 ) ;
#35526 = B_SPLINE_CURVE_WITH_KNOTS ( 'NONE', 3,
 ( #44958, #66444, #13311, #33722, #24213, #12967, #17884, #39341, #67140, #1355, #22807, #55153, #38640, #11901, #18231, #49880, #1706, #60784 ),
 .UNSPECIFIED., .F., .F.,
 ( 4, 2, 2, 2, 2, 2, 2, 2, 4 ),
 ( 0.000000000000000000, 0.001730692900494939504, 0.002596039350742405244, 0.003461385800989870767, 0.005192078701484792273, 0.006922771601979714647, 0.008653464502474636152, 0.01038415740296955853, 0.01384554320395945531 ),
 .UNSPECIFIED. ) ;
#35527 = VECTOR ( 'NONE', #54536, 1000.000000000000000 ) ;
#35528 = CARTESIAN_POINT ( 'NONE',  ( -128.1219934350341703, 47.97781708504718523, 45.29597212495090730 ) ) ;
#35529 = DIRECTION ( 'NONE',  ( 0.000000000000000000, 0.000000000000000000, 1.000000000000000000 ) ) ;
#35530 = CIRCLE ( 'NONE', #62498, 63.00000000000000000 ) ;
#35531 = CARTESIAN_POINT ( 'NONE',  ( 84.05289558242220949, 19.61733656419350424, -23.52466748769439064 ) ) ;
#35532 = CARTESIAN_POINT ( 'NONE',  ( -172.7154982671752350, 86.67743928531949393, 30.82169460664102445 ) ) ;
#35533 = CARTESIAN_POINT ( 'NONE',  ( -34.74740905761644427, 10.15745573515589051, -62.91308403526972626 ) ) ;
#35534 = LINE ( 'NONE', #4549, #56318 ) ;
#35535 = ORIENTED_EDGE ( 'NONE', *, *, #16192, .T. ) ;
#35536 = CARTESIAN_POINT ( 'NONE',  ( -98.67557579989346550, 32.10670856967970366, 58.26914703332497680 ) ) ;
#35537 = CARTESIAN_POINT ( 'NONE',  ( -25.99999999999999289, 29.79383981485516841, -25.00000000000000000 ) ) ;
#35538 = ORIENTED_EDGE ( 'NONE', *, *, #40705, .F. ) ;
#35539 = CARTESIAN_POINT ( 'NONE',  ( 151.7783534118502189, 54.60545177578660514, -11.88952959584610447 ) ) ;
#35540 = DIRECTION ( 'NONE',  ( 0.000000000000000000, -1.000000000000000000, 0.000000000000000000 ) ) ;
#35541 = CARTESIAN_POINT ( 'NONE',  ( 104.4006536356074264, 27.36759527624478849, 32.38183756136254488 ) ) ;
#35542 = LINE ( 'NONE', #46083, #69185 ) ;
#35543 = CARTESIAN_POINT ( 'NONE',  ( 60.76851555108127911, 12.16255188786386121, 83.83909766377725248 ) ) ;
#35544 = CARTESIAN_POINT ( 'NONE',  ( 184.3879440808139805, 83.47316703125160586, 16.70068145515297076 ) ) ;
#35545 = CARTESIAN_POINT ( 'NONE',  ( 208.6132326550594485, 111.8685719053116685, -37.41518418271493829 ) ) ;
#35546 = CYLINDRICAL_SURFACE ( 'NONE', #16387, 7.500000000000013323 ) ;
#35547 = CARTESIAN_POINT ( 'NONE',  ( 74.39890044415652426, -7.951074708186081530, 43.58025477438756923 ) ) ;
#35548 = ORIENTED_EDGE ( 'NONE', *, *, #51238, .T. ) ;
#35549 = CARTESIAN_POINT ( 'NONE',  ( -41.50537345350708307, 50.04124777106294886, 43.58025477438756923 ) ) ;
#35550 = VERTEX_POINT ( 'NONE', #33991 ) ;
#35551 = CARTESIAN_POINT ( 'NONE',  ( 103.9652201950894863, 26.08439499369982784, -66.15590445722637014 ) ) ;
#35552 = CARTESIAN_POINT ( 'NONE',  ( 3.673940397442059178E-15, 70.00000000000000000, 30.00000000000000000 ) ) ;
#35553 = PRESENTATION_STYLE_ASSIGNMENT (( #20395 ) ) ;
#35554 = CARTESIAN_POINT ( 'NONE',  ( 25.00000000000000000, 3.061616997868383043E-15, 30.00000000000000000 ) ) ;
#35555 = CARTESIAN_POINT ( 'NONE',  ( -1.186912488840190738, 6.549538057797848367, 87.79949317012332699 ) ) ;
#35556 = DIRECTION ( 'NONE',  ( -1.000000000000000000, 0.000000000000000000, 0.000000000000000000 ) ) ;
#35557 = EDGE_LOOP ( 'NONE', ( #40534, #53076, #48176, #13907 ) ) ;
#35558 = EDGE_CURVE ( 'NONE', #24043, #17523, #28133, .T. ) ;
#35559 = FACE_OUTER_BOUND ( 'NONE', #14734, .T. ) ;
#35560 = CARTESIAN_POINT ( 'NONE',  ( -172.3057147739576749, 86.22480007276996616, 57.69916216524889307 ) ) ;
#35561 = ORIENTED_EDGE ( 'NONE', *, *, #64944, .F. ) ;
#35562 = EDGE_LOOP ( 'NONE', ( #8788, #37796, #60336, #54133 ) ) ;
#35563 = CARTESIAN_POINT ( 'NONE',  ( -154.7998111145352027, 68.80117179139328698, 32.88503397576067044 ) ) ;
#35564 = CARTESIAN_POINT ( 'NONE',  ( 24.86543756664854143, -29.17542814769260318, 13.32819299319723250 ) ) ;
#35565 = CARTESIAN_POINT ( 'NONE',  ( 173.8575673535406168, 71.59843387604338716, -18.90830546057937056 ) ) ;
#35566 = VECTOR ( 'NONE', #34349, 1000.000000000000000 ) ;
#35567 = CARTESIAN_POINT ( 'NONE',  ( 104.7042813665017746, 27.49927371769997819, 69.03645308503956812 ) ) ;
#35568 = LINE ( 'NONE', #57028, #2685 ) ;
#35569 = VECTOR ( 'NONE', #66718, 1000.000000000000000 ) ;
#35570 = CARTESIAN_POINT ( 'NONE',  ( 55.77012379229940819, 12.13428856597101557, -14.42319032175540450 ) ) ;
#35571 = EDGE_LOOP ( 'NONE', ( #36212, #11586, #14482, #47785 ) ) ;
#35572 = DIRECTION ( 'NONE',  ( 0.000000000000000000, 0.000000000000000000, -1.000000000000000000 ) ) ;
#35573 = VECTOR ( 'NONE', #27955, 1000.000000000000000 ) ;
#35574 = ORIENTED_EDGE ( 'NONE', *, *, #61789, .F. ) ;
#35575 = CARTESIAN_POINT ( 'NONE',  ( 210.6475357757682332, 114.8748261044495962, 5.289591715120433690 ) ) ;
#35576 = CARTESIAN_POINT ( 'NONE',  ( -142.3260422482980516, 59.60034523324940636, 40.45550101730454884 ) ) ;
#35577 = CARTESIAN_POINT ( 'NONE',  ( 210.6475357757682332, 114.8748261044495962, 32.13414230558411333 ) ) ;
#35578 = FACE_BOUND ( 'NONE', #67494, .T. ) ;
#35579 = EDGE_CURVE ( 'NONE', #14950, #46092, #45594, .T. ) ;
#35580 = EDGE_CURVE ( 'NONE', #36414, #39565, #12888, .T. ) ;
#35581 = EDGE_CURVE ( 'NONE', #57236, #65498, #28680, .T. ) ;
#35582 = ORIENTED_EDGE ( 'NONE', *, *, #50364, .F. ) ;
#35583 = ORIENTED_EDGE ( 'NONE', *, *, #15772, .T. ) ;
#35584 = PLANE ( 'NONE',  #6421 ) ;
#35585 = CARTESIAN_POINT ( 'NONE',  ( -119.1595461276717742, 43.39759378353400621, 88.49148495774751666 ) ) ;
#35586 = DIRECTION ( 'NONE',  ( 1.000000000000000000, -0.000000000000000000, 0.000000000000000000 ) ) ;
#35587 = CARTESIAN_POINT ( 'NONE',  ( -179.5186635612083705, 96.12511541314938768, 15.42972251793390903 ) ) ;
#35588 = ADVANCED_FACE ( 'NONE', ( #29066 ), #17446, .F. ) ;
#35589 = CARTESIAN_POINT ( 'NONE',  ( 8.469671715138490597, 6.376661621676603886, 92.87585994188762584 ) ) ;
#35590 = CARTESIAN_POINT ( 'NONE',  ( 60.40479419793764038, 24.00543350795394915, 40.00000000000003553 ) ) ;
#35591 = ORIENTED_EDGE ( 'NONE', *, *, #2182, .T. ) ;
#35592 = CARTESIAN_POINT ( 'NONE',  ( 18.89356949897823768, 62.19351277735707839, 170.0000000000000000 ) ) ;
#35593 = CARTESIAN_POINT ( 'NONE',  ( 201.9822477997853412, 104.3642793804899895, -50.82886203894460664 ) ) ;
#35594 = EDGE_LOOP ( 'NONE', ( #24631, #47708, #5815, #31831 ) ) ;
#35595 = DIRECTION ( 'NONE',  ( 0.000000000000000000, -0.000000000000000000, 1.000000000000000000 ) ) ;
#35596 = ORIENTED_EDGE ( 'NONE', *, *, #31514, .T. ) ;
#35597 = CARTESIAN_POINT ( 'NONE',  ( -79.62258606008205675, 22.68765733708499255, -76.91402268787508945 ) ) ;
#35598 = CARTESIAN_POINT ( 'NONE',  ( -27.00000000000000355, -30.00000000000000355, 0.000000000000000000 ) ) ;
#35599 = B_SPLINE_CURVE_WITH_KNOTS ( 'NONE', 3,
 ( #17144, #6957, #48797, #59708, #59367, #7316, #11179, #54077, #60061, #38262, #11881, #49497, #38978, #54428, #22091, #23145, #27354, #55485, #27708, #43875, #34046, #17863 ),
 .UNSPECIFIED., .F., .F.,
 ( 4, 2, 2, 2, 2, 2, 2, 2, 2, 2, 4 ),
 ( 0.000000000000000000, 0.001465307722066868214, 0.002197961583100300695, 0.002930615444133732525, 0.004395923166200650829, 0.005128577027234123425, 0.005861230888267594287, 0.007326538610334516928, 0.008791846332401438702, 0.01025715405446836308, 0.01172246177653528745 ),
 .UNSPECIFIED. ) ;
#35601 = VERTEX_POINT ( 'NONE', #33650 ) ;
#35600 = ADVANCED_FACE ( 'NONE', ( #60371 ), #43477, .T. ) ;
#35602 = VERTEX_POINT ( 'NONE', #932 ) ;
#35603 = CARTESIAN_POINT ( 'NONE',  ( 15.29293866748104769, 6.484959508098438796, -35.51894409868578606 ) ) ;
#35604 = EDGE_CURVE ( 'NONE', #20984, #902, #21398, .T. ) ;
#35606 = ADVANCED_FACE ( 'NONE', ( #43822 ), #65299, .T. ) ;
#35605 = DIRECTION ( 'NONE',  ( -1.000000000000000000, -0.000000000000000000, -0.000000000000000000 ) ) ;
#35607 = EDGE_CURVE ( 'NONE', #32410, #9716, #6898, .T. ) ;
#35608 = CARTESIAN_POINT ( 'NONE',  ( 106.4072861358879010, 28.24787347451999153, 16.71615381848508974 ) ) ;
#35609 = VERTEX_POINT ( 'NONE', #51558 ) ;
#35610 = PRODUCT_DEFINITION_SHAPE ( 'NONE', 'NONE',  #43475 ) ;
#35611 = CARTESIAN_POINT ( 'NONE',  ( -24.05175394599741523, 8.494885318775043714, 89.95382958585727806 ) ) ;
#35612 = VECTOR ( 'NONE', #65671, 1000.000000000000000 ) ;
#35613 = CARTESIAN_POINT ( 'NONE',  ( 174.9161599490640526, 73.97365196673302989, -74.84476842227203974 ) ) ;
#35614 = DIRECTION ( 'NONE',  ( -0.000000000000000000, 1.000000000000000000, -0.000000000000000000 ) ) ;
#35615 = CARTESIAN_POINT ( 'NONE',  ( -45.81425895439360829, -46.10914959592906825, 170.0000000000000000 ) ) ;
#35616 = CARTESIAN_POINT ( 'NONE',  ( -31.43908319763709969, 9.591432048623765638, 30.21645440618916112 ) ) ;
#35617 = VECTOR ( 'NONE', #60395, 1000.000000000000000 ) ;
#35618 = CARTESIAN_POINT ( 'NONE',  ( -166.2471992823174958, 81.23280767746210529, -92.85267937552322337 ) ) ;
#35619 = ORIENTED_EDGE ( 'NONE', *, *, #27011, .T. ) ;
#35620 = AXIS2_PLACEMENT_3D ( 'NONE', #68049, #57483, #3326 ) ;
#35621 = ORIENTED_EDGE ( 'NONE', *, *, #15715, .F. ) ;
#35622 = CARTESIAN_POINT ( 'NONE',  ( 43.14712943604300222, 8.926114770663675202, 17.07187046130982822 ) ) ;
#35623 = CARTESIAN_POINT ( 'NONE',  ( 116.8004147899731748, 32.03558746084399189, -93.44768873162850298 ) ) ;
#35624 = LINE ( 'NONE', #57764, #66027 ) ;
#35625 = LINE ( 'NONE', #57078, #16418 ) ;
#35626 = AXIS2_PLACEMENT_3D ( 'NONE', #41519, #52071, #3887 ) ;
#35627 = CARTESIAN_POINT ( 'NONE',  ( 126.5880720616305553, 37.20544379858411332, 12.03288608235020973 ) ) ;
#35628 = FACE_OUTER_BOUND ( 'NONE', #62538, .T. ) ;
#35629 = CARTESIAN_POINT ( 'NONE',  ( 211.6571441797747468, 118.2476110685686592, 87.59423805443044841 ) ) ;
#35630 = CARTESIAN_POINT ( 'NONE',  ( 207.4610690199661462, 111.9701171077052209, 43.69190904262227093 ) ) ;
#35631 = DIRECTION ( 'NONE',  ( 0.000000000000000000, 0.000000000000000000, 1.000000000000000000 ) ) ;
#35632 = FACE_OUTER_BOUND ( 'NONE', #66293, .T. ) ;
#35633 = EDGE_LOOP ( 'NONE', ( #47670, #51046, #33550, #23106 ) ) ;
#35634 = AXIS2_PLACEMENT_3D ( 'NONE', #64234, #17797, #56457 ) ;
#35635 = ITEM_DEFINED_TRANSFORMATION ( 'NONE', 'NONE', #45560,  #66832 ) ;
#35636 = CARTESIAN_POINT ( 'NONE',  ( 14.08810621383467243, 7.458732232275137264, -23.48329793243775399 ) ) ;
#35637 = ORIENTED_EDGE ( 'NONE', *, *, #3263, .F. ) ;
#35638 = CARTESIAN_POINT ( 'NONE',  ( 199.3671895066314335, 99.30947926630335587, -22.28159174662976483 ) ) ;
#35639 = VERTEX_POINT ( 'NONE', #29400 ) ;
#35640 = B_SPLINE_CURVE_WITH_KNOTS ( 'NONE', 3,
 ( #1805, #30516, #51631, #55600, #24902, #46333, #12696, #34162, #7429, #2149, #23604, #9411, #68821, #42781, #20999, #10093, #20642, #42103, #47036, #16057, #37509, #25933, #63563, #31550, #26620, #4134, #21332, #58962, #10777, #36142, #52312, #69171, #3779, #36835, #19971, #57599, #4475, #64249, #20299, #42446, #4809, #30869, #51967, #68494, #15717, #15373 ),
 .UNSPECIFIED., .F., .F.,
 ( 4, 2, 2, 2, 2, 2, 2, 2, 2, 2, 2, 2, 2, 2, 2, 2, 2, 2, 2, 2, 2, 2, 4 ),
 ( 0.02989107162308292723, 0.03170280136394034581, 0.03351453110479776093, 0.03532626084565517605, 0.03713799058651259116, 0.03894972032737000628, 0.03985558519779868608, 0.04076145006822736588, 0.04166731493865603875, 0.04257317980908471855, 0.04347904467951339835, 0.04438490954994207816, 0.04529077442037075796, 0.04619663929079943776, 0.04710250416122811756, 0.04800836903165679737, 0.04891423390208547717, 0.04982009877251415697, 0.05163182851337153045, 0.05344355825422891781, 0.05525528799508629130, 0.05706701773594367866, 0.05887874747680105214 ),
 .UNSPECIFIED. ) ;
#35641 = DIRECTION ( 'NONE',  ( 0.000000000000000000, -0.9940777367219241212, 0.1086713087885527174 ) ) ;
#35642 = CARTESIAN_POINT ( 'NONE',  ( 0.000000000000000000, 0.000000000000000000, 41.38025477438755928 ) ) ;
#35643 = CARTESIAN_POINT ( 'NONE',  ( -168.0003605155415016, 83.06333427281275306, 32.83646999918969556 ) ) ;
#35644 = CARTESIAN_POINT ( 'NONE',  ( 33.03621582719332395, 7.666716336587119152, -47.09313870449056338 ) ) ;
#35645 = CARTESIAN_POINT ( 'NONE',  ( -106.6940984894958149, 35.07986071359381697, 5.092223517931543597 ) ) ;
#35646 = EDGE_CURVE ( 'NONE', #33134, #913, #19536, .T. ) ;
#35647 = CARTESIAN_POINT ( 'NONE',  ( 10.15118267943872787, 7.391905976536038203, -47.97213281097538129 ) ) ;
#35648 = PLANE ( 'NONE',  #61043 ) ;
#35649 = ORIENTED_EDGE ( 'NONE', *, *, #56243, .T. ) ;
#35650 = VERTEX_POINT ( 'NONE', #30441 ) ;
#35651 = EDGE_CURVE ( 'NONE', #28296, #68802, #30791, .T. ) ;
#35652 = LINE ( 'NONE', #30367, #63043 ) ;
#35653 = CARTESIAN_POINT ( 'NONE',  ( 0.000000000000000000, 0.000000000000000000, 170.0000000000000000 ) ) ;
#35654 = B_SPLINE_CURVE_WITH_KNOTS ( 'NONE', 3,
 ( #4090, #4427, #20259, #41717, #47666, #31178 ),
 .UNSPECIFIED., .F., .F.,
 ( 4, 2, 4 ),
 ( 0.03218943375184197403, 0.06469838935233396260, 0.09720734495282595811 ),
 .UNSPECIFIED. ) ;
#35655 = CARTESIAN_POINT ( 'NONE',  ( -29.75049355503753645, 9.320234381800291956, -76.97328196399489286 ) ) ;
#35656 = DIRECTION ( 'NONE',  ( -1.000000000000000000, 0.000000000000000000, 0.000000000000000000 ) ) ;
#35657 = CARTESIAN_POINT ( 'NONE',  ( 284.4903733860909938, 21.88945422885941028, -2.223679814509739394 ) ) ;
#35658 = CARTESIAN_POINT ( 'NONE',  ( 0.000000000000000000, 0.000000000000000000, 0.000000000000000000 ) ) ;
#35659 = CARTESIAN_POINT ( 'NONE',  ( 173.5837434292114096, 71.34409607026154276, -70.85766065640814304 ) ) ;
#35660 = CARTESIAN_POINT ( 'NONE',  ( -180.6213815675304772, 95.88446356933845038, -42.52151308631101756 ) ) ;
#35661 = CARTESIAN_POINT ( 'NONE',  ( 8.000000000000000000, 4.618802153516997855, -9.500000000000000000 ) ) ;
#35662 = CARTESIAN_POINT ( 'NONE',  ( -171.0758681675585819, 84.87997360100519018, 18.70530542384813089 ) ) ;
#35663 = CARTESIAN_POINT ( 'NONE',  ( 51.85299110299499148, -39.21848821248373440, 170.0000000000000000 ) ) ;
#35664 = EDGE_CURVE ( 'NONE', #49951, #64171, #62800, .T. ) ;
#35665 = B_SPLINE_CURVE_WITH_KNOTS ( 'NONE', 3,
 ( #68469, #51264, #14653, #24538 ),
 .UNSPECIFIED., .F., .F.,
 ( 4, 4 ),
 ( 0.1259919275528357530, 0.1829744153748744662 ),
 .UNSPECIFIED. ) ;
#35666 = CARTESIAN_POINT ( 'NONE',  ( -47.95193882091086834, 12.89180642785319186, 62.19750565756635297 ) ) ;
#35667 = ADVANCED_FACE ( 'NONE', ( #46260 ), #2331, .F. ) ;
#35668 = AXIS2_PLACEMENT_3D ( 'NONE', #60901, #65493, #7453 ) ;
#35669 = CARTESIAN_POINT ( 'NONE',  ( -98.25600799348289627, 30.78291175898263887, -89.85991034338427141 ) ) ;
#35670 = ADVANCED_FACE ( 'NONE', ( #24821 ), #40997, .T. ) ;
#35671 = ORIENTED_EDGE ( 'NONE', *, *, #50583, .F. ) ;
#35672 = VECTOR ( 'NONE', #6667, 1000.000000000000000 ) ;
#35673 = DIRECTION ( 'NONE',  ( -0.9909497617679331460, -0.1342332658176667304, 0.000000000000000000 ) ) ;
#35674 = CARTESIAN_POINT ( 'NONE',  ( -15.55634918610396866, 36.11269837220808654, 0.000000000000000000 ) ) ;
#35675 = CARTESIAN_POINT ( 'NONE',  ( -102.2801239173131194, 33.91021738430207932, -61.85912785543958847 ) ) ;
#35676 = DIRECTION ( 'NONE',  ( 1.387778780781445429E-16, -1.000000000000000000, -3.081487911019577365E-33 ) ) ;
#35677 = CARTESIAN_POINT ( 'NONE',  ( -26.07811460555694438, -76.21509903021816967, 133.5802547743875550 ) ) ;
#35678 = CARTESIAN_POINT ( 'NONE',  ( -15.55634918610400597, 20.55634918610405748, 85.00100000000000477 ) ) ;
#35679 = VECTOR ( 'NONE', #45900, 1000.000000000000000 ) ;
#35680 = VECTOR ( 'NONE', #16901, 1000.000000000000000 ) ;
#35681 = VERTEX_POINT ( 'NONE', #40301 ) ;
#35682 = FILL_AREA_STYLE_COLOUR ( '', #51633 ) ;
#35683 = CARTESIAN_POINT ( 'NONE',  ( 447.3372781065086201, 400.0000000000044338, 113.5502958579838122 ) ) ;
#35684 = ORIENTED_EDGE ( 'NONE', *, *, #62022, .T. ) ;
#35685 = VECTOR ( 'NONE', #68651, 1000.000000000000000 ) ;
#35686 = VERTEX_POINT ( 'NONE', #23781 ) ;
#35687 = DIRECTION ( 'NONE',  ( -0.8118923937861950435, -0.5838071093367415143, 0.000000000000000000 ) ) ;
#35688 = CARTESIAN_POINT ( 'NONE',  ( -178.2427210808090194, 93.01567669683346651, -74.54080329974289043 ) ) ;
#35689 = DIRECTION ( 'NONE',  ( 0.000000000000000000, 0.000000000000000000, -1.000000000000000000 ) ) ;
#35690 = EDGE_LOOP ( 'NONE', ( #40328, #39476, #14452, #61165 ) ) ;
#35691 = FACE_OUTER_BOUND ( 'NONE', #31126, .T. ) ;
#35692 = CARTESIAN_POINT ( 'NONE',  ( 32.02161712141799654, -16.09918303830818687, 0.000000000000000000 ) ) ;
#35693 = CARTESIAN_POINT ( 'NONE',  ( -5.885876544836658120, 6.772369038004114827, 3.521998547665712742 ) ) ;
#35694 = FACE_OUTER_BOUND ( 'NONE', #15553, .T. ) ;
#35695 = ADVANCED_FACE ( 'NONE', ( #35029 ), #60725, .T. ) ;
#35697 = EDGE_CURVE ( 'NONE', #18069, #11517, #2670, .T. ) ;
#35696 = CARTESIAN_POINT ( 'NONE',  ( -78.66644367742109978, 23.39876645725290061, 45.41820113967312977 ) ) ;
#35698 = CARTESIAN_POINT ( 'NONE',  ( 150.9203732286581783, 52.73242726514098422, 86.92778406629997789 ) ) ;
#35699 = CARTESIAN_POINT ( 'NONE',  ( -190.6985136298602015, 109.1272424661243434, 42.87371446347281534 ) ) ;
#35700 = ADVANCED_FACE ( 'NONE', ( #56475 ), #13913, .F. ) ;
#35701 = VERTEX_POINT ( 'NONE', #35728 ) ;
#35702 = CARTESIAN_POINT ( 'NONE',  ( -2.999999999999992450, 0.000000000000000000, -21.50000000000000000 ) ) ;
#35703 = CARTESIAN_POINT ( 'NONE',  ( 44.01696072965949469, 47.84694004974210912, 0.000000000000000000 ) ) ;
#35704 = CARTESIAN_POINT ( 'NONE',  ( -71.75757423844133598, 20.87429366976958889, 88.67075130327452825 ) ) ;
#35706 = ORIENTED_EDGE ( 'NONE', *, *, #52436, .T. ) ;
#35705 = CARTESIAN_POINT ( 'NONE',  ( 424.8372781065087906, 400.0000000000109139, 91.05029585798442326 ) ) ;
#35707 = FACE_OUTER_BOUND ( 'NONE', #41897, .T. ) ;
#35708 = ORIENTED_EDGE ( 'NONE', *, *, #11809, .T. ) ;
#35709 = VERTEX_POINT ( 'NONE', #67393 ) ;
#35710 = PLANE ( 'NONE',  #43578 ) ;
#35711 = CIRCLE ( 'NONE', #69382, 2.999999999999999112 ) ;
#35712 = CARTESIAN_POINT ( 'NONE',  ( -2.374459999240197572, -25.00999262126968148, 0.000000000000000000 ) ) ;
#35713 = CARTESIAN_POINT ( 'NONE',  ( 197.3685896092616190, 96.80423329231987850, -72.29383356998032184 ) ) ;
#35714 = PLANE ( 'NONE',  #38380 ) ;
#35715 = CARTESIAN_POINT ( 'NONE',  ( -119.2682179969168175, 42.28333404791698769, 68.51757058174662518 ) ) ;
#35716 = VECTOR ( 'NONE', #43936, 1000.000000000000000 ) ;
#35717 = CARTESIAN_POINT ( 'NONE',  ( 44.99999999999999289, -20.00000000000000355, 4.000000000000000000 ) ) ;
#35718 = CARTESIAN_POINT ( 'NONE',  ( 18.66025561752211459, 6.609375019058818523, -23.11559368035124251 ) ) ;
#35719 = CARTESIAN_POINT ( 'NONE',  ( -53.13788504024111603, 15.21566150156364472, 30.54986303373576462 ) ) ;
#35720 = VERTEX_POINT ( 'NONE', #57177 ) ;
#35721 = VERTEX_POINT ( 'NONE', #8298 ) ;
#35722 = VECTOR ( 'NONE', #18271, 1000.000000000000000 ) ;
#35723 = CARTESIAN_POINT ( 'NONE',  ( 2.905661822261151883E-14, 15.55634918610403084, 2.000000000000001776 ) ) ;
#35724 = CARTESIAN_POINT ( 'NONE',  ( 107.9301116202191650, 27.82606182274594175, 56.80549743259531681 ) ) ;
#35725 = CARTESIAN_POINT ( 'NONE',  ( -24.17157287525367693, 5.337719384915982763E-15, 2.000000000000001776 ) ) ;
#35726 = CARTESIAN_POINT ( 'NONE',  ( 14.66690460840507804, -20.39656099473392814, 0.000000000000000000 ) ) ;
#35727 = VECTOR ( 'NONE', #374, 1000.000000000000000 ) ;
#35728 = CARTESIAN_POINT ( 'NONE',  ( -28.32746765835526048, 69.45586423092609607, 133.5802547743875550 ) ) ;
#35729 = CARTESIAN_POINT ( 'NONE',  ( -31.11269837220809364, -10.55634918610397932, 2.000000000000001776 ) ) ;
#35730 = CARTESIAN_POINT ( 'NONE',  ( -142.0050623352988737, 59.34725908986624887, 91.61396122507353823 ) ) ;
#35731 = EDGE_LOOP ( 'NONE', ( #26495, #8823, #16512, #58515, #2427, #36975, #35517, #55410 ) ) ;
#35732 = ORIENTED_EDGE ( 'NONE', *, *, #51845, .T. ) ;
#35733 = ORIENTED_EDGE ( 'NONE', *, *, #15901, .T. ) ;
#35734 = AXIS2_PLACEMENT_3D ( 'NONE', #13069, #55263, #55615 ) ;
#35735 = EDGE_CURVE ( 'NONE', #36637, #58864, #12733, .T. ) ;
#35736 = SURFACE_STYLE_USAGE ( .BOTH. , #62807 ) ;
#35737 = CARTESIAN_POINT ( 'NONE',  ( -85.75947274862032543, 25.15128705015479582, 62.27437794546533212 ) ) ;
#35738 = CARTESIAN_POINT ( 'NONE',  ( 65.41496713438824884, 13.24164235279044100, -36.09838966426160312 ) ) ;
#35739 = FACE_OUTER_BOUND ( 'NONE', #59413, .T. ) ;
#35740 = CARTESIAN_POINT ( 'NONE',  ( -56.97556689808916985, 16.24958672959845529, 45.07069295579339752 ) ) ;
#35741 = CARTESIAN_POINT ( 'NONE',  ( -34.52542994698666945, 11.14027065218090762, -62.82190222610383046 ) ) ;
#35742 = CARTESIAN_POINT ( 'NONE',  ( 182.7745872728867766, 81.77554423487161728, 71.01052022670802444 ) ) ;
#35743 = CARTESIAN_POINT ( 'NONE',  ( 12.46704290855393005, 6.417105965824391411, -22.90343017382230428 ) ) ;
#35744 =( LENGTH_UNIT ( ) NAMED_UNIT ( * ) SI_UNIT ( .MILLI., .METRE. ) );
#35745 = ORIENTED_EDGE ( 'NONE', *, *, #47237, .F. ) ;
#35746 = CARTESIAN_POINT ( 'NONE',  ( -3.244108878396739559, 6.635632329121487594, -36.95954016693644206 ) ) ;
#35747 = CARTESIAN_POINT ( 'NONE',  ( 181.9406741394862195, 79.47484497224793643, 71.11619196314875069 ) ) ;
#35748 = CARTESIAN_POINT ( 'NONE',  ( -123.4416615615272548, 44.90042688650404301, 18.36697774316868959 ) ) ;
#35749 = CARTESIAN_POINT ( 'NONE',  ( 100.0000000000000284, 5.000000000000000000, 18.50000000000000000 ) ) ;
#35750 = FACE_OUTER_BOUND ( 'NONE', #69158, .T. ) ;
#35751 = EDGE_CURVE ( 'NONE', #35720, #20416, #47634, .T. ) ;
#35752 = CARTESIAN_POINT ( 'NONE',  ( 22.62427395637551086, 7.823784829753561709, -19.26947666278158877 ) ) ;
#35753 = CARTESIAN_POINT ( 'NONE',  ( 197.8436586345020487, 97.39326576892285914, 60.45424050539947558 ) ) ;
#35754 = EDGE_CURVE ( 'NONE', #8487, #60309, #42028, .T. ) ;
#35755 = EDGE_CURVE ( 'NONE', #15022, #20970, #41683, .T. ) ;
#35756 = VERTEX_POINT ( 'NONE', #47978 ) ;
#35757 = APPLICATION_PROTOCOL_DEFINITION ( 'draft international standard', 'automotive_design', 1998, #5772 ) ;
#35758 = CARTESIAN_POINT ( 'NONE',  ( 61.91366885787816443, -28.42865614898931881, 170.0000000000000000 ) ) ;
#35759 = PLANE ( 'NONE',  #21947 ) ;
#35760 = CARTESIAN_POINT ( 'NONE',  ( 0.4969600502617522730, -8.860760056385746708, -0.6527133886630286375 ) ) ;
#35761 = CARTESIAN_POINT ( 'NONE',  ( 63.01563776193091826, 12.67277567978498531, -50.72069083216976537 ) ) ;
#35762 = ORIENTED_EDGE ( 'NONE', *, *, #14208, .F. ) ;
#35763 = ORIENTED_EDGE ( 'NONE', *, *, #14979, .T. ) ;
#35764 = CARTESIAN_POINT ( 'NONE',  ( 0.000000000000000000, 0.000000000000000000, 85.00100000000000477 ) ) ;
#35765 = CARTESIAN_POINT ( 'NONE',  ( -86.05211524933166345, 25.27371147724188916, -95.00000000000133582 ) ) ;
#35766 = ORIENTED_EDGE ( 'NONE', *, *, #49054, .F. ) ;
#35767 = SHAPE_REPRESENTATION ( 'hex bolt gradeab_iso_ISO 4014 - M10 x 45 x 26-N', ( #66832 ), #28752 ) ;
#35768 = AXIS2_PLACEMENT_3D ( 'NONE', #46039, #31262, #67181 ) ;
#35769 = CARTESIAN_POINT ( 'NONE',  ( 164.8082524270398608, 64.90614020105162751, 89.03617402024222827 ) ) ;
#35770 = EDGE_LOOP ( 'NONE', ( #27412, #57218, #6489, #30952, #14148 ) ) ;
#35771 = CARTESIAN_POINT ( 'NONE',  ( 129.5225439633634323, 40.02995148249140556, -76.50699716606419543 ) ) ;
#35772 = CARTESIAN_POINT ( 'NONE',  ( 126.3737790127713083, 37.08609730334948296, 37.58129485337921949 ) ) ;
#35773 = VECTOR ( 'NONE', #61867, 1000.000000000000000 ) ;
#35774 = CARTESIAN_POINT ( 'NONE',  ( -156.8728827992624701, 72.05711009495561825, 36.77836446409524740 ) ) ;
#35775 = CARTESIAN_POINT ( 'NONE',  ( -96.78198318406111866, 30.07417864442865252, 32.89477166860936563 ) ) ;
#35776 = AXIS2_PLACEMENT_3D ( 'NONE', #40123, #61580, #55959 ) ;
#35777 = CARTESIAN_POINT ( 'NONE',  ( 8.000000000000007105, 249.8719672152120381, 94.99999999999866418 ) ) ;
#35779 = VERTEX_POINT ( 'NONE', #69445 ) ;
#35778 = CARTESIAN_POINT ( 'NONE',  ( -447.6627218934913230, 1.665334536937734811E-13, 83.55029585798817493 ) ) ;
#35780 = ADVANCED_FACE ( 'NONE', ( #58533 ), #46962, .F. ) ;
#35781 = LINE ( 'NONE', #57230, #58669 ) ;
#35782 = ORIENTED_EDGE ( 'NONE', *, *, #67937, .F. ) ;
#35783 = ORIENTED_EDGE ( 'NONE', *, *, #63831, .T. ) ;
#35784 = CARTESIAN_POINT ( 'NONE',  ( 173.7225111622554437, 72.84868911716897344, 38.27220697509852698 ) ) ;
#35785 = CARTESIAN_POINT ( 'NONE',  ( 18.19980344696536534, 6.589834367837007711, -76.96946507082562050 ) ) ;
#35787 = ORIENTED_EDGE ( 'NONE', *, *, #19720, .F. ) ;
#35786 = DIRECTION ( 'NONE',  ( 0.000000000000000000, 0.000000000000000000, -1.000000000000000000 ) ) ;
#35788 = CARTESIAN_POINT ( 'NONE',  ( -173.1211646369891355, 88.63826465341151106, -49.71195716475001092 ) ) ;
#35789 = FACE_OUTER_BOUND ( 'NONE', #38297, .T. ) ;
#35790 = ORIENTED_EDGE ( 'NONE', *, *, #19872, .F. ) ;
#35791 = CARTESIAN_POINT ( 'NONE',  ( -62.30463872474475551, 16.74658165105248386, -17.84944043806595815 ) ) ;
#35792 = B_SPLINE_CURVE_WITH_KNOTS ( 'NONE', 3,
 ( #66736, #61092, #2016, #28737, #12918, #2699, #39981, #50878, #7974, #18530, #44566, #12557, #61440, #34719, #23113, #23811, #61771, #34373, #56156, #66043, #66394, #29428, #24161, #45603, #12210, #55820, #17836, #39635, #2358, #7641, #45252, #67088, #18877, #39293, #29091, #60737, #40325, #33677 ),
 .UNSPECIFIED., .F., .F.,
 ( 4, 2, 2, 2, 2, 2, 2, 2, 2, 2, 2, 2, 2, 2, 2, 2, 2, 2, 4 ),
 ( 0.02546424207107601811, 0.02703543426729208832, 0.02782103036540015811, 0.02860662646350822791, 0.03017781865972443342, 0.03174901085594063893, 0.03332020305215684791, 0.03489139524837305689, 0.03646258744458925893, 0.03724818354269734955, 0.03803377964080544016, 0.03881937573891353077, 0.03960497183702162138, 0.04117616403323780261, 0.04274735622945398383, 0.04431854842567016506, 0.04588974062188634628, 0.04746093281810252751, 0.05060331721053488302 ),
 .UNSPECIFIED. ) ;
#35793 = CARTESIAN_POINT ( 'NONE',  ( 136.9822423813093053, 44.53121110416871176, 30.18860586589651618 ) ) ;
#35794 = CARTESIAN_POINT ( 'NONE',  ( 86.62931800182293784, -170.0000000000000000, -70.16611478937539914 ) ) ;
#35795 = CARTESIAN_POINT ( 'NONE',  ( -101.8191498210054675, 32.54686850610962523, 3.674523915951419362 ) ) ;
#35796 = CARTESIAN_POINT ( 'NONE',  ( 67.54641595172913071, 14.80690682047550943, -64.06872420909932941 ) ) ;
#35797 = EDGE_LOOP ( 'NONE', ( #3582, #4963, #61848, #2983, #41604, #40384, #61094 ) ) ;
#35798 = ORIENTED_EDGE ( 'NONE', *, *, #63761, .T. ) ;
#35799 = CARTESIAN_POINT ( 'NONE',  ( 8.485361335568063268, 7.382900357301075189, -95.00000000000133582 ) ) ;
#35800 = DIRECTION ( 'NONE',  ( 0.6234898018587431423, -0.7818314824680220321, 0.000000000000000000 ) ) ;
#35801 = LINE ( 'NONE', #3780, #51991 ) ;
#35802 = PRODUCT_RELATED_PRODUCT_CATEGORY ( 'part', '', ( #36615 ) ) ;
#35803 = FACE_OUTER_BOUND ( 'NONE', #67490, .T. ) ;
#35804 = DIRECTION ( 'NONE',  ( 1.000000000000000000, 0.000000000000000000, -0.000000000000000000 ) ) ;
#35805 = DIRECTION ( 'NONE',  ( -0.000000000000000000, -1.000000000000000000, -0.000000000000000000 ) ) ;
#35806 = CARTESIAN_POINT ( 'NONE',  ( 69.48877314113907744, 15.30784187978995092, -39.42461950060443598 ) ) ;
#35807 = CARTESIAN_POINT ( 'NONE',  ( -447.6627218934916073, 370.0000000000085265, 108.5502958579925377 ) ) ;
#35808 = CARTESIAN_POINT ( 'NONE',  ( 205.0999694062793424, 106.8955893716604777, 56.05227132923311473 ) ) ;
#35810 = ORIENTED_EDGE ( 'NONE', *, *, #61959, .F. ) ;
#35809 = EDGE_CURVE ( 'NONE', #8769, #32122, #42710, .T. ) ;
#35811 = FACE_OUTER_BOUND ( 'NONE', #8760, .T. ) ;
#35812 = VERTEX_POINT ( 'NONE', #20226 ) ;
#35813 = CARTESIAN_POINT ( 'NONE',  ( -175.0671597231267924, 89.32002174371487513, -88.64685081530532784 ) ) ;
#35814 = EDGE_CURVE ( 'NONE', #14487, #34211, #25864, .T. ) ;
#35815 = CARTESIAN_POINT ( 'NONE',  ( 25.02868014889590498, -33.38981655027261297, 13.79046340968177731 ) ) ;
#35816 = ORIENTED_EDGE ( 'NONE', *, *, #48500, .T. ) ;
#35817 = CARTESIAN_POINT ( 'NONE',  ( -81.57257563421755719, 23.44953612320489711, -89.37733141453014696 ) ) ;
#35818 = CARTESIAN_POINT ( 'NONE',  ( -190.6985136298601731, 109.1272424661242582, 94.99999999999866418 ) ) ;
#35819 = CARTESIAN_POINT ( 'NONE',  ( 447.3372781065085633, 400.0000000000000568, -146.4497041420118251 ) ) ;
#35820 = VECTOR ( 'NONE', #44844, 1000.000000000000000 ) ;
#35821 = CARTESIAN_POINT ( 'NONE',  ( 35.65775178405254309, 7.951994368745593178, 4.066108867012141914 ) ) ;
#35822 = CARTESIAN_POINT ( 'NONE',  ( -11.14668121284976721, 8.139398342256733088, -36.18907776356625305 ) ) ;
#35823 = CARTESIAN_POINT ( 'NONE',  ( 209.9999999999999716, -2.000000000000001776, 72.99999999999998579 ) ) ;
#35824 = VECTOR ( 'NONE', #2231, 1000.000000000000000 ) ;
#35825 = ORIENTED_EDGE ( 'NONE', *, *, #22784, .T. ) ;
#35826 = CARTESIAN_POINT ( 'NONE',  ( -119.9488317262643875, 43.88555072835348625, -91.50783509519961001 ) ) ;
#35827 = ORIENTED_EDGE ( 'NONE', *, *, #5572, .F. ) ;
#35828 = CARTESIAN_POINT ( 'NONE',  ( 311.8713128290285113, 2.000000000000001776, -151.4173447659616443 ) ) ;
#35829 = CARTESIAN_POINT ( 'NONE',  ( -57.89360529881253825, 16.50663720601370343, 71.61556157776966813 ) ) ;
#35830 = DIRECTION ( 'NONE',  ( 2.220446049250313081E-16, -0.000000000000000000, 1.000000000000000000 ) ) ;
#35831 = CARTESIAN_POINT ( 'NONE',  ( -452.6627218934913230, 217.8591479523843475, -111.4497041420117966 ) ) ;
#35832 = CARTESIAN_POINT ( 'NONE',  ( -60.86068608946850844, 16.31596860244180291, -91.65520414832201368 ) ) ;
#35833 = CARTESIAN_POINT ( 'NONE',  ( -99.98930671699734773, 31.63190627461931470, -22.82702748219488242 ) ) ;
#35834 = CARTESIAN_POINT ( 'NONE',  ( 150.4542242713869484, 53.63744268572192198, -40.96015938328587680 ) ) ;
#35835 = EDGE_CURVE ( 'NONE', #25430, #48110, #44615, .T. ) ;
#35836 = ADVANCED_FACE ( 'NONE', ( #5431, #21601, #37094, #20564, #63488 ), #10024, .T. ) ;
#35837 = ORIENTED_EDGE ( 'NONE', *, *, #63523, .F. ) ;
#35838 = DIRECTION ( 'NONE',  ( 9.801828090421496776E-15, -3.870007156971564233E-15, 0.9999999999999998890 ) ) ;
#35839 = CARTESIAN_POINT ( 'NONE',  ( -149.7268278745402199, 65.68859631971237434, 57.56537183036276417 ) ) ;
#35840 = CARTESIAN_POINT ( 'NONE',  ( 174.1348882614951208, 73.23561817543357222, -14.04505384645303856 ) ) ;
#35841 = CARTESIAN_POINT ( 'NONE',  ( -118.4553071845214731, 41.78724769484929880, 37.02199087950304346 ) ) ;
#35842 = DIRECTION ( 'NONE',  ( -1.000000000000000000, 0.000000000000000000, 0.000000000000000000 ) ) ;
#35843 = ORIENTED_EDGE ( 'NONE', *, *, #7048, .F. ) ;
#35844 = CARTESIAN_POINT ( 'NONE',  ( -180.2188652555596491, 96.98354576637422042, -71.49711507050399462 ) ) ;
#35845 = CARTESIAN_POINT ( 'NONE',  ( 136.0649627081555195, 43.95772869497660906, 83.52517116066933056 ) ) ;
#35846 = CARTESIAN_POINT ( 'NONE',  ( 204.6977192012829505, 108.0580384837234931, -24.48138044215792419 ) ) ;
#35847 = CARTESIAN_POINT ( 'NONE',  ( -21.78980970457817179, 70.00000000000000000, 33.04664611826583354 ) ) ;
#35848 = CARTESIAN_POINT ( 'NONE',  ( 99.99999999999997158, 0.000000000000000000, -3.000000000000030198 ) ) ;
#35849 = EDGE_LOOP ( 'NONE', ( #15499, #60478, #9816, #26241 ) ) ;
#35850 = DIRECTION ( 'NONE',  ( -0.000000000000000000, -0.000000000000000000, 1.000000000000000000 ) ) ;
#35851 = CARTESIAN_POINT ( 'NONE',  ( 112.1012908502484748, 29.75117929736502020, -77.53697030799570200 ) ) ;
#35852 = CARTESIAN_POINT ( 'NONE',  ( 188.5838389098763344, 88.03667982118679447, 37.11779938872467000 ) ) ;
#35853 = CARTESIAN_POINT ( 'NONE',  ( 183.8564736226039713, 81.45095818237477658, -90.40950570902288064 ) ) ;
#35854 = LINE ( 'NONE', #2806, #48753 ) ;
#35855 = AXIS2_PLACEMENT_3D ( 'NONE', #31891, #13810, #60356 ) ;
#35856 = VERTEX_POINT ( 'NONE', #52910 ) ;
#35857 = CARTESIAN_POINT ( 'NONE',  ( 164.4761273435911733, 64.62485394454741083, -19.50930807920846632 ) ) ;
#35858 = ORIENTED_EDGE ( 'NONE', *, *, #59531, .T. ) ;
#35859 = CARTESIAN_POINT ( 'NONE',  ( 66.94365390260638549, 14.65531706601758977, 57.76378685776548849 ) ) ;
#35860 = CARTESIAN_POINT ( 'NONE',  ( 141.2963039856138039, 46.10182040858772723, 89.73232225052716160 ) ) ;
#35861 = VECTOR ( 'NONE', #16388, 1000.000000000000000 ) ;
#35863 = EDGE_LOOP ( 'NONE', ( #14176, #44490, #65810, #22006 ) ) ;
#35862 = LINE ( 'NONE', #68884, #28654 ) ;
#35864 = CARTESIAN_POINT ( 'NONE',  ( 161.1112535418156710, 61.83422628788724751, -37.06319131123839128 ) ) ;
#35865 = CARTESIAN_POINT ( 'NONE',  ( 544.6745185807129701, 0.000000000000000000, 34.73878747406611467 ) ) ;
#35866 = AXIS2_PLACEMENT_3D ( 'NONE', #7294, #2368, #43862 ) ;
#35867 = DIRECTION ( 'NONE',  ( 7.703719777548945123E-34, 1.479221584281240009E-31, -1.000000000000000000 ) ) ;
#35868 = ORIENTED_EDGE ( 'NONE', *, *, #27312, .F. ) ;
#35869 = CARTESIAN_POINT ( 'NONE',  ( -94.77890319529974761, 30.24118571794803501, 10.67444691552502256 ) ) ;
#35870 = CARTESIAN_POINT ( 'NONE',  ( -131.7724154034330581, 50.48821165954357326, 42.78414996048509522 ) ) ;
#35871 = CARTESIAN_POINT ( 'NONE',  ( 153.9458454029195877, 56.21976558811522295, -90.68237876674034226 ) ) ;
#35872 = CARTESIAN_POINT ( 'NONE',  ( 82.73618382051371611, 19.18661415186667440, -10.06194520202119591 ) ) ;
#35873 = CARTESIAN_POINT ( 'NONE',  ( -166.5704851812740515, 80.12110537694670143, 34.65906088291280440 ) ) ;
#35874 = CARTESIAN_POINT ( 'NONE',  ( 63.01563776193091826, 13.70579113808094895, 29.81296093922127710 ) ) ;
#35875 = CARTESIAN_POINT ( 'NONE',  ( 210.6189312023034574, -170.0000000000000000, 94.99999999999866418 ) ) ;
#35876 = ORIENTED_EDGE ( 'NONE', *, *, #65850, .T. ) ;
#35877 = CARTESIAN_POINT ( 'NONE',  ( 181.0840389613909736, 78.60582251573003987, 29.30859410551139277 ) ) ;
#35878 = CARTESIAN_POINT ( 'NONE',  ( 150.3360255159550150, 52.31024849487489803, -95.00000000000133582 ) ) ;
#35879 = EDGE_LOOP ( 'NONE', ( #1770, #16887, #27927, #59793 ) ) ;
#35880 = CIRCLE ( 'NONE', #38122, 72.99999999999998579 ) ;
#35881 = LINE ( 'NONE', #63308, #42924 ) ;
#35882 = EDGE_CURVE ( 'NONE', #54393, #26798, #64804, .T. ) ;
#35883 = CARTESIAN_POINT ( 'NONE',  ( 212.1976655298228991, 119.0878071902807704, -17.15924209720097693 ) ) ;
#35884 = CARTESIAN_POINT ( 'NONE',  ( 106.4072861358878441, 28.24787347451998443, 43.56070440894875873 ) ) ;
#35885 = DIRECTION ( 'NONE',  ( 1.000000000000000000, -0.000000000000000000, -0.000000000000000000 ) ) ;
#35886 = CARTESIAN_POINT ( 'NONE',  ( -25.00000000000028066, -65.13282190615278466, -9.999999999999998224 ) ) ;
#35887 = CARTESIAN_POINT ( 'NONE',  ( 188.4918087359956473, 87.93403732562656216, 8.752912527378605034 ) ) ;
#35888 = CARTESIAN_POINT ( 'NONE',  ( 211.7451286015361518, 116.5372661580811666, -41.24269329785643379 ) ) ;
#35889 = EDGE_CURVE ( 'NONE', #68707, #38702, #43047, .T. ) ;
#35890 = DIRECTION ( 'NONE',  ( -0.000000000000000000, 1.000000000000000000, -0.000000000000000000 ) ) ;
#35891 = ORIENTED_EDGE ( 'NONE', *, *, #64793, .F. ) ;
#35892 = PLANE ( 'NONE',  #11601 ) ;
#35894 = VERTEX_POINT ( 'NONE', #65936 ) ;
#35893 = EDGE_CURVE ( 'NONE', #1254, #66403, #59567, .T. ) ;
#35895 = CARTESIAN_POINT ( 'NONE',  ( 106.4107271020439782, 27.14892220304137993, -76.71846769895172713 ) ) ;
#35896 = APPLICATION_CONTEXT ( 'automotive_design' ) ;
#35897 = CARTESIAN_POINT ( 'NONE',  ( 41.80869235728138733, 9.750404582811606602, -23.39550270451861635 ) ) ;
#35898 = PLANE ( 'NONE',  #61941 ) ;
#35899 = CARTESIAN_POINT ( 'NONE',  ( -64.18058723658653264, 10.37664328995176888, 170.0000000000000000 ) ) ;
#35900 = ADVANCED_FACE ( 'NONE', ( #44810 ), #32508, .T. ) ;
#35901 = CARTESIAN_POINT ( 'NONE',  ( 412.3372781065082791, 400.0000000000040927, 78.55029585798418168 ) ) ;
#35902 = AXIS2_PLACEMENT_3D ( 'NONE', #40543, #3606, #49436 ) ;
#35903 = CARTESIAN_POINT ( 'NONE',  ( -109.7686203588201579, 37.90089348911613598, -15.17831855726085521 ) ) ;
#35904 = VERTEX_POINT ( 'NONE', #50081 ) ;
#35905 = CARTESIAN_POINT ( 'NONE',  ( -71.43874587651176000, 19.69883891272895937, 62.74430205168221875 ) ) ;
#35906 = CARTESIAN_POINT ( 'NONE',  ( -167.1540252468941503, 80.72321878831101571, 60.61552501969690354 ) ) ;
#35907 = ORIENTED_EDGE ( 'NONE', *, *, #13682, .T. ) ;
#35908 = VERTEX_POINT ( 'NONE', #33571 ) ;
#35909 = CARTESIAN_POINT ( 'NONE',  ( -156.1462053606562677, 70.02140399657017156, 41.72074378258265881 ) ) ;
#35910 = DIRECTION ( 'NONE',  ( -0.8090169943749422332, -0.5877852522924802425, 0.000000000000000000 ) ) ;
#35911 = B_SPLINE_CURVE_WITH_KNOTS ( 'NONE', 3,
 ( #47564, #59501, #5694, #63422, #26475, #42646, #11315, #15913, #69020, #10280, #52511, #4338, #27152, #5361, #31745, #21874, #16599, #53182, #75, #48583 ),
 .UNSPECIFIED., .F., .F.,
 ( 4, 2, 2, 2, 2, 2, 2, 2, 2, 4 ),
 ( 0.009941967776246129346, 0.01118871530018490136, 0.01243546282412367338, 0.01305883658609307066, 0.01368221034806246968, 0.01492895787200121047, 0.01617570539593995299, 0.01742245291987869205, 0.01866920044381743110, 0.01991594796775617363 ),
 .UNSPECIFIED. ) ;
#35912 = CARTESIAN_POINT ( 'NONE',  ( 175.5493994043409316, 73.18740965572600032, -11.81303265696679183 ) ) ;
#35913 = PRESENTATION_STYLE_ASSIGNMENT (( #68605 ) ) ;
#35914 = LINE ( 'NONE', #18698, #33000 ) ;
#35915 = EDGE_CURVE ( 'NONE', #13533, #19369, #66287, .T. ) ;
#35916 = VECTOR ( 'NONE', #51099, 1000.000000000000000 ) ;
#35917 = ORIENTED_EDGE ( 'NONE', *, *, #46850, .T. ) ;
#35918 =( GEOMETRIC_REPRESENTATION_CONTEXT ( 3 ) GLOBAL_UNCERTAINTY_ASSIGNED_CONTEXT ( ( #13504 ) ) GLOBAL_UNIT_ASSIGNED_CONTEXT ( ( #30058, #36016, #24440 ) ) REPRESENTATION_CONTEXT ( 'NONE', 'WORKASPACE' ) );
#35919 = LINE ( 'NONE', #57369, #33412 ) ;
#35920 = ORIENTED_EDGE ( 'NONE', *, *, #55101, .F. ) ;
#35921 = CARTESIAN_POINT ( 'NONE',  ( 212.0047492081760083, 116.9348962082588343, 8.142182148364424776 ) ) ;
#35922 = CARTESIAN_POINT ( 'NONE',  ( -148.6426892915312123, 64.76241938621078020, 45.72082123989908098 ) ) ;
#35923 = CARTESIAN_POINT ( 'NONE',  ( 210.4897348480408539, 114.6382060222044714, 31.93660676264083165 ) ) ;
#35924 = FACE_BOUND ( 'NONE', #59442, .T. ) ;
#35925 = ORIENTED_EDGE ( 'NONE', *, *, #11540, .T. ) ;
#35926 = ORIENTED_EDGE ( 'NONE', *, *, #788, .F. ) ;
#35927 = CARTESIAN_POINT ( 'NONE',  ( 410.0000000000000000, 0.000000000000000000, 380.0000000000000000 ) ) ;
#35928 = CARTESIAN_POINT ( 'NONE',  ( -118.7786458613889806, 43.16353039193077734, 89.41427216433091019 ) ) ;
#35929 = CARTESIAN_POINT ( 'NONE',  ( -165.7143741370936993, 79.24519349471958662, -16.58517908087970838 ) ) ;
#35930 = LINE ( 'NONE', #67599, #26478 ) ;
#35931 = CARTESIAN_POINT ( 'NONE',  ( 23.17475323415827404, 6.849528528214888112, 92.54444823000328313 ) ) ;
#35932 = CIRCLE ( 'NONE', #23581, 65.36598343705435354 ) ;
#35933 = CARTESIAN_POINT ( 'NONE',  ( 86.62931800182293784, 19.42108912189596381, -77.66611478937542756 ) ) ;
#35934 = ORIENTED_EDGE ( 'NONE', *, *, #20198, .T. ) ;
#35935 = CYLINDRICAL_SURFACE ( 'NONE', #20195, 7.500000000000020428 ) ;
#35936 = CARTESIAN_POINT ( 'NONE',  ( -99.97541017369792371, 31.62502926470686759, 72.01622551138805761 ) ) ;
#35937 = ORIENTED_EDGE ( 'NONE', *, *, #25747, .T. ) ;
#35938 = CARTESIAN_POINT ( 'NONE',  ( -85.45399718454960691, 25.02415453493131281, 14.27398530813207245 ) ) ;
#35939 = ORIENTED_EDGE ( 'NONE', *, *, #58675, .F. ) ;
#35940 = CARTESIAN_POINT ( 'NONE',  ( 46.66904755831212981, 20.55634918610394379, 0.000000000000000000 ) ) ;
#35941 = ORIENTED_EDGE ( 'NONE', *, *, #8041, .T. ) ;
#35942 = EDGE_LOOP ( 'NONE', ( #54693, #12245, #50580, #48959 ) ) ;
#35943 = CARTESIAN_POINT ( 'NONE',  ( 43.96421756700840433, 10.06386361114659778, 58.28564946010243375 ) ) ;
#35944 = VECTOR ( 'NONE', #7534, 1000.000000000000000 ) ;
#35945 = CARTESIAN_POINT ( 'NONE',  ( -106.6624114166473305, 36.20432260969276683, -90.10160425761682745 ) ) ;
#35946 = CARTESIAN_POINT ( 'NONE',  ( 105.7953515382196628, 27.97683113100024244, 16.32495411353482595 ) ) ;
#35947 = ORIENTED_EDGE ( 'NONE', *, *, #28030, .T. ) ;
#35948 = EDGE_CURVE ( 'NONE', #11952, #24193, #54994, .T. ) ;
#35949 = CARTESIAN_POINT ( 'NONE',  ( -24.07560883032475729, 8.498111648314747413, 92.86635853022728782 ) ) ;
#35950 = CARTESIAN_POINT ( 'NONE',  ( 173.9405361758639117, 73.05302209498820787, -68.26724894106142472 ) ) ;
#35951 = LINE ( 'NONE', #31029, #7843 ) ;
#35952 = CARTESIAN_POINT ( 'NONE',  ( 110.2429982417149290, 28.88204397445231209, -50.92243756565370916 ) ) ;
#35953 = CARTESIAN_POINT ( 'NONE',  ( -7.486743542469089796, -64.58150799671139453, 43.58025477438756923 ) ) ;
#35954 = LINE ( 'NONE', #57406, #33269 ) ;
#35955 = ORIENTED_EDGE ( 'NONE', *, *, #45120, .F. ) ;
#35956 = B_SPLINE_CURVE_WITH_KNOTS ( 'NONE', 3,
 ( #28497, #60503, #45014, #55929, #50305, #12667, #44315, #12319, #60847, #49940, #34132, #40096, #1771, #13367, #56264, #65799, #29195, #23235, #7746, #44679, #8080, #66155, #17947, #2463, #28854, #2122, #23574, #18288, #5502, #54368, #48057, #26955, #6196, #37862, #5160, #32928, #22029, #43817, #927, #54726, #10428, #16746, #38204 ),
 .UNSPECIFIED., .F., .F.,
 ( 4, 2, 2, 2, 2, 2, 2, 2, 1, 2, 2, 2, 2, 2, 2, 2, 2, 2, 2, 2, 2, 4 ),
 ( 0.000000000000000000, 0.001465684626643319350, 0.002198526939964978808, 0.002931369253286638700, 0.004397053879929970627, 0.005862738506573303421, 0.007328423133216635348, 0.008061265446538309551, 0.008794107759859986356, 0.009526950073181661427, 0.01025979238650333650, 0.01172547701314670572, 0.01319116163979007321, 0.01465684626643344417, 0.01538968857975512618, 0.01612253089307680992, 0.01758821551972015659, 0.01905390014636350327, 0.01978674245968517140, 0.02051958477300683606, 0.02198526939965016885, 0.02345095402629350512 ),
 .UNSPECIFIED. ) ;
#35957 = AXIS2_PLACEMENT_3D ( 'NONE', #31351, #20432, #10222 ) ;
#35958 = ORIENTED_EDGE ( 'NONE', *, *, #30497, .F. ) ;
#35959 = CARTESIAN_POINT ( 'NONE',  ( 50.97490815085634352, 6.000000000000000000, -41.68900338898716740 ) ) ;
#35960 = CARTESIAN_POINT ( 'NONE',  ( -85.96384504792887071, 26.32782846176032976, -67.71012703438472613 ) ) ;
#35961 = CARTESIAN_POINT ( 'NONE',  ( 175.0634607207819045, 74.11351956991636314, 14.44380243719841594 ) ) ;
#35962 = DIRECTION ( 'NONE',  ( -1.387778780781445429E-16, 1.000000000000000000, 3.081487911019577365E-33 ) ) ;
#35963 = CARTESIAN_POINT ( 'NONE',  ( -102.2801239173131052, 32.78103895658057354, -88.70367844590326456 ) ) ;
#35964 = CARTESIAN_POINT ( 'NONE',  ( 127.2397149628677369, 37.56999625068102233, 13.73394111055298339 ) ) ;
#35965 = CARTESIAN_POINT ( 'NONE',  ( 32.69830313199977212, 7.632043626524796842, -93.43925476920368567 ) ) ;
#35966 = CARTESIAN_POINT ( 'NONE',  ( -124.1095621208148572, 46.52671329146387080, -61.91586655676568540 ) ) ;
#35967 = EDGE_CURVE ( 'NONE', #14985, #22952, #65216, .T. ) ;
#35968 = CARTESIAN_POINT ( 'NONE',  ( 205.5049354810107332, 109.1776577097391510, 29.20772073876942088 ) ) ;
#35969 = LINE ( 'NONE', #67641, #46762 ) ;
#35970 = CARTESIAN_POINT ( 'NONE',  ( -108.9452487746634120, 36.29752968355630571, 34.54237325803290304 ) ) ;
#35971 = ORIENTED_EDGE ( 'NONE', *, *, #55401, .F. ) ;
#35972 = CARTESIAN_POINT ( 'NONE',  ( 15.29912143387263690, 7.491799981865496783, -23.67439350822212774 ) ) ;
#35973 = VERTEX_POINT ( 'NONE', #22648 ) ;
#35974 = DIRECTION ( 'NONE',  ( 0.000000000000000000, 0.000000000000000000, -1.000000000000000000 ) ) ;
#35975 = B_SPLINE_CURVE_WITH_KNOTS ( 'NONE', 3,
 ( #35799, #56910, #51630, #57598, #9410, #30177, #30514, #39091, #44341, #8379 ),
 .UNSPECIFIED., .F., .F.,
 ( 4, 2, 2, 2, 4 ),
 ( 0.000000000000000000, 0.002502989122560414677, 0.005005978245120829354, 0.007508967367681244030, 0.01001195649024165871 ),
 .UNSPECIFIED. ) ;
#35976 = ORIENTED_EDGE ( 'NONE', *, *, #3964, .F. ) ;
#35977 = CARTESIAN_POINT ( 'NONE',  ( -149.5074843970971017, 65.50121172469319220, 3.876270649435370252 ) ) ;
#35978 = FACE_OUTER_BOUND ( 'NONE', #52116, .T. ) ;
#35979 = LINE ( 'NONE', #46878, #4293 ) ;
#35980 = EDGE_CURVE ( 'NONE', #6273, #47103, #6815, .T. ) ;
#35981 = DIRECTION ( 'NONE',  ( 1.000000000000000000, 0.000000000000000000, 0.000000000000000000 ) ) ;
#35982 = AXIS2_PLACEMENT_3D ( 'NONE', #13997, #40380, #3443 ) ;
#35983 = CARTESIAN_POINT ( 'NONE',  ( 139.2794027252094224, 45.99190465195510313, -38.31979582468038359 ) ) ;
#35984 = CARTESIAN_POINT ( 'NONE',  ( 32.67604581760323867, 7.629767527669977234, -39.79224508708363572 ) ) ;
#35985 = CARTESIAN_POINT ( 'NONE',  ( 203.9150235420940476, 105.2750102756484978, 82.91810571397343210 ) ) ;
#35986 = CARTESIAN_POINT ( 'NONE',  ( 13.37708032728285268, 7.441924986912761497, -50.12502757588696767 ) ) ;
#35987 = CARTESIAN_POINT ( 'NONE',  ( 126.8237978310704506, 37.33705012421152958, -40.90458718104599001 ) ) ;
#35988 = ORIENTED_EDGE ( 'NONE', *, *, #50811, .T. ) ;
#35989 = ORIENTED_EDGE ( 'NONE', *, *, #22790, .F. ) ;
#35990 = DIRECTION ( 'NONE',  ( 0.000000000000000000, -1.000000000000000000, 0.000000000000000000 ) ) ;
#35991 = FILL_AREA_STYLE ('',( #14534 ) ) ;
#35992 = CARTESIAN_POINT ( 'NONE',  ( -23.93965512371324422, 8.480096402797089539, -70.16679352128214475 ) ) ;
#35993 = EDGE_CURVE ( 'NONE', #57471, #988, #44087, .T. ) ;
#35994 = UNCERTAINTY_MEASURE_WITH_UNIT (LENGTH_MEASURE( 1.000000000000000082E-05 ), #33878, 'distance_accuracy_value', 'NONE');
#35995 = AXIS2_PLACEMENT_3D ( 'NONE', #8299, #20565, #8995 ) ;
#35996 = EDGE_CURVE ( 'NONE', #1913, #65404, #17733, .T. ) ;
#35997 = CARTESIAN_POINT ( 'NONE',  ( 8.683531412707425901, 6.377173148747123044, 13.08527713931978198 ) ) ;
#35998 = ADVANCED_FACE ( 'NONE', ( #38125 ), #17362, .F. ) ;
#35999 = CARTESIAN_POINT ( 'NONE',  ( -56.92000000000000171, 0.000000000000000000, 30.00000000000000000 ) ) ;
#36000 = ORIENTED_EDGE ( 'NONE', *, *, #28263, .F. ) ;
#36001 = DIRECTION ( 'NONE',  ( -0.000000000000000000, -0.000000000000000000, -1.000000000000000000 ) ) ;
#36002 = CARTESIAN_POINT ( 'NONE',  ( 179.4279766878530040, 76.94722012158230484, -77.89655909951385127 ) ) ;
#36003 = CARTESIAN_POINT ( 'NONE',  ( 0.4969600502617602111, -8.860760056385760919, -0.6527133886630297477 ) ) ;
#36004 = CARTESIAN_POINT ( 'NONE',  ( 9.850262805259839993, 188.0000000000000000, -1.724042536399416070 ) ) ;
#36005 = CARTESIAN_POINT ( 'NONE',  ( -28.35957743809533937, 10.12373109553626804, 57.71800868584409017 ) ) ;
#36006 = DIRECTION ( 'NONE',  ( 0.000000000000000000, 0.000000000000000000, 1.000000000000000000 ) ) ;
#36007 = CARTESIAN_POINT ( 'NONE',  ( -47.60396279792517760, 12.80997843568595052, 63.65564769673237322 ) ) ;
#36008 = EDGE_LOOP ( 'NONE', ( #25362, #60971, #48852, #10886 ) ) ;
#36009 = CARTESIAN_POINT ( 'NONE',  ( 444.9999999999999432, 225.0000000000000000, 378.0000000000000000 ) ) ;
#36010 = CARTESIAN_POINT ( 'NONE',  ( 150.5744176759382640, 53.72473166688032364, 60.79328936379504000 ) ) ;
#36011 = CARTESIAN_POINT ( 'NONE',  ( -109.6657532478350845, 37.84376708859253569, -70.68994547012663077 ) ) ;
#36012 = CARTESIAN_POINT ( 'NONE',  ( -422.6627218934918915, 395.0000000000064801, -116.4497041420121377 ) ) ;
#36013 = CARTESIAN_POINT ( 'NONE',  ( -102.2801239173131194, 32.78103895658057354, -35.01457726497591239 ) ) ;
#36014 = DIRECTION ( 'NONE',  ( 1.000000000000000000, 0.000000000000000000, -0.000000000000000000 ) ) ;
#36015 = VERTEX_POINT ( 'NONE', #1541 ) ;
#36016 =( NAMED_UNIT ( * ) PLANE_ANGLE_UNIT ( ) SI_UNIT ( $, .RADIAN. ) );
#36017 = DIRECTION ( 'NONE',  ( 0.000000000000000000, -0.000000000000000000, -1.000000000000000000 ) ) ;
#36018 = ORIENTED_EDGE ( 'NONE', *, *, #15097, .F. ) ;
#36019 = ORIENTED_EDGE ( 'NONE', *, *, #57827, .F. ) ;
#36020 = DIRECTION ( 'NONE',  ( 1.000000000000000000, 0.000000000000000000, -0.000000000000000000 ) ) ;
#36021 = CARTESIAN_POINT ( 'NONE',  ( -180.2244609727084992, 95.39945930389644957, -71.48059130514354820 ) ) ;
#36022 = DIRECTION ( 'NONE',  ( 0.8345732537212999791, 0.5508969814521065267, 0.000000000000000000 ) ) ;
#36023 = ORIENTED_EDGE ( 'NONE', *, *, #14986, .T. ) ;
#36024 = CYLINDRICAL_SURFACE ( 'NONE', #14736, 5.000000000000004441 ) ;
#36025 = DIRECTION ( 'NONE',  ( 0.000000000000000000, -0.000000000000000000, 1.000000000000000000 ) ) ;
#36026 = FACE_OUTER_BOUND ( 'NONE', #39949, .T. ) ;
#36027 = CIRCLE ( 'NONE', #15831, 4.999999999999997335 ) ;
#36028 = CARTESIAN_POINT ( 'NONE',  ( -46.06722295615723795, -46.37372919877118704, 6.377659838150142862E-18 ) ) ;
#36029 = CARTESIAN_POINT ( 'NONE',  ( 6.564829507346455983, -24.24955267099640110, 0.000000000000000000 ) ) ;
#36030 = CARTESIAN_POINT ( 'NONE',  ( -24.18270484670772902, 9.527492911955588895, -14.01251953149264473 ) ) ;
#36031 = CARTESIAN_POINT ( 'NONE',  ( 141.3445468829084746, 46.13338528906588465, 10.66957849498047928 ) ) ;
#36032 = AXIS2_PLACEMENT_3D ( 'NONE', #29786, #8342, #25217 ) ;
#36033 = EDGE_CURVE ( 'NONE', #16881, #68798, #496, .T. ) ;
#36034 = PRODUCT ( 'key2', 'key2', '', ( #3391 ) ) ;
#36035 = ORIENTED_EDGE ( 'NONE', *, *, #58048, .T. ) ;
#36037 = EDGE_CURVE ( 'NONE', #33721, #48827, #53810, .T. ) ;
#36036 = CARTESIAN_POINT ( 'NONE',  ( -2.116120943111210906, -74.98056102853675497, 170.0000000000000000 ) ) ;
#36038 = CARTESIAN_POINT ( 'NONE',  ( 9.827939172326074058, 6.382931149346556587, 68.93830584714513066 ) ) ;
#36039 = CARTESIAN_POINT ( 'NONE',  ( 157.4703587214989398, -170.0000000000000000, -62.96873488960130771 ) ) ;
#36040 = CARTESIAN_POINT ( 'NONE',  ( 200.8383807319521281, 102.8517715783673339, 30.26259293534468497 ) ) ;
#36041 = CARTESIAN_POINT ( 'NONE',  ( 65.02478361689730946, 37.39438481344068776, 170.0000000000000000 ) ) ;
#36043 = ORIENTED_EDGE ( 'NONE', *, *, #59298, .F. ) ;
#36042 = CARTESIAN_POINT ( 'NONE',  ( 0.000000000000000000, 0.000000000000000000, 41.38025477438755928 ) ) ;
#36044 = CARTESIAN_POINT ( 'NONE',  ( 70.11969827741708627, 15.47408882293423993, 39.76769945686178431 ) ) ;
#36045 = ORIENTED_EDGE ( 'NONE', *, *, #17243, .F. ) ;
#36046 = VECTOR ( 'NONE', #46274, 1000.000000000000227 ) ;
#36047 = EDGE_LOOP ( 'NONE', ( #20922, #54655, #62725, #7846 ) ) ;
#36048 = CARTESIAN_POINT ( 'NONE',  ( 110.7117404013330884, 30.20916032354562830, -77.76698815611739235 ) ) ;
#36049 = CARTESIAN_POINT ( 'NONE',  ( 64.08056813503714011, -12.89932471814424986, 43.58025477438756212 ) ) ;
#36050 = CARTESIAN_POINT ( 'NONE',  ( 21.27121078971695312, -61.42097029141944375, 40.00000000000003553 ) ) ;
#36051 = EDGE_CURVE ( 'NONE', #56852, #59604, #40914, .T. ) ;
#36052 = CARTESIAN_POINT ( 'NONE',  ( -38.69449158134467126, 11.92067517118076125, 62.59844393972618803 ) ) ;
#36053 = ADVANCED_FACE ( 'NONE', ( #40224 ), #23700, .T. ) ;
#36054 = LINE ( 'NONE', #63130, #17436 ) ;
#36055 = CARTESIAN_POINT ( 'NONE',  ( -417.6627218934913230, 219.4906275429376308, 111.5502958579881749 ) ) ;
#36056 = CYLINDRICAL_SURFACE ( 'NONE', #14025, 7.500000000000014211 ) ;
#36057 = CARTESIAN_POINT ( 'NONE',  ( -50.14523569787233725, 14.45648954445650602, 32.12416558293933377 ) ) ;
#36058 = ORIENTED_EDGE ( 'NONE', *, *, #65508, .T. ) ;
#36059 = ORIENTED_EDGE ( 'NONE', *, *, #26208, .F. ) ;
#36060 = EDGE_CURVE ( 'NONE', #40134, #32392, #19451, .T. ) ;
#36061 = CARTESIAN_POINT ( 'NONE',  ( 0.000000000000000000, 0.000000000000000000, 0.000000000000000000 ) ) ;
#36062 = DIRECTION ( 'NONE',  ( -1.000000000000000000, 0.000000000000000000, 0.000000000000000000 ) ) ;
#36063 = CARTESIAN_POINT ( 'NONE',  ( 102.8816949008297712, 25.62288855336258564, 89.32272773285413336 ) ) ;
#36064 = EDGE_CURVE ( 'NONE', #36681, #69450, #62987, .T. ) ;
#36065 = CYLINDRICAL_SURFACE ( 'NONE', #2641, 5.000000000000004441 ) ;
#36066 = CARTESIAN_POINT ( 'NONE',  ( 183.3913492984168556, 80.96922346472079823, -50.86455848634233945 ) ) ;
#36067 = PLANE ( 'NONE',  #11219 ) ;
#36068 = CARTESIAN_POINT ( 'NONE',  ( 164.9534461562627428, 63.71129898458564611, -71.04616183406005803 ) ) ;
#36069 = ORIENTED_EDGE ( 'NONE', *, *, #38744, .T. ) ;
#36070 = ORIENTED_EDGE ( 'NONE', *, *, #623, .T. ) ;
#36071 = ORIENTED_EDGE ( 'NONE', *, *, #38589, .F. ) ;
#36072 = SURFACE_STYLE_FILL_AREA ( #25870 ) ;
#36073 = CARTESIAN_POINT ( 'NONE',  ( -79.62258606008208517, 22.68765733708499965, 57.30873026444331231 ) ) ;
#36074 = LINE ( 'NONE', #12023, #42190 ) ;
#36075 = CARTESIAN_POINT ( 'NONE',  ( 105.5096892522198573, -21.88944388124440721, 2.223599993928985885 ) ) ;
#36076 = EDGE_CURVE ( 'NONE', #64911, #59267, #3621, .T. ) ;
#36077 = VECTOR ( 'NONE', #20769, 1000.000000000000000 ) ;
#36078 = CARTESIAN_POINT ( 'NONE',  ( -33.36965723649376514, 10.93726715887721390, -76.91312719118394625 ) ) ;
#36079 = EDGE_CURVE ( 'NONE', #34064, #51605, #36027, .T. ) ;
#36080 = CARTESIAN_POINT ( 'NONE',  ( -60.67627457812066183, -44.08389392193601708, 43.58025477438756212 ) ) ;
#36081 = EDGE_CURVE ( 'NONE', #18148, #53590, #6843, .T. ) ;
#36082 = CARTESIAN_POINT ( 'NONE',  ( 187.8965227056807521, 87.27289477191499145, 66.80197625647082305 ) ) ;
#36083 = CARTESIAN_POINT ( 'NONE',  ( 13.37820144534468625, 6.435512790162279728, -9.067908514598384428 ) ) ;
#36084 = AXIS2_PLACEMENT_3D ( 'NONE', #6147, #49049, #65612 ) ;
#36085 = ORIENTED_EDGE ( 'NONE', *, *, #13260, .T. ) ;
#36086 = CARTESIAN_POINT ( 'NONE',  ( 19.10949903373832015, 7.636938177523838078, 3.941116430307622487 ) ) ;
#36087 = CARTESIAN_POINT ( 'NONE',  ( 183.1910712700538681, 80.76073941711165105, 70.86391971262702327 ) ) ;
#36088 = CARTESIAN_POINT ( 'NONE',  ( 5.690023276062394331, 5.952467836904148157, -0.1306530452038075496 ) ) ;
#36089 = CARTESIAN_POINT ( 'NONE',  ( 0.000000000000000000, 0.000000000000000000, -0.002000000000002000178 ) ) ;
#36090 = CARTESIAN_POINT ( 'NONE',  ( 132.7179291807801746, 40.74118679001691845, -24.09532512744151589 ) ) ;
#36091 = CARTESIAN_POINT ( 'NONE',  ( 21.44191228441539465, 7.755009954762318358, -21.12731977189180199 ) ) ;
#36092 = CARTESIAN_POINT ( 'NONE',  ( 200.4559562755961224, 100.7034888016685272, 57.34971855850135825 ) ) ;
#36093 = VECTOR ( 'NONE', #17865, 1000.000000000000000 ) ;
#36094 = PRESENTATION_LAYER_ASSIGNMENT (  '', '', ( #32715 ) ) ;
#36095 = EDGE_LOOP ( 'NONE', ( #63347, #61118, #38179, #5603 ) ) ;
#36096 = LINE ( 'NONE', #64193, #22606 ) ;
#36097 = PRODUCT_CONTEXT ( 'NONE', #19240, 'mechanical' ) ;
#36098 = VECTOR ( 'NONE', #56833, 1000.000000000000000 ) ;
#36099 = CARTESIAN_POINT ( 'NONE',  ( -21.27554331372908081, -61.43430442924895374, 170.0000000000000000 ) ) ;
#36100 = DIRECTION ( 'NONE',  ( -0.000000000000000000, 1.000000000000000000, -0.000000000000000000 ) ) ;
#36101 = CARTESIAN_POINT ( 'NONE',  ( -109.4995148930278219, 37.75156937139181679, -44.61333367425208252 ) ) ;
#36102 = ITEM_DEFINED_TRANSFORMATION ( 'NONE', 'NONE', #16280,  #66832 ) ;
#36103 = CARTESIAN_POINT ( 'NONE',  ( 185.5412249395995730, 84.70425786166002524, -49.76124368019702615 ) ) ;
#36104 = VERTEX_POINT ( 'NONE', #41266 ) ;
#36105 = ORIENTED_EDGE ( 'NONE', *, *, #36304, .F. ) ;
#36106 = FACE_OUTER_BOUND ( 'NONE', #46330, .T. ) ;
#36107 = CARTESIAN_POINT ( 'NONE',  ( -36.11269837220804391, 15.55634918610408945, 0.000000000000000000 ) ) ;
#36108 = ORIENTED_EDGE ( 'NONE', *, *, #26512, .F. ) ;
#36109 = CARTESIAN_POINT ( 'NONE',  ( 111.8699272271189358, 29.64190505307780299, 56.63057503623819144 ) ) ;
#36110 = ORIENTED_EDGE ( 'NONE', *, *, #20168, .T. ) ;
#36111 = CARTESIAN_POINT ( 'NONE',  ( 126.4633682455862100, 38.28837286275648211, -69.07996067011775665 ) ) ;
#36112 = CARTESIAN_POINT ( 'NONE',  ( 126.5710838895481913, 37.19597237024179748, 35.21041822320580650 ) ) ;
#36113 = CARTESIAN_POINT ( 'NONE',  ( -15.55634918610411077, -41.66904755831209428, 0.000000000000000000 ) ) ;
#36114 = CARTESIAN_POINT ( 'NONE',  ( -95.05546640093039912, 29.25972325950978359, 35.93932265320741948 ) ) ;
#36115 = CARTESIAN_POINT ( 'NONE',  ( -46.66904755831212981, -15.55634918610397222, 2.000000000000001776 ) ) ;
#36117 = ORIENTED_EDGE ( 'NONE', *, *, #7935, .F. ) ;
#36116 = CARTESIAN_POINT ( 'NONE',  ( -439.4229916354183842, 400.0000000000021032, 101.0502958579930066 ) ) ;
#36118 = CARTESIAN_POINT ( 'NONE',  ( -50.12142425878460728, 12.53590371354408894, 26.66469066592269144 ) ) ;
#36119 = ORIENTED_EDGE ( 'NONE', *, *, #18590, .T. ) ;
#36120 = ORIENTED_EDGE ( 'NONE', *, *, #35410, .F. ) ;
#36122 = EDGE_CURVE ( 'NONE', #25478, #6992, #24403, .T. ) ;
#36121 = CARTESIAN_POINT ( 'NONE',  ( -168.7329347389695613, 83.83901812802758968, 5.376343091447946421 ) ) ;
#36123 = CARTESIAN_POINT ( 'NONE',  ( -145.9181947914994737, 62.49417193455357733, -35.72346211350654954 ) ) ;
#36125 = ORIENTED_EDGE ( 'NONE', *, *, #37793, .F. ) ;
#36124 = CARTESIAN_POINT ( 'NONE',  ( -133.2787743207940707, 52.78950725740544669, 66.30037897548639592 ) ) ;
#36126 = CARTESIAN_POINT ( 'NONE',  ( -29.87147652227456263, -74.98256102853682137, 73.58025477438756923 ) ) ;
#36127 = CIRCLE ( 'NONE', #49606, 5.000000000000170530 ) ;
#36128 = FACE_BOUND ( 'NONE', #62899, .T. ) ;
#36129 = EDGE_LOOP ( 'NONE', ( #362, #30030, #10684, #57565 ) ) ;
#36130 = AXIS2_PLACEMENT_3D ( 'NONE', #4369, #15611, #36376 ) ;
#36131 = CARTESIAN_POINT ( 'NONE',  ( -60.65612136648952912, 16.25551606627059442, -10.86259259823188472 ) ) ;
#36132 = ADVANCED_FACE ( 'NONE', ( #34259 ), #34951, .F. ) ;
#36133 = CARTESIAN_POINT ( 'NONE',  ( -133.3799602664182089, 52.86209125874979264, -68.72809787019492944 ) ) ;
#36134 = CARTESIAN_POINT ( 'NONE',  ( 111.9975424824652634, 172.0000000000000284, 354.1673509436691347 ) ) ;
#36135 = LINE ( 'NONE', #57594, #57193 ) ;
#36136 = CARTESIAN_POINT ( 'NONE',  ( 65.40383840050415643, 14.27443447873227633, -77.19146956980890195 ) ) ;
#36137 = ORIENTED_EDGE ( 'NONE', *, *, #59243, .T. ) ;
#36138 = EDGE_CURVE ( 'NONE', #46466, #19256, #53963, .T. ) ;
#36139 = ORIENTED_EDGE ( 'NONE', *, *, #57432, .F. ) ;
#36140 = CARTESIAN_POINT ( 'NONE',  ( -147.1538409485623049, 63.51600817366544049, -22.59291464346527434 ) ) ;
#36141 = VECTOR ( 'NONE', #19802, 1000.000000000000000 ) ;
#36142 = CARTESIAN_POINT ( 'NONE',  ( -166.2028657618940883, 79.74389853943291939, -39.30140056895983491 ) ) ;
#36143 = CARTESIAN_POINT ( 'NONE',  ( -55.05276343752909440, 15.72344139423349141, -35.21632399845986328 ) ) ;
#36144 = B_SPLINE_CURVE_WITH_KNOTS ( 'NONE', 3,
 ( #66384, #45940, #13586, #30122, #66724, #8318, #61430, #35047, #24151, #50869, #2348, #12548, #56147, #18868, #29083, #18176, #29420, #44557, #39626, #34008, #61082, #13929, #7276, #55447, #34710, #56489, #50529, #66036, #29763, #12909, #51225, #67406, #19197, #13250, #40658, #35391, #56850, #23801, #8667, #17828, #52593, #46627, #25194, #68102, #31492, #20240, #14621, #63501, #42388, #57195, #41013, #14958, #9697, #30807, #53268 ),
 .UNSPECIFIED., .F., .F.,
 ( 4, 2, 2, 2, 2, 2, 2, 2, 2, 2, 2, 2, 1, 2, 2, 2, 2, 2, 2, 2, 2, 2, 2, 2, 2, 2, 2, 4 ),
 ( 0.000000000000000000, 0.001981718938158233759, 0.002972578407237350638, 0.003963437876316467517, 0.004954297345395584397, 0.005945156814474701276, 0.006936016283553818156, 0.007926875752632935035, 0.009908594690791121956, 0.01089945415987021021, 0.01189031362894929673, 0.01288117309802838326, 0.01387203256710746978, 0.01486289203618655803, 0.01585375150526564456, 0.01684461097434472934, 0.01783547044342381413, 0.01981718938158197676, 0.02080804885066105808, 0.02179890831974014287, 0.02278976778881922419, 0.02378062725789830550, 0.02477148672697738682, 0.02576234619605646814, 0.02774406513421459261, 0.02972578407237271708, 0.03071664354145177758, 0.03170750301053083808 ),
 .UNSPECIFIED. ) ;
#36145 = LINE ( 'NONE', #61821, #25479 ) ;
#36146 = CARTESIAN_POINT ( 'NONE',  ( -72.21947956767111521, 21.03570528348186741, 34.07763384368087856 ) ) ;
#36147 = DIRECTION ( 'NONE',  ( -0.1342332658176667304, 0.9909497617679331460, 0.000000000000000000 ) ) ;
#36148 = CARTESIAN_POINT ( 'NONE',  ( 65.62985354949972816, 14.32996029952553485, -36.18682722834029875 ) ) ;
#36149 = LINE ( 'NONE', #31226, #11503 ) ;
#36150 = CARTESIAN_POINT ( 'NONE',  ( -167.9853834315979952, 81.58767916550901589, -63.57040599627210042 ) ) ;
#36151 = VERTEX_POINT ( 'NONE', #34617 ) ;
#36152 = CARTESIAN_POINT ( 'NONE',  ( -25.99999999999999289, 0.000000000000000000, -33.00000000000000000 ) ) ;
#36153 = ORIENTED_EDGE ( 'NONE', *, *, #18653, .T. ) ;
#36154 = DIRECTION ( 'NONE',  ( -0.8496664383351307803, 0.000000000000000000, 0.5273205320930463014 ) ) ;
#36155 = CARTESIAN_POINT ( 'NONE',  ( 444.9999999999999432, -35.00000000000000000, 378.0000000000000000 ) ) ;
#36156 = LINE ( 'NONE', #62550, #4881 ) ;
#36157 = CARTESIAN_POINT ( 'NONE',  ( 30.28348399776043465, 22.91216519805204754, -30.77441063284156897 ) ) ;
#36158 = CARTESIAN_POINT ( 'NONE',  ( 33.77444274891858811, 8.756048688386675494, 5.605216617422771108 ) ) ;
#36159 = LINE ( 'NONE', #57618, #112 ) ;
#36160 = CARTESIAN_POINT ( 'NONE',  ( 34.45817031441433897, 7.817703378455677310, 4.907621799910686811 ) ) ;
#36161 = CARTESIAN_POINT ( 'NONE',  ( -12.78319349481551015, 8.274445259016799170, -37.26919679932123586 ) ) ;
#36162 = CARTESIAN_POINT ( 'NONE',  ( -31.92572261726338922, 10.69135962481465363, -23.47264677473819816 ) ) ;
#36163 = ADVANCED_FACE ( 'NONE', ( #56395 ), #62371, .F. ) ;
#36164 = ORIENTED_EDGE ( 'NONE', *, *, #15864, .F. ) ;
#36165 = CARTESIAN_POINT ( 'NONE',  ( -121.3890712762008235, 44.78736737435725246, -90.10228078854700584 ) ) ;
#36166 = VERTEX_POINT ( 'NONE', #8216 ) ;
#36167 = CARTESIAN_POINT ( 'NONE',  ( 46.66904755831210139, -9.150666335777657423E-14, 0.000000000000000000 ) ) ;
#36168 = CARTESIAN_POINT ( 'NONE',  ( 8.287863202055541834, 7.382585476140732794, -69.37525033522064177 ) ) ;
#36170 = ADVANCED_FACE ( 'NONE', ( #35294 ), #30017, .F. ) ;
#36169 = CARTESIAN_POINT ( 'NONE',  ( -31.43908319763709969, 9.591432048623765638, 3.371903815725488585 ) ) ;
#36171 = DIRECTION ( 'NONE',  ( -0.000000000000000000, -1.000000000000000000, 0.000000000000000000 ) ) ;
#36172 = CARTESIAN_POINT ( 'NONE',  ( -14.66033866466834823, 7.432913330382392658, -72.86005857283349485 ) ) ;
#36173 = CARTESIAN_POINT ( 'NONE',  ( -51.66904755831210139, 6.635317295611287136E-14, 0.000000000000000000 ) ) ;
#36174 = SHAPE_REPRESENTATION ( 'rotor', ( #66832 ), #11806 ) ;
#36175 = CARTESIAN_POINT ( 'NONE',  ( 153.2523375521184335, 55.69936538551847605, -49.83022819104369461 ) ) ;
#36176 = EDGE_LOOP ( 'NONE', ( #155, #22600, #46941, #2674 ) ) ;
#36177 = AXIS2_PLACEMENT_3D ( 'NONE', #10214, #43951, #5628 ) ;
#36178 = DIRECTION ( 'NONE',  ( 1.001694258352608139E-14, -1.000000000000000000, -4.041831966856716756E-15 ) ) ;
#36179 = CARTESIAN_POINT ( 'NONE',  ( -65.00200000000002376, -1.250000000000021094, 170.0000000000000000 ) ) ;
#36180 = CARTESIAN_POINT ( 'NONE',  ( 179.4074606910091632, 78.34362448405030932, -9.519745835405062806 ) ) ;
#36181 = CARTESIAN_POINT ( 'NONE',  ( -106.7004823116342180, 36.22460663120045865, 70.94159824621738153 ) ) ;
#36182 = CARTESIAN_POINT ( 'NONE',  ( 0.000000000000000000, 0.000000000000000000, 0.000000000000000000 ) ) ;
#36183 = EDGE_LOOP ( 'NONE', ( #13349, #50762, #25248, #17867 ) ) ;
#36184 = CARTESIAN_POINT ( 'NONE',  ( 0.000000000000000000, 0.000000000000000000, 170.0000000000000000 ) ) ;
#36185 = VECTOR ( 'NONE', #22098, 1000.000000000000000 ) ;
#36186 = CARTESIAN_POINT ( 'NONE',  ( -0.5751131641471360911, 6.527254166626917709, -14.13863482346338429 ) ) ;
#36187 = CARTESIAN_POINT ( 'NONE',  ( 116.8937673311172887, 32.08228998570056945, 33.63549503582235900 ) ) ;
#36188 = VECTOR ( 'NONE', #43905, 1000.000000000000000 ) ;
#36189 = LINE ( 'NONE', #57647, #68756 ) ;
#36190 = CARTESIAN_POINT ( 'NONE',  ( -119.2682179969168601, 42.28333404791700900, -65.70518237057183342 ) ) ;
#36191 = CIRCLE ( 'NONE', #66538, 24.99999999999985434 ) ;
#36192 = ORIENTED_EDGE ( 'NONE', *, *, #65862, .T. ) ;
#36193 = CYLINDRICAL_SURFACE ( 'NONE', #13217, 7.500000000000020428 ) ;
#36194 = CARTESIAN_POINT ( 'NONE',  ( 117.3281529665582354, 32.29994712002883972, -67.75427984652691293 ) ) ;
#36195 = LINE ( 'NONE', #30925, #30817 ) ;
#36196 = CARTESIAN_POINT ( 'NONE',  ( 181.7896739982670908, 79.32116015393873454, -89.93903081948376155 ) ) ;
#36197 = DIRECTION ( 'NONE',  ( 0.8191520442889886899, 0.000000000000000000, 0.5735764363510506003 ) ) ;
#36198 = CLOSED_SHELL ( 'NONE', ( #18520, #69221, #1590, #46587, #59694, #22615, #61380, #54613, #36163, #14069, #30722, #1663, #61453, #38163, #6757, #37707, #7881, #29708, #13665, #11926, #13820, #35780, #52871, #11799, #50385, #60735, #19859, #23831 ) ) ;
#36199 = PRODUCT_RELATED_PRODUCT_CATEGORY ( 'part', '', ( #28232 ) ) ;
#36200 = VERTEX_POINT ( 'NONE', #2590 ) ;
#36201 = EDGE_CURVE ( 'NONE', #23006, #59231, #24049, .T. ) ;
#36202 = DIRECTION ( 'NONE',  ( -0.000000000000000000, 0.000000000000000000, 1.000000000000000000 ) ) ;
#36203 = ORIENTED_EDGE ( 'NONE', *, *, #16814, .T. ) ;
#36205 = EDGE_CURVE ( 'NONE', #63860, #52163, #54111, .T. ) ;
#36204 = CARTESIAN_POINT ( 'NONE',  ( -78.66644367742111399, 22.32174330031318021, -23.27090004125422595 ) ) ;
#36206 = CARTESIAN_POINT ( 'NONE',  ( 140.4959942426281998, 45.58042999908606419, 87.19380765129805866 ) ) ;
#36208 = ORIENTED_EDGE ( 'NONE', *, *, #40565, .F. ) ;
#36207 = DIRECTION ( 'NONE',  ( 1.000000000000000000, 0.000000000000000000, 0.000000000000000000 ) ) ;
#36209 = DIRECTION ( 'NONE',  ( -0.000000000000000000, 1.000000000000000000, -0.000000000000000000 ) ) ;
#36210 = LINE ( 'NONE', #31619, #55260 ) ;
#36211 = CARTESIAN_POINT ( 'NONE',  ( 2.905661822261151883E-14, 15.55634918610403084, 0.000000000000000000 ) ) ;
#36212 = ORIENTED_EDGE ( 'NONE', *, *, #48567, .T. ) ;
#36213 = FACE_OUTER_BOUND ( 'NONE', #17584, .T. ) ;
#36214 = ADVANCED_FACE ( 'NONE', ( #22128 ), #57440, .F. ) ;
#36215 = PLANE ( 'NONE',  #68059 ) ;
#36216 = ORIENTED_EDGE ( 'NONE', *, *, #15027, .T. ) ;
#36217 = CARTESIAN_POINT ( 'NONE',  ( -20.63749999999999929, 0.000000000000000000, 0.000000000000000000 ) ) ;
#36218 = CARTESIAN_POINT ( 'NONE',  ( -176.1917263072137416, 92.15415277106538383, -89.04606407215415231 ) ) ;
#36219 = CARTESIAN_POINT ( 'NONE',  ( 154.0293889979057269, 55.02370422818216866, 57.07356254584302491 ) ) ;
#36220 = EDGE_CURVE ( 'NONE', #44581, #40831, #5938, .T. ) ;
#36221 = CARTESIAN_POINT ( 'NONE',  ( -34.29440389294403246, -17.09499999999999886, 0.000000000000000000 ) ) ;
#36222 = EDGE_LOOP ( 'NONE', ( #43180, #59135, #59263, #44775 ) ) ;
#36224 = EDGE_CURVE ( 'NONE', #22804, #36796, #43744, .T. ) ;
#36223 = DIRECTION ( 'NONE',  ( -1.000000000000000000, -3.697785493223490648E-32, 0.000000000000000000 ) ) ;
#36225 = ORIENTED_EDGE ( 'NONE', *, *, #36532, .F. ) ;
#36226 = VECTOR ( 'NONE', #19938, 1000.000000000000000 ) ;
#36227 = CARTESIAN_POINT ( 'NONE',  ( 150.0980941434704334, 53.37942190380060481, -18.18456334522878848 ) ) ;
#36228 = CARTESIAN_POINT ( 'NONE',  ( -56.63808869004000712, 15.11210435325983070, 84.16920984612842460 ) ) ;
#36229 = CARTESIAN_POINT ( 'NONE',  ( 8.000000000000007105, 249.8719672152120381, -95.00000000000133582 ) ) ;
#36230 = VECTOR ( 'NONE', #53915, 1000.000000000000000 ) ;
#36231 = CARTESIAN_POINT ( 'NONE',  ( -152.9121563765244218, 67.12206067149023170, -62.47090493325013227 ) ) ;
#36232 = DIRECTION ( 'NONE',  ( 1.000000000000000000, 0.000000000000000000, -0.000000000000000000 ) ) ;
#36233 = DIRECTION ( 'NONE',  ( -0.000000000000000000, 0.001173758924898823768, 0.9999993111447559313 ) ) ;
#36234 = CARTESIAN_POINT ( 'NONE',  ( 210.6741002223296846, 114.9147155784838503, -39.28712141022325710 ) ) ;
#36236 = CARTESIAN_POINT ( 'NONE',  ( 180.6710448012268273, 78.18844465372403363, 2.464043515047717570 ) ) ;
#36235 = VECTOR ( 'NONE', #61748, 1000.000000000000000 ) ;
#36237 = VERTEX_POINT ( 'NONE', #27051 ) ;
#36238 = LINE ( 'NONE', #62631, #22921 ) ;
#36239 = ORIENTED_EDGE ( 'NONE', *, *, #5767, .F. ) ;
#36240 = CARTESIAN_POINT ( 'NONE',  ( -72.78270026377325053, 21.23376443558120741, 69.44000555021129628 ) ) ;
#36241 = CARTESIAN_POINT ( 'NONE',  ( 56.53635105806416306, 11.26263375223564012, -73.85080886644499287 ) ) ;
#36242 = DIRECTION ( 'NONE',  ( 0.000000000000000000, 1.000000000000000000, 0.000000000000000000 ) ) ;
#36243 = CYLINDRICAL_SURFACE ( 'NONE', #1944, 97.99999999999994316 ) ;
#36244 = CARTESIAN_POINT ( 'NONE',  ( 19.11382977197791178, 7.636807742668411336, 44.25505563586381896 ) ) ;
#36245 = CARTESIAN_POINT ( 'NONE',  ( -108.0902552660050446, 36.97681740369922210, -20.43870904558432855 ) ) ;
#36246 = EDGE_LOOP ( 'NONE', ( #41938, #45628, #62585, #22177 ) ) ;
#36247 = CARTESIAN_POINT ( 'NONE',  ( -71.16584859396992613, 19.60484997908768179, 64.99771648647357836 ) ) ;
#36248 = DIRECTION ( 'NONE',  ( -0.6427876096865403621, 0.7660444431189770143, 0.000000000000000000 ) ) ;
#36249 = ORIENTED_EDGE ( 'NONE', *, *, #65706, .T. ) ;
#36250 = EDGE_CURVE ( 'NONE', #22437, #11268, #61874, .T. ) ;
#36251 = EDGE_LOOP ( 'NONE', ( #46132, #46123, #56314, #17769 ) ) ;
#36252 = CARTESIAN_POINT ( 'NONE',  ( -151.6716822472524200, 66.03661194063731443, 31.02609834145020429 ) ) ;
#36253 = FACE_OUTER_BOUND ( 'NONE', #10573, .T. ) ;
#36254 = CARTESIAN_POINT ( 'NONE',  ( 173.9413349464226428, 71.67637800842355489, -19.18543995565300975 ) ) ;
#36255 = CARTESIAN_POINT ( 'NONE',  ( 0.000000000000000000, 0.000000000000000000, 170.0000000000000000 ) ) ;
#36256 = B_SPLINE_CURVE_WITH_KNOTS ( 'NONE', 3,
 ( #54990, #22643, #59562, #33208 ),
 .UNSPECIFIED., .F., .F.,
 ( 4, 4 ),
 ( 0.1259919275528365301, 0.1829744153748764923 ),
 .UNSPECIFIED. ) ;
#36257 = CARTESIAN_POINT ( 'NONE',  ( -142.0902782307734924, 58.13494170556000995, 10.22982670401919947 ) ) ;
#36258 = ORIENTED_EDGE ( 'NONE', *, *, #62688, .T. ) ;
#36259 = CYLINDRICAL_SURFACE ( 'NONE', #30045, 65.00000000000000000 ) ;
#36260 = EDGE_LOOP ( 'NONE', ( #51737, #16600, #15677 ) ) ;
#36261 = CARTESIAN_POINT ( 'NONE',  ( 212.1983751099433562, 117.2326047784727336, 10.00450108283069639 ) ) ;
#36262 = CARTESIAN_POINT ( 'NONE',  ( -144.3939084932121091, 61.25241660819418144, 43.71263044045074508 ) ) ;
#36263 = PRESENTATION_STYLE_ASSIGNMENT (( #26059 ) ) ;
#36264 = CARTESIAN_POINT ( 'NONE',  ( 9.934517078398117818, 6.383749116521619804, -92.00087700128223389 ) ) ;
#36265 = ORIENTED_EDGE ( 'NONE', *, *, #26991, .T. ) ;
#36266 = ORIENTED_EDGE ( 'NONE', *, *, #41530, .T. ) ;
#36267 = CARTESIAN_POINT ( 'NONE',  ( 64.16679220703380793, -10.37413986118096254, 170.0000000000000000 ) ) ;
#36268 = CARTESIAN_POINT ( 'NONE',  ( -128.7374182412640664, 49.61100189511262926, 84.84501753385171696 ) ) ;
#36269 = AXIS2_PLACEMENT_3D ( 'NONE', #24532, #14313, #41393 ) ;
#36270 = CARTESIAN_POINT ( 'NONE',  ( 157.4703587214989398, -170.0000000000000000, 90.59856865318074881 ) ) ;
#36271 = DIRECTION ( 'NONE',  ( -0.000000000000000000, 1.000000000000000000, -0.000000000000000000 ) ) ;
#36272 = CARTESIAN_POINT ( 'NONE',  ( 22.42430175529976211, 6.803777996989659904, 94.71421917802801715 ) ) ;
#36273 = CARTESIAN_POINT ( 'NONE',  ( 82.13067365723604496, 17.93447087949267527, -76.18668206738985305 ) ) ;
#36274 = EDGE_CURVE ( 'NONE', #55797, #45282, #62174, .T. ) ;
#36275 = ADVANCED_FACE ( 'NONE', ( #16078 ), #33820, .T. ) ;
#36276 = AXIS2_PLACEMENT_3D ( 'NONE', #68822, #48739, #4810 ) ;
#36277 = ORIENTED_EDGE ( 'NONE', *, *, #29018, .T. ) ;
#36279 = EDGE_CURVE ( 'NONE', #60290, #8293, #23105, .T. ) ;
#36278 = CARTESIAN_POINT ( 'NONE',  ( 412.3372781065085633, 179.4906275429376024, 111.5502958579881749 ) ) ;
#36280 = CARTESIAN_POINT ( 'NONE',  ( 204.6977192012829789, 108.0580384837234789, -36.32593103262158252 ) ) ;
#36281 = ADVANCED_FACE ( 'NONE', ( #26977 ), #6214, .F. ) ;
#36282 = VERTEX_POINT ( 'NONE', #48408 ) ;
#36283 = AXIS2_PLACEMENT_3D ( 'NONE', #34011, #54394, #22054 ) ;
#36284 = CARTESIAN_POINT ( 'NONE',  ( -78.66644367742111399, 22.32174330031319798, 18.57365054920947500 ) ) ;
#36285 = ORIENTED_EDGE ( 'NONE', *, *, #19380, .F. ) ;
#36286 = CARTESIAN_POINT ( 'NONE',  ( -40.99999999999995737, 0.000000000000000000, -50.00000000000000000 ) ) ;
#36287 = EDGE_CURVE ( 'NONE', #33243, #26373, #64669, .T. ) ;
#36288 = CIRCLE ( 'NONE', #46414, 24.99999999999985434 ) ;
#36289 = ORIENTED_EDGE ( 'NONE', *, *, #18540, .T. ) ;
#36290 = EDGE_CURVE ( 'NONE', #18523, #54877, #65318, .T. ) ;
#36291 = VECTOR ( 'NONE', #67644, 1000.000000000000000 ) ;
#36292 = EDGE_LOOP ( 'NONE', ( #42354, #7930, #21143, #34218, #55338 ) ) ;
#36293 = CARTESIAN_POINT ( 'NONE',  ( 8.528421445032398296, 6.376778749352038922, -44.96446147396655846 ) ) ;
#36294 = DIRECTION ( 'NONE',  ( 0.7530714660036195163, -0.6579387259397027066, 0.000000000000000000 ) ) ;
#36295 = CARTESIAN_POINT ( 'NONE',  ( 129.5193594945039308, 38.86618897895345270, 69.99177176951431534 ) ) ;
#36296 = VERTEX_POINT ( 'NONE', #17104 ) ;
#36297 = CARTESIAN_POINT ( 'NONE',  ( -38.90396040047801307, 10.93641556689195049, 90.61005997619054142 ) ) ;
#36298 = CARTESIAN_POINT ( 'NONE',  ( 181.0840389613909736, 80.03940679743418229, -63.06960825634327961 ) ) ;
#36299 = CARTESIAN_POINT ( 'NONE',  ( 0.000000000000000000, 0.000000000000000000, 43.58025477438756212 ) ) ;
#36300 = ADVANCED_FACE ( 'NONE', ( #44186 ), #11842, .T. ) ;
#36301 = CARTESIAN_POINT ( 'NONE',  ( 106.4107271020440209, 27.14892220304137282, -49.87391710848807946 ) ) ;
#36302 = CARTESIAN_POINT ( 'NONE',  ( 79.63513233364427890, 18.20496177163926177, -46.04061524578445130 ) ) ;
#36304 = EDGE_CURVE ( 'NONE', #23177, #12488, #43495, .T. ) ;
#36303 = DIRECTION ( 'NONE',  ( -1.000000000000000000, 0.000000000000000000, -0.000000000000000000 ) ) ;
#36305 = VERTEX_POINT ( 'NONE', #39286 ) ;
#36306 = FACE_OUTER_BOUND ( 'NONE', #13891, .T. ) ;
#36307 = CARTESIAN_POINT ( 'NONE',  ( -86.16504208171677703, 26.41251233979377133, -69.98968484780580468 ) ) ;
#36308 = CARTESIAN_POINT ( 'NONE',  ( -13.24252603915608617, 63.63674649211943546, 170.0000000000000000 ) ) ;
#36309 = CARTESIAN_POINT ( 'NONE',  ( 0.000000000000000000, 0.000000000000000000, -3.000000000000030198 ) ) ;
#36310 = CARTESIAN_POINT ( 'NONE',  ( -190.6985136298602015, 109.1272424661243434, -10.81538671745452795 ) ) ;
#36311 = CARTESIAN_POINT ( 'NONE',  ( 126.8947007444828614, 37.37669340849690514, 7.364425276940866461 ) ) ;
#36312 = CARTESIAN_POINT ( 'NONE',  ( -156.8764584803561775, 70.69066846313522490, 9.952307344159024183 ) ) ;
#36313 = FACE_OUTER_BOUND ( 'NONE', #52710, .T. ) ;
#36314 = CARTESIAN_POINT ( 'NONE',  ( 211.5034924207027700, 118.0100795718635425, 39.87353999634708401 ) ) ;
#36315 = DIRECTION ( 'NONE',  ( 0.4338837391175526248, 0.9009688679024218105, 0.000000000000000000 ) ) ;
#36316 = CARTESIAN_POINT ( 'NONE',  ( -103.2129897037411013, 33.25684593987700310, 45.47526677688482266 ) ) ;
#36317 = VERTEX_POINT ( 'NONE', #2008 ) ;
#36318 = AXIS2_PLACEMENT_3D ( 'NONE', #67410, #45246, #51229 ) ;
#36319 = CARTESIAN_POINT ( 'NONE',  ( -47.60153151963581308, 13.84303696664763095, 90.59163266529853331 ) ) ;
#36320 = EDGE_LOOP ( 'NONE', ( #16466, #15471, #55287, #15261 ) ) ;
#36321 = CARTESIAN_POINT ( 'NONE',  ( 0.000000000000000000, 0.000000000000000000, 0.000000000000000000 ) ) ;
#36322 = ORIENTED_EDGE ( 'NONE', *, *, #22874, .F. ) ;
#36323 = FACE_OUTER_BOUND ( 'NONE', #11363, .T. ) ;
#36324 = CARTESIAN_POINT ( 'NONE',  ( -439.4229916354182706, 388.0000000000064801, -123.9497041420119530 ) ) ;
#36325 = CYLINDRICAL_SURFACE ( 'NONE', #53672, 185.0000000000000000 ) ;
#36326 = PLANE ( 'NONE',  #67064 ) ;
#36327 = CARTESIAN_POINT ( 'NONE',  ( 137.6104751318277124, 44.92718313329109492, -50.02061863167904932 ) ) ;
#36328 = CARTESIAN_POINT ( 'NONE',  ( -30.46002654261639009, 10.45132580906817665, 3.420144955256299468 ) ) ;
#36329 = AXIS2_PLACEMENT_3D ( 'NONE', #51308, #35464, #42119 ) ;
#36330 = CARTESIAN_POINT ( 'NONE',  ( 11.21312910819262854, 7.403355431336990478, -48.98232984902662679 ) ) ;
#36331 = CARTESIAN_POINT ( 'NONE',  ( 46.39999999999999858, 0.000000000000000000, 0.000000000000000000 ) ) ;
#36332 = CARTESIAN_POINT ( 'NONE',  ( -119.2949674747224975, 43.48097822533564738, -11.96626569522580574 ) ) ;
#36333 = ORIENTED_EDGE ( 'NONE', *, *, #45037, .T. ) ;
#36334 = AXIS2_PLACEMENT_3D ( 'NONE', #46785, #58033, #30274 ) ;
#36335 = ORIENTED_EDGE ( 'NONE', *, *, #29449, .T. ) ;
#36336 = VECTOR ( 'NONE', #17840, 1000.000000000000000 ) ;
#36337 = CARTESIAN_POINT ( 'NONE',  ( 174.1571680927775105, 73.25653429923636395, 93.39935691738303092 ) ) ;
#36338 = AXIS2_PLACEMENT_3D ( 'NONE', #20177, #25811, #63087 ) ;
#36339 = CARTESIAN_POINT ( 'NONE',  ( -24.94151142167917001, 8.614613465433004436, -73.43986976775646269 ) ) ;
#36340 = VECTOR ( 'NONE', #56211, 1000.000000000000000 ) ;
#36341 = CARTESIAN_POINT ( 'NONE',  ( 9.823983574062875590, 6.382904402091123863, 6.096740015399423562 ) ) ;
#36342 = CARTESIAN_POINT ( 'NONE',  ( 43.14565945994675644, 9.942782559600564340, -76.46782334873067555 ) ) ;
#36343 = DIRECTION ( 'NONE',  ( 0.000000000000000000, 0.000000000000000000, 1.000000000000000000 ) ) ;
#36344 = DIRECTION ( 'NONE',  ( 0.000000000000000000, 1.000000000000000000, -0.000000000000000000 ) ) ;
#36345 =( LENGTH_UNIT ( ) NAMED_UNIT ( * ) SI_UNIT ( .MILLI., .METRE. ) );
#36346 = CARTESIAN_POINT ( 'NONE',  ( -179.2177980985565284, 94.18084789436638005, -46.58799062249927658 ) ) ;
#36347 = FACE_OUTER_BOUND ( 'NONE', #27904, .T. ) ;
#36348 = CARTESIAN_POINT ( 'NONE',  ( -28.13128612339710344, 10.08889185338653149, 71.30996116462026180 ) ) ;
#36349 = CARTESIAN_POINT ( 'NONE',  ( 108.7021502624939302, 21.46117544541992572, 4.839652729015487154 ) ) ;
#36350 = CARTESIAN_POINT ( 'NONE',  ( -52.45215874217871743, 13.99961488531757148, 57.62305164748294573 ) ) ;
#36351 = ORIENTED_EDGE ( 'NONE', *, *, #15952, .T. ) ;
#36352 = CARTESIAN_POINT ( 'NONE',  ( -29.47687737404360675, -68.96458294135908318, 0.000000000000000000 ) ) ;
#36353 = DIRECTION ( 'NONE',  ( 0.000000000000000000, 0.000000000000000000, -1.000000000000000000 ) ) ;
#36354 = FACE_OUTER_BOUND ( 'NONE', #59896, .T. ) ;
#36355 = CARTESIAN_POINT ( 'NONE',  ( -109.6752351740181979, 37.84903014964773860, -68.08238526816469971 ) ) ;
#36356 = CARTESIAN_POINT ( 'NONE',  ( 447.3372781065085633, 400.0000000000000568, -111.4497041420118251 ) ) ;
#36357 = LINE ( 'NONE', #57813, #18896 ) ;
#36358 = DIRECTION ( 'NONE',  ( -0.000000000000000000, -0.000000000000000000, -1.000000000000000000 ) ) ;
#36359 = EDGE_LOOP ( 'NONE', ( #26192, #12777 ) ) ;
#36360 = CARTESIAN_POINT ( 'NONE',  ( 6.400000000000000355, -7.806255641895631925E-15, -15.99999999999998579 ) ) ;
#36361 = LINE ( 'NONE', #42996, #29351 ) ;
#36362 = EDGE_CURVE ( 'NONE', #47461, #50613, #55809, .T. ) ;
#36363 = EDGE_LOOP ( 'NONE', ( #42052, #20923 ) ) ;
#36364 = EDGE_LOOP ( 'NONE', ( #2727, #21488, #23666, #39275, #10486, #25386, #63825, #48843 ) ) ;
#36365 = STYLED_ITEM ( 'NONE', ( #36263 ), #41747 ) ;
#36366 = CARTESIAN_POINT ( 'NONE',  ( 42.60194873408148908, 9.863670188337772871, 84.31185681664037190 ) ) ;
#36367 = CARTESIAN_POINT ( 'NONE',  ( -173.1211646369891355, 87.12891641440857882, -76.55650775521370122 ) ) ;
#36368 = LINE ( 'NONE', #62760, #44847 ) ;
#36369 = ORIENTED_EDGE ( 'NONE', *, *, #16732, .T. ) ;
#36370 = FACE_BOUND ( 'NONE', #26549, .T. ) ;
#36371 = LINE ( 'NONE', #57830, #10605 ) ;
#36372 = STYLED_ITEM ( 'NONE', ( #36499 ), #40140 ) ;
#36373 = EDGE_CURVE ( 'NONE', #13843, #38713, #45593, .T. ) ;
#36374 = CARTESIAN_POINT ( 'NONE',  ( 57.57684776206770749, 12.50442334002048561, -48.39072336876083824 ) ) ;
#36375 = CARTESIAN_POINT ( 'NONE',  ( 9.133089968245061030, -32.15384561068184865, 6.893343212288923993 ) ) ;
#36376 = DIRECTION ( 'NONE',  ( 1.000000000000000000, 0.000000000000000000, 0.000000000000000000 ) ) ;
#36377 = AXIS2_PLACEMENT_3D ( 'NONE', #14107, #19035, #25020 ) ;
#36378 = CARTESIAN_POINT ( 'NONE',  ( -65.36598343705435354, 0.000000000000000000, 41.38025477438755928 ) ) ;
#36379 = VECTOR ( 'NONE', #52662, 1000.000000000000000 ) ;
#36380 = EDGE_LOOP ( 'NONE', ( #59331, #31966, #65287, #51031, #56096, #39901, #59232, #47612, #42703, #46348 ) ) ;
#36381 = VECTOR ( 'NONE', #33157, 1000.000000000000000 ) ;
#36382 = CARTESIAN_POINT ( 'NONE',  ( -31.11269837220806878, 5.594483210025202879E-14, 2.000000000000001776 ) ) ;
#36383 = AXIS2_PLACEMENT_3D ( 'NONE', #58482, #54235, #48263 ) ;
#36384 = CARTESIAN_POINT ( 'NONE',  ( 9.058156535714477542, 6.378495712187263855, 61.04019519618436362 ) ) ;
#36386 = EDGE_CURVE ( 'NONE', #383, #34775, #45243, .T. ) ;
#36385 = CARTESIAN_POINT ( 'NONE',  ( -26.88635117726412105, 9.904687797303049379, 43.69655592291272228 ) ) ;
#36387 = CARTESIAN_POINT ( 'NONE',  ( 197.9843579228223973, 99.18296459057398806, 40.06359268299852516 ) ) ;
#36388 = LINE ( 'NONE', #30768, #2798 ) ;
#36390 = ORIENTED_EDGE ( 'NONE', *, *, #68300, .T. ) ;
#36389 = DIRECTION ( 'NONE',  ( -0.04486483035051862939, 0.9989930665413143673, 0.000000000000000000 ) ) ;
#36391 = CARTESIAN_POINT ( 'NONE',  ( 6.933333333333328241, 0.000000000000000000, -11.86666666666666536 ) ) ;
#36392 = ORIENTED_EDGE ( 'NONE', *, *, #65209, .T. ) ;
#36393 = EDGE_LOOP ( 'NONE', ( #26042, #9557, #12138, #46324 ) ) ;
#36394 = CARTESIAN_POINT ( 'NONE',  ( 111.1829448509513014, 30.43012797723692842, -62.81146689644553760 ) ) ;
#36395 = CARTESIAN_POINT ( 'NONE',  ( -10.00000000000000178, -31.50328976398030534, 5.000000000000000000 ) ) ;
#36396 = CARTESIAN_POINT ( 'NONE',  ( 197.6145711261845292, 97.10888456119693046, -73.21698153998225678 ) ) ;
#36397 = LINE ( 'NONE', #15629, #10307 ) ;
#36398 = CARTESIAN_POINT ( 'NONE',  ( -125.8938041572051105, 46.49392987655495091, 72.46449846362081360 ) ) ;
#36399 = CARTESIAN_POINT ( 'NONE',  ( -85.95621526752228192, 26.32462117888286102, -17.55249673712375369 ) ) ;
#36400 = DIRECTION ( 'NONE',  ( -0.000000000000000000, -0.000000000000000000, -1.000000000000000000 ) ) ;
#36401 = DIRECTION ( 'NONE',  ( -0.000000000000000000, 1.000000000000000000, -0.000000000000000000 ) ) ;
#36402 = ORIENTED_EDGE ( 'NONE', *, *, #23379, .T. ) ;
#36403 =( REPRESENTATION_RELATIONSHIP ('NONE','NONE', #46031, #38847 ) REPRESENTATION_RELATIONSHIP_WITH_TRANSFORMATION ( #45612 )SHAPE_REPRESENTATION_RELATIONSHIP( ) );
#36404 = ORIENTED_EDGE ( 'NONE', *, *, #150, .F. ) ;
#36405 = CARTESIAN_POINT ( 'NONE',  ( 64.93224207568368911, 14.16036304753835395, -9.121094072479223769 ) ) ;
#36406 = CARTESIAN_POINT ( 'NONE',  ( -85.66184035008924980, 26.20110535976566979, -39.89909253867068628 ) ) ;
#36407 = CARTESIAN_POINT ( 'NONE',  ( 116.3987821536696146, 31.83542673691012226, 86.50273311544268040 ) ) ;
#36408 = CARTESIAN_POINT ( 'NONE',  ( -31.43908319763710679, -170.0000000000000000, 37.71645440618917888 ) ) ;
#36409 = CARTESIAN_POINT ( 'NONE',  ( 48.11816970607237209, 43.69944786994017250, 40.00000000000003553 ) ) ;
#36410 = DIRECTION ( 'NONE',  ( -4.314083075427411048E-32, -1.000000000000000000, -6.123233995736762338E-17 ) ) ;
#36411 = CARTESIAN_POINT ( 'NONE',  ( 164.3702714028688376, 63.22112480708619131, -67.51708439595032019 ) ) ;
#36412 = ORIENTED_EDGE ( 'NONE', *, *, #62910, .F. ) ;
#36413 = ORIENTED_EDGE ( 'NONE', *, *, #11597, .T. ) ;
#36414 = VERTEX_POINT ( 'NONE', #39972 ) ;
#36415 = VECTOR ( 'NONE', #67715, 1000.000000000000000 ) ;
#36416 = CARTESIAN_POINT ( 'NONE',  ( 16.00641379534997455, -64.51123194475178479, 133.5802547743875550 ) ) ;
#36417 = CARTESIAN_POINT ( 'NONE',  ( -81.67992981004169906, 23.49232121719083821, 57.89061922115716641 ) ) ;
#36418 = CARTESIAN_POINT ( 'NONE',  ( 103.0463737467386665, 25.69265572325593538, -95.00000000000133582 ) ) ;
#36419 = VECTOR ( 'NONE', #56401, 1000.000000000000000 ) ;
#36420 = CARTESIAN_POINT ( 'NONE',  ( -37.37206033059241150, 11.66494618096610836, -74.25636662139309863 ) ) ;
#36421 = CARTESIAN_POINT ( 'NONE',  ( 15.55634918610406103, 15.55634918610400241, 85.00100000000000477 ) ) ;
#36422 = CARTESIAN_POINT ( 'NONE',  ( 31.91375106836930087, 7.553354707452895056, 63.77039173626905466 ) ) ;
#36423 = CARTESIAN_POINT ( 'NONE',  ( 15.29293866748104413, 6.484959508098438796, -8.674393508222099314 ) ) ;
#36424 = EDGE_CURVE ( 'NONE', #42749, #2120, #19194, .T. ) ;
#36425 = CARTESIAN_POINT ( 'NONE',  ( 23.04797191264876233, 7.849755664016357493, 8.723983137946492050 ) ) ;
#36426 = CARTESIAN_POINT ( 'NONE',  ( 183.1865184929770862, 80.75677158533828504, 56.45068346174127782 ) ) ;
#36427 = CARTESIAN_POINT ( 'NONE',  ( -124.1094910780272329, 45.33021696310839133, 3.987170503012005263 ) ) ;
#36428 = CARTESIAN_POINT ( 'NONE',  ( 3.678442866637813759E-12, -65.13282190615278466, -9.999999999999998224 ) ) ;
#36429 = CIRCLE ( 'NONE', #3846, 20.00000000000000355 ) ;
#36430 = CARTESIAN_POINT ( 'NONE',  ( 132.0440382699655117, 40.34028297386455364, -23.97074691722912121 ) ) ;
#36431 = DIRECTION ( 'NONE',  ( -1.000000000000000000, -0.000000000000000000, -0.000000000000000000 ) ) ;
#36432 = CARTESIAN_POINT ( 'NONE',  ( 15.29912143387264223, 7.491799981865497671, 3.170157082241544799 ) ) ;
#36433 = CONICAL_SURFACE ( 'NONE', #46511, 8.000000000000001776, 1.047197551196595855 ) ;
#36434 = ADVANCED_FACE ( 'NONE', ( #61762 ), #51574, .T. ) ;
#36435 = VECTOR ( 'NONE', #59017, 1000.000000000000000 ) ;
#36436 = ORIENTED_EDGE ( 'NONE', *, *, #51736, .T. ) ;
#36437 = CARTESIAN_POINT ( 'NONE',  ( 186.6118452967672852, 84.37814701615444335, 15.05814710111441457 ) ) ;
#36438 = APPLICATION_PROTOCOL_DEFINITION ( 'draft international standard', 'automotive_design', 1998, #29618 ) ;
#36439 = CARTESIAN_POINT ( 'NONE',  ( 173.6012773665503630, 71.36035397668605640, 36.22030391453991882 ) ) ;
#36440 = PLANE ( 'NONE',  #33162 ) ;
#36441 = CARTESIAN_POINT ( 'NONE',  ( -15.67984581961064450, 63.08044415722863363, 133.5802547743875550 ) ) ;
#36442 = CARTESIAN_POINT ( 'NONE',  ( 187.2296622856351291, 86.53808614709453195, -48.03209938450030592 ) ) ;
#36443 = ORIENTED_EDGE ( 'NONE', *, *, #56327, .T. ) ;
#36444 = EDGE_LOOP ( 'NONE', ( #49405, #46617, #27235, #4012 ) ) ;
#36445 = EDGE_CURVE ( 'NONE', #58070, #12845, #44902, .T. ) ;
#36446 = CARTESIAN_POINT ( 'NONE',  ( -142.4991775570125299, 58.45550857435407721, -12.74363189635909421 ) ) ;
#36447 = CARTESIAN_POINT ( 'NONE',  ( 197.9843579228224542, 99.18296459057401648, 13.21904209253488816 ) ) ;
#36448 = EDGE_CURVE ( 'NONE', #38167, #30354, #36144, .T. ) ;
#36449 = ORIENTED_EDGE ( 'NONE', *, *, #18981, .T. ) ;
#36450 = CYLINDRICAL_SURFACE ( 'NONE', #40327, 4.999999999999997335 ) ;
#36451 = VERTEX_POINT ( 'NONE', #46976 ) ;
#36452 = CARTESIAN_POINT ( 'NONE',  ( 126.8114659053431694, 38.48351437375814044, -72.99081090039057074 ) ) ;
#36453 = CARTESIAN_POINT ( 'NONE',  ( 126.5880720616305837, 37.20544379858409201, 38.87743667281387872 ) ) ;
#36454 = DIRECTION ( 'NONE',  ( 0.000000000000000000, 0.000000000000000000, 1.000000000000000000 ) ) ;
#36455 = EDGE_CURVE ( 'NONE', #22304, #67008, #32775, .T. ) ;
#36456 = CARTESIAN_POINT ( 'NONE',  ( -94.88380767928866533, 29.17964217339916289, 39.28844685949278670 ) ) ;
#36457 = LINE ( 'NONE', #45633, #35028 ) ;
#36459 = ORIENTED_EDGE ( 'NONE', *, *, #38007, .F. ) ;
#36458 = DIRECTION ( 'NONE',  ( 1.000000000000000000, 0.000000000000000000, 0.000000000000000000 ) ) ;
#36460 = CARTESIAN_POINT ( 'NONE',  ( -190.6985136298602015, 109.1272424661243434, 42.87371446347281534 ) ) ;
#36461 = VERTEX_POINT ( 'NONE', #15314 ) ;
#36462 = EDGE_LOOP ( 'NONE', ( #37598, #12635, #25807, #22195 ) ) ;
#36463 = CYLINDRICAL_SURFACE ( 'NONE', #31161, 5.000000000000004441 ) ;
#36464 = AXIS2_PLACEMENT_3D ( 'NONE', #61896, #13719, #51703 ) ;
#36465 = DIRECTION ( 'NONE',  ( -0.000000000000000000, 1.000000000000000000, -0.000000000000000000 ) ) ;
#36466 = ADVANCED_FACE ( 'NONE', ( #36777 ), #58220, .F. ) ;
#36467 = CARTESIAN_POINT ( 'NONE',  ( -145.3233446620410803, 62.00659513626054320, -36.07151025764724750 ) ) ;
#36469 = ORIENTED_EDGE ( 'NONE', *, *, #26104, .F. ) ;
#36468 = CARTESIAN_POINT ( 'NONE',  ( -127.6881387055493207, 48.89937523111244388, 57.67872152613632153 ) ) ;
#36470 = CARTESIAN_POINT ( 'NONE',  ( -78.66644367742111399, -170.0000000000000000, 18.57365054920947500 ) ) ;
#36471 = EDGE_CURVE ( 'NONE', #66651, #15369, #15215, .T. ) ;
#36472 = EDGE_CURVE ( 'NONE', #36947, #1035, #32871, .T. ) ;
#36473 = FACE_OUTER_BOUND ( 'NONE', #64438, .T. ) ;
#36474 = EDGE_CURVE ( 'NONE', #69562, #25590, #49025, .T. ) ;
#36475 = AXIS2_PLACEMENT_3D ( 'NONE', #65154, #33843, #38412 ) ;
#36476 = VERTEX_POINT ( 'NONE', #43757 ) ;
#36477 = CARTESIAN_POINT ( 'NONE',  ( -62.54085973597667447, 16.81797209566547480, -16.36302326089210268 ) ) ;
#36478 = CARTESIAN_POINT ( 'NONE',  ( -132.0870433264403516, 51.94057326482885628, -65.02066728891763603 ) ) ;
#36479 = CARTESIAN_POINT ( 'NONE',  ( 181.0840389613909736, 78.60582251573003987, -89.91415884680696990 ) ) ;
#36480 = AXIS2_PLACEMENT_3D ( 'NONE', #58928, #36454, #5473 ) ;
#36481 = CARTESIAN_POINT ( 'NONE',  ( 25.00000000000000000, 65.13282190615278466, -9.999999999999998224 ) ) ;
#36482 = CARTESIAN_POINT ( 'NONE',  ( -24.39249304643438521, 60.24953346690454481, 170.0000000000000000 ) ) ;
#36483 = ORIENTED_EDGE ( 'NONE', *, *, #2469, .F. ) ;
#36484 = VERTEX_POINT ( 'NONE', #37442 ) ;
#36485 = EDGE_LOOP ( 'NONE', ( #19411, #8634, #3382, #67193 ) ) ;
#36486 = CARTESIAN_POINT ( 'NONE',  ( -783.0172411895269988, -622.0000000000060254, 10.00000000000000000 ) ) ;
#36487 = DIRECTION ( 'NONE',  ( 1.000000000000000000, 0.000000000000000000, 0.000000000000000000 ) ) ;
#36488 = DIRECTION ( 'NONE',  ( 1.000000000000000000, 0.000000000000000000, -0.000000000000000000 ) ) ;
#36489 = CARTESIAN_POINT ( 'NONE',  ( 103.5589117581614431, 27.00490790413959630, -66.82677417890924687 ) ) ;
#36490 = CARTESIAN_POINT ( 'NONE',  ( -75.43271753227888610, 22.18711452892410918, 44.70239127070650653 ) ) ;
#36491 = CARTESIAN_POINT ( 'NONE',  ( 79.52861599156695149, 17.11914630560288586, 34.74630206043598690 ) ) ;
#36492 = PLANE ( 'NONE',  #55007 ) ;
#36493 = CARTESIAN_POINT ( 'NONE',  ( -119.5563837756079550, 43.64229894412653721, 42.16241770139036049 ) ) ;
#36494 = CARTESIAN_POINT ( 'NONE',  ( -166.9969673948021693, 80.56076768517782227, -64.71887823221233305 ) ) ;
#36495 = EDGE_LOOP ( 'NONE', ( #30892, #49427, #26739, #48473 ) ) ;
#36496 = CARTESIAN_POINT ( 'NONE',  ( -109.6660553119434951, 36.69391917620599486, -14.34154704396632418 ) ) ;
#36497 = VERTEX_POINT ( 'NONE', #26558 ) ;
#36498 = CARTESIAN_POINT ( 'NONE',  ( -177.9668641613811531, 92.68804954532606644, -90.16053173884390048 ) ) ;
#36499 = PRESENTATION_STYLE_ASSIGNMENT (( #25614 ) ) ;
#36500 = PLANE ( 'NONE',  #32950 ) ;
#36501 = CARTESIAN_POINT ( 'NONE',  ( -189.2346268516247392, 107.0830361517164846, -68.74365180755535221 ) ) ;
#36502 = DIRECTION ( 'NONE',  ( -0.000000000000000000, 1.000000000000000000, -0.000000000000000000 ) ) ;
#36503 = DIRECTION ( 'NONE',  ( -0.000000000000000000, -1.000000000000000000, -0.000000000000000000 ) ) ;
#36504 = CARTESIAN_POINT ( 'NONE',  ( 37.00112095025829717, 8.109340230899352520, 17.67886562343527856 ) ) ;
#36505 = CARTESIAN_POINT ( 'NONE',  ( -53.31111153860250340, -37.18770477615797176, 170.0000000000000000 ) ) ;
#36506 = CARTESIAN_POINT ( 'NONE',  ( -38.54237244144231767, 11.89088379031760034, -13.55305385010844432 ) ) ;
#36507 = EDGE_LOOP ( 'NONE', ( #15363, #6378, #17648, #8008 ) ) ;
#36508 = FACE_OUTER_BOUND ( 'NONE', #16647, .T. ) ;
#36510 = VERTEX_POINT ( 'NONE', #26897 ) ;
#36509 = EDGE_CURVE ( 'NONE', #60060, #21253, #46156, .T. ) ;
#36511 = DIRECTION ( 'NONE',  ( -1.000000000000000000, 0.000000000000000000, -1.337618101958020291E-16 ) ) ;
#36512 = SURFACE_SIDE_STYLE ('',( #57628 ) ) ;
#36513 = CARTESIAN_POINT ( 'NONE',  ( -25.50312845906833914, 8.692070753302667541, 6.281119717299506355 ) ) ;
#36514 = CARTESIAN_POINT ( 'NONE',  ( 0.000000000000000000, 0.000000000000000000, 170.0000000000000000 ) ) ;
#36515 = CARTESIAN_POINT ( 'NONE',  ( -12.77647591501652791, 7.263973827022343066, -75.41787670511681085 ) ) ;
#36516 = CARTESIAN_POINT ( 'NONE',  ( -94.79166046756726871, 29.13671350128075943, -15.17907392333536087 ) ) ;
#36517 = CARTESIAN_POINT ( 'NONE',  ( 150.9013375937531407, 53.96275732797612790, -39.99563633385837846 ) ) ;
#36518 = EDGE_CURVE ( 'NONE', #28258, #11580, #21615, .T. ) ;
#36519 = CIRCLE ( 'NONE', #57901, 242.4895526022646379 ) ;
#36520 = ORIENTED_EDGE ( 'NONE', *, *, #5320, .F. ) ;
#36521 = VECTOR ( 'NONE', #15541, 1000.000000000000000 ) ;
#36522 = DIRECTION ( 'NONE',  ( -0.01967768242440602611, 0.9998063756620100273, 4.132858238445186898E-15 ) ) ;
#36523 = CARTESIAN_POINT ( 'NONE',  ( -155.7455325080991599, 71.01834415181988902, 69.23728585488152021 ) ) ;
#36524 = CARTESIAN_POINT ( 'NONE',  ( 174.4978817191264113, 73.57770570413205746, -20.47869960585826732 ) ) ;
#36525 = CARTESIAN_POINT ( 'NONE',  ( 39.54205320694339321, 51.58901073076764021, 170.0000000000000000 ) ) ;
#36526 = CARTESIAN_POINT ( 'NONE',  ( -55.15976438495155776, 34.41253982194033512, 43.58025477438756923 ) ) ;
#36527 = EDGE_LOOP ( 'NONE', ( #33600, #55070 ) ) ;
#36529 = CARTESIAN_POINT ( 'NONE',  ( -173.9526029538036198, 89.57590038685104616, -76.52212602822480392 ) ) ;
#36528 = CIRCLE ( 'NONE', #1676, 19.99999999999999645 ) ;
#36530 = VECTOR ( 'NONE', #967, 1000.000000000000000 ) ;
#36531 = CARTESIAN_POINT ( 'NONE',  ( -1.319107422865894552, 6.554467368239822456, -19.83637397167817440 ) ) ;
#36532 = EDGE_CURVE ( 'NONE', #51087, #17040, #34553, .T. ) ;
#36534 = EDGE_CURVE ( 'NONE', #53581, #52273, #39544, .T. ) ;
#36533 = CARTESIAN_POINT ( 'NONE',  ( 110.2429982417149432, 28.88204397445228722, 44.61121420573733332 ) ) ;
#36535 = VECTOR ( 'NONE', #6783, 1000.000000000000000 ) ;
#36536 = DIRECTION ( 'NONE',  ( 0.7071067811865463515, 0.000000000000000000, -0.7071067811865487940 ) ) ;
#36537 = ADVANCED_FACE ( 'NONE', ( #12463 ), #34967, .F. ) ;
#36538 = CIRCLE ( 'NONE', #63495, 25.12245591505646303 ) ;
#36539 = CARTESIAN_POINT ( 'NONE',  ( 137.4117721579688407, 43.61242559081431125, 43.63136637536613449 ) ) ;
#36540 = EDGE_CURVE ( 'NONE', #27181, #65685, #10967, .T. ) ;
#36541 = ORIENTED_EDGE ( 'NONE', *, *, #63357, .F. ) ;
#36542 = CARTESIAN_POINT ( 'NONE',  ( 197.3054165770396935, 96.72615186924558373, 35.39984128414984355 ) ) ;
#36543 = CARTESIAN_POINT ( 'NONE',  ( 111.1868021579656443, 29.32055685204858975, -62.81157359280074814 ) ) ;
#36544 = CARTESIAN_POINT ( 'NONE',  ( 185.5457097283155008, 84.70846743303874860, 42.85523241993036692 ) ) ;
#36545 = CARTESIAN_POINT ( 'NONE',  ( 164.0073343966822108, 64.23003864582456401, 13.75067327205471912 ) ) ;
#36546 = CARTESIAN_POINT ( 'NONE',  ( 75.00000000000000000, 0.000000000000000000, 0.000000000000000000 ) ) ;
#36547 = VERTEX_POINT ( 'NONE', #40927 ) ;
#36548 = DIRECTION ( 'NONE',  ( -0.000000000000000000, -0.000000000000000000, -1.000000000000000000 ) ) ;
#36549 = ORIENTED_EDGE ( 'NONE', *, *, #43090, .F. ) ;
#36550 = CARTESIAN_POINT ( 'NONE',  ( -74.40004226286974642, 20.74218500375954122, -21.94398046546645986 ) ) ;
#36551 = DIRECTION ( 'NONE',  ( 0.000000000000000000, -1.000000000000000000, 0.000000000000000000 ) ) ;
#36552 = CARTESIAN_POINT ( 'NONE',  ( -62.45356936877017517, 16.79156452995240301, 36.57604332370287636 ) ) ;
#36554 = ORIENTED_EDGE ( 'NONE', *, *, #36122, .T. ) ;
#36553 = CARTESIAN_POINT ( 'NONE',  ( 150.4722669492348359, 53.65054032737657508, 7.353690365303933163 ) ) ;
#36555 = CARTESIAN_POINT ( 'NONE',  ( 181.0840389613909736, -170.0000000000000000, 9.964043515047732669 ) ) ;
#36556 = DIRECTION ( 'NONE',  ( 1.000000000000000000, 0.000000000000000000, 0.000000000000000000 ) ) ;
#36557 = EDGE_CURVE ( 'NONE', #38023, #65787, #25800, .T. ) ;
#36558 = ADVANCED_FACE ( 'NONE', ( #30375 ), #46897, .F. ) ;
#36559 = CARTESIAN_POINT ( 'NONE',  ( 111.1865443042262029, 30.43181341527239070, -50.87768516474636726 ) ) ;
#36560 = VERTEX_POINT ( 'NONE', #9264 ) ;
#36561 = ADVANCED_FACE ( 'NONE', ( #31079 ), #62387, .F. ) ;
#36562 = DIRECTION ( 'NONE',  ( 0.000000000000000000, -0.8660254037844382635, -0.5000000000000006661 ) ) ;
#36563 = DIRECTION ( 'NONE',  ( -1.156482317317871232E-16, 0.000000000000000000, -1.000000000000000000 ) ) ;
#36564 = CIRCLE ( 'NONE', #48878, 5.000000000000004441 ) ;
#36565 = VERTEX_POINT ( 'NONE', #57114 ) ;
#36566 = CARTESIAN_POINT ( 'NONE',  ( 141.0804878838241052, 45.96076546397617335, 65.94046305877685654 ) ) ;
#36567 = CARTESIAN_POINT ( 'NONE',  ( 157.4703587214989398, 58.92748579479259519, 71.25401806271709404 ) ) ;
#36568 = CARTESIAN_POINT ( 'NONE',  ( 149.9552318559267121, 52.03645904563055780, 63.77717096610509628 ) ) ;
#36569 = DIRECTION ( 'NONE',  ( -0.000000000000000000, -0.000000000000000000, 1.000000000000000000 ) ) ;
#36570 = ORIENTED_EDGE ( 'NONE', *, *, #35119, .T. ) ;
#36571 = CARTESIAN_POINT ( 'NONE',  ( 46.65860211212412878, 10.48377752989033951, 12.52835627842576294 ) ) ;
#36572 = ORIENTED_EDGE ( 'NONE', *, *, #42335, .F. ) ;
#36573 = VECTOR ( 'NONE', #65041, 1000.000000000000000 ) ;
#36574 = CARTESIAN_POINT ( 'NONE',  ( 156.3797504404255676, 58.07856685387021400, -24.20320859245837752 ) ) ;
#36575 = CARTESIAN_POINT ( 'NONE',  ( 212.0104729185451617, 118.7959000526602722, -15.28514065634545283 ) ) ;
#36576 = AXIS2_PLACEMENT_3D ( 'NONE', #32089, #26811, #39447 ) ;
#36577 = VECTOR ( 'NONE', #27166, 1000.000000000000000 ) ;
#36578 = DIRECTION ( 'NONE',  ( -0.000000000000000000, 1.000000000000000000, -0.000000000000000000 ) ) ;
#36579 = CARTESIAN_POINT ( 'NONE',  ( -151.2410113808309120, 65.66338888995504419, -76.46739901466715139 ) ) ;
#36580 = DIRECTION ( 'NONE',  ( -0.000000000000000000, 1.000000000000000000, -0.000000000000000000 ) ) ;
#36581 = AXIS2_PLACEMENT_3D ( 'NONE', #25972, #42483, #10467 ) ;
#36582 = CARTESIAN_POINT ( 'NONE',  ( 181.9295958320008424, 80.90438706151873305, 2.499716765681279096 ) ) ;
#36583 = CARTESIAN_POINT ( 'NONE',  ( 211.0967808702091020, 115.5516932918876734, -47.74761114722220157 ) ) ;
#36584 = CARTESIAN_POINT ( 'NONE',  ( -4.364688291132793552, 24.74039788130344419, 0.000000000000000000 ) ) ;
#36586 = EDGE_LOOP ( 'NONE', ( #52053, #6853, #9868, #38004 ) ) ;
#36585 = SHAPE_REPRESENTATION ( 'back cover', ( #66832 ), #51149 ) ;
#36587 = CARTESIAN_POINT ( 'NONE',  ( 109.9975424824652634, 179.2896996249788799, 369.5505932007772003 ) ) ;
#36588 = EDGE_LOOP ( 'NONE', ( #52309, #53552, #52739, #9306 ) ) ;
#36589 = CARTESIAN_POINT ( 'NONE',  ( -74.20136529587827567, 21.74007521413449595, 70.79374357570557663 ) ) ;
#36590 = LINE ( 'NONE', #13828, #61031 ) ;
#36591 = CARTESIAN_POINT ( 'NONE',  ( 39.40195752203892710, 9.424259417798131366, -23.77526687496409608 ) ) ;
#36592 =( LENGTH_UNIT ( ) NAMED_UNIT ( * ) SI_UNIT ( .MILLI., .METRE. ) );
#36593 = CARTESIAN_POINT ( 'NONE',  ( -3.306248862503413655, 500.0000000000000000, -51.64566090791306863 ) ) ;
#36594 = CARTESIAN_POINT ( 'NONE',  ( -0.7888889703213518567, 6.534858899049522662, 88.68874176213427063 ) ) ;
#36595 = CARTESIAN_POINT ( 'NONE',  ( -103.2164890789475322, 34.39030697009940951, -8.213902352593930090 ) ) ;
#36596 = ORIENTED_EDGE ( 'NONE', *, *, #29454, .T. ) ;
#36597 = LINE ( 'NONE', #9866, #25200 ) ;
#36598 = DIRECTION ( 'NONE',  ( -0.6910626489868685329, 0.7227948638273878901, 0.000000000000000000 ) ) ;
#36599 = VERTEX_POINT ( 'NONE', #31414 ) ;
#36600 = ORIENTED_EDGE ( 'NONE', *, *, #62855, .F. ) ;
#36601 = CARTESIAN_POINT ( 'NONE',  ( -150.3898662070192245, 64.92828409760431896, 45.72082123989907387 ) ) ;
#36602 = CARTESIAN_POINT ( 'NONE',  ( 57.07734607129818727, 11.37318329671159489, -47.82811536398262575 ) ) ;
#36603 = CARTESIAN_POINT ( 'NONE',  ( 181.0840389613909736, 78.60582251573003987, -24.38050707541595230 ) ) ;
#36604 =( NAMED_UNIT ( * ) PLANE_ANGLE_UNIT ( ) SI_UNIT ( $, .RADIAN. ) );
#36605 = EDGE_CURVE ( 'NONE', #1104, #62158, #58800, .T. ) ;
#36606 = CARTESIAN_POINT ( 'NONE',  ( 99.71998884745383407, 190.0000000000000000, 7.478223336038896996 ) ) ;
#36607 = EDGE_LOOP ( 'NONE', ( #62323, #59726, #58034 ) ) ;
#36608 = CARTESIAN_POINT ( 'NONE',  ( -127.4644500646574556, 48.74852676951794450, 30.78273999091167568 ) ) ;
#36609 = EDGE_LOOP ( 'NONE', ( #44239, #17252, #22325, #42126 ) ) ;
#36610 = CARTESIAN_POINT ( 'NONE',  ( 210.1954643503415525, 114.1986276268023488, 14.97053208330250484 ) ) ;
#36611 = CARTESIAN_POINT ( 'NONE',  ( -142.0227972901369071, 59.36121938936275200, 37.66433558148366956 ) ) ;
#36612 = CARTESIAN_POINT ( 'NONE',  ( 210.1633650091869185, 114.1507944623966750, 31.56596133871580179 ) ) ;
#36613 = FACE_OUTER_BOUND ( 'NONE', #34579, .T. ) ;
#36614 = ADVANCED_FACE ( 'NONE', ( #32447 ), #32789, .F. ) ;
#36615 = PRODUCT ( 'key', 'key', '', ( #20946 ) ) ;
#36616 = CIRCLE ( 'NONE', #69130, 65.36598343705435354 ) ;
#36617 = ADVANCED_FACE ( 'NONE', ( #38408 ), #10629, .T. ) ;
#36618 = ORIENTED_EDGE ( 'NONE', *, *, #33804, .F. ) ;
#36619 = EDGE_CURVE ( 'NONE', #5211, #32318, #4260, .T. ) ;
#36620 = EDGE_LOOP ( 'NONE', ( #24816, #41353, #14262, #59290 ) ) ;
#36621 = CARTESIAN_POINT ( 'NONE',  ( 114.4930355657061511, -21.89000795769331376, -2.217852339353778124 ) ) ;
#36622 = CARTESIAN_POINT ( 'NONE',  ( -133.3409562061681584, 52.83409703973299543, 92.75988323507705502 ) ) ;
#36623 = AXIS2_PLACEMENT_3D ( 'NONE', #22826, #32681, #315 ) ;
#36624 = CARTESIAN_POINT ( 'NONE',  ( 34.45158752686798209, 8.829194381142023929, -64.30894078306647543 ) ) ;
#36625 = LINE ( 'NONE', #8155, #37712 ) ;
#36626 = CARTESIAN_POINT ( 'NONE',  ( -48.00000000000000711, -20.00000000000000355, 4.000000000000000000 ) ) ;
#36627 = CARTESIAN_POINT ( 'NONE',  ( 8.727163641868461497, 7.383472852351860460, 88.65466339244591154 ) ) ;
#36628 = CIRCLE ( 'NONE', #11903, 8.000000000000000000 ) ;
#36629 = VECTOR ( 'NONE', #18032, 1000.000000000000000 ) ;
#36630 = ORIENTED_EDGE ( 'NONE', *, *, #18444, .T. ) ;
#36631 = PRODUCT_DEFINITION_FORMATION_WITH_SPECIFIED_SOURCE ( 'ANY', '', #52880, .NOT_KNOWN. ) ;
#36632 = DIRECTION ( 'NONE',  ( -1.000000000000000000, 0.000000000000000000, -2.168404344971009361E-16 ) ) ;
#36633 = AXIS2_PLACEMENT_3D ( 'NONE', #11715, #12774, #23339 ) ;
#36634 = CARTESIAN_POINT ( 'NONE',  ( -97.49219489034503283, 30.41416107059312068, 59.07020065800807629 ) ) ;
#36635 = ORIENTED_EDGE ( 'NONE', *, *, #49395, .T. ) ;
#36636 = CARTESIAN_POINT ( 'NONE',  ( -85.46258339457286013, 25.02772366257410042, 7.891551977632535575 ) ) ;
#36637 = VERTEX_POINT ( 'NONE', #50370 ) ;
#36638 = AXIS2_PLACEMENT_3D ( 'NONE', #44794, #66274, #18066 ) ;
#36639 = ORIENTED_EDGE ( 'NONE', *, *, #31350, .F. ) ;
#36640 = VERTEX_POINT ( 'NONE', #28201 ) ;
#36641 = CARTESIAN_POINT ( 'NONE',  ( -118.3918229753714968, 42.92682904595258719, 10.76576233191594234 ) ) ;
#36642 = CARTESIAN_POINT ( 'NONE',  ( -177.5259994307673423, 92.16784265327248704, 59.07817098000860057 ) ) ;
#36643 = CARTESIAN_POINT ( 'NONE',  ( 131.6005058089755266, 40.07838125795768747, 56.68696652403973957 ) ) ;
#36644 = ORIENTED_EDGE ( 'NONE', *, *, #67276, .T. ) ;
#36645 = EDGE_CURVE ( 'NONE', #59608, #27414, #51060, .T. ) ;
#36646 = CARTESIAN_POINT ( 'NONE',  ( -32.09835183227463773, 9.700355081940386981, 83.92768983820710105 ) ) ;
#36647 = CARTESIAN_POINT ( 'NONE',  ( 152.2940756559018780, 53.73566983921581652, 31.47669956291998616 ) ) ;
#36648 = DIRECTION ( 'NONE',  ( 1.000000000000000000, 0.000000000000000000, 0.000000000000000000 ) ) ;
#36649 = CYLINDRICAL_SURFACE ( 'NONE', #11356, 7.500000000000013323 ) ;
#36650 = CARTESIAN_POINT ( 'NONE',  ( -25.98312968277007329, 8.759224980175259745, 32.56453152482685454 ) ) ;
#36651 = CARTESIAN_POINT ( 'NONE',  ( -143.4048679855200987, 60.45763799613827416, -64.79020762706440451 ) ) ;
#36652 = ORIENTED_EDGE ( 'NONE', *, *, #51091, .F. ) ;
#36653 = DIRECTION ( 'NONE',  ( -0.9959742939952382912, -0.08963930890344087854, 0.000000000000000000 ) ) ;
#36654 = CARTESIAN_POINT ( 'NONE',  ( -85.10909119100207931, 25.97025675005451717, -73.33204673147415065 ) ) ;
#36655 = CARTESIAN_POINT ( 'NONE',  ( 174.2468109002383585, 73.34092405459593067, 13.05881135404167637 ) ) ;
#36656 = DIRECTION ( 'NONE',  ( 0.000000000000000000, 0.000000000000000000, 1.000000000000000000 ) ) ;
#36657 = CARTESIAN_POINT ( 'NONE',  ( 34.76618902119740540, 54.93755186520760958, 170.0000000000000000 ) ) ;
#36658 = CARTESIAN_POINT ( 'NONE',  ( 11.29825944729837062, -74.09495289492984682, 41.38025477438755928 ) ) ;
#36659 = CARTESIAN_POINT ( 'NONE',  ( -156.3790798118593557, 70.23422112803314121, 8.359172547404261522 ) ) ;
#36660 = CARTESIAN_POINT ( 'NONE',  ( -118.7011544766493074, 43.11604763363182968, -67.11694934325225859 ) ) ;
#36661 = CARTESIAN_POINT ( 'NONE',  ( 64.69649025047539226, 13.06878919510320891, 3.155138310929866741 ) ) ;
#36662 = DIRECTION ( 'NONE',  ( -0.000000000000000000, -0.000000000000000000, -1.000000000000000000 ) ) ;
#36663 = CARTESIAN_POINT ( 'NONE',  ( -105.4556185321791446, 34.42302275449793569, 44.83015365805241004 ) ) ;
#36664 = EDGE_LOOP ( 'NONE', ( #55707, #49282, #44542, #65724 ) ) ;
#36665 = AXIS2_PLACEMENT_3D ( 'NONE', #22203, #53501, #68989 ) ;
#36666 = CONTEXT_DEPENDENT_SHAPE_REPRESENTATION ( #40408, #8653 ) ;
#36667 = CARTESIAN_POINT ( 'NONE',  ( -50.38034822888705833, 14.51481641465389671, 85.63106280517327207 ) ) ;
#36668 = VERTEX_POINT ( 'NONE', #65867 ) ;
#36669 = DIRECTION ( 'NONE',  ( -1.000000000000000000, 0.000000000000000000, 0.000000000000000000 ) ) ;
#36670 = ORIENTED_EDGE ( 'NONE', *, *, #49351, .F. ) ;
#36671 = CARTESIAN_POINT ( 'NONE',  ( 16.54503815046424009, 18.74197728628641002, 0.000000000000000000 ) ) ;
#36672 = AXIS2_PLACEMENT_3D ( 'NONE', #6309, #33047, #5948 ) ;
#36673 = CARTESIAN_POINT ( 'NONE',  ( 0.000000000000000000, 0.000000000000000000, 41.38025477438755928 ) ) ;
#36674 = CARTESIAN_POINT ( 'NONE',  ( -172.3127615181935823, 87.73358064377643473, 30.85409139483959606 ) ) ;
#36675 = CARTESIAN_POINT ( 'NONE',  ( 63.01563776193091826, 12.67277567978500308, -23.87614024170608218 ) ) ;
#36676 = PLANE ( 'NONE',  #10359 ) ;
#36677 = AXIS2_PLACEMENT_3D ( 'NONE', #52271, #62485, #41721 ) ;
#36678 = CARTESIAN_POINT ( 'NONE',  ( 447.3372781065083927, 395.0000000000043769, 91.05029585798419589 ) ) ;
#36679 = B_SPLINE_CURVE_WITH_KNOTS ( 'NONE', 3,
 ( #55208, #50293, #7027, #1400, #11588, #11953 ),
 .UNSPECIFIED., .F., .F.,
 ( 4, 2, 4 ),
 ( 0.01291313371729459203, 0.01525081363757311431, 0.01758849355785163660 ),
 .UNSPECIFIED. ) ;
#36680 = DIRECTION ( 'NONE',  ( -0.000000000000000000, -0.000000000000000000, -1.000000000000000000 ) ) ;
#36681 = VERTEX_POINT ( 'NONE', #18177 ) ;
#36682 = CARTESIAN_POINT ( 'NONE',  ( 110.2429982417149432, 29.99119854320847267, 56.45576479620100940 ) ) ;
#36683 = CARTESIAN_POINT ( 'NONE',  ( -120.1650841064593891, 44.02024060322521137, -10.72207681748146513 ) ) ;
#36684 = ORIENTED_EDGE ( 'NONE', *, *, #35835, .T. ) ;
#36685 = EDGE_CURVE ( 'NONE', #8520, #65221, #40159, .T. ) ;
#36686 = ORIENTED_EDGE ( 'NONE', *, *, #59946, .T. ) ;
#36687 = ADVANCED_FACE ( 'NONE', ( #22936 ), #66560, .T. ) ;
#36688 = CARTESIAN_POINT ( 'NONE',  ( 177.5852526894774712, 76.54518907282665907, 83.85689353362545262 ) ) ;
#36689 = VECTOR ( 'NONE', #61597, 999.9999999999998863 ) ;
#36690 =( NAMED_UNIT ( * ) SI_UNIT ( $, .STERADIAN. ) SOLID_ANGLE_UNIT ( ) );
#36691 = EDGE_CURVE ( 'NONE', #62726, #12932, #13427, .T. ) ;
#36692 = CARTESIAN_POINT ( 'NONE',  ( 125.2194818923508848, 188.0000000000000000, -23.09547038499562888 ) ) ;
#36693 = UNCERTAINTY_MEASURE_WITH_UNIT (LENGTH_MEASURE( 1.000000000000000082E-05 ), #37192, 'distance_accuracy_value', 'NONE');
#36694 = DIRECTION ( 'NONE',  ( -0.9639628606958550172, 0.2660368455666687892, 0.000000000000000000 ) ) ;
#36695 = DIRECTION ( 'NONE',  ( -0.000000000000000000, 1.000000000000000000, -0.000000000000000000 ) ) ;
#36696 = CARTESIAN_POINT ( 'NONE',  ( 74.62299871641508275, -5.461138973197948054, 0.000000000000000000 ) ) ;
#36697 = DIRECTION ( 'NONE',  ( 0.000000000000000000, 0.000000000000000000, 1.000000000000000000 ) ) ;
#36698 = CARTESIAN_POINT ( 'NONE',  ( 0.7145311798163349604, -9.237604307034033013, 2.857026868940023748E-16 ) ) ;
#36699 = CARTESIAN_POINT ( 'NONE',  ( 86.62931800182293784, 19.42108912189597447, -23.97701360844805407 ) ) ;
#36700 = CARTESIAN_POINT ( 'NONE',  ( 205.5004956747122264, 107.4493581495448069, -24.44922967293032201 ) ) ;
#36701 = CARTESIAN_POINT ( 'NONE',  ( 107.4892320395363186, 21.56923944770097634, -4.336110802034259137 ) ) ;
#36702 = CARTESIAN_POINT ( 'NONE',  ( 162.0812592823605200, 62.62783216273701470, 69.68866734599082235 ) ) ;
#36703 = EDGE_CURVE ( 'NONE', #23177, #15890, #34552, .T. ) ;
#36704 = ORIENTED_EDGE ( 'NONE', *, *, #49118, .F. ) ;
#36705 = EDGE_CURVE ( 'NONE', #4257, #19256, #24885, .T. ) ;
#36706 = CARTESIAN_POINT ( 'NONE',  ( 126.6266894765173703, 38.37986986668739320, 12.22883615118388079 ) ) ;
#36707 = FACE_OUTER_BOUND ( 'NONE', #52716, .T. ) ;
#36708 = LINE ( 'NONE', #30737, #35227 ) ;
#36709 = CARTESIAN_POINT ( 'NONE',  ( -109.0291978193666438, 37.49173305805086187, -72.64004148779659431 ) ) ;
#36710 = LINE ( 'NONE', #36356, #54279 ) ;
#36711 = CARTESIAN_POINT ( 'NONE',  ( -6.528484601666539433, 7.817818436116853675, 83.91048964419407241 ) ) ;
#36712 = ORIENTED_EDGE ( 'NONE', *, *, #54467, .T. ) ;
#36713 = LINE ( 'NONE', #42995, #41490 ) ;
#36714 = CARTESIAN_POINT ( 'NONE',  ( -62.56514071794335052, 16.82532503654672240, 64.66934574899191546 ) ) ;
#36715 = ORIENTED_EDGE ( 'NONE', *, *, #50885, .T. ) ;
#36716 = VECTOR ( 'NONE', #10269, 1000.000000000000000 ) ;
#36717 = EDGE_LOOP ( 'NONE', ( #36652, #49339, #39067, #7665 ) ) ;
#36718 = CARTESIAN_POINT ( 'NONE',  ( 32.28474208827732639, 8.601490596599902005, 93.49151023392415993 ) ) ;
#36719 = CARTESIAN_POINT ( 'NONE',  ( -177.5259994307673992, 92.16784265327254388, -75.14458197230979408 ) ) ;
#36720 = B_SPLINE_CURVE_WITH_KNOTS ( 'NONE', 3,
 ( #11297, #6384, #19365, #8125, #51391, #40474, #18685, #19023, #34868, #24318, #13068, #62276, #23617, #2165, #61919, #23275, #51038, #2506, #17991, #44722, #34531, #55614, #55972, #45054, #7784, #7082, #2851, #29237, #50348, #66199, #50682, #7443, #67564, #46095, #12711, #66540, #45407, #40822, #23956, #14094, #66890, #13405, #55262, #28539, #61594 ),
 .UNSPECIFIED., .F., .F.,
 ( 4, 2, 2, 2, 2, 2, 2, 2, 2, 2, 2, 2, 2, 1, 2, 2, 2, 2, 2, 2, 2, 2, 4 ),
 ( 0.02352719711393055566, 0.02499986300757020205, 0.02573619595439003566, 0.02647252890120986579, 0.02794519479484951566, 0.02941786068848916899, 0.03015419363530899219, 0.03089052658212881886, 0.03236319247576845137, 0.03309952542258825375, 0.03383585836940805613, 0.03530852426304766783, 0.03604485720986745634, 0.03678119015668723790, 0.03751752310350701947, 0.03825385605032680103, 0.03972652194396641273, 0.04119918783760601749, 0.04267185373124562919, 0.04340818667806543851, 0.04414451962488524783, 0.04561718551852483872, 0.04708985141216442960 ),
 .UNSPECIFIED. ) ;
#36721 = CARTESIAN_POINT ( 'NONE',  ( -42.36049017605959932, 61.90437280228238137, 170.0000000000000000 ) ) ;
#36722 = VERTEX_POINT ( 'NONE', #12382 ) ;
#36723 = VECTOR ( 'NONE', #69207, 999.9999999999998863 ) ;
#36724 = CARTESIAN_POINT ( 'NONE',  ( 22.25657943806483274, 7.801867731668604478, 94.99999999999866418 ) ) ;
#36725 = DIRECTION ( 'NONE',  ( -0.000000000000000000, 1.000000000000000000, -0.000000000000000000 ) ) ;
#36726 = CARTESIAN_POINT ( 'NONE',  ( 33.75639351246965703, 7.742023566824293823, -21.23742916720711449 ) ) ;
#36727 = CARTESIAN_POINT ( 'NONE',  ( 173.5836858989432301, 72.71885240881779566, -43.43828145153533171 ) ) ;
#36728 = AXIS2_PLACEMENT_3D ( 'NONE', #61361, #13184, #7903 ) ;
#36729 = CARTESIAN_POINT ( 'NONE',  ( 163.5430354047457229, 62.53125887746119105, 94.99999999999866418 ) ) ;
#36730 = CARTESIAN_POINT ( 'NONE',  ( 93.63037639125408873, 21.92981100938039773, 39.91368610796941852 ) ) ;
#36731 = CIRCLE ( 'NONE', #23281, 125.0000000000000000 ) ;
#36732 = VERTEX_POINT ( 'NONE', #18009 ) ;
#36733 = CARTESIAN_POINT ( 'NONE',  ( 0.06730325657896424341, -1.557442666625489025, 7.999999999999996447 ) ) ;
#36734 = CARTESIAN_POINT ( 'NONE',  ( 14.80205238535216772, 6.470775952815776222, 56.90826214576678410 ) ) ;
#36735 = CARTESIAN_POINT ( 'NONE',  ( 8.288696687633805738, 7.382586467017839382, 37.01382362586534924 ) ) ;
#36736 = CARTESIAN_POINT ( 'NONE',  ( 201.5987353083855567, 103.8544727311227120, 29.86444194458761814 ) ) ;
#36737 = CARTESIAN_POINT ( 'NONE',  ( 80.34841469379381351, 17.37275484083203381, 94.99999999999866418 ) ) ;
#36739 = VERTEX_POINT ( 'NONE', #24339 ) ;
#36738 = CARTESIAN_POINT ( 'NONE',  ( 24.34685647902980676, 70.88683439560453792, 41.38025477438755928 ) ) ;
#36740 = ORIENTED_EDGE ( 'NONE', *, *, #50893, .F. ) ;
#36741 = ORIENTED_EDGE ( 'NONE', *, *, #36474, .F. ) ;
#36742 = CARTESIAN_POINT ( 'NONE',  ( 114.6659427952415200, 32.10199811723106222, -64.19130057980802917 ) ) ;
#36743 = CARTESIAN_POINT ( 'NONE',  ( 0.000000000000000000, 0.000000000000000000, 0.000000000000000000 ) ) ;
#36744 = FACE_OUTER_BOUND ( 'NONE', #45434, .T. ) ;
#36745 = CARTESIAN_POINT ( 'NONE',  ( -452.6627218934913230, 177.8591479523843475, -111.4497041420117966 ) ) ;
#36746 = CARTESIAN_POINT ( 'NONE',  ( -125.4433371161043880, 46.19736518073189302, 72.46449846362084202 ) ) ;
#36747 = CARTESIAN_POINT ( 'NONE',  ( 154.0401952541423043, 55.03227529428313858, -63.79514857056523169 ) ) ;
#36748 = CARTESIAN_POINT ( 'NONE',  ( 22.99481266947290337, 7.846456081397400695, -94.58791541915923062 ) ) ;
#36749 = CARTESIAN_POINT ( 'NONE',  ( -155.7495771807047902, 69.65980221699321362, -46.50072862889067693 ) ) ;
#36750 = ORIENTED_EDGE ( 'NONE', *, *, #22144, .T. ) ;
#36751 = EDGE_LOOP ( 'NONE', ( #6232, #65676, #26456, #4894 ) ) ;
#36752 = CARTESIAN_POINT ( 'NONE',  ( 69.35866309798979046, 15.27376159675663558, -12.36654855831349842 ) ) ;
#36753 = DIRECTION ( 'NONE',  ( 0.000000000000000000, 0.000000000000000000, -1.000000000000000000 ) ) ;
#36754 = CARTESIAN_POINT ( 'NONE',  ( 160.5141379054754225, 60.05651755415394177, 70.62330748442225570 ) ) ;
#36755 = CARTESIAN_POINT ( 'NONE',  ( 116.5100763992442978, 33.01539745157282368, -12.45056777525001301 ) ) ;
#36756 = EDGE_CURVE ( 'NONE', #16484, #63871, #29418, .T. ) ;
#36758 = CARTESIAN_POINT ( 'NONE',  ( 34.76618902119821541, -54.93755186520709799, 41.38025477438755928 ) ) ;
#36757 = CIRCLE ( 'NONE', #27752, 30.00000000000000000 ) ;
#36759 = CARTESIAN_POINT ( 'NONE',  ( 18.21423326326598158, 6.590134686181414736, 44.62829782856979222 ) ) ;
#36760 = CARTESIAN_POINT ( 'NONE',  ( 74.01791526339570737, -12.16185512414842051, 43.58025477438756923 ) ) ;
#36761 = ORIENTED_EDGE ( 'NONE', *, *, #498, .F. ) ;
#36762 = ORIENTED_EDGE ( 'NONE', *, *, #6341, .T. ) ;
#36763 = ADVANCED_FACE ( 'NONE', ( #24683 ), #68281, .T. ) ;
#36764 = ORIENTED_EDGE ( 'NONE', *, *, #66672, .T. ) ;
#36765 = AXIS2_PLACEMENT_3D ( 'NONE', #18687, #2167, #23619 ) ;
#36766 = CARTESIAN_POINT ( 'NONE',  ( 0.000000000000000000, 0.000000000000000000, 41.38025477438755928 ) ) ;
#36767 = EDGE_CURVE ( 'NONE', #8782, #39218, #51749, .T. ) ;
#36768 = CARTESIAN_POINT ( 'NONE',  ( 36.30999198706538778, 9.040534725358947199, -36.28248531905617114 ) ) ;
#36769 = CARTESIAN_POINT ( 'NONE',  ( 105.1608565259479633, -21.96391085485758410, -1.300312621757638620 ) ) ;
#36770 = VECTOR ( 'NONE', #57032, 1000.000000000000000 ) ;
#36771 = EDGE_CURVE ( 'NONE', #69259, #49668, #17711, .T. ) ;
#36772 = CARTESIAN_POINT ( 'NONE',  ( 169.9999999999999716, -6.319444444444440201, 0.000000000000000000 ) ) ;
#36773 = CARTESIAN_POINT ( 'NONE',  ( 197.8598785550297237, 99.02620879292952338, 60.45626783609857569 ) ) ;
#36774 = ORIENTED_EDGE ( 'NONE', *, *, #27435, .T. ) ;
#36775 = VECTOR ( 'NONE', #15262, 1000.000000000000114 ) ;
#36776 = FACE_OUTER_BOUND ( 'NONE', #42215, .T. ) ;
#36777 = FACE_OUTER_BOUND ( 'NONE', #62469, .T. ) ;
#36778 = CIRCLE ( 'NONE', #50290, 5.000000000000000888 ) ;
#36779 = FACE_OUTER_BOUND ( 'NONE', #10357, .T. ) ;
#36780 = DIRECTION ( 'NONE',  ( -1.000000000000000000, 0.000000000000000000, 0.000000000000000000 ) ) ;
#36781 = CARTESIAN_POINT ( 'NONE',  ( -118.8689810167775960, 42.03922634358562505, 8.635105111016807555 ) ) ;
#36782 = CARTESIAN_POINT ( 'NONE',  ( 9.850262805259839993, 200.0000000000000000, -1.724042536399416070 ) ) ;
#36783 = DIRECTION ( 'NONE',  ( 0.000000000000000000, 0.000000000000000000, -1.000000000000000000 ) ) ;
#36784 = CARTESIAN_POINT ( 'NONE',  ( 34.76618902119820831, -54.93755186520709799, 3.061616997868437868E-16 ) ) ;
#36785 = CARTESIAN_POINT ( 'NONE',  ( 14.08810621383467243, 7.458732232275136376, 3.361252658025919438 ) ) ;
#36786 = AXIS2_PLACEMENT_3D ( 'NONE', #36743, #15284, #62438 ) ;
#36787 = EDGE_CURVE ( 'NONE', #27257, #46646, #55445, .T. ) ;
#36788 = ORIENTED_EDGE ( 'NONE', *, *, #69466, .T. ) ;
#36789 = CARTESIAN_POINT ( 'NONE',  ( 188.4904153916303642, 86.42965364612517476, 8.744626016292592396 ) ) ;
#36790 = APPLICATION_PROTOCOL_DEFINITION ( 'draft international standard', 'automotive_design', 1998, #32296 ) ;
#36791 = CARTESIAN_POINT ( 'NONE',  ( 180.2473887773227545, 77.76029175826236894, 44.30859410551141764 ) ) ;
#36792 = FACE_OUTER_BOUND ( 'NONE', #49623, .T. ) ;
#36793 = CARTESIAN_POINT ( 'NONE',  ( -106.4728934171454142, 36.10295170132725673, -48.73770635309175248 ) ) ;
#36794 = DIRECTION ( 'NONE',  ( -0.000000000000000000, -0.000000000000000000, -1.000000000000000000 ) ) ;
#36795 = ORIENTED_EDGE ( 'NONE', *, *, #39384, .F. ) ;
#36796 = VERTEX_POINT ( 'NONE', #48169 ) ;
#36797 = DIRECTION ( 'NONE',  ( 0.000000000000000000, 0.000000000000000000, -1.000000000000000000 ) ) ;
#36798 = CARTESIAN_POINT ( 'NONE',  ( 173.5922027797725207, 71.35194229497426477, 90.90255056565294467 ) ) ;
#36799 = EDGE_LOOP ( 'NONE', ( #27799, #65586, #54852, #53301 ) ) ;
#36800 = CARTESIAN_POINT ( 'NONE',  ( 115.2288739107204805, 31.25773204386716486, 58.34775827273530524 ) ) ;
#36801 = VERTEX_POINT ( 'NONE', #63689 ) ;
#36802 = FACE_BOUND ( 'NONE', #15488, .T. ) ;
#36803 = CARTESIAN_POINT ( 'NONE',  ( 132.0440382699655117, 40.34028297386453232, 29.71835426369820965 ) ) ;
#36804 = CARTESIAN_POINT ( 'NONE',  ( 47.73902449248994628, 57.85799893277891215, 170.0000000000000000 ) ) ;
#36805 = CARTESIAN_POINT ( 'NONE',  ( -98.67723517640904163, 30.98797878696538888, 44.60132663403577169 ) ) ;
#36806 = CARTESIAN_POINT ( 'NONE',  ( 93.71772995179814814, 21.96265635001559247, -40.85830305015011277 ) ) ;
#36808 = VERTEX_POINT ( 'NONE', #43242 ) ;
#36807 = DIRECTION ( 'NONE',  ( -1.000000000000000000, 0.000000000000000000, 0.000000000000000000 ) ) ;
#36809 = VECTOR ( 'NONE', #53040, 1000.000000000000000 ) ;
#36810 = CYLINDRICAL_SURFACE ( 'NONE', #15989, 7.500000000000013323 ) ;
#36811 = ORIENTED_EDGE ( 'NONE', *, *, #6745, .T. ) ;
#36812 = ORIENTED_EDGE ( 'NONE', *, *, #11660, .F. ) ;
#36813 = AXIS2_PLACEMENT_3D ( 'NONE', #30121, #67405, #24150 ) ;
#36814 = CARTESIAN_POINT ( 'NONE',  ( -118.3927673406137160, 41.74929850983303226, -15.33123327190856600 ) ) ;
#36815 = LINE ( 'NONE', #13374, #22395 ) ;
#36816 =( REPRESENTATION_RELATIONSHIP ('NONE','NONE', #40274, #35767 ) REPRESENTATION_RELATIONSHIP_WITH_TRANSFORMATION ( #18191 )SHAPE_REPRESENTATION_RELATIONSHIP( ) );
#36817 = CARTESIAN_POINT ( 'NONE',  ( -180.5231752320738110, 95.76423526868921954, -14.11972369233568436 ) ) ;
#36818 = VECTOR ( 'NONE', #54759, 1000.000000000000000 ) ;
#36820 = VERTEX_POINT ( 'NONE', #32706 ) ;
#36819 = CARTESIAN_POINT ( 'NONE',  ( -149.2910611247327779, 63.99625741915655652, -34.81283053149194728 ) ) ;
#36821 = CARTESIAN_POINT ( 'NONE',  ( 60.40531521312254171, 13.11276739283242243, 3.433157306431154687 ) ) ;
#36822 = LINE ( 'NONE', #14665, #36230 ) ;
#36823 = VECTOR ( 'NONE', #56805, 1000.000000000000114 ) ;
#36824 = ORIENTED_EDGE ( 'NONE', *, *, #49458, .T. ) ;
#36825 = EDGE_CURVE ( 'NONE', #52414, #27866, #52945, .T. ) ;
#36826 = CARTESIAN_POINT ( 'NONE',  ( -60.13226458141418362, 16.10241298991027037, -10.34831921288341583 ) ) ;
#36827 = CIRCLE ( 'NONE', #22211, 5.000000000000004441 ) ;
#36828 = CARTESIAN_POINT ( 'NONE',  ( -132.8257891167039304, 52.46553896898736014, -66.38325077981791367 ) ) ;
#36829 = CARTESIAN_POINT ( 'NONE',  ( -61.29635759142615115, 21.66977272663494958, 43.58025477438756923 ) ) ;
#36830 = CARTESIAN_POINT ( 'NONE',  ( -94.79534239005252516, 29.13842790650044634, 10.63132434853593367 ) ) ;
#36831 = CARTESIAN_POINT ( 'NONE',  ( -99.31850058233800382, 31.30166762705808381, -62.46462738374896873 ) ) ;
#36832 = EDGE_LOOP ( 'NONE', ( #66802, #47574, #51803, #22279 ) ) ;
#36833 = ORIENTED_EDGE ( 'NONE', *, *, #3415, .F. ) ;
#36834 = CARTESIAN_POINT ( 'NONE',  ( 181.0840389613909736, 78.60582251573005408, -63.06960825634327961 ) ) ;
#36835 = CARTESIAN_POINT ( 'NONE',  ( -166.9969673948021409, 80.56076768517783648, -37.87432764174864985 ) ) ;
#36836 = DIRECTION ( 'NONE',  ( 0.000000000000000000, 0.000000000000000000, 1.000000000000000000 ) ) ;
#36837 = CARTESIAN_POINT ( 'NONE',  ( 110.2429982417149574, 29.99119854320844425, -62.76698815611734972 ) ) ;
#36838 = CARTESIAN_POINT ( 'NONE',  ( -77.71801202538874520, 23.03755222122951096, 45.37301624558984514 ) ) ;
#36839 = CARTESIAN_POINT ( 'NONE',  ( 86.15410276028862313, 19.25894675708892123, 29.71208757247930521 ) ) ;
#36840 = CARTESIAN_POINT ( 'NONE',  ( 68.94309019697858787, 15.16533147648755175, -38.59916606691003693 ) ) ;
#36841 = CARTESIAN_POINT ( 'NONE',  ( -122.8202784017355498, 45.69728649588467562, 44.96525387181218747 ) ) ;
#36842 = PLANE ( 'NONE',  #58757 ) ;
#36843 = VERTEX_POINT ( 'NONE', #65067 ) ;
#36844 = LINE ( 'NONE', #58283, #8578 ) ;
#36845 = ADVANCED_FACE ( 'NONE', ( #16866 ), #700, .T. ) ;
#36846 = ORIENTED_EDGE ( 'NONE', *, *, #3203, .F. ) ;
#36847 = CARTESIAN_POINT ( 'NONE',  ( -35.38560449531985341, 10.27249159032101744, 4.489560872237628786 ) ) ;
#36848 = CARTESIAN_POINT ( 'NONE',  ( 79.18180043629686793, 18.06526831600450222, 63.03804907646694033 ) ) ;
#36849 = CARTESIAN_POINT ( 'NONE',  ( 3.678442866637813759E-12, -65.13282190615278466, 5.000000000000000000 ) ) ;
#36850 = CARTESIAN_POINT ( 'NONE',  ( 155.7277429502854034, 56.30804678861340307, -24.08774153568633380 ) ) ;
#36851 = CARTESIAN_POINT ( 'NONE',  ( 34.83823433017390414, 8.871835168107976344, 4.597148557001253799 ) ) ;
#36852 = DIRECTION ( 'NONE',  ( 0.9749279121818227312, 0.2225209339563184729, 5.102127870520021228E-18 ) ) ;
#36853 = CARTESIAN_POINT ( 'NONE',  ( 32.56927464314651388, 7.618924692399909659, -73.06680367152966937 ) ) ;
#36854 = CARTESIAN_POINT ( 'NONE',  ( -102.2801239173131194, 33.91021738430207932, -61.85912785543958847 ) ) ;
#36855 = EDGE_CURVE ( 'NONE', #57935, #13481, #68943, .T. ) ;
#36856 = CARTESIAN_POINT ( 'NONE',  ( -38.68632430131781064, 11.91908191268691297, -14.02620273824548924 ) ) ;
#36857 = ORIENTED_EDGE ( 'NONE', *, *, #5061, .F. ) ;
#36858 = FACE_OUTER_BOUND ( 'NONE', #24668, .T. ) ;
#36859 = ORIENTED_EDGE ( 'NONE', *, *, #28252, .T. ) ;
#36860 = PLANE ( 'NONE',  #54227 ) ;
#36861 = CARTESIAN_POINT ( 'NONE',  ( -39.40355473380300566, -43.02169567653766080, 27.58472369436602634 ) ) ;
#36862 = CARTESIAN_POINT ( 'NONE',  ( -24.41864932425147927, 8.543938959778817122, 13.52232210049978356 ) ) ;
#36863 = CARTESIAN_POINT ( 'NONE',  ( -440.1146514826278349, 394.9999999999998295, 101.0022254471246441 ) ) ;
#36864 = CARTESIAN_POINT ( 'NONE',  ( -12.39701069459754201, 7.231688578592716077, -75.72825898634536657 ) ) ;
#36865 = CARTESIAN_POINT ( 'NONE',  ( -98.46684543088103680, 30.88557736720388647, -9.207280559787971441 ) ) ;
#36866 = AXIS2_PLACEMENT_3D ( 'NONE', #699, #69299, #36953 ) ;
#36867 = CARTESIAN_POINT ( 'NONE',  ( 151.1827182658834090, 54.16800928478852484, -47.74454161914079009 ) ) ;
#36868 = EDGE_CURVE ( 'NONE', #58577, #24108, #34977, .T. ) ;
#36869 = AXIS2_PLACEMENT_3D ( 'NONE', #20178, #4006, #19837 ) ;
#36870 = ORIENTED_EDGE ( 'NONE', *, *, #60674, .T. ) ;
#36871 = CARTESIAN_POINT ( 'NONE',  ( 403.0071894358308100, 629.9915846175144907, 569.0068267248720986 ) ) ;
#36872 = CYLINDRICAL_SURFACE ( 'NONE', #52045, 5.000000000000004441 ) ;
#36874 = ADVANCED_FACE ( 'NONE', ( #10898 ), #64028, .T. ) ;
#36873 = CARTESIAN_POINT ( 'NONE',  ( 173.6737675136087660, 72.80308721038097985, -18.07488780512645832 ) ) ;
#36875 = EDGE_CURVE ( 'NONE', #39681, #10970, #61183, .T. ) ;
#36876 = CARTESIAN_POINT ( 'NONE',  ( -109.6657532478350561, 37.84376708859252858, 63.53280748219179941 ) ) ;
#36877 = CONICAL_SURFACE ( 'NONE', #6537, 74.95140232871122521, 0.8777644062502172329 ) ;
#36878 = CARTESIAN_POINT ( 'NONE',  ( -442.6627218934913230, 399.9999999999997726, 108.5502958579881891 ) ) ;
#36879 = ORIENTED_EDGE ( 'NONE', *, *, #42666, .T. ) ;
#36880 = PLANE ( 'NONE',  #22287 ) ;
#36881 = CARTESIAN_POINT ( 'NONE',  ( 91.51282003084290295, 21.14522045960332619, 69.76978587635888118 ) ) ;
#36882 = FILL_AREA_STYLE ('',( #15422 ) ) ;
#36883 = CARTESIAN_POINT ( 'NONE',  ( -156.9664270383552491, 70.77351443782143292, 91.10669583694630091 ) ) ;
#36884 = CARTESIAN_POINT ( 'NONE',  ( 141.0804878838241336, 45.96076546397619467, 39.09591246831315914 ) ) ;
#36885 = VERTEX_POINT ( 'NONE', #34469 ) ;
#36886 = LINE ( 'NONE', #69224, #43556 ) ;
#36887 = DIRECTION ( 'NONE',  ( 0.3513748240813435175, -0.9362348706397369824, 0.000000000000000000 ) ) ;
#36888 = CARTESIAN_POINT ( 'NONE',  ( 188.2086267457325448, 87.61890531228286250, 34.44826965832049126 ) ) ;
#36889 = CARTESIAN_POINT ( 'NONE',  ( 162.7963212667073662, 63.21900188423072819, 15.35118721056019986 ) ) ;
#36890 = CARTESIAN_POINT ( 'NONE',  ( -100.4440683050664518, 32.98184228837415333, 45.30557044946138490 ) ) ;
#36891 = EDGE_LOOP ( 'NONE', ( #64912, #19969, #62362, #16030 ) ) ;
#36892 = CARTESIAN_POINT ( 'NONE',  ( 173.6700117628886346, 72.79957362875116189, 64.82362119438116110 ) ) ;
#36893 = ORIENTED_EDGE ( 'NONE', *, *, #6501, .T. ) ;
#36894 = CARTESIAN_POINT ( 'NONE',  ( -108.9452487746634120, 36.29752968355630571, -45.99127851335813943 ) ) ;
#36895 = DIRECTION ( 'NONE',  ( 0.000000000000000000, -1.000000000000000000, 0.000000000000000000 ) ) ;
#36896 = DIRECTION ( 'NONE',  ( -0.000000000000000000, 1.000000000000000000, -0.000000000000000000 ) ) ;
#36898 = EDGE_LOOP ( 'NONE', ( #28939, #48610, #36105, #68039 ) ) ;
#36897 = DIRECTION ( 'NONE',  ( 0.000000000000000000, 0.000000000000000000, 1.000000000000000000 ) ) ;
#36899 = CARTESIAN_POINT ( 'NONE',  ( -178.5835577246388368, 93.42126246260829703, 33.17678452161792535 ) ) ;
#36900 = CARTESIAN_POINT ( 'NONE',  ( 133.8566784816069344, -170.0000000000000000, -24.17876034193199786 ) ) ;
#36901 = CARTESIAN_POINT ( 'NONE',  ( 0.000000000000000000, 0.000000000000000000, 43.58025477438756212 ) ) ;
#36902 = ORIENTED_EDGE ( 'NONE', *, *, #35171, .F. ) ;
#36903 = EDGE_CURVE ( 'NONE', #30795, #30237, #49560, .T. ) ;
#36904 = CARTESIAN_POINT ( 'NONE',  ( 149.0250918491436778, 6.000000000000000000, -9.435653166495526989 ) ) ;
#36905 = AXIS2_PLACEMENT_3D ( 'NONE', #26998, #618, #48428 ) ;
#36906 = EDGE_CURVE ( 'NONE', #44801, #32676, #56309, .T. ) ;
#36907 = CARTESIAN_POINT ( 'NONE',  ( 136.9798231265810102, 43.34196232604178789, 57.02028350268891899 ) ) ;
#36908 = CARTESIAN_POINT ( 'NONE',  ( -173.5372686962701039, 89.10569330281725797, 30.82169460664102800 ) ) ;
#36909 = CARTESIAN_POINT ( 'NONE',  ( 152.6560521232695180, 54.00248515670892857, 57.99803634713506284 ) ) ;
#36910 = CARTESIAN_POINT ( 'NONE',  ( 94.11733320392094981, 23.18939451097131865, 36.71840950062001241 ) ) ;
#36911 = ORIENTED_EDGE ( 'NONE', *, *, #12412, .F. ) ;
#36912 = AXIS2_PLACEMENT_3D ( 'NONE', #46299, #45269, #24529 ) ;
#36913 = CARTESIAN_POINT ( 'NONE',  ( 40.38132770291768736, 9.553709436640065888, 18.02098113922875555 ) ) ;
#36914 = VERTEX_POINT ( 'NONE', #11945 ) ;
#36915 = CARTESIAN_POINT ( 'NONE',  ( 152.1381498073140790, 54.87048121475570639, -22.07591650116782844 ) ) ;
#36916 = PRESENTATION_LAYER_ASSIGNMENT (  '', '', ( #52623 ) ) ;
#36917 = CARTESIAN_POINT ( 'NONE',  ( 206.2957331585308793, 110.2946564621822887, -24.35451595762442167 ) ) ;
#36918 = CARTESIAN_POINT ( 'NONE',  ( -71.96466849523078224, 21.15771699336999845, 170.0000000000000000 ) ) ;
#36919 = FACE_OUTER_BOUND ( 'NONE', #56908, .T. ) ;
#36920 = CARTESIAN_POINT ( 'NONE',  ( 64.66528157600511406, 13.06122252980780019, 83.67837878186749379 ) ) ;
#36921 = DIRECTION ( 'NONE',  ( 0.000000000000000000, 0.000000000000000000, 1.000000000000000000 ) ) ;
#36922 = EDGE_CURVE ( 'NONE', #3968, #69309, #28474, .T. ) ;
#36923 = DIRECTION ( 'NONE',  ( 1.000000000000000000, 0.000000000000000000, 0.000000000000000000 ) ) ;
#36924 = FACE_OUTER_BOUND ( 'NONE', #32974, .T. ) ;
#36925 = ADVANCED_FACE ( 'NONE', ( #39040 ), #60130, .T. ) ;
#36926 = ORIENTED_EDGE ( 'NONE', *, *, #36386, .F. ) ;
#36927 = LINE ( 'NONE', #30618, #45364 ) ;
#36928 = ORIENTED_EDGE ( 'NONE', *, *, #37390, .F. ) ;
#36929 = CARTESIAN_POINT ( 'NONE',  ( -75.00636493611887090, 22.03142602679958983, 71.32676556850506699 ) ) ;
#36930 = CARTESIAN_POINT ( 'NONE',  ( 205.0999694062793424, 106.8955893716605061, -78.17048162308529413 ) ) ;
#36931 = EDGE_CURVE ( 'NONE', #60956, #69323, #10096, .T. ) ;
#36932 = CARTESIAN_POINT ( 'NONE',  ( 40.38495044702529668, 9.554194848483446023, -23.72658219154430626 ) ) ;
#36933 = DIRECTION ( 'NONE',  ( -1.000000000000000000, -0.000000000000000000, -0.000000000000000000 ) ) ;
#36934 = LINE ( 'NONE', #679, #822 ) ;
#36935 = CARTESIAN_POINT ( 'NONE',  ( 22.89270809252618832, 7.840160460323052583, 39.93075722470221933 ) ) ;
#36936 = EDGE_CURVE ( 'NONE', #67695, #4696, #31604, .T. ) ;
#36937 = CARTESIAN_POINT ( 'NONE',  ( 447.3372781065085633, 399.9999999999998863, 78.55029585798817493 ) ) ;
#36938 = EDGE_LOOP ( 'NONE', ( #55387, #3427, #38903, #29311 ) ) ;
#36939 = CARTESIAN_POINT ( 'NONE',  ( -71.59086462055189770, 19.75139532313339430, 62.26276460702656124 ) ) ;
#36940 = CARTESIAN_POINT ( 'NONE',  ( 203.0745197111477580, 104.1448368405267786, -90.18520043603034253 ) ) ;
#36941 = ORIENTED_EDGE ( 'NONE', *, *, #31145, .T. ) ;
#36942 = VERTEX_POINT ( 'NONE', #12299 ) ;
#36943 = CARTESIAN_POINT ( 'NONE',  ( -156.4960819023050931, 70.34114605623871341, 40.99531223057345386 ) ) ;
#36944 = CARTESIAN_POINT ( 'NONE',  ( 55.90910788310614521, 11.13585330978401267, -40.77322039613591897 ) ) ;
#36945 = FACE_OUTER_BOUND ( 'NONE', #21857, .T. ) ;
#36946 = CARTESIAN_POINT ( 'NONE',  ( -149.5074843970971017, 64.17983161892348676, 3.876270649435373361 ) ) ;
#36947 = VERTEX_POINT ( 'NONE', #12652 ) ;
#36948 = EDGE_CURVE ( 'NONE', #38815, #2018, #61533, .T. ) ;
#36949 = EDGE_CURVE ( 'NONE', #5435, #18335, #50287, .T. ) ;
#36950 = EDGE_CURVE ( 'NONE', #20231, #55364, #19245, .T. ) ;
#36951 = LINE ( 'NONE', #26738, #43524 ) ;
#36952 = EDGE_LOOP ( 'NONE', ( #48614, #58773, #29285, #63813 ) ) ;
#36953 = DIRECTION ( 'NONE',  ( 1.000000000000000000, 0.000000000000000000, 0.000000000000000000 ) ) ;
#36954 = CARTESIAN_POINT ( 'NONE',  ( 187.3988733513474756, 86.72376876819507174, -93.34304573699913021 ) ) ;
#36955 = DIRECTION ( 'NONE',  ( -0.000000000000000000, 1.000000000000000000, -0.000000000000000000 ) ) ;
#36956 = DIRECTION ( 'NONE',  ( -1.000000000000000000, 0.000000000000000000, 0.000000000000000000 ) ) ;
#36957 = ADVANCED_FACE ( 'NONE', ( #29178 ), #2441, .F. ) ;
#36958 = CARTESIAN_POINT ( 'NONE',  ( 76.57571471437145760, 10.00000000000000000, -30.00000000000000000 ) ) ;
#36959 = PLANE ( 'NONE',  #26049 ) ;
#36960 = VERTEX_POINT ( 'NONE', #6670 ) ;
#36961 = B_SPLINE_CURVE_WITH_KNOTS ( 'NONE', 3,
 ( #58253, #51944, #9044, #10069 ),
 .UNSPECIFIED., .F., .F.,
 ( 4, 4 ),
 ( 0.1259919275528361138, 0.1829744153748754099 ),
 .UNSPECIFIED. ) ;
#36962 = CIRCLE ( 'NONE', #65179, 2.999999999999999112 ) ;
#36963 = AXIS2_PLACEMENT_3D ( 'NONE', #34991, #56433, #56794 ) ;
#36964 = VERTEX_POINT ( 'NONE', #49215 ) ;
#36965 = DIRECTION ( 'NONE',  ( -0.000000000000000000, -0.000000000000000000, -1.000000000000000000 ) ) ;
#36966 = CARTESIAN_POINT ( 'NONE',  ( -133.1441247387262194, 52.69302668368034404, 93.75700809079965836 ) ) ;
#36967 = CARTESIAN_POINT ( 'NONE',  ( 37.45439421541016145, 9.177432671831368793, -62.70490429592918957 ) ) ;
#36968 = DIRECTION ( 'NONE',  ( 0.000000000000000000, 0.000000000000000000, 1.000000000000000000 ) ) ;
#36969 = CARTESIAN_POINT ( 'NONE',  ( 69.08240197259638649, 14.16210831900842315, 32.89646892813778578 ) ) ;
#36970 = CARTESIAN_POINT ( 'NONE',  ( 20.10890210143426771, 7.684797874382650384, 85.06464190967132311 ) ) ;
#36971 = AXIS2_PLACEMENT_3D ( 'NONE', #2751, #49522, #1357 ) ;
#36972 = EDGE_LOOP ( 'NONE', ( #12390, #36335, #41328, #16054 ) ) ;
#36973 = CARTESIAN_POINT ( 'NONE',  ( -20.63749999999999929, 0.000000000000000000, -21.02500000000000213 ) ) ;
#36974 = CARTESIAN_POINT ( 'NONE',  ( -97.85576954355161661, 30.58918648956189656, 70.93880484806753373 ) ) ;
#36975 = ORIENTED_EDGE ( 'NONE', *, *, #66483, .T. ) ;
#36976 = CARTESIAN_POINT ( 'NONE',  ( -82.32931163805226049, 23.75065981441938234, 4.524469639083367412 ) ) ;
#36977 = VERTEX_POINT ( 'NONE', #50623 ) ;
#36978 = ORIENTED_EDGE ( 'NONE', *, *, #50356, .T. ) ;
#36979 = ORIENTED_EDGE ( 'NONE', *, *, #19586, .T. ) ;
#36980 = CARTESIAN_POINT ( 'NONE',  ( -118.4470345550925856, 42.96051736048242731, 10.23307076808440463 ) ) ;
#36981 = CARTESIAN_POINT ( 'NONE',  ( -180.5231752320737542, 95.76423526868920533, 66.41392807905532436 ) ) ;
#36982 = CARTESIAN_POINT ( 'NONE',  ( 127.2397149628677653, 37.56999625068104365, 67.42304229148038530 ) ) ;
#36983 = ORIENTED_EDGE ( 'NONE', *, *, #65385, .F. ) ;
#36984 = CARTESIAN_POINT ( 'NONE',  ( -29.23666642776608526, 9.240073959287249394, 84.22891760168137409 ) ) ;
#36985 = ADVANCED_FACE ( 'NONE', ( #28119 ), #17926, .F. ) ;
#36986 = CARTESIAN_POINT ( 'NONE',  ( 151.6192474229129346, 53.24103268919209597, 32.21058103104000025 ) ) ;
#36987 = CARTESIAN_POINT ( 'NONE',  ( -452.6627218934860934, 395.0000000000064801, -133.9497041420121377 ) ) ;
#36988 = CARTESIAN_POINT ( 'NONE',  ( 106.6228877857910646, 27.24245963308693064, -36.83655804471349171 ) ) ;
#36989 = CARTESIAN_POINT ( 'NONE',  ( 139.6150621148398159, 46.20856238844173447, -65.53656864805886073 ) ) ;
#36990 = CARTESIAN_POINT ( 'NONE',  ( 209.9518228411288874, 20.00000000000003197, 31.43423095485942298 ) ) ;
#36991 = EDGE_LOOP ( 'NONE', ( #53141, #25527, #43933, #22855 ) ) ;
#36992 = DIRECTION ( 'NONE',  ( -0.08963930890344089242, 0.9959742939952384022, 5.102127870520021228E-18 ) ) ;
#36993 = CARTESIAN_POINT ( 'NONE',  ( -2.309976723937614107, 7.903938623646865835, -9.369346954796188953 ) ) ;
#36994 = CARTESIAN_POINT ( 'NONE',  ( -452.6627218934912094, 399.9999999999998295, 113.5502958579882602 ) ) ;
#36995 = CARTESIAN_POINT ( 'NONE',  ( -119.5404913382140251, 43.63271406506960659, -46.40773658427427506 ) ) ;
#36996 = CARTESIAN_POINT ( 'NONE',  ( -85.10909119100209352, 25.97025675005451006, 7.201605039916894491 ) ) ;
#36997 = CARTESIAN_POINT ( 'NONE',  ( -2.700000000000004619, 0.000000000000000000, 0.000000000000000000 ) ) ;
#36998 = CARTESIAN_POINT ( 'NONE',  ( -156.7487895666416762, 70.57327586518564999, 9.403214650218792769 ) ) ;
#36999 = EDGE_CURVE ( 'NONE', #41404, #48198, #65418, .T. ) ;
#37000 = CARTESIAN_POINT ( 'NONE',  ( 197.2002799314678896, 98.19982998998082735, 89.90084543270276640 ) ) ;
#37001 = CARTESIAN_POINT ( 'NONE',  ( 69.50572373348799715, 14.27208627753790360, 14.25933825401109800 ) ) ;
#37002 = CARTESIAN_POINT ( 'NONE',  ( -61.29635759142615115, 21.66977272663494958, 0.000000000000000000 ) ) ;
#37003 = CARTESIAN_POINT ( 'NONE',  ( -107.0584934212648704, 35.27493744466470815, 43.82066438551851917 ) ) ;
#37004 = ORIENTED_EDGE ( 'NONE', *, *, #39922, .T. ) ;
#37005 = ITEM_DEFINED_TRANSFORMATION ( 'NONE', 'NONE', #66925,  #66832 ) ;
#37006 = CARTESIAN_POINT ( 'NONE',  ( -62.53610861913121255, 17.86800032500430646, 90.91069339059835386 ) ) ;
#37007 = ORIENTED_EDGE ( 'NONE', *, *, #29864, .T. ) ;
#37008 = EDGE_CURVE ( 'NONE', #46955, #20487, #16003, .T. ) ;
#37009 = CARTESIAN_POINT ( 'NONE',  ( -45.99287096254393248, -23.53639463186987868, 26.66469066592268078 ) ) ;
#37010 = VERTEX_POINT ( 'NONE', #52602 ) ;
#37011 = CIRCLE ( 'NONE', #44897, 242.4895526022646379 ) ;
#37012 = EDGE_CURVE ( 'NONE', #10653, #3542, #36096, .T. ) ;
#37013 = CARTESIAN_POINT ( 'NONE',  ( -46.66904755831212981, -15.55634918610397222, 85.00100000000000477 ) ) ;
#37014 = CARTESIAN_POINT ( 'NONE',  ( 0.000000000000000000, 0.000000000000000000, 41.38025477438755928 ) ) ;
#37015 = CARTESIAN_POINT ( 'NONE',  ( -173.1211646369891355, 88.63826465341151106, 30.82169460664101734 ) ) ;
#37016 = CARTESIAN_POINT ( 'NONE',  ( 311.9975424824652350, 20.00000000000003197, 380.0000000000001137 ) ) ;
#37017 = EDGE_CURVE ( 'NONE', #54100, #57391, #67567, .T. ) ;
#37019 = LINE ( 'NONE', #31732, #18263 ) ;
#37018 = CIRCLE ( 'NONE', #50479, 25.12245591505646303 ) ;
#37020 = CARTESIAN_POINT ( 'NONE',  ( -50.14440374537738876, 14.45628984983895648, -63.86889621594647792 ) ) ;
#37021 = LINE ( 'NONE', #53523, #63344 ) ;
#37022 = CARTESIAN_POINT ( 'NONE',  ( -120.6739978760426197, 44.33795494230365364, -10.17821021773952594 ) ) ;
#37023 = VERTEX_POINT ( 'NONE', #9357 ) ;
#37024 = ORIENTED_EDGE ( 'NONE', *, *, #55358, .T. ) ;
#37025 = CARTESIAN_POINT ( 'NONE',  ( 174.6728071617951059, 73.74298290599254813, 94.40752414145283922 ) ) ;
#37026 = CARTESIAN_POINT ( 'NONE',  ( 412.3372781065087906, 400.0000000000065938, -111.4497041420121093 ) ) ;
#37027 = DIRECTION ( 'NONE',  ( -0.000000000000000000, -0.000000000000000000, -1.000000000000000000 ) ) ;
#37028 = AXIS2_PLACEMENT_3D ( 'NONE', #53322, #31213, #21670 ) ;
#37029 = FACE_OUTER_BOUND ( 'NONE', #53468, .T. ) ;
#37030 = EDGE_CURVE ( 'NONE', #37226, #43800, #69468, .T. ) ;
#37031 = FACE_OUTER_BOUND ( 'NONE', #49230, .T. ) ;
#37032 = CARTESIAN_POINT ( 'NONE',  ( 184.5867277229704086, 83.68414666546580349, -10.24489875072611866 ) ) ;
#37033 = CARTESIAN_POINT ( 'NONE',  ( 210.9631450001601252, 117.1791136960929549, 5.703577349153958309 ) ) ;
#37034 = CARTESIAN_POINT ( 'NONE',  ( -178.5835577246388368, 93.42126246260829703, -47.35686724977312423 ) ) ;
#37035 = CARTESIAN_POINT ( 'NONE',  ( 93.63037639125411715, 21.92981100938039063, -13.77541507295795853 ) ) ;
#37036 = CARTESIAN_POINT ( 'NONE',  ( -30.95341298663139185, 10.53108683215057262, 57.06100499665286918 ) ) ;
#37037 = PLANE ( 'NONE',  #53128 ) ;
#37038 = EDGE_CURVE ( 'NONE', #44856, #38713, #30821, .T. ) ;
#37039 = CARTESIAN_POINT ( 'NONE',  ( 164.6561571795775194, 64.77723933022093661, 65.97358011928493227 ) ) ;
#37040 = ORIENTED_EDGE ( 'NONE', *, *, #26436, .F. ) ;
#37041 = DIRECTION ( 'NONE',  ( 0.000000000000000000, 0.000000000000000000, 1.000000000000000000 ) ) ;
#37042 = DIRECTION ( 'NONE',  ( -1.850371928290090422E-16, 1.000000000000000000, 1.110223024625156171E-16 ) ) ;
#37043 = CARTESIAN_POINT ( 'NONE',  ( 32.68347998332510684, -12.52158680757303344, 30.00000000000000000 ) ) ;
#37044 = CARTESIAN_POINT ( 'NONE',  ( 133.8566784816069344, -170.0000000000000000, -43.52331093239567394 ) ) ;
#37045 = CARTESIAN_POINT ( 'NONE',  ( 154.0401952541423611, 55.03227529428311726, 16.73850320082579657 ) ) ;
#37046 = AXIS2_PLACEMENT_3D ( 'NONE', #6634, #42862, #10865 ) ;
#37047 = CARTESIAN_POINT ( 'NONE',  ( -1.036819421871533864, 7.550827156688815656, 88.09984161770725564 ) ) ;
#37048 = VERTEX_POINT ( 'NONE', #63512 ) ;
#37049 = DIRECTION ( 'NONE',  ( 0.9959742939952382912, 0.08963930890344089242, 0.000000000000000000 ) ) ;
#37050 = EDGE_LOOP ( 'NONE', ( #30215, #39349, #69295, #812 ) ) ;
#37051 = ORIENTED_EDGE ( 'NONE', *, *, #46621, .F. ) ;
#37052 = CARTESIAN_POINT ( 'NONE',  ( 36.82270405522987744, 9.100602243567198713, 84.02932348124475936 ) ) ;
#37053 = LINE ( 'NONE', #68045, #20900 ) ;
#37054 = CARTESIAN_POINT ( 'NONE',  ( 137.5016378680191735, 44.85812207451340328, -90.64634188293649686 ) ) ;
#37055 = VERTEX_POINT ( 'NONE', #4424 ) ;
#37056 = CARTESIAN_POINT ( 'NONE',  ( 204.6977192012829505, 108.0580384837234931, 2.363170148305746565 ) ) ;
#37057 = LINE ( 'NONE', #4366, #30863 ) ;
#37058 = CARTESIAN_POINT ( 'NONE',  ( 32.46582151331404020, 7.608418548522498881, -13.39088614318420412 ) ) ;
#37059 = CARTESIAN_POINT ( 'NONE',  ( 174.2538192999569731, 73.34752463892030505, -46.83513099018006898 ) ) ;
#37060 = VECTOR ( 'NONE', #58408, 1000.000000000000000 ) ;
#37061 = CARTESIAN_POINT ( 'NONE',  ( -152.9008427825210106, 68.45483453645051952, -75.84960517240774891 ) ) ;
#37062 = PRODUCT_RELATED_PRODUCT_CATEGORY ( 'part', '', ( #58503 ) ) ;
#37063 = DIRECTION ( 'NONE',  ( -0.000000000000000000, 0.000000000000000000, -1.000000000000000000 ) ) ;
#37064 = ADVANCED_FACE ( 'NONE', ( #31847 ), #26569, .T. ) ;
#37065 = ORIENTED_EDGE ( 'NONE', *, *, #40417, .T. ) ;
#37066 = ADVANCED_FACE ( 'NONE', ( #25889 ), #46986, .F. ) ;
#37067 = FACE_OUTER_BOUND ( 'NONE', #34322, .T. ) ;
#37068 = CARTESIAN_POINT ( 'NONE',  ( -31.43908319763709969, 10.61114334766716105, 30.21645440618916112 ) ) ;
#37069 = CARTESIAN_POINT ( 'NONE',  ( 437.3372781065091885, 395.0000000000066507, -136.4497041420121661 ) ) ;
#37070 = DIRECTION ( 'NONE',  ( -0.000000000000000000, 1.000000000000000000, -0.000000000000000000 ) ) ;
#37072 = ORIENTED_EDGE ( 'NONE', *, *, #22449, .F. ) ;
#37071 = CARTESIAN_POINT ( 'NONE',  ( 1.667562369267748368, -64.99262834925670518, 3.061616997868437868E-16 ) ) ;
#37073 = ORIENTED_EDGE ( 'NONE', *, *, #25721, .T. ) ;
#37074 = AXIS2_PLACEMENT_3D ( 'NONE', #64767, #32066, #390 ) ;
#37075 = ORIENTED_EDGE ( 'NONE', *, *, #15434, .F. ) ;
#37076 = CARTESIAN_POINT ( 'NONE',  ( 111.1865443042261603, 30.43181341527238359, -77.72223575521005046 ) ) ;
#37077 = DIRECTION ( 'NONE',  ( 0.000000000000000000, 0.000000000000000000, 1.000000000000000000 ) ) ;
#37078 = PLANE ( 'NONE',  #50120 ) ;
#37079 = EDGE_CURVE ( 'NONE', #9838, #30336, #44481, .T. ) ;
#37080 = CARTESIAN_POINT ( 'NONE',  ( -31.43908319763709969, 10.61114334766715928, 57.06100499665286208 ) ) ;
#37081 = CARTESIAN_POINT ( 'NONE',  ( -9.779603649692305112, 8.034615131607072414, -8.815743396744277760 ) ) ;
#37082 = CARTESIAN_POINT ( 'NONE',  ( 152.3102623290679105, 53.74757787434985801, -65.02056816791532867 ) ) ;
#37083 = CARTESIAN_POINT ( 'NONE',  ( 19.10216788411012701, 6.629360741291161041, -22.90701642875757926 ) ) ;
#37084 = CARTESIAN_POINT ( 'NONE',  ( -156.6692143066620702, 70.50016761530885390, -44.55701924433694927 ) ) ;
#37085 = VERTEX_POINT ( 'NONE', #59949 ) ;
#37086 = EDGE_CURVE ( 'NONE', #9108, #1887, #16696, .T. ) ;
#37087 = ORIENTED_EDGE ( 'NONE', *, *, #49796, .T. ) ;
#37088 = EDGE_CURVE ( 'NONE', #8605, #24127, #64546, .T. ) ;
#37089 = CARTESIAN_POINT ( 'NONE',  ( 70.41705859591009187, 15.55317472777718102, -17.61350428500981025 ) ) ;
#37090 = CARTESIAN_POINT ( 'NONE',  ( -31.43908319763709969, 9.591432048623758533, -23.47264677473818395 ) ) ;
#37091 = CARTESIAN_POINT ( 'NONE',  ( 141.9165763529819344, -52.00000000000000711, 129.0000000000000000 ) ) ;
#37092 = CIRCLE ( 'NONE', #6764, 5.000000000000004441 ) ;
#37093 = CARTESIAN_POINT ( 'NONE',  ( -152.2873556200145799, 67.91256772393731467, 4.406972807603752429 ) ) ;
#37094 = FACE_BOUND ( 'NONE', #42854, .T. ) ;
#37095 = CARTESIAN_POINT ( 'NONE',  ( 22.30016284075437127, 6.796348835713779124, 41.26772859709231511 ) ) ;
#37096 = CARTESIAN_POINT ( 'NONE',  ( -157.0087551414807194, 72.18321165533608053, 91.79709723166649837 ) ) ;
#37097 = VERTEX_POINT ( 'NONE', #27246 ) ;
#37098 = ORIENTED_EDGE ( 'NONE', *, *, #15473, .T. ) ;
#37099 = ORIENTED_EDGE ( 'NONE', *, *, #3029, .T. ) ;
#37100 = CARTESIAN_POINT ( 'NONE',  ( -150.5993571094983281, 66.43939758484178526, -22.89157138131998437 ) ) ;
#37101 = CARTESIAN_POINT ( 'NONE',  ( 93.02946412630693374, 22.77895695581315039, -93.07924972775212780 ) ) ;
#37102 = B_SPLINE_CURVE_WITH_KNOTS ( 'NONE', 3,
 ( #38362, #59462, #5319, #53490, #43280, #5649 ),
 .UNSPECIFIED., .F., .F.,
 ( 4, 2, 4 ),
 ( 1.095770181115393514E-06, 0.03239442681617710901, 0.06478775786217311206 ),
 .UNSPECIFIED. ) ;
#37103 = CARTESIAN_POINT ( 'NONE',  ( -6.802008071587034799, -24.18409554641273473, 0.000000000000000000 ) ) ;
#37104 = CARTESIAN_POINT ( 'NONE',  ( -33.36721086971962080, 9.915747831546610769, 71.81304879671020558 ) ) ;
#37105 = CARTESIAN_POINT ( 'NONE',  ( -155.7495771807047333, 69.65980221699317099, -19.65617803842697242 ) ) ;
#37106 = ORIENTED_EDGE ( 'NONE', *, *, #27151, .F. ) ;
#37107 = FACE_BOUND ( 'NONE', #39399, .T. ) ;
#37108 = DIRECTION ( 'NONE',  ( -0.000000000000000000, 1.000000000000000000, -0.000000000000000000 ) ) ;
#37109 = CARTESIAN_POINT ( 'NONE',  ( 22.72762739171800561, 7.830015800126076009, 13.54664626853137577 ) ) ;
#37110 = CARTESIAN_POINT ( 'NONE',  ( 186.6118452967672567, 84.37814701615440072, 68.74724828204176674 ) ) ;
#37111 = DIRECTION ( 'NONE',  ( 0.000000000000000000, 0.000000000000000000, -1.000000000000000000 ) ) ;
#37112 = DIRECTION ( 'NONE',  ( -0.8118923937861950435, -0.5838071093367415143, 0.000000000000000000 ) ) ;
#37114 = EDGE_CURVE ( 'NONE', #56047, #8968, #878, .T. ) ;
#37113 = DIRECTION ( 'NONE',  ( 1.000000000000000000, 0.000000000000000000, 0.000000000000000000 ) ) ;
#37115 = LINE ( 'NONE', #31840, #28748 ) ;
#37116 = CYLINDRICAL_SURFACE ( 'NONE', #20997, 35.00000000000000000 ) ;
#37117 = VERTEX_POINT ( 'NONE', #16354 ) ;
#37118 = CARTESIAN_POINT ( 'NONE',  ( 187.2354698746857196, 85.05376776489252677, 5.644151847218983775 ) ) ;
#37119 = APPLICATION_PROTOCOL_DEFINITION ( 'draft international standard', 'automotive_design', 1998, #33228 ) ;
#37120 = AXIS2_PLACEMENT_3D ( 'NONE', #61823, #8733, #24906 ) ;
#37121 = CARTESIAN_POINT ( 'NONE',  ( 132.0249343950657135, 41.49728247212332377, -36.19146592362032777 ) ) ;
#37122 = CARTESIAN_POINT ( 'NONE',  ( -132.4819073909166320, 50.98736898418876251, -38.79117142572575005 ) ) ;
#37123 = CARTESIAN_POINT ( 'NONE',  ( -104.7956873821848802, 35.21322275870668506, -49.58398961066640709 ) ) ;
#37124 = CARTESIAN_POINT ( 'NONE',  ( 60.63380853769237433, 13.16344960520420848, -77.18114081708419860 ) ) ;
#37125 = ORIENTED_EDGE ( 'NONE', *, *, #64901, .T. ) ;
#37126 = ORIENTED_EDGE ( 'NONE', *, *, #17240, .F. ) ;
#37127 = FACE_OUTER_BOUND ( 'NONE', #3334, .T. ) ;
#37128 = CARTESIAN_POINT ( 'NONE',  ( 173.6061830963395778, 71.36490884257202083, 91.10848141826026847 ) ) ;
#37129 = ORIENTED_EDGE ( 'NONE', *, *, #41385, .F. ) ;
#37130 = DIRECTION ( 'NONE',  ( -0.000000000000000000, 1.000000000000000000, -0.000000000000000000 ) ) ;
#37131 = ORIENTED_EDGE ( 'NONE', *, *, #38334, .T. ) ;
#37132 = CARTESIAN_POINT ( 'NONE',  ( 132.0249343950657703, 41.49728247212335219, -63.03601651408401096 ) ) ;
#37133 = CARTESIAN_POINT ( 'NONE',  ( 130.7260704202055024, 39.56565398554882051, 30.17888742523724943 ) ) ;
#37134 = CARTESIAN_POINT ( 'NONE',  ( 36.85262215550071119, 53.56030941157734304, 3.061616997868437868E-16 ) ) ;
#37135 = VECTOR ( 'NONE', #9089, 1000.000000000000000 ) ;
#37137 = ADVANCED_FACE ( 'NONE', ( #49737 ), #48682, .T. ) ;
#37136 = CARTESIAN_POINT ( 'NONE',  ( 163.1459438811106679, 62.20198481903361909, -92.39285677337488778 ) ) ;
#37138 = CARTESIAN_POINT ( 'NONE',  ( 94.11746922806584337, 22.11341285603782936, -42.82955049988751739 ) ) ;
#37140 = ORIENTED_EDGE ( 'NONE', *, *, #57409, .F. ) ;
#37139 = DIRECTION ( 'NONE',  ( 0.000000000000000000, 0.000000000000000000, 1.000000000000000000 ) ) ;
#37141 = EDGE_CURVE ( 'NONE', #41688, #19218, #49037, .T. ) ;
#37142 = ORIENTED_EDGE ( 'NONE', *, *, #7929, .F. ) ;
#37143 = ORIENTED_EDGE ( 'NONE', *, *, #28339, .T. ) ;
#37144 = CARTESIAN_POINT ( 'NONE',  ( -124.1094910780272755, 45.33021696310842685, -22.85738008745166994 ) ) ;
#37145 = EDGE_CURVE ( 'NONE', #11779, #13157, #23727, .T. ) ;
#37146 = FACE_BOUND ( 'NONE', #62101, .T. ) ;
#37147 = CARTESIAN_POINT ( 'NONE',  ( -173.5394735271663365, 87.59446374803715685, -22.86740657428633838 ) ) ;
#37148 = CARTESIAN_POINT ( 'NONE',  ( 0.7145311798161616545, -4.618802153517262532, -8.000000000000001776 ) ) ;
#37150 = ORIENTED_EDGE ( 'NONE', *, *, #58760, .F. ) ;
#37149 = CARTESIAN_POINT ( 'NONE',  ( -143.8566410313463280, 59.53044870492033880, -37.35523672868243494 ) ) ;
#37151 = DIRECTION ( 'NONE',  ( 1.000000000000000000, -0.000000000000000000, 0.000000000000000000 ) ) ;
#37152 = EDGE_CURVE ( 'NONE', #8163, #26255, #46205, .T. ) ;
#37153 = VERTEX_POINT ( 'NONE', #32881 ) ;
#37154 = CARTESIAN_POINT ( 'NONE',  ( -133.2698123908828620, 51.54642138335024981, 39.50404384874914854 ) ) ;
#37155 = LINE ( 'NONE', #9055, #60323 ) ;
#37156 = CARTESIAN_POINT ( 'NONE',  ( 133.8566784816069344, 41.42467568809809109, -24.17876034193199786 ) ) ;
#37157 = DIRECTION ( 'NONE',  ( -0.000000000000000000, -0.000000000000000000, -1.000000000000000000 ) ) ;
#37158 = DIRECTION ( 'NONE',  ( -1.850169831522831466E-16, 1.000000000000000000, 1.110223024625156294E-16 ) ) ;
#37159 = CARTESIAN_POINT ( 'NONE',  ( -96.43148989374458324, 29.90755650959363265, 15.89613036013473923 ) ) ;
#37160 = CARTESIAN_POINT ( 'NONE',  ( -149.9130953879582364, 64.52387832078942154, -88.50193171241933499 ) ) ;
#37161 = EDGE_LOOP ( 'NONE', ( #49493, #13240, #2748, #56948 ) ) ;
#37162 = EDGE_CURVE ( 'NONE', #26944, #38916, #6503, .T. ) ;
#37163 = EDGE_LOOP ( 'NONE', ( #26737, #42892 ) ) ;
#37164 = VECTOR ( 'NONE', #7965, 1000.000000000000000 ) ;
#37165 = CARTESIAN_POINT ( 'NONE',  ( 187.8959968237854525, 85.77553094678181367, -73.71938198361095829 ) ) ;
#37166 = CARTESIAN_POINT ( 'NONE',  ( -39.55079474733700096, 51.59997227570983114, 41.38025477438755928 ) ) ;
#37167 = PLANE ( 'NONE',  #67773 ) ;
#37168 = CARTESIAN_POINT ( 'NONE',  ( 103.0124792097646349, 26.77148435100180990, -72.32543776868688212 ) ) ;
#37169 = VECTOR ( 'NONE', #34297, 1000.000000000000000 ) ;
#37170 = CARTESIAN_POINT ( 'NONE',  ( -78.66644367742111399, 23.39876645725287219, 30.41820113967310490 ) ) ;
#37171 = CARTESIAN_POINT ( 'NONE',  ( 79.92465405224848496, 17.24122384219593584, 40.60998972530957474 ) ) ;
#37172 = CARTESIAN_POINT ( 'NONE',  ( 15.55634918610406103, 15.55634918610400241, 0.000000000000000000 ) ) ;
#37173 = CARTESIAN_POINT ( 'NONE',  ( -125.8938041572051389, 47.69968343338778283, 30.61994787315706290 ) ) ;
#37174 = CARTESIAN_POINT ( 'NONE',  ( 212.0047492081760936, 116.9348962082588628, 61.83128332929177873 ) ) ;
#37175 = ORIENTED_EDGE ( 'NONE', *, *, #14938, .F. ) ;
#37176 = CARTESIAN_POINT ( 'NONE',  ( -106.6781182590523542, 35.07133425426476236, -9.576435181703248034 ) ) ;
#37177 = ORIENTED_EDGE ( 'NONE', *, *, #63155, .F. ) ;
#37178 = VECTOR ( 'NONE', #16037, 1000.000000000000000 ) ;
#37179 = DIRECTION ( 'NONE',  ( 1.000000000000000000, 0.000000000000000000, 0.000000000000000000 ) ) ;
#37180 = DIRECTION ( 'NONE',  ( -0.000000000000000000, -0.000000000000000000, 1.000000000000000000 ) ) ;
#37181 = CARTESIAN_POINT ( 'NONE',  ( -85.97225349031586461, 25.24026879827588132, -94.54786562133661221 ) ) ;
#37182 = PLANE ( 'NONE',  #28694 ) ;
#37183 = DIRECTION ( 'NONE',  ( -0.8090169943749506709, 0.5877852522924686962, 0.000000000000000000 ) ) ;
#37184 = DIRECTION ( 'NONE',  ( 1.000000000000000000, 0.000000000000000000, -0.000000000000000000 ) ) ;
#37185 = CARTESIAN_POINT ( 'NONE',  ( -156.9402586331177361, 70.74941713998435944, -95.00000000000133582 ) ) ;
#37186 = CARTESIAN_POINT ( 'NONE',  ( -31.43908319763710679, -170.0000000000000000, -8.472646774738155528 ) ) ;
#37187 = VERTEX_POINT ( 'NONE', #65237 ) ;
#37188 = B_SPLINE_CURVE_WITH_KNOTS ( 'NONE', 3,
 ( #52145, #62710, #36316, #14511, #68334, #36663, #15552, #25773, #37003, #52489, #47202, #46169, #31721, #4311, #31385, #57772, #41932, #4641, #63744, #63045, #19437, #30693, #67642, #14850, #31045, #35970, #14170, #9238, #19791, #68660, #62357, #41254, #20470, #3962, #40898, #63398, #9585, #58114 ),
 .UNSPECIFIED., .F., .F.,
 ( 4, 2, 2, 2, 2, 2, 2, 2, 2, 2, 2, 2, 2, 2, 2, 2, 2, 2, 4 ),
 ( 1.551583845779545699E-17, 0.001559859933532273648, 0.003119719867064531683, 0.004679579800596789067, 0.006239439734129047753, 0.007799299667661305571, 0.008579229634427429710, 0.009359159601193552114, 0.01091901953472580039, 0.01169894950149191065, 0.01247887946825801918, 0.01403873940179021888, 0.01559859933532241859, 0.01715845926885461656, 0.01871831920238681626, 0.02027817913591901597, 0.02183803906945121567, 0.02339789900298341538, 0.02495775893651561508 ),
 .UNSPECIFIED. ) ;
#37189 = DIRECTION ( 'NONE',  ( -0.8160245890732938934, -0.5780171883497599028, 0.000000000000000000 ) ) ;
#37190 = ORIENTED_EDGE ( 'NONE', *, *, #33678, .F. ) ;
#37191 = DIRECTION ( 'NONE',  ( 0.000000000000000000, 0.000000000000000000, 1.000000000000000000 ) ) ;
#37192 =( LENGTH_UNIT ( ) NAMED_UNIT ( * ) SI_UNIT ( .MILLI., .METRE. ) );
#37193 = CARTESIAN_POINT ( 'NONE',  ( -190.6985136298601731, 109.1272424661242582, 94.99999999999866418 ) ) ;
#37194 = CARTESIAN_POINT ( 'NONE',  ( 187.0823097343935331, 86.37667841017882608, 94.99999999999866418 ) ) ;
#37195 = CARTESIAN_POINT ( 'NONE',  ( -1.088326810997878535, 6.545818265928947000, 34.28345951116151724 ) ) ;
#37196 = CARTESIAN_POINT ( 'NONE',  ( -200.0000000000000000, 2.449293598294706434E-14, -10.00000000000000000 ) ) ;
#37197 = FILL_AREA_STYLE_COLOUR ( '', #66486 ) ;
#37198 = ORIENTED_EDGE ( 'NONE', *, *, #49680, .T. ) ;
#37199 = DIRECTION ( 'NONE',  ( 9.967721092962736720E-15, -1.000000000000000000, -4.052314039881822161E-15 ) ) ;
#37200 = LINE ( 'NONE', #16092, #9369 ) ;
#37201 = FACE_OUTER_BOUND ( 'NONE', #62943, .T. ) ;
#37202 = CARTESIAN_POINT ( 'NONE',  ( -109.7643866341847456, 37.89854104106755983, 64.31230601605615504 ) ) ;
#37203 = ITEM_DEFINED_TRANSFORMATION ( 'NONE', 'NONE', #24242,  #66832 ) ;
#37204 = CARTESIAN_POINT ( 'NONE',  ( -133.3944793432480367, 52.87251459353621641, -42.15878017665119870 ) ) ;
#37205 = ORIENTED_EDGE ( 'NONE', *, *, #41055, .F. ) ;
#37206 = LINE ( 'NONE', #16453, #13169 ) ;
#37207 = EDGE_CURVE ( 'NONE', #17325, #21790, #34416, .T. ) ;
#37208 = CARTESIAN_POINT ( 'NONE',  ( 90.31682503704260512, 20.71196693118262289, 70.60568123287703202 ) ) ;
#37209 = PRESENTATION_STYLE_ASSIGNMENT (( #15762 ) ) ;
#37210 = CARTESIAN_POINT ( 'NONE',  ( -142.0064771034751061, 58.06937679312856204, 91.78148141502676083 ) ) ;
#37211 = CARTESIAN_POINT ( 'NONE',  ( 137.3958226571047021, 43.60243650158411555, 30.38137377392774141 ) ) ;
#37212 = VERTEX_POINT ( 'NONE', #1567 ) ;
#37213 = CARTESIAN_POINT ( 'NONE',  ( 0.000000000000000000, 0.000000000000000000, 22.50000000000000000 ) ) ;
#37214 = CARTESIAN_POINT ( 'NONE',  ( 79.14113188808478583, 18.05280674635439553, 10.85844641349727624 ) ) ;
#37215 = CARTESIAN_POINT ( 'NONE',  ( 163.1370549780983481, 63.50181104276883559, 5.126036944425179875 ) ) ;
#37216 = FACE_OUTER_BOUND ( 'NONE', #56013, .T. ) ;
#37217 = ORIENTED_EDGE ( 'NONE', *, *, #66672, .F. ) ;
#37218 = CARTESIAN_POINT ( 'NONE',  ( 32.99392442438140449, 8.673943046035248017, 94.99999999999866418 ) ) ;
#37219 = EDGE_CURVE ( 'NONE', #20457, #65969, #22326, .T. ) ;
#37220 = AXIS2_PLACEMENT_3D ( 'NONE', #47054, #36503, #9085 ) ;
#37221 = ORIENTED_EDGE ( 'NONE', *, *, #27376, .T. ) ;
#37222 = CARTESIAN_POINT ( 'NONE',  ( -107.0584934212648704, 35.27493744466470815, -36.71298738587253752 ) ) ;
#37223 = CARTESIAN_POINT ( 'NONE',  ( 70.51484748609223630, 14.53801151001410652, -70.57721950703738401 ) ) ;
#37224 = CARTESIAN_POINT ( 'NONE',  ( -60.65612136648952912, 16.25551606627059442, 42.82650858269547456 ) ) ;
#37226 = VERTEX_POINT ( 'NONE', #6842 ) ;
#37225 = CARTESIAN_POINT ( 'NONE',  ( 150.2805372522807374, 53.51147386362153924, 12.21657638438227167 ) ) ;
#37227 = CARTESIAN_POINT ( 'NONE',  ( 158.3516718297675538, 59.61984652322051659, -51.08544735948212434 ) ) ;
#37228 = EDGE_CURVE ( 'NONE', #23144, #5719, #53629, .T. ) ;
#37229 = DIRECTION ( 'NONE',  ( -1.000000000000000000, 0.000000000000000000, -0.000000000000000000 ) ) ;
#37230 = CARTESIAN_POINT ( 'NONE',  ( 117.7417271423229863, 33.63613196344607559, -42.88727997055872265 ) ) ;
#37231 = ORIENTED_EDGE ( 'NONE', *, *, #17569, .F. ) ;
#37232 = CARTESIAN_POINT ( 'NONE',  ( 8.000000000000007105, 249.8719672152120381, -95.00000000000133582 ) ) ;
#37233 = CARTESIAN_POINT ( 'NONE',  ( 134.7770330630253000, 41.98246829846534922, 71.31249374605413038 ) ) ;
#37234 = CARTESIAN_POINT ( 'NONE',  ( -173.9526029538035914, 89.57590038685106038, 30.85607633362990398 ) ) ;
#37235 = CARTESIAN_POINT ( 'NONE',  ( -35.38560449531986762, 10.27249159032102810, -76.04409089915343145 ) ) ;
#37236 = EDGE_CURVE ( 'NONE', #18627, #31561, #21973, .T. ) ;
#37237 = ORIENTED_EDGE ( 'NONE', *, *, #27230, .F. ) ;
#37238 = CARTESIAN_POINT ( 'NONE',  ( 45.04020069093783007, 10.22779424730543241, 15.53914219526992468 ) ) ;
#37239 = VERTEX_POINT ( 'NONE', #26908 ) ;
#37240 = ORIENTED_EDGE ( 'NONE', *, *, #19296, .F. ) ;
#37241 =( NAMED_UNIT ( * ) SI_UNIT ( $, .STERADIAN. ) SOLID_ANGLE_UNIT ( ) );
#37242 = ADVANCED_FACE ( 'NONE', ( #33244 ), #27951, .F. ) ;
#37243 = CARTESIAN_POINT ( 'NONE',  ( -62.52556685097597722, 16.81334402605504508, 90.59652277792575603 ) ) ;
#37244 = DIRECTION ( 'NONE',  ( -0.000000000000000000, -0.000000000000000000, -1.000000000000000000 ) ) ;
#37245 = CARTESIAN_POINT ( 'NONE',  ( -155.7495771807047618, 69.65980221699318520, -73.34527921935438144 ) ) ;
#37246 = CARTESIAN_POINT ( 'NONE',  ( 5.799999999999999822, -4.618802153517012954, -8.000000000000001776 ) ) ;
#37247 = FACE_OUTER_BOUND ( 'NONE', #19237, .T. ) ;
#37248 = CARTESIAN_POINT ( 'NONE',  ( 8.828807734114020533, 74.48902371486721563, 170.0000000000000000 ) ) ;
#37249 = FACE_BOUND ( 'NONE', #55559, .T. ) ;
#37250 = ORIENTED_EDGE ( 'NONE', *, *, #67937, .T. ) ;
#37251 = CARTESIAN_POINT ( 'NONE',  ( -17.50000000000002842, 207.5000000000000284, 378.0000000000000000 ) ) ;
#37252 = ORIENTED_EDGE ( 'NONE', *, *, #54050, .T. ) ;
#37253 = CARTESIAN_POINT ( 'NONE',  ( -71.97171223898808989, 20.94894057408426491, 68.18058196594357412 ) ) ;
#37254 = CARTESIAN_POINT ( 'NONE',  ( 207.8675797643809631, 110.7908513421272119, -63.86012885756652224 ) ) ;
#37255 = CARTESIAN_POINT ( 'NONE',  ( 1.667562369266827327, 64.99262834925669097, 170.0000000000000000 ) ) ;
#37256 = CARTESIAN_POINT ( 'NONE',  ( -74.17694007417655655, 20.66176641130876135, 17.10122609394768389 ) ) ;
#37257 = PLANE ( 'NONE',  #67127 ) ;
#37258 = CARTESIAN_POINT ( 'NONE',  ( 19.54326199789021601, 7.657220834818549093, 31.01773977966792728 ) ) ;
#37259 = VECTOR ( 'NONE', #53546, 999.9999999999998863 ) ;
#37260 = CARTESIAN_POINT ( 'NONE',  ( 197.1968910587178243, 96.59211440045608299, 90.83512555983344328 ) ) ;
#37261 = FACE_OUTER_BOUND ( 'NONE', #50516, .T. ) ;
#37262 = ORIENTED_EDGE ( 'NONE', *, *, #41443, .T. ) ;
#37263 = CARTESIAN_POINT ( 'NONE',  ( -75.00168449119591685, 20.95943092127968654, 71.31086889332340206 ) ) ;
#37264 = DIRECTION ( 'NONE',  ( 0.000000000000000000, 0.000000000000000000, 1.000000000000000000 ) ) ;
#37265 = ORIENTED_EDGE ( 'NONE', *, *, #48372, .T. ) ;
#37266 = ORIENTED_EDGE ( 'NONE', *, *, #34942, .T. ) ;
#37267 = LINE ( 'NONE', #54124, #617 ) ;
#37268 = CARTESIAN_POINT ( 'NONE',  ( -31.43908319763709969, 10.61114334766716105, -23.47264677473818395 ) ) ;
#37270 = PLANE ( 'NONE',  #42378 ) ;
#37269 = AXIS2_PLACEMENT_3D ( 'NONE', #16574, #65473, #16227 ) ;
#37271 = MECHANICAL_DESIGN_GEOMETRIC_PRESENTATION_REPRESENTATION (  '', ( #52978 ), #12588 ) ;
#37272 = DIRECTION ( 'NONE',  ( -0.6234898018587431423, 0.7818314824680220321, 0.000000000000000000 ) ) ;
#37273 = DIRECTION ( 'NONE',  ( 1.000000000000000000, 0.000000000000000000, 0.000000000000000000 ) ) ;
#37274 = CONICAL_SURFACE ( 'NONE', #6958, 8.000000000000000000, 1.047197551196600296 ) ;
#37275 = EDGE_LOOP ( 'NONE', ( #51057, #2290, #30394, #31026 ) ) ;
#37276 = ORIENTED_EDGE ( 'NONE', *, *, #33922, .T. ) ;
#37277 = CARTESIAN_POINT ( 'NONE',  ( -133.1566699306513613, 52.70203339370771545, 36.22971255361426302 ) ) ;
#37278 = ORIENTED_EDGE ( 'NONE', *, *, #60960, .F. ) ;
#37279 = CARTESIAN_POINT ( 'NONE',  ( 204.6977192012829789, 106.3443248447423315, 17.36317014830577321 ) ) ;
#37280 = CARTESIAN_POINT ( 'NONE',  ( -144.7530445311634537, 61.54314312182905411, 32.41526756990536740 ) ) ;
#37281 = CARTESIAN_POINT ( 'NONE',  ( 61.09275639403233527, 12.23448398202909893, 56.89203593337313691 ) ) ;
#37282 = EDGE_CURVE ( 'NONE', #8542, #47295, #22675, .T. ) ;
#37283 = DIRECTION ( 'NONE',  ( 0.000000000000000000, 0.000000000000000000, 1.000000000000000000 ) ) ;
#37284 = FILL_AREA_STYLE ('',( #10554 ) ) ;
#37285 = CARTESIAN_POINT ( 'NONE',  ( -422.6627218934914936, 399.9999999999998863, -146.4497041420118251 ) ) ;
#37286 = EDGE_CURVE ( 'NONE', #36843, #14304, #44113, .T. ) ;
#37287 = ORIENTED_EDGE ( 'NONE', *, *, #8979, .F. ) ;
#37288 = ORIENTED_EDGE ( 'NONE', *, *, #62884, .T. ) ;
#37289 = LINE ( 'NONE', #64035, #1971 ) ;
#37290 = DIRECTION ( 'NONE',  ( -0.000000000000000000, 1.000000000000000000, -0.000000000000000000 ) ) ;
#37291 = CARTESIAN_POINT ( 'NONE',  ( -166.7049310409072689, 80.25944422923579680, -11.47475090231446160 ) ) ;
#37292 = DIRECTION ( 'NONE',  ( 0.000000000000000000, 0.000000000000000000, -1.000000000000000000 ) ) ;
#37293 = CARTESIAN_POINT ( 'NONE',  ( -0.4996266546846081513, 7.531422798935177632, -95.00000000000133582 ) ) ;
#37294 = CARTESIAN_POINT ( 'NONE',  ( 17.42558916372104250, 7.565465075731206746, 83.87742723891268781 ) ) ;
#37295 = ORIENTED_EDGE ( 'NONE', *, *, #3663, .F. ) ;
#37296 = EDGE_CURVE ( 'NONE', #4563, #53791, #53961, .T. ) ;
#37297 = CARTESIAN_POINT ( 'NONE',  ( -95.86612279493098754, 29.64021615886204941, 68.75908302673695971 ) ) ;
#37298 = ORIENTED_EDGE ( 'NONE', *, *, #32385, .T. ) ;
#37299 = EDGE_CURVE ( 'NONE', #44224, #1555, #20069, .T. ) ;
#37300 = CARTESIAN_POINT ( 'NONE',  ( -71.67841390531688717, 19.78168466957075466, 35.18329047664818177 ) ) ;
#37301 = EDGE_LOOP ( 'NONE', ( #41339, #12179, #58527, #34909 ) ) ;
#37302 = EDGE_CURVE ( 'NONE', #12108, #64034, #45871, .T. ) ;
#37303 = AXIS2_PLACEMENT_3D ( 'NONE', #12934, #55839, #61457 ) ;
#37304 = ORIENTED_EDGE ( 'NONE', *, *, #68245, .F. ) ;
#37305 = CARTESIAN_POINT ( 'NONE',  ( -122.1940143064357187, 45.29738883755585732, 17.80353666295016879 ) ) ;
#37306 = EDGE_CURVE ( 'NONE', #59358, #1423, #67342, .T. ) ;
#37307 = CARTESIAN_POINT ( 'NONE',  ( -178.2427210808089058, 93.01567669683340966, 59.68194965257550422 ) ) ;
#37308 = CARTESIAN_POINT ( 'NONE',  ( 126.3737790127712799, 37.08609730334949006, 64.42584544384298795 ) ) ;
#37309 = VECTOR ( 'NONE', #53395, 1000.000000000000000 ) ;
#37310 = EDGE_LOOP ( 'NONE', ( #32427, #36216, #38483, #31559 ) ) ;
#37311 = CARTESIAN_POINT ( 'NONE',  ( -24.69950091090638722, 8.581800362251172487, 94.71242551333074289 ) ) ;
#37312 = CARTESIAN_POINT ( 'NONE',  ( 155.7262569076171985, 56.30477153194512852, 44.25956702222304529 ) ) ;
#37313 = DIRECTION ( 'NONE',  ( -1.000000000000000000, 0.000000000000000000, 0.000000000000000000 ) ) ;
#37314 = LINE ( 'NONE', #48543, #54732 ) ;
#37315 = CARTESIAN_POINT ( 'NONE',  ( 0.000000000000000000, 0.000000000000000000, 41.38025477438755928 ) ) ;
#37316 = EDGE_CURVE ( 'NONE', #50492, #64271, #55374, .T. ) ;
#37317 = CARTESIAN_POINT ( 'NONE',  ( -24.07146903340143140, 8.497560047608727629, 39.18234541147268857 ) ) ;
#37318 = PLANE ( 'NONE',  #2947 ) ;
#37319 = VERTEX_POINT ( 'NONE', #19132 ) ;
#37320 = EDGE_CURVE ( 'NONE', #33172, #53230, #45521, .T. ) ;
#37321 = EDGE_CURVE ( 'NONE', #35904, #18015, #8005, .T. ) ;
#37322 = FACE_BOUND ( 'NONE', #13442, .T. ) ;
#37323 = EDGE_CURVE ( 'NONE', #48044, #16146, #8597, .T. ) ;
#37324 = CARTESIAN_POINT ( 'NONE',  ( 22.93737758745385946, -9.943676855698914352, 0.000000000000000000 ) ) ;
#37325 = CARTESIAN_POINT ( 'NONE',  ( -80.31482177285911916, 24.03632224640839610, -76.78049980088347581 ) ) ;
#37326 = LINE ( 'NONE', #53499, #7978 ) ;
#37327 = CARTESIAN_POINT ( 'NONE',  ( -122.3994536713185255, 45.42826354555016621, -35.77335078514256850 ) ) ;
#37328 = DIRECTION ( 'NONE',  ( -0.000000000000000000, -0.000000000000000000, -1.000000000000000000 ) ) ;
#37329 = CARTESIAN_POINT ( 'NONE',  ( 132.7179291807801178, 40.74118679001691135, 2.749225463022159310 ) ) ;
#37330 = CARTESIAN_POINT ( 'NONE',  ( -63.33140416796831573, -16.18162651919486095, 41.38025477438755928 ) ) ;
#37331 = DIRECTION ( 'NONE',  ( 0.000000000000000000, 0.000000000000000000, 1.000000000000000000 ) ) ;
#37332 = CARTESIAN_POINT ( 'NONE',  ( -450.6627218934913230, 177.8591479523843475, -111.4497041420117966 ) ) ;
#37333 = DIRECTION ( 'NONE',  ( 0.000000000000000000, 0.000000000000000000, -1.000000000000000000 ) ) ;
#37334 = CARTESIAN_POINT ( 'NONE',  ( 89.88147981065579017, 21.62466191578950614, -9.701577234200509992 ) ) ;
#37335 = ORIENTED_EDGE ( 'NONE', *, *, #34823, .F. ) ;
#37336 = CARTESIAN_POINT ( 'NONE',  ( -38.17232309348612773, 11.81874355808868238, 14.21233894131476738 ) ) ;
#37337 = ORIENTED_EDGE ( 'NONE', *, *, #68060, .F. ) ;
#37338 = CARTESIAN_POINT ( 'NONE',  ( -78.66644367742111399, -170.0000000000000000, -76.96000122218160300 ) ) ;
#37339 = ORIENTED_EDGE ( 'NONE', *, *, #41634, .T. ) ;
#37340 = CARTESIAN_POINT ( 'NONE',  ( 20.36233635256088803, 7.697399815318436644, -75.82726962297421380 ) ) ;
#37341 = DIRECTION ( 'NONE',  ( 0.000000000000000000, 0.000000000000000000, 1.000000000000000000 ) ) ;
#37342 = DIRECTION ( 'NONE',  ( -0.000000000000000000, -1.000000000000000000, 0.000000000000000000 ) ) ;
#37343 = LINE ( 'NONE', #43306, #36716 ) ;
#37344 = CARTESIAN_POINT ( 'NONE',  ( 141.3036441389950824, 47.31002705502927341, -44.56327115119219684 ) ) ;
#37345 = CARTESIAN_POINT ( 'NONE',  ( 290.0000000000000568, -5.000000000000000888, 21.42428528562853529 ) ) ;
#37346 = CARTESIAN_POINT ( 'NONE',  ( 99.71998884745383407, 2.000000000000001776, 7.478223336038896996 ) ) ;
#37347 = CARTESIAN_POINT ( 'NONE',  ( -31.43908319763710679, -170.0000000000000000, 91.40555558711655237 ) ) ;
#37348 = EDGE_LOOP ( 'NONE', ( #56989, #41773, #9030, #38875 ) ) ;
#37349 = EDGE_LOOP ( 'NONE', ( #282, #68241, #57694, #61140 ) ) ;
#37350 = CARTESIAN_POINT ( 'NONE',  ( 66.08620257826613908, 13.40585338179127284, -36.37378492149262144 ) ) ;
#37351 = DIRECTION ( 'NONE',  ( -0.3513748240813305279, -0.9362348706397418674, 0.000000000000000000 ) ) ;
#37352 = CARTESIAN_POINT ( 'NONE',  ( 126.8188448246704780, 38.48775085959175613, -94.58402359101047807 ) ) ;
#37353 = PRODUCT_DEFINITION_CONTEXT ( 'detailed design', #30970, 'design' ) ;
#37354 = AXIS2_PLACEMENT_3D ( 'NONE', #11088, #65888, #31865 ) ;
#37355 = CARTESIAN_POINT ( 'NONE',  ( -1.666933348992582609, 64.97862212458815634, 73.58025477438755502 ) ) ;
#37356 = ORIENTED_EDGE ( 'NONE', *, *, #31767, .T. ) ;
#37357 = CARTESIAN_POINT ( 'NONE',  ( 284.9679224117287504, 21.99264416388322374, 0.6532133356533497137 ) ) ;
#37358 = CARTESIAN_POINT ( 'NONE',  ( -15.22871623201694291, 7.486724405784663361, 63.23486717562329318 ) ) ;
#37359 = CARTESIAN_POINT ( 'NONE',  ( -79.14678386417814693, 22.50468917936073510, -8.270900041254199309 ) ) ;
#37360 = CIRCLE ( 'NONE', #51941, 21.00000000000000355 ) ;
#37361 = SHAPE_REPRESENTATION_RELATIONSHIP ( 'NONE' , 'NONE' ,  #64925, #20676 ) ;
#37362 = CARTESIAN_POINT ( 'NONE',  ( 0.1306530452038165702, -7.903938623646881823, -2.309976723937614107 ) ) ;
#37363 = CARTESIAN_POINT ( 'NONE',  ( 46.90141780929663184, 9.503798448769773088, -16.77990280306253013 ) ) ;
#37364 = CARTESIAN_POINT ( 'NONE',  ( 30.47484967065694761, -59.26962189778872414, 34.48241795236665297 ) ) ;
#37365 = CARTESIAN_POINT ( 'NONE',  ( 106.9485791615413461, 21.63883785544751603, -3.974247539526119422 ) ) ;
#37366 = CARTESIAN_POINT ( 'NONE',  ( 164.9700808964341547, 65.04346068891115351, 64.04275777180556872 ) ) ;
#37367 = B_SPLINE_CURVE_WITH_KNOTS ( 'NONE', 3,
 ( #29191, #50633, #66151, #1064, #12316, #12664 ),
 .UNSPECIFIED., .F., .F.,
 ( 4, 2, 4 ),
 ( 0.03218932929355812489, 0.06469831333814424212, 0.09720729738273037324 ),
 .UNSPECIFIED. ) ;
#37368 = EDGE_CURVE ( 'NONE', #27491, #5170, #24768, .T. ) ;
#37369 = AXIS2_PLACEMENT_3D ( 'NONE', #10040, #59251, #43414 ) ;
#37370 = ORIENTED_EDGE ( 'NONE', *, *, #31782, .T. ) ;
#37371 = DIRECTION ( 'NONE',  ( -1.000000000000000000, 0.000000000000000000, 0.000000000000000000 ) ) ;
#37372 = DIRECTION ( 'NONE',  ( 1.000000000000000000, 0.000000000000000000, -0.000000000000000000 ) ) ;
#37373 = VECTOR ( 'NONE', #8724, 999.9999999999998863 ) ;
#37374 = CARTESIAN_POINT ( 'NONE',  ( 151.6178224291901415, 54.48737267587420519, 68.45106349240374755 ) ) ;
#37375 = DIRECTION ( 'NONE',  ( 0.000000000000000000, 0.000000000000000000, -1.000000000000000000 ) ) ;
#37376 = CARTESIAN_POINT ( 'NONE',  ( 151.6192474229130198, 53.24103268919207466, 5.366030440576345484 ) ) ;
#37377 = CARTESIAN_POINT ( 'NONE',  ( -9.123606769528260330, 7.986935641101333694, 83.88886893069803818 ) ) ;
#37378 = ORIENTED_EDGE ( 'NONE', *, *, #47604, .F. ) ;
#37380 = ADVANCED_FACE ( 'NONE', ( #34289 ), #66653, .T. ) ;
#37379 = CARTESIAN_POINT ( 'NONE',  ( -15.55634918610403439, 0.000000000000000000, 0.000000000000000000 ) ) ;
#37381 = ADVANCED_FACE ( 'NONE', ( #57462 ), #26489, .T. ) ;
#37382 = LINE ( 'NONE', #10652, #49561 ) ;
#37383 = VERTEX_POINT ( 'NONE', #46906 ) ;
#37384 = EDGE_CURVE ( 'NONE', #51166, #16495, #47576, .T. ) ;
#37385 = VERTEX_POINT ( 'NONE', #62397 ) ;
#37386 = CARTESIAN_POINT ( 'NONE',  ( 45.80999061969644970, 10.34829880103435507, 94.99999999999866418 ) ) ;
#37387 = CARTESIAN_POINT ( 'NONE',  ( -25.87147652227456263, 100.0000000000000000, 77.58025477438755502 ) ) ;
#37388 = LINE ( 'NONE', #36721, #48177 ) ;
#37389 = ORIENTED_EDGE ( 'NONE', *, *, #40906, .F. ) ;
#37390 = EDGE_CURVE ( 'NONE', #65127, #65221, #4002, .T. ) ;
#37391 = CARTESIAN_POINT ( 'NONE',  ( -56.02027488966933078, 14.94257193099085868, -62.10801344035115790 ) ) ;
#37392 = CARTESIAN_POINT ( 'NONE',  ( -4.731197926646204088, 7.716745361328044339, 3.934633056432215614 ) ) ;
#37393 = EDGE_CURVE ( 'NONE', #31642, #55255, #51835, .T. ) ;
#37394 = CARTESIAN_POINT ( 'NONE',  ( 174.4978817191264682, 73.57770570413205746, -47.32325019632195762 ) ) ;
#37395 = CARTESIAN_POINT ( 'NONE',  ( -152.2873556200145799, 67.91256772393732888, -76.12667896378731314 ) ) ;
#37396 = CARTESIAN_POINT ( 'NONE',  ( 15.55634918610397399, -26.11269837220809364, 2.000000000000001776 ) ) ;
#37397 = ORIENTED_EDGE ( 'NONE', *, *, #2556, .T. ) ;
#37398 = DIRECTION ( 'NONE',  ( 0.000000000000000000, -0.000000000000000000, 1.000000000000000000 ) ) ;
#37399 = VECTOR ( 'NONE', #33749, 1000.000000000000114 ) ;
#37400 = DIRECTION ( 'NONE',  ( 0.000000000000000000, 0.000000000000000000, -1.000000000000000000 ) ) ;
#37401 = CARTESIAN_POINT ( 'NONE',  ( 9.050324533885207856, 7.384616180193988910, 34.18438138347604394 ) ) ;
#37402 = PLANE ( 'NONE',  #22575 ) ;
#37403 = FACE_OUTER_BOUND ( 'NONE', #40618, .T. ) ;
#37405 = VERTEX_POINT ( 'NONE', #68371 ) ;
#37404 = FACE_OUTER_BOUND ( 'NONE', #7832, .T. ) ;
#37406 = ORIENTED_EDGE ( 'NONE', *, *, #11199, .F. ) ;
#37407 = VECTOR ( 'NONE', #47539, 1000.000000000000000 ) ;
#37408 = ADVANCED_FACE ( 'NONE', ( #3647 ), #46552, .T. ) ;
#37409 = EDGE_CURVE ( 'NONE', #772, #54998, #53195, .T. ) ;
#37410 = ORIENTED_EDGE ( 'NONE', *, *, #66424, .T. ) ;
#37411 = VECTOR ( 'NONE', #16058, 1000.000000000000000 ) ;
#37412 = FACE_OUTER_BOUND ( 'NONE', #48634, .T. ) ;
#37413 = DIRECTION ( 'NONE',  ( -1.000000000000000000, 0.000000000000000000, 0.000000000000000000 ) ) ;
#37414 = ADVANCED_FACE ( 'NONE', ( #26144 ), #68033, .F. ) ;
#37415 = AXIS2_PLACEMENT_3D ( 'NONE', #49684, #22978, #7140 ) ;
#37416 = DIRECTION ( 'NONE',  ( 1.000000000000000000, 0.000000000000000000, 0.000000000000000000 ) ) ;
#37417 = DIRECTION ( 'NONE',  ( 0.000000000000000000, 1.000000000000000000, -0.000000000000000000 ) ) ;
#37418 = CARTESIAN_POINT ( 'NONE',  ( 150.5550643769628039, 52.46819381604268528, -73.38422485962182407 ) ) ;
#37419 = CARTESIAN_POINT ( 'NONE',  ( 22.29513692215318343, 6.796052026456518291, -19.93622960288293200 ) ) ;
#37420 = AXIS2_PLACEMENT_3D ( 'NONE', #50792, #44828, #18787 ) ;
#37421 = CYLINDRICAL_SURFACE ( 'NONE', #64343, 7.500000000000013323 ) ;
#37422 = ORIENTED_EDGE ( 'NONE', *, *, #19381, .F. ) ;
#37423 = ORIENTED_EDGE ( 'NONE', *, *, #23615, .T. ) ;
#37424 = LINE ( 'NONE', #4395, #69082 ) ;
#37425 = B_SPLINE_CURVE_WITH_KNOTS ( 'NONE', 3,
 ( #11583, #58393, #53452, #5284, #43243, #43599, #59769, #21128, #42899, #32025, #11240, #42572, #26742, #32708, #64361, #53107, #59428, #48511, #22155, #27420, #54493, #15838, #16530, #38325, #340, #22502, #32370, #15505, #43939, #58731, #16177, #27774, #49216, #5617, #64029, #64719, #65068, #37632, #16867, #59081, #37281, #10899, #37985, #1051 ),
 .UNSPECIFIED., .F., .F.,
 ( 4, 2, 2, 2, 2, 2, 2, 2, 2, 2, 2, 2, 2, 2, 2, 2, 2, 2, 2, 2, 2, 4 ),
 ( 1.430489624538199204E-17, 0.001482469635030033046, 0.002223704452545043064, 0.002964939270060053082, 0.004447408905090053169, 0.005929878540120054123, 0.007412348175150054209, 0.008153582992665062493, 0.008894817810180068174, 0.01037728744521007954, 0.01185975708024009263, 0.01260099189775507923, 0.01334222671527006236, 0.01482469635030007372, 0.01556593116781507594, 0.01630716598533007641, 0.01778963562036007043, 0.01927210525539006097, 0.02001334007290505798, 0.02075457489042005152, 0.02223704452545007329, 0.02371951416048009159 ),
 .UNSPECIFIED. ) ;
#37426 = CARTESIAN_POINT ( 'NONE',  ( -62.33646982747445264, 17.80738194613631364, -94.56263670386991294 ) ) ;
#37427 = VECTOR ( 'NONE', #44172, 1000.000000000000000 ) ;
#37428 = CARTESIAN_POINT ( 'NONE',  ( -23.94843400007326295, 9.496257175156115338, 91.90182630676891051 ) ) ;
#37429 = CARTESIAN_POINT ( 'NONE',  ( 116.8917656767876281, 33.20682060519246903, -13.09834932968690246 ) ) ;
#37430 = CARTESIAN_POINT ( 'NONE',  ( 185.1802655733641529, 82.84606286178495793, -37.42643899651594808 ) ) ;
#37431 = CARTESIAN_POINT ( 'NONE',  ( 23.03578842369135060, 6.840884649289439956, 35.56935612319515627 ) ) ;
#37432 = DIRECTION ( 'NONE',  ( -9.109522253334613014E-16, -1.000000000000000000, 3.889846672687432470E-31 ) ) ;
#37433 = VERTEX_POINT ( 'NONE', #41628 ) ;
#37434 = ORIENTED_EDGE ( 'NONE', *, *, #67514, .F. ) ;
#37435 = ORIENTED_EDGE ( 'NONE', *, *, #60991, .F. ) ;
#37436 = CARTESIAN_POINT ( 'NONE',  ( -156.3734885497381697, 71.59531449004288106, -18.49822134472886148 ) ) ;
#37437 = CARTESIAN_POINT ( 'NONE',  ( 33.31166872005966439, 8.707041209322245123, -47.50374935772406104 ) ) ;
#37438 = CARTESIAN_POINT ( 'NONE',  ( -31.92580063159127590, 9.671320706097198183, 57.06100499665285497 ) ) ;
#37439 = CARTESIAN_POINT ( 'NONE',  ( 39.40195752203892710, -170.0000000000000000, 64.25838489642696061 ) ) ;
#37440 = VERTEX_POINT ( 'NONE', #52183 ) ;
#37441 = LINE ( 'NONE', #27585, #12052 ) ;
#37442 = CARTESIAN_POINT ( 'NONE',  ( 157.4703587214989113, 58.92748579479258808, 2.564916881789689462 ) ) ;
#37443 = SHAPE_REPRESENTATION_RELATIONSHIP ( 'NONE' , 'NONE' ,  #36585, #61784 ) ;
#37444 = CARTESIAN_POINT ( 'NONE',  ( 20.36233635256088093, 7.697399815318435756, 4.706382148416831335 ) ) ;
#37445 =( NAMED_UNIT ( * ) PLANE_ANGLE_UNIT ( ) SI_UNIT ( $, .RADIAN. ) );
#37446 = FACE_OUTER_BOUND ( 'NONE', #1338, .T. ) ;
#37447 = CARTESIAN_POINT ( 'NONE',  ( -85.91089317961402116, 25.21459833389209848, -44.62272628199698232 ) ) ;
#37448 = CARTESIAN_POINT ( 'NONE',  ( 20.37135563017389117, 6.690359945346087578, 70.31641744500336699 ) ) ;
#37449 = CARTESIAN_POINT ( 'NONE',  ( 10.55634918610409656, 36.11269837220803680, 85.00100000000000477 ) ) ;
#37450 = CARTESIAN_POINT ( 'NONE',  ( 13.37366753069833436, 6.435102282077987290, -76.98119335383468353 ) ) ;
#37451 = ADVANCED_FACE ( 'NONE', ( #36707 ), #14887, .F. ) ;
#37452 = ORIENTED_EDGE ( 'NONE', *, *, #3257, .F. ) ;
#37454 = CARTESIAN_POINT ( 'NONE',  ( -8.000000000000000000, 0.7809653281576027783, 9.834052517622422992E-16 ) ) ;
#37453 = CIRCLE ( 'NONE', #4875, 21.00000000000000355 ) ;
#37455 = APPLICATION_PROTOCOL_DEFINITION ( 'draft international standard', 'automotive_design', 1998, #44923 ) ;
#37456 = DIRECTION ( 'NONE',  ( 1.000000000000000000, -0.000000000000000000, -0.000000000000000000 ) ) ;
#37457 = DIRECTION ( 'NONE',  ( 0.000000000000000000, -1.000000000000000000, 0.000000000000000000 ) ) ;
#37458 = CARTESIAN_POINT ( 'NONE',  ( -103.2061297292849389, 34.38496953192504435, -49.97177337113672735 ) ) ;
#37459 = CARTESIAN_POINT ( 'NONE',  ( 57.41085175769455873, 12.46982565415946986, -75.05494575928295831 ) ) ;
#37460 = ORIENTED_EDGE ( 'NONE', *, *, #69237, .F. ) ;
#37461 = VECTOR ( 'NONE', #17900, 1000.000000000000000 ) ;
#37462 = EDGE_LOOP ( 'NONE', ( #58240, #17195, #42377, #20538 ) ) ;
#37463 = AXIS2_PLACEMENT_3D ( 'NONE', #67065, #3977, #57785 ) ;
#37465 = EDGE_CURVE ( 'NONE', #59098, #48854, #62748, .T. ) ;
#37464 = CARTESIAN_POINT ( 'NONE',  ( -23.93965512371324422, 8.480096402797085986, -16.47769234035476771 ) ) ;
#37466 = VECTOR ( 'NONE', #26490, 1000.000000000000000 ) ;
#37467 = CARTESIAN_POINT ( 'NONE',  ( 201.5876148766343761, 103.8397408698165520, 16.70131438898428300 ) ) ;
#37468 = VERTEX_POINT ( 'NONE', #14211 ) ;
#37469 = VERTEX_POINT ( 'NONE', #14550 ) ;
#37470 = VECTOR ( 'NONE', #48779, 1000.000000000000000 ) ;
#37471 = EDGE_CURVE ( 'NONE', #417, #35550, #9629, .T. ) ;
#37472 = CARTESIAN_POINT ( 'NONE',  ( 117.3281529665581928, 32.29994712002883261, 66.46847310579148882 ) ) ;
#37473 = VERTEX_POINT ( 'NONE', #36009 ) ;
#37474 = CARTESIAN_POINT ( 'NONE',  ( 113.4402889550712672, 31.50582881646777622, 70.75682576111141486 ) ) ;
#37475 = DIRECTION ( 'NONE',  ( -0.1342332658176522420, -0.9909497617679352555, 0.000000000000000000 ) ) ;
#37476 = EDGE_CURVE ( 'NONE', #3161, #6104, #5774, .T. ) ;
#37477 = CARTESIAN_POINT ( 'NONE',  ( 141.3556389957210229, 47.34429831367556574, 64.15079552814040653 ) ) ;
#37478 = CARTESIAN_POINT ( 'NONE',  ( 0.000000000000000000, -2.000000000000000000, -0.000000000000000000 ) ) ;
#37479 = VECTOR ( 'NONE', #62644, 1000.000000000000000 ) ;
#37480 = ADVANCED_FACE ( 'NONE', ( #63434 ), #10294, .F. ) ;
#37481 = CARTESIAN_POINT ( 'NONE',  ( 162.8721509409114105, 61.97589144837539976, -92.09519880210693543 ) ) ;
#37482 = CARTESIAN_POINT ( 'NONE',  ( 92.19920907511531993, 21.39700525884452986, -48.36761472064368661 ) ) ;
#37483 = CARTESIAN_POINT ( 'NONE',  ( 5.799999999999999822, -9.237604307034018802, 3.355146209984123968E-17 ) ) ;
#37484 = ORIENTED_EDGE ( 'NONE', *, *, #42402, .T. ) ;
#37485 = EDGE_LOOP ( 'NONE', ( #61601, #3341, #42407, #12665 ) ) ;
#37486 = CARTESIAN_POINT ( 'NONE',  ( -122.3963566076408256, 44.23346594671848209, -22.22042909780819642 ) ) ;
#37487 = FACE_OUTER_BOUND ( 'NONE', #7988, .T. ) ;
#37488 = CARTESIAN_POINT ( 'NONE',  ( -180.0175713311536185, 95.14770835574074681, -18.32925981149572081 ) ) ;
#37489 = B_SPLINE_CURVE_WITH_KNOTS ( 'NONE', 3,
 ( #19026, #30627, #8833, #62639, #14781, #47132, #51731, #13749, #30975, #40478, #41179, #35207, #68595, #29930, #36245, #25361, #51396, #3209, #57702, #41522, #9166, #24664, #20400, #3889, #46099, #62282, #35903, #67568, #19368, #46796, #41869, #40826, #14448, #52073, #14097, #68265, #20068, #62975, #63325, #29575, #15133, #36595, #51041, #58041 ),
 .UNSPECIFIED., .F., .F.,
 ( 4, 2, 2, 2, 2, 2, 2, 2, 2, 2, 2, 2, 2, 2, 2, 2, 2, 2, 2, 2, 2, 4 ),
 ( 0.02477387709520258857, 0.02633314402883777869, 0.02711277749565536854, 0.02789241096247295840, 0.02945167789610817974, 0.03023131136292576959, 0.03101094482974336292, 0.03257021176337852875, 0.03334984523019610125, 0.03412947869701367376, 0.03568874563064881877, 0.03646837909746639128, 0.03724801256428395685, 0.03802764603110153629, 0.03880727949791912268, 0.04036654643155428851, 0.04192581336518945434, 0.04348508029882461323, 0.04504434723245977212, 0.04660361416609493795, 0.04816288109973010378, 0.04972214803336526268 ),
 .UNSPECIFIED. ) ;
#37490 = CARTESIAN_POINT ( 'NONE',  ( -165.9154624515709884, 80.89088623112731113, -66.95487838069742281 ) ) ;
#37492 = ORIENTED_EDGE ( 'NONE', *, *, #46593, .T. ) ;
#37491 = CARTESIAN_POINT ( 'NONE',  ( -145.5261806899007411, 60.87473129144527917, -48.67308456771189640 ) ) ;
#37493 = CARTESIAN_POINT ( 'NONE',  ( 57.39233401791015865, 12.46575990788836918, 15.45527492068149122 ) ) ;
#37494 = ORIENTED_EDGE ( 'NONE', *, *, #14142, .F. ) ;
#37495 = CARTESIAN_POINT ( 'NONE',  ( 442.3372781065085633, 392.9289321881414594, -141.4497041420116261 ) ) ;
#37496 = DIRECTION ( 'NONE',  ( -0.000000000000000000, 1.000000000000000000, -0.000000000000000000 ) ) ;
#37497 = EDGE_CURVE ( 'NONE', #40354, #5206, #12579, .T. ) ;
#37498 = CARTESIAN_POINT ( 'NONE',  ( 86.62931800182293784, 19.42108912189597447, -23.97701360844805407 ) ) ;
#37499 = CARTESIAN_POINT ( 'NONE',  ( -126.3453033442920344, 47.99870040347948930, -76.75825448869764500 ) ) ;
#37501 = CARTESIAN_POINT ( 'NONE',  ( 62.60845276312630858, 12.57833377949302189, -89.40979201309711755 ) ) ;
#37500 = AXIS2_PLACEMENT_3D ( 'NONE', #6778, #38445, #1504 ) ;
#37502 = PLANE ( 'NONE',  #12295 ) ;
#37503 = CARTESIAN_POINT ( 'NONE',  ( -96.43148989374459745, 29.90755650959362910, -64.63752141125630146 ) ) ;
#37504 = VERTEX_POINT ( 'NONE', #19476 ) ;
#37505 = ORIENTED_EDGE ( 'NONE', *, *, #7716, .F. ) ;
#37506 = VECTOR ( 'NONE', #55354, 1000.000000000000114 ) ;
#37507 = CARTESIAN_POINT ( 'NONE',  ( 182.5617509987553717, 80.11195108039724744, -77.92569941903248321 ) ) ;
#37508 = CARTESIAN_POINT ( 'NONE',  ( 0.000000000000000000, 0.000000000000000000, 170.0000000000000000 ) ) ;
#37509 = CARTESIAN_POINT ( 'NONE',  ( -165.7143741370936709, 79.24519349471955820, -43.42972967134339513 ) ) ;
#37510 = LINE ( 'NONE', #58963, #30656 ) ;
#37511 = CIRCLE ( 'NONE', #38626, 89.99999999999998579 ) ;
#37512 = DIRECTION ( 'NONE',  ( -1.000000000000000000, 0.000000000000000000, 0.000000000000000000 ) ) ;
#37513 = CARTESIAN_POINT ( 'NONE',  ( -71.86568654225716557, 20.91200104397925230, 34.74601522620152849 ) ) ;
#37514 = CARTESIAN_POINT ( 'NONE',  ( 80.16939877002758408, 17.31693935407229290, 41.05451173327999470 ) ) ;
#37515 = CARTESIAN_POINT ( 'NONE',  ( -71.69927128652682313, 36.58596684574255420, -74.30072871347312002 ) ) ;
#37516 = CIRCLE ( 'NONE', #7206, 54.99999999999995026 ) ;
#37517 = CARTESIAN_POINT ( 'NONE',  ( 43.14669449386823175, 9.942681284149132992, -36.60324319909982194 ) ) ;
#37518 = DIRECTION ( 'NONE',  ( 1.110223024625156294E-16, 3.697785493223491743E-32, -1.000000000000000000 ) ) ;
#37519 = VERTEX_POINT ( 'NONE', #40937 ) ;
#37520 = CARTESIAN_POINT ( 'NONE',  ( -107.7743374187917027, 35.66028478413600311, -10.54119851968185095 ) ) ;
#37521 = ORIENTED_EDGE ( 'NONE', *, *, #63944, .T. ) ;
#37522 = CARTESIAN_POINT ( 'NONE',  ( -15.26524495591509023, 7.490231452641286758, -43.89783010401615115 ) ) ;
#37523 = VECTOR ( 'NONE', #4106, 1000.000000000000000 ) ;
#37524 = CARTESIAN_POINT ( 'NONE',  ( 0.000000000000000000, 0.000000000000000000, 0.000000000000000000 ) ) ;
#37525 = LINE ( 'NONE', #5516, #29591 ) ;
#37526 = CARTESIAN_POINT ( 'NONE',  ( 110.7117404013331026, 30.20916032354564251, 2.766663615273644350 ) ) ;
#37527 = CARTESIAN_POINT ( 'NONE',  ( 99.99999999999997158, 6.000000000000000000, -25.00000000000000000 ) ) ;
#37528 = DIRECTION ( 'NONE',  ( 1.000000000000000000, 0.000000000000000000, 0.000000000000000000 ) ) ;
#37529 = VECTOR ( 'NONE', #6747, 1000.000000000000000 ) ;
#37530 = CARTESIAN_POINT ( 'NONE',  ( -102.2801239173131052, 33.91021738430207222, -8.170026674512225640 ) ) ;
#37531 = VERTEX_POINT ( 'NONE', #42320 ) ;
#37532 = CARTESIAN_POINT ( 'NONE',  ( 210.6189312023034574, 114.8321746285510301, 94.99999999999866418 ) ) ;
#37533 = DIRECTION ( 'NONE',  ( -0.000000000000000000, -1.000000000000000000, -0.000000000000000000 ) ) ;
#37534 = ORIENTED_EDGE ( 'NONE', *, *, #31683, .F. ) ;
#37535 = CARTESIAN_POINT ( 'NONE',  ( 1.951563910473907981E-14, 0.000000000000000000, -146.4497041420118251 ) ) ;
#37536 = CARTESIAN_POINT ( 'NONE',  ( 13.84704553156522167, 7.452804552247572545, -77.11207471772274857 ) ) ;
#37537 = DIRECTION ( 'NONE',  ( 1.000000000000000000, 0.000000000000000000, 0.000000000000000000 ) ) ;
#37538 = EDGE_CURVE ( 'NONE', #39848, #1555, #63784, .T. ) ;
#37539 = CARTESIAN_POINT ( 'NONE',  ( 110.2429982417149574, -170.0000000000000000, 37.11121420573731911 ) ) ;
#37541 = EDGE_CURVE ( 'NONE', #37939, #54242, #55901, .T. ) ;
#37540 = CARTESIAN_POINT ( 'NONE',  ( -7.825402957745083654, 6.891034867348166060, 30.11558103944718923 ) ) ;
#37542 = PLANE ( 'NONE',  #55804 ) ;
#37543 = CARTESIAN_POINT ( 'NONE',  ( 91.71454558664912327, 22.29094817986854693, 85.37844496027901187 ) ) ;
#37544 = EDGE_CURVE ( 'NONE', #38316, #15138, #67612, .T. ) ;
#37545 = VERTEX_POINT ( 'NONE', #48600 ) ;
#37546 = EDGE_CURVE ( 'NONE', #20826, #50073, #33514, .T. ) ;
#37547 = DIRECTION ( 'NONE',  ( 1.000000000000000000, 0.000000000000000000, 0.000000000000000000 ) ) ;
#37548 = LINE ( 'NONE', #16781, #35170 ) ;
#37549 = CARTESIAN_POINT ( 'NONE',  ( 0.000000000000000000, 190.0000000000000000, 0.000000000000000000 ) ) ;
#37550 = B_SPLINE_CURVE_WITH_KNOTS ( 'NONE', 3,
 ( #46772, #45387, #67547, #35181, #56286, #51019, #29552, #8456, #3868, #34510, #30260, #2828, #25335, #67218, #69163, #56990, #20988, #41157, #19345, #29909, #50663, #24297, #24643, #46076, #13388, #63896, #62256, #40456, #14071, #35536, #67897, #62617, #8808, #51709, #3515, #24986 ),
 .UNSPECIFIED., .F., .F.,
 ( 4, 2, 2, 2, 2, 2, 2, 2, 2, 2, 2, 2, 2, 2, 2, 2, 2, 4 ),
 ( 0.000000000000000000, 0.001548367318450182602, 0.003096734636900365205, 0.004645101955350548241, 0.006193469273800730410, 0.007741836592250906507, 0.008516020251475981545, 0.009290203910701058318, 0.01083857122915121186, 0.01238693854760136194, 0.01393530586605151375, 0.01548367318450166730, 0.01703204050295181737, 0.01858040782140197092, 0.02012877513985212447, 0.02167714245830228148, 0.02322550977675243503, 0.02477387709520259204 ),
 .UNSPECIFIED. ) ;
#37551 = CARTESIAN_POINT ( 'NONE',  ( -102.7447593990059147, 34.14748189312169302, 57.36362509687879907 ) ) ;
#37552 = CARTESIAN_POINT ( 'NONE',  ( -132.6092625803567273, 52.31125232006264270, -39.06397555526168475 ) ) ;
#37553 = EDGE_LOOP ( 'NONE', ( #64871, #22580, #47044, #57090, #45136, #58921, #45334, #40375, #49915 ) ) ;
#37554 = CARTESIAN_POINT ( 'NONE',  ( 299.8372781065085064, 399.9999999999998863, -33.94970414201181796 ) ) ;
#37555 = CARTESIAN_POINT ( 'NONE',  ( -7.825402957745083654, 6.891034867348163395, -23.57352014148015584 ) ) ;
#37556 = CARTESIAN_POINT ( 'NONE',  ( 199.9103251464698872, 101.6434290204575319, -11.20346956314359943 ) ) ;
#37557 = DIRECTION ( 'NONE',  ( -0.000000000000000000, -1.000000000000000000, -0.000000000000000000 ) ) ;
#37558 = EDGE_CURVE ( 'NONE', #25097, #2530, #438, .T. ) ;
#37559 = CARTESIAN_POINT ( 'NONE',  ( 134.7697261969508986, 41.97802808873667857, 29.55217423902721663 ) ) ;
#37560 = EDGE_CURVE ( 'NONE', #38758, #44050, #201, .T. ) ;
#37561 = ORIENTED_EDGE ( 'NONE', *, *, #23968, .F. ) ;
#37562 = CYLINDRICAL_SURFACE ( 'NONE', #62671, 60.00000000000000000 ) ;
#37563 = CARTESIAN_POINT ( 'NONE',  ( 84.97658021689284169, 19.92447159015900837, 3.047988274556576727 ) ) ;
#37564 = ADVANCED_FACE ( 'NONE', ( #12042 ), #32113, .F. ) ;
#37566 = CARTESIAN_POINT ( 'NONE',  ( 164.1338586910085837, 64.33646242148860495, 13.51726694518641381 ) ) ;
#37565 = B_SPLINE_CURVE_WITH_KNOTS ( 'NONE', 3,
 ( #42379, #30798, #52245, #25532, #37100, #58541, #51564, #14275, #3373, #24827, #46268, #19543, #41006, #38132, #5769, #16337, #31826, #26552, #148, #37436, #43054, #5087, #60294, #32862, #59927, #64878, #857, #33225, #22655, #21957, #47985, #65579, #54295, #64173, #48316, #43404, #53610, #69451, #17371, #37791, #27931, #21608, #27579, #11053, #21267, #6118, #16678, #17014 ),
 .UNSPECIFIED., .F., .F.,
 ( 4, 2, 2, 2, 2, 2, 2, 2, 2, 2, 2, 2, 2, 2, 2, 2, 2, 2, 2, 2, 2, 2, 2, 4 ),
 ( 0.02698595842317762575, 0.02784423243973407555, 0.02870250645629052189, 0.03041905448940333129, 0.03127732850595971864, 0.03213560252251611293, 0.03385215055562888764, 0.03471042457218524030, 0.03556869858874159990, 0.03728524662185429828, 0.03814352063841063012, 0.03900179465496696196, 0.03986006867152329380, 0.04071834268807963259, 0.04157661670463596443, 0.04243489072119230321, 0.04415143875430497383, 0.04500971277086131261, 0.04586798678741765833, 0.04758453482053030814, 0.04930108285364295795, 0.05101763088675561469, 0.05273417891986827144, 0.05445072695298092125 ),
 .UNSPECIFIED. ) ;
#37567 = CARTESIAN_POINT ( 'NONE',  ( -20.93485882276955579, 13.66498028065538861, 0.000000000000000000 ) ) ;
#37568 = AXIS2_PLACEMENT_3D ( 'NONE', #45333, #34101, #2095 ) ;
#37569 = EDGE_LOOP ( 'NONE', ( #7820, #45569, #34490, #35920 ) ) ;
#37570 = VECTOR ( 'NONE', #38307, 1000.000000000000114 ) ;
#37571 = DIRECTION ( 'NONE',  ( 1.000000000000000000, -0.000000000000000000, 0.000000000000000000 ) ) ;
#37572 = CIRCLE ( 'NONE', #60115, 245.3095347406802205 ) ;
#37573 = VERTEX_POINT ( 'NONE', #5378 ) ;
#37574 = CARTESIAN_POINT ( 'NONE',  ( -108.6909373351217596, 36.15835109565443162, -46.43893206896224513 ) ) ;
#37575 = CARTESIAN_POINT ( 'NONE',  ( 63.98009977735161158, 12.89803120691696670, -77.51887576910404221 ) ) ;
#37576 = VECTOR ( 'NONE', #69486, 1000.000000000000000 ) ;
#37577 = CARTESIAN_POINT ( 'NONE',  ( -59.36813706141739999, 15.88103696331963377, 43.95624469312958382 ) ) ;
#37579 = ORIENTED_EDGE ( 'NONE', *, *, #42065, .T. ) ;
#37578 = CARTESIAN_POINT ( 'NONE',  ( 63.58578643762691485, 0.000000000000000000, 41.41421356237313489 ) ) ;
#37580 = CARTESIAN_POINT ( 'NONE',  ( 26.99999999999999645, 26.99999999999999645, 15.00000000000000000 ) ) ;
#37581 = CARTESIAN_POINT ( 'NONE',  ( -74.81012118577227454, 5.477980300262931479, 43.58025477438756923 ) ) ;
#37582 = DIRECTION ( 'NONE',  ( 0.000000000000000000, 0.000000000000000000, 1.000000000000000000 ) ) ;
#37583 = VERTEX_POINT ( 'NONE', #32801 ) ;
#37584 = DIRECTION ( 'NONE',  ( 1.000000000000000000, 0.000000000000000000, 0.000000000000000000 ) ) ;
#37585 = DIRECTION ( 'NONE',  ( -8.784520486427686400E-17, -2.340627113153429324E-16, 1.000000000000000000 ) ) ;
#37586 = CARTESIAN_POINT ( 'NONE',  ( -166.2028657618940883, 79.74389853943291939, 41.23225120243120756 ) ) ;
#37587 = CARTESIAN_POINT ( 'NONE',  ( 126.3554864210862121, 38.22801630372152459, 64.08286055307904405 ) ) ;
#37588 = EDGE_LOOP ( 'NONE', ( #50033, #12021, #36857, #67573 ) ) ;
#37589 = VERTEX_POINT ( 'NONE', #59171 ) ;
#37590 = ORIENTED_EDGE ( 'NONE', *, *, #40010, .T. ) ;
#37591 = SURFACE_STYLE_USAGE ( .BOTH. , #53066 ) ;
#37592 = FACE_OUTER_BOUND ( 'NONE', #66267, .T. ) ;
#37593 = DIRECTION ( 'NONE',  ( 8.893845946170152056E-21, -1.110223024625156294E-16, 1.000000000000000000 ) ) ;
#37594 = CARTESIAN_POINT ( 'NONE',  ( 70.52164504723299387, 14.53981718869930084, 90.84488468013880436 ) ) ;
#37595 = PLANE ( 'NONE',  #39315 ) ;
#37596 = CARTESIAN_POINT ( 'NONE',  ( -24.09190246691234805, 8.500289797445409690, -95.00000000000133582 ) ) ;
#37597 = CARTESIAN_POINT ( 'NONE',  ( 18.07314801315378006, 17.44990292519104003, 3.061616997868437868E-16 ) ) ;
#37598 = ORIENTED_EDGE ( 'NONE', *, *, #19864, .T. ) ;
#37599 = AXIS2_PLACEMENT_3D ( 'NONE', #19604, #55865, #18224 ) ;
#37600 = DIRECTION ( 'NONE',  ( 1.000000000000000000, 0.000000000000000000, 0.000000000000000000 ) ) ;
#37601 = ORIENTED_EDGE ( 'NONE', *, *, #17794, .F. ) ;
#37602 = CARTESIAN_POINT ( 'NONE',  ( -73.09214866197369531, 21.34321757515763807, 59.72063747903552411 ) ) ;
#37603 = CARTESIAN_POINT ( 'NONE',  ( 209.6525588430077960, 113.3929734759396695, -76.30558542174757974 ) ) ;
#37604 = CARTESIAN_POINT ( 'NONE',  ( 0.000000000000000000, 0.000000000000000000, 0.000000000000000000 ) ) ;
#37606 = LINE ( 'NONE', #5593, #23710 ) ;
#37605 = VECTOR ( 'NONE', #26092, 1000.000000000000000 ) ;
#37607 = CARTESIAN_POINT ( 'NONE',  ( -37.22864127331250472, 10.61359798105728913, -91.73382525222255879 ) ) ;
#37608 = CARTESIAN_POINT ( 'NONE',  ( 22.51798020284706325, 7.817376421459703018, 34.19479625308969872 ) ) ;
#37609 = DIRECTION ( 'NONE',  ( -0.000000000000000000, 1.000000000000000000, -0.000000000000000000 ) ) ;
#37610 = CARTESIAN_POINT ( 'NONE',  ( -20.63749999999999574, 3.061616997868383831E-15, 25.00000000000000711 ) ) ;
#37611 = VECTOR ( 'NONE', #59940, 1000.000000000000000 ) ;
#37612 = ORIENTED_EDGE ( 'NONE', *, *, #37086, .T. ) ;
#37613 = DIRECTION ( 'NONE',  ( -1.000000000000000000, 0.000000000000000000, 0.000000000000000000 ) ) ;
#37614 = CARTESIAN_POINT ( 'NONE',  ( 100.0000000000000284, 0.000000000000000000, 0.000000000000000000 ) ) ;
#37615 = EDGE_LOOP ( 'NONE', ( #53102, #21005 ) ) ;
#37616 = EDGE_LOOP ( 'NONE', ( #49149, #55927, #48762, #48991 ) ) ;
#37617 = VECTOR ( 'NONE', #16121, 1000.000000000000000 ) ;
#37619 = EDGE_CURVE ( 'NONE', #47435, #8388, #794, .T. ) ;
#37618 = CARTESIAN_POINT ( 'NONE',  ( -24.60892750534350526, 9.584951112520235128, -72.76977437635076740 ) ) ;
#37620 = CARTESIAN_POINT ( 'NONE',  ( 55.52750043885181697, 11.05966813607792254, -43.71057030527602905 ) ) ;
#37621 =( NAMED_UNIT ( * ) SI_UNIT ( $, .STERADIAN. ) SOLID_ANGLE_UNIT ( ) );
#37622 = CIRCLE ( 'NONE', #7317, 89.99999999999998579 ) ;
#37623 = CARTESIAN_POINT ( 'NONE',  ( -147.7860806339124906, 62.73248524776227697, 4.063553114042554704 ) ) ;
#37624 = EDGE_CURVE ( 'NONE', #1332, #47869, #42724, .T. ) ;
#37625 = ORIENTED_EDGE ( 'NONE', *, *, #50831, .T. ) ;
#37626 = EDGE_CURVE ( 'NONE', #56020, #20206, #8152, .T. ) ;
#37627 = EDGE_LOOP ( 'NONE', ( #6468, #60078, #59176, #13520 ) ) ;
#37628 = DIRECTION ( 'NONE',  ( -1.000000000000000000, -0.000000000000000000, 0.000000000000000000 ) ) ;
#37629 = ORIENTED_EDGE ( 'NONE', *, *, #51624, .F. ) ;
#37630 = DIRECTION ( 'NONE',  ( 0.000000000000000000, 0.000000000000000000, -1.000000000000000000 ) ) ;
#37631 = CARTESIAN_POINT ( 'NONE',  ( -142.3187766126155225, 59.59460822661993262, 36.01124715683158684 ) ) ;
#37632 = CARTESIAN_POINT ( 'NONE',  ( 59.72897338775219112, 11.93428797217974946, 57.41156910716014750 ) ) ;
#37633 = CARTESIAN_POINT ( 'NONE',  ( 133.8566784816069344, -170.0000000000000000, -70.36786152285935714 ) ) ;
#37634 = LINE ( 'NONE', #16533, #45956 ) ;
#37635 = CARTESIAN_POINT ( 'NONE',  ( 0.000000000000000000, 0.000000000000000000, 0.000000000000000000 ) ) ;
#37636 = EDGE_CURVE ( 'NONE', #38916, #22933, #36127, .T. ) ;
#37637 = DIRECTION ( 'NONE',  ( 0.9195277725514489076, 0.3930250316539278810, -2.126835218476880762E-16 ) ) ;
#37638 = ORIENTED_EDGE ( 'NONE', *, *, #15336, .T. ) ;
#37639 = EDGE_LOOP ( 'NONE', ( #8081, #8282, #61240, #41098 ) ) ;
#37640 = CARTESIAN_POINT ( 'NONE',  ( 160.4963793545269084, 60.04225845346908841, -23.65658366629068254 ) ) ;
#37641 = CARTESIAN_POINT ( 'NONE',  ( -62.31345272479883590, -18.49415068377726357, 170.0000000000000000 ) ) ;
#37642 = DIRECTION ( 'NONE',  ( -1.000000000000000000, 0.000000000000000000, 0.000000000000000000 ) ) ;
#37643 = DIRECTION ( 'NONE',  ( 0.000000000000000000, -1.000000000000000000, 0.000000000000000000 ) ) ;
#37644 = CARTESIAN_POINT ( 'NONE',  ( 68.93219921887764201, 14.12322281954859982, 32.69723793727709449 ) ) ;
#37645 = CARTESIAN_POINT ( 'NONE',  ( -190.6985136298601731, 109.1272424661242582, -73.40678087856149148 ) ) ;
#37646 = ORIENTED_EDGE ( 'NONE', *, *, #363, .T. ) ;
#37647 = CARTESIAN_POINT ( 'NONE',  ( 80.73012746365752434, 17.49169339352364716, 15.02525433145232192 ) ) ;
#37648 = ORIENTED_EDGE ( 'NONE', *, *, #47796, .F. ) ;
#37649 = CARTESIAN_POINT ( 'NONE',  ( -72.78737098446268305, 20.16853011470087864, 33.23444075940503240 ) ) ;
#37650 = EDGE_LOOP ( 'NONE', ( #23564, #12583, #65016, #10034 ) ) ;
#37651 = VECTOR ( 'NONE', #62059, 1000.000000000000000 ) ;
#37652 = AXIS2_PLACEMENT_3D ( 'NONE', #54094, #658, #43429 ) ;
#37653 = VERTEX_POINT ( 'NONE', #40504 ) ;
#37654 = CARTESIAN_POINT ( 'NONE',  ( -121.1841775822198457, 44.65790002524552449, 5.417918675821312924 ) ) ;
#37655 = CARTESIAN_POINT ( 'NONE',  ( -18.24318075359480318, 17.27206262134385284, 3.061616997868437868E-16 ) ) ;
#37656 = CARTESIAN_POINT ( 'NONE',  ( 128.3856248084844651, 38.21741401878865219, 58.70131835549462096 ) ) ;
#37657 = AXIS2_PLACEMENT_3D ( 'NONE', #44647, #34798, #56236 ) ;
#37658 = VECTOR ( 'NONE', #59682, 1000.000000000000000 ) ;
#37659 = ORIENTED_EDGE ( 'NONE', *, *, #25756, .F. ) ;
#37660 = AXIS2_PLACEMENT_3D ( 'NONE', #44104, #55724, #49729 ) ;
#37661 = AXIS2_PLACEMENT_3D ( 'NONE', #28962, #32830, #54259 ) ;
#37662 = DIRECTION ( 'NONE',  ( 1.000000000000000000, 2.042810365310287719E-14, 0.000000000000000000 ) ) ;
#37663 = CARTESIAN_POINT ( 'NONE',  ( -173.1211646369891071, 88.63826465341152527, -61.55650775521367279 ) ) ;
#37664 = CONICAL_SURFACE ( 'NONE', #32053, 74.95140232871122521, 0.8777644062502172329 ) ;
#37665 = CARTESIAN_POINT ( 'NONE',  ( 70.51583798635768119, 15.57951509147424041, 37.07105218285969528 ) ) ;
#37666 = DIRECTION ( 'NONE',  ( -1.000000000000000000, 0.000000000000000000, 0.000000000000000000 ) ) ;
#37667 = DIRECTION ( 'NONE',  ( -1.000000000000000000, 0.000000000000000000, 0.000000000000000000 ) ) ;
#37668 = LINE ( 'NONE', #5650, #67577 ) ;
#37669 = DIRECTION ( 'NONE',  ( -0.000000000000000000, -0.000000000000000000, 1.000000000000000000 ) ) ;
#37670 = CARTESIAN_POINT ( 'NONE',  ( -142.1332311300253366, 59.44822332309654200, -70.55302544014286070 ) ) ;
#37671 = VERTEX_POINT ( 'NONE', #55289 ) ;
#37672 = DIRECTION ( 'NONE',  ( 0.000000000000000000, 1.000000000000000000, 0.000000000000000000 ) ) ;
#37673 = DIRECTION ( 'NONE',  ( 0.000000000000000000, 0.000000000000000000, 1.000000000000000000 ) ) ;
#37674 = CARTESIAN_POINT ( 'NONE',  ( -179.8989115484067440, 96.59045402602914976, 68.38918859239640824 ) ) ;
#37675 = CARTESIAN_POINT ( 'NONE',  ( 0.7145311798163228589, 4.618802153517005848, 8.000000000000000000 ) ) ;
#37676 = CARTESIAN_POINT ( 'NONE',  ( -102.2801239173131052, 32.78103895658057354, -61.85912785543958847 ) ) ;
#37677 = EDGE_CURVE ( 'NONE', #16122, #58159, #23305, .T. ) ;
#37678 = CARTESIAN_POINT ( 'NONE',  ( -85.75002235020436103, 26.23806300442549144, 13.55091505814834640 ) ) ;
#37679 = PLANE ( 'NONE',  #51695 ) ;
#37680 = CARTESIAN_POINT ( 'NONE',  ( 114.9679224117287646, 21.99264416388322374, 0.6532133356533591506 ) ) ;
#37681 = CARTESIAN_POINT ( 'NONE',  ( -124.1007047332778228, 46.52282960291164926, -76.55490961030825758 ) ) ;
#37682 = LINE ( 'NONE', #53505, #42203 ) ;
#37683 = CARTESIAN_POINT ( 'NONE',  ( -85.75002235020438945, 26.23806300442547723, 67.24001623907572878 ) ) ;
#37684 = CARTESIAN_POINT ( 'NONE',  ( 89.87840278991590992, 21.62393877508909767, -23.24105151053815632 ) ) ;
#37685 = ORIENTED_EDGE ( 'NONE', *, *, #14142, .T. ) ;
#37686 = CARTESIAN_POINT ( 'NONE',  ( -37.93983213483221562, 11.77368372188051282, 14.64435496287500449 ) ) ;
#37687 = EDGE_LOOP ( 'NONE', ( #39569, #14486, #9855, #69448 ) ) ;
#37688 = CARTESIAN_POINT ( 'NONE',  ( -46.06722295615789875, 46.37372919877053334, 43.58025477438756212 ) ) ;
#37689 = ORIENTED_EDGE ( 'NONE', *, *, #52016, .F. ) ;
#37690 = CARTESIAN_POINT ( 'NONE',  ( 19.10949903373832370, 7.636938177523840743, -76.59253534108344752 ) ) ;
#37691 = CARTESIAN_POINT ( 'NONE',  ( 113.6770630153551167, 31.62064605900739167, 84.12484067033027202 ) ) ;
#37692 = DIRECTION ( 'NONE',  ( -1.000000000000000000, 0.000000000000000000, 0.000000000000000000 ) ) ;
#37693 = CARTESIAN_POINT ( 'NONE',  ( 67.93926590385572695, 13.86859831467923598, -10.69750007213145082 ) ) ;
#37694 = CARTESIAN_POINT ( 'NONE',  ( -27.70115495247213389, 10.02455692117576369, -36.29670080177614011 ) ) ;
#37695 = CARTESIAN_POINT ( 'NONE',  ( -49.43836229152577033, 14.28302414152160082, -74.55831633533836111 ) ) ;
#37696 = CARTESIAN_POINT ( 'NONE',  ( -75.37792209610570637, 22.16719325496249482, -89.55030856586989785 ) ) ;
#37697 = CARTESIAN_POINT ( 'NONE',  ( 0.000000000000000000, 0.000000000000000000, 10.00000000000000000 ) ) ;
#37698 = VERTEX_POINT ( 'NONE', #22946 ) ;
#37699 = ADVANCED_FACE ( 'NONE', ( #39817 ), #51884, .T. ) ;
#37700 = ORIENTED_EDGE ( 'NONE', *, *, #55423, .F. ) ;
#37702 = EDGE_CURVE ( 'NONE', #11134, #39147, #52972, .T. ) ;
#37701 = LINE ( 'NONE', #59152, #65756 ) ;
#37703 = AXIS2_PLACEMENT_3D ( 'NONE', #19170, #56117, #17798 ) ;
#37704 = CARTESIAN_POINT ( 'NONE',  ( -168.1839487819771080, 83.25723186408069409, 70.81687309716325274 ) ) ;
#37705 = CARTESIAN_POINT ( 'NONE',  ( 0.000000000000000000, 0.000000000000000000, 41.38025477438755928 ) ) ;
#37706 = AXIS2_PLACEMENT_3D ( 'NONE', #37013, #42956, #25439 ) ;
#37707 = ADVANCED_FACE ( 'NONE', ( #50378 ), #7477, .F. ) ;
#37708 = DIRECTION ( 'NONE',  ( -0.9999168736529502333, 0.000000000000000000, 0.01289363347198229856 ) ) ;
#37709 = VERTEX_POINT ( 'NONE', #13772 ) ;
#37710 = CARTESIAN_POINT ( 'NONE',  ( 183.2136430849847955, 6.000000000000000000, -41.68900338898720292 ) ) ;
#37711 = CONICAL_SURFACE ( 'NONE', #55702, 4.171999999999999709, 0.7853981633974472798 ) ;
#37712 = VECTOR ( 'NONE', #24349, 1000.000000000000000 ) ;
#37713 = CARTESIAN_POINT ( 'NONE',  ( 188.4365915667138438, 87.87248959723055464, -15.37144753093564908 ) ) ;
#37714 = DIRECTION ( 'NONE',  ( 0.000000000000000000, -0.000000000000000000, -1.000000000000000000 ) ) ;
#37715 = CARTESIAN_POINT ( 'NONE',  ( -79.52000911032672548, 23.72680920995770038, -88.84120912474600118 ) ) ;
#37716 = DIRECTION ( 'NONE',  ( -0.000000000000000000, -0.000000000000000000, 1.000000000000000000 ) ) ;
#37717 = DIRECTION ( 'NONE',  ( -0.000000000000000000, -0.000000000000000000, -1.000000000000000000 ) ) ;
#37718 = LINE ( 'NONE', #47920, #23934 ) ;
#37719 = CARTESIAN_POINT ( 'NONE',  ( 164.0105905242218114, 64.23277447906892235, 60.07396046421560243 ) ) ;
#37720 = AXIS2_PLACEMENT_3D ( 'NONE', #46853, #69340, #21162 ) ;
#37721 = B_SPLINE_CURVE_WITH_KNOTS ( 'NONE', 3,
 ( #16477, #16165, #52428, #63678, #47828, #9871, #4251, #47476, #69288, #15143, #32359, #21116, #25711, #27061, #42218, #47140, #20408, #36944, #58721, #68934, #53095, #4923, #37620, #10888, #41876, #32013, #5271, #26731, #63333, #21441, #42887, #36602, #53783, #5605, #20077, #41531, #62982, #58050, #28467, #1384, #59757, #44648, #39372, #48495 ),
 .UNSPECIFIED., .F., .F.,
 ( 4, 2, 2, 2, 2, 2, 2, 2, 2, 2, 2, 2, 2, 2, 2, 2, 2, 2, 2, 2, 2, 4 ),
 ( 1.734723475976807094E-18, 0.001482469635030026541, 0.002223704452545041763, 0.002964939270060056552, 0.004447408905090094802, 0.005929878540120132185, 0.007412348175150170436, 0.008153582992665182189, 0.008894817810180194809, 0.01037728744521020791, 0.01185975708024022274, 0.01260099189775521974, 0.01334222671527021502, 0.01482469635030021077, 0.01556593116781520431, 0.01630716598533020478, 0.01778963562036018492, 0.01927210525539016506, 0.02001334007290515860, 0.02075457489042015213, 0.02223704452545011839, 0.02371951416048008465 ),
 .UNSPECIFIED. ) ;
#37722 = VECTOR ( 'NONE', #61828, 1000.000000000000114 ) ;
#37723 = APPLICATION_CONTEXT ( 'automotive_design' ) ;
#37724 = EDGE_CURVE ( 'NONE', #37473, #59570, #39136, .T. ) ;
#37725 = ORIENTED_EDGE ( 'NONE', *, *, #61365, .F. ) ;
#37726 = DIRECTION ( 'NONE',  ( -1.393823445737823288E-16, -0.7660444431189770143, 0.6427876096865403621 ) ) ;
#37727 = CARTESIAN_POINT ( 'NONE',  ( 151.1700480242206481, 54.15904440870136938, 67.83133139760614938 ) ) ;
#37728 = CARTESIAN_POINT ( 'NONE',  ( -25.57361536219950082, 28.55671314637929470, 13.32819397642333037 ) ) ;
#37729 = CARTESIAN_POINT ( 'NONE',  ( 442.3372781065086201, 0.000000000000000000, -116.4497041420118393 ) ) ;
#37730 = EDGE_CURVE ( 'NONE', #42114, #35721, #7112, .T. ) ;
#37731 = EDGE_CURVE ( 'NONE', #24493, #43605, #50017, .T. ) ;
#37732 = CARTESIAN_POINT ( 'NONE',  ( -11.27383957674984849, 8.149435916118470402, 84.63656658335857230 ) ) ;
#37733 = ORIENTED_EDGE ( 'NONE', *, *, #31784, .F. ) ;
#37734 = LINE ( 'NONE', #52859, #60612 ) ;
#37735 = CARTESIAN_POINT ( 'NONE',  ( 39.40195752203892710, -170.0000000000000000, -16.27526687496408542 ) ) ;
#37736 = ORIENTED_EDGE ( 'NONE', *, *, #64384, .F. ) ;
#37737 = ORIENTED_EDGE ( 'NONE', *, *, #66345, .F. ) ;
#37738 = FACE_OUTER_BOUND ( 'NONE', #30474, .T. ) ;
#37739 = DIRECTION ( 'NONE',  ( -0.7818314824680221431, -0.6234898018587431423, 0.000000000000000000 ) ) ;
#37740 = CARTESIAN_POINT ( 'NONE',  ( 92.20490818459941806, 22.47175429302963323, -65.12600615666283943 ) ) ;
#37741 = ORIENTED_EDGE ( 'NONE', *, *, #8021, .T. ) ;
#37742 = DIRECTION ( 'NONE',  ( 1.000000000000000000, -0.000000000000000000, -0.000000000000000000 ) ) ;
#37743 = CARTESIAN_POINT ( 'NONE',  ( -1.862553927312058821, 7.582910205528085257, 6.195710318879104506 ) ) ;
#37744 = CARTESIAN_POINT ( 'NONE',  ( 181.0840389613909451, 80.03940679743416808, -36.22505766587961062 ) ) ;
#37745 = CARTESIAN_POINT ( 'NONE',  ( -150.5993571094983281, 66.43939758484179947, -76.58067256224735786 ) ) ;
#37746 = CARTESIAN_POINT ( 'NONE',  ( 88.98408042523109884, 20.23787745328939280, 30.08728822265231884 ) ) ;
#37747 = PRODUCT ( 'top cover', 'top cover', '', ( #25890 ) ) ;
#37748 = ORIENTED_EDGE ( 'NONE', *, *, #21433, .T. ) ;
#37749 = CARTESIAN_POINT ( 'NONE',  ( -48.58011387679027848, 14.07568064779664141, -46.51327318317784432 ) ) ;
#37750 = AXIS2_PLACEMENT_3D ( 'NONE', #55685, #56038, #7854 ) ;
#37751 = FACE_OUTER_BOUND ( 'NONE', #1825, .T. ) ;
#37752 = CARTESIAN_POINT ( 'NONE',  ( 9.819093282782489496, 7.389085782749409859, 42.08183418655492147 ) ) ;
#37753 = CARTESIAN_POINT ( 'NONE',  ( 66.90836167404864909, 13.60846798854640127, -90.44605171876324334 ) ) ;
#37754 = CARTESIAN_POINT ( 'NONE',  ( -82.50457182857807936, 24.90487912293252037, 85.15644553449918419 ) ) ;
#37755 = VECTOR ( 'NONE', #11214, 1000.000000000000114 ) ;
#37757 = ORIENTED_EDGE ( 'NONE', *, *, #13292, .T. ) ;
#37756 = FACE_OUTER_BOUND ( 'NONE', #59068, .T. ) ;
#37758 = VERTEX_POINT ( 'NONE', #2532 ) ;
#37759 = CIRCLE ( 'NONE', #67076, 5.000000000000000888 ) ;
#37760 = VECTOR ( 'NONE', #68711, 1000.000000000000000 ) ;
#37761 = EDGE_LOOP ( 'NONE', ( #60794, #19595, #58363, #28672 ) ) ;
#37762 = CARTESIAN_POINT ( 'NONE',  ( -14.92903005859421306, 7.458185427130748835, -13.65509502686643195 ) ) ;
#37763 = CARTESIAN_POINT ( 'NONE',  ( -167.3263409977197398, 82.35496590386728144, 87.23955561701365014 ) ) ;
#37764 = CARTESIAN_POINT ( 'NONE',  ( 151.3976820382521851, 53.07948349322499837, 94.99999999999866418 ) ) ;
#37765 = EDGE_CURVE ( 'NONE', #13447, #31009, #28927, .T. ) ;
#37766 = FACE_OUTER_BOUND ( 'NONE', #51252, .T. ) ;
#37767 = PRODUCT_DEFINITION_FORMATION_WITH_SPECIFIED_SOURCE ( 'ANY', '', #36034, .NOT_KNOWN. ) ;
#37769 = CARTESIAN_POINT ( 'NONE',  ( -55.54036735998995766, 15.85474597822063636, -35.21632399845986328 ) ) ;
#37768 = AXIS2_PLACEMENT_3D ( 'NONE', #55418, #6884, #66357 ) ;
#37770 = CARTESIAN_POINT ( 'NONE',  ( -9.765753193741730342, 8.033970690975920093, -23.32232872259482548 ) ) ;
#37771 = CARTESIAN_POINT ( 'NONE',  ( 154.4429418375333114, 55.33424769452792447, -77.34545030156257894 ) ) ;
#37772 = CARTESIAN_POINT ( 'NONE',  ( 20.37135563017390183, 6.690359945346087578, -10.21723432638768614 ) ) ;
#37774 = ORIENTED_EDGE ( 'NONE', *, *, #4372, .T. ) ;
#37773 = ADVANCED_FACE ( 'NONE', ( #66568 ), #66916, .F. ) ;
#37775 = CIRCLE ( 'NONE', #46766, 19.99999999999999645 ) ;
#37776 = CARTESIAN_POINT ( 'NONE',  ( -8.000000000000000000, -4.618802153517024500, -8.785468820183664818 ) ) ;
#37777 = ORIENTED_EDGE ( 'NONE', *, *, #413, .F. ) ;
#37778 = ORIENTED_EDGE ( 'NONE', *, *, #5063, .T. ) ;
#37779 = CARTESIAN_POINT ( 'NONE',  ( -50.88541732109732862, -55.03078243218159571, 41.38025477438755928 ) ) ;
#37780 = DIRECTION ( 'NONE',  ( -0.000000000000000000, -0.000000000000000000, -1.000000000000000000 ) ) ;
#37781 = CARTESIAN_POINT ( 'NONE',  ( 117.5606268127798160, 32.41702750294250990, 92.48114496397971607 ) ) ;
#37782 = CARTESIAN_POINT ( 'NONE',  ( -155.1359377029285724, 70.46175948311801562, 16.35866617282277602 ) ) ;
#37783 = CARTESIAN_POINT ( 'NONE',  ( 188.2133404574782389, 86.12414067617876867, -41.37883977796289514 ) ) ;
#37784 = CARTESIAN_POINT ( 'NONE',  ( 20.74093720376649586, 6.709541214524347374, 31.86137974890134572 ) ) ;
#37785 = CARTESIAN_POINT ( 'NONE',  ( -156.8713506010090839, 72.05569703773764445, 93.37478388102675808 ) ) ;
#37786 = EDGE_LOOP ( 'NONE', ( #68093, #30165, #43689, #5755, #69161, #66499, #28331, #63358, #29886, #16583 ) ) ;
#37787 = ADVANCED_FACE ( 'NONE', ( #34896 ), #12392, .F. ) ;
#37788 = ORIENTED_EDGE ( 'NONE', *, *, #38557, .F. ) ;
#37789 = EDGE_LOOP ( 'NONE', ( #5095, #58886, #34250, #60792 ) ) ;
#37790 = EDGE_CURVE ( 'NONE', #65005, #43260, #13436, .T. ) ;
#37791 = CARTESIAN_POINT ( 'NONE',  ( -154.0833774771448645, 69.51012195447351871, -9.506901666534069761 ) ) ;
#37792 = CARTESIAN_POINT ( 'NONE',  ( 35.66087318222940894, 8.964867769223234362, -49.63888608646336564 ) ) ;
#37793 = EDGE_CURVE ( 'NONE', #45595, #57264, #38368, .T. ) ;
#37794 = CARTESIAN_POINT ( 'NONE',  ( -36.37663950036512261, 10.45389057208229033, 70.22755886848516127 ) ) ;
#37795 = CARTESIAN_POINT ( 'NONE',  ( 197.9868529032975459, 99.18611233336800126, 60.19158866520284334 ) ) ;
#37796 = ORIENTED_EDGE ( 'NONE', *, *, #61227, .T. ) ;
#37797 = B_SPLINE_CURVE_WITH_KNOTS ( 'NONE', 3,
 ( #11463, #7258, #66017, #12887, #49444, #60712, #28000, #23087, #6896, #33649, #54730, #22032, #38922, #55077, #60002, #38211, #12185, #17813, #28714, #18155, #17445, #28353, #6556, #43476, #49799, #1624, #11824, #59648, #33300, #43821, #44536, #50160, #1276, #22734, #65297, #66365, #44168, #65654, #39609, #32931, #39268, #12527, #54372, #33990 ),
 .UNSPECIFIED., .F., .F.,
 ( 4, 2, 2, 2, 2, 2, 2, 2, 2, 2, 2, 2, 2, 2, 2, 2, 2, 2, 2, 2, 2, 4 ),
 ( 0.000000000000000000, 0.004120577325733526357, 0.006180865988600314255, 0.008241154651467101286, 0.01030144331433388918, 0.01133158764576725278, 0.01236173197720061984, 0.01339187630863398343, 0.01442202064006734875, 0.01545216497150071581, 0.01648230930293407767, 0.01699738146865076294, 0.01751245363436744473, 0.01854259796580083608, 0.01957274229723423090, 0.02060288662866762224, 0.02266317529153437718, 0.02472346395440113212, 0.02678375261726789053, 0.02781389694870122983, 0.02884404128013456567, 0.03296461860586801657 ),
 .UNSPECIFIED. ) ;
#37798 = DIRECTION ( 'NONE',  ( 0.9839295885986321100, -0.1785568947986229116, 0.000000000000000000 ) ) ;
#37799 = CARTESIAN_POINT ( 'NONE',  ( -152.5046761101291963, 66.76407727525179325, 71.94415056971432421 ) ) ;
#37800 =( LENGTH_UNIT ( ) NAMED_UNIT ( * ) SI_UNIT ( .MILLI., .METRE. ) );
#37801 = CARTESIAN_POINT ( 'NONE',  ( -0.9897066053608898351, 7.549089325901767289, -46.01382324979444860 ) ) ;
#37802 = SURFACE_STYLE_USAGE ( .BOTH. , #55014 ) ;
#37803 = DIRECTION ( 'NONE',  ( -1.000000000000000000, 0.000000000000000000, 0.000000000000000000 ) ) ;
#37804 = DIRECTION ( 'NONE',  ( 1.000000000000000000, 1.850550996349095901E-16, 1.228197773518735191E-20 ) ) ;
#37805 = CARTESIAN_POINT ( 'NONE',  ( 437.3372781065086201, 0.000000000000000000, 108.5502958579881749 ) ) ;
#37806 = CARTESIAN_POINT ( 'NONE',  ( -51.82969867401435948, -54.20961478705483927, 43.58025477438756212 ) ) ;
#37807 = CARTESIAN_POINT ( 'NONE',  ( 15.29899606819415858, 6.485153354884283239, -77.36349468914947636 ) ) ;
#37808 = AXIS2_PLACEMENT_3D ( 'NONE', #63223, #10097, #5163 ) ;
#37809 = ORIENTED_EDGE ( 'NONE', *, *, #51571, .F. ) ;
#37810 = DIRECTION ( 'NONE',  ( 0.000000000000000000, 1.000000000000000000, 0.000000000000000000 ) ) ;
#37811 = APPLICATION_PROTOCOL_DEFINITION ( 'draft international standard', 'automotive_design', 1998, #35896 ) ;
#37812 = DIRECTION ( 'NONE',  ( 0.000000000000000000, 0.000000000000000000, 1.000000000000000000 ) ) ;
#37813 = CARTESIAN_POINT ( 'NONE',  ( -131.6508182719823026, 50.40277850441007246, -47.24685355452295710 ) ) ;
#37814 = EDGE_CURVE ( 'NONE', #58488, #56789, #46927, .T. ) ;
#37815 = LINE ( 'NONE', #60662, #27816 ) ;
#37816 = EDGE_CURVE ( 'NONE', #49197, #54158, #19393, .T. ) ;
#37817 = DIRECTION ( 'NONE',  ( 1.000000000000000000, 0.000000000000000000, -0.000000000000000000 ) ) ;
#37818 = ORIENTED_EDGE ( 'NONE', *, *, #33510, .T. ) ;
#37819 = CIRCLE ( 'NONE', #34484, 5.400000000000001243 ) ;
#37820 = DIRECTION ( 'NONE',  ( 0.000000000000000000, -1.000000000000000000, 0.000000000000000000 ) ) ;
#37821 = ORIENTED_EDGE ( 'NONE', *, *, #21999, .F. ) ;
#37822 = ADVANCED_FACE ( 'NONE', ( #52771 ), #1323, .T. ) ;
#37823 = CARTESIAN_POINT ( 'NONE',  ( -2.116120943111210906, -74.98056102853675497, 170.0000000000000000 ) ) ;
#37824 = CARTESIAN_POINT ( 'NONE',  ( 197.8588046850313447, 99.02485934465610740, 12.95651097256631878 ) ) ;
#37825 = ORIENTED_EDGE ( 'NONE', *, *, #18455, .F. ) ;
#37826 = CIRCLE ( 'NONE', #61441, 242.4895526022646379 ) ;
#37827 = ORIENTED_EDGE ( 'NONE', *, *, #32697, .T. ) ;
#37828 = DIRECTION ( 'NONE',  ( -1.000000000000000000, 0.000000000000000000, 0.000000000000000000 ) ) ;
#37829 = ORIENTED_EDGE ( 'NONE', *, *, #13353, .F. ) ;
#37830 = DIRECTION ( 'NONE',  ( -0.000000000000000000, -0.000000000000000000, -1.000000000000000000 ) ) ;
#37831 = DIRECTION ( 'NONE',  ( 1.000000000000000000, 0.000000000000000000, 0.000000000000000000 ) ) ;
#37832 = CARTESIAN_POINT ( 'NONE',  ( 140.8855094313932739, 47.03549517811092784, 66.48436074708210697 ) ) ;
#37833 = DIRECTION ( 'NONE',  ( -0.8160245890732938934, -0.5780171883497599028, 0.000000000000000000 ) ) ;
#37834 = CARTESIAN_POINT ( 'NONE',  ( 158.9231328297667289, 58.78767772853188944, -89.91818538214990042 ) ) ;
#37835 = CARTESIAN_POINT ( 'NONE',  ( 76.57571471437145760, 10.00000000000000000, -20.00000000000000000 ) ) ;
#37836 = CARTESIAN_POINT ( 'NONE',  ( 188.9999999999999432, 0.000000000000000000, 72.99999999999998579 ) ) ;
#37837 = ORIENTED_EDGE ( 'NONE', *, *, #33854, .T. ) ;
#37838 = VERTEX_POINT ( 'NONE', #51421 ) ;
#37839 = DIRECTION ( 'NONE',  ( 0.000000000000000000, 0.000000000000000000, -1.000000000000000000 ) ) ;
#37840 = CARTESIAN_POINT ( 'NONE',  ( 410.0000000000000000, 0.000000000000000000, 174.3129005282752928 ) ) ;
#37841 = B_SPLINE_CURVE_WITH_KNOTS ( 'NONE', 3,
 ( #18753, #38548, #61657, #59992, #17437, #45828, #22722, #34934, #56376, #24385, #19432, #33639, #33290, #55068, #8198, #8549, #67304, #30001, #3270, #46164 ),
 .UNSPECIFIED., .F., .F.,
 ( 4, 2, 2, 2, 2, 2, 2, 2, 2, 4 ),
 ( 0.000000000000000000, 0.001285001623041191797, 0.002570003246082383595, 0.003855004869123575175, 0.005140006492164767189, 0.006425008115205958770, 0.007710009738247150350, 0.008995011361288341931, 0.009637512172808941624, 0.01028001298432954305 ),
 .UNSPECIFIED. ) ;
#37842 = CARTESIAN_POINT ( 'NONE',  ( -144.3939084932120807, 61.25241660819418144, -36.82102133094029739 ) ) ;
#37843 = CARTESIAN_POINT ( 'NONE',  ( -166.2053056899075045, 81.18967388993337408, -71.97276839613554955 ) ) ;
#37845 = ORIENTED_EDGE ( 'NONE', *, *, #25598, .T. ) ;
#37844 = DIRECTION ( 'NONE',  ( -0.000000000000000000, -1.000000000000000000, -0.000000000000000000 ) ) ;
#37846 = DIRECTION ( 'NONE',  ( 0.000000000000000000, -0.000000000000000000, 1.000000000000000000 ) ) ;
#37847 = ORIENTED_EDGE ( 'NONE', *, *, #65020, .T. ) ;
#37848 = CARTESIAN_POINT ( 'NONE',  ( -143.7151964745329451, 59.41799441280381444, 60.29410247371058063 ) ) ;
#37849 = CYLINDRICAL_SURFACE ( 'NONE', #39046, 7.500000000000027534 ) ;
#37850 = DIRECTION ( 'NONE',  ( -1.850371928290090422E-16, 1.000000000000000000, 1.110223024625156171E-16 ) ) ;
#37851 = CARTESIAN_POINT ( 'NONE',  ( 81.57482918025357321, 17.75786713398421668, -10.93062121972884349 ) ) ;
#37852 = AXIS2_PLACEMENT_3D ( 'NONE', #11299, #54200, #6023 ) ;
#37853 = CARTESIAN_POINT ( 'NONE',  ( 88.53517449242357884, 20.08005703101045469, -62.90834010636418583 ) ) ;
#37854 = EDGE_CURVE ( 'NONE', #16854, #21376, #51756, .T. ) ;
#37855 = CARTESIAN_POINT ( 'NONE',  ( 57.27073671374542130, 11.41305252370465162, -92.07090031608234426 ) ) ;
#37856 = CARTESIAN_POINT ( 'NONE',  ( 447.3372781065084496, 390.0000000000043769, 108.5502958579838122 ) ) ;
#37857 = CARTESIAN_POINT ( 'NONE',  ( -151.5114545224535902, 65.89821478636478957, -88.77172430480310084 ) ) ;
#37858 = VERTEX_POINT ( 'NONE', #26410 ) ;
#37859 = ORIENTED_EDGE ( 'NONE', *, *, #2786, .F. ) ;
#37860 = CIRCLE ( 'NONE', #8662, 5.000000000000004441 ) ;
#37861 = CARTESIAN_POINT ( 'NONE',  ( 188.2076037774874919, 86.11782719225438143, -72.93302748442802397 ) ) ;
#37862 = CARTESIAN_POINT ( 'NONE',  ( 11.21387192505586761, 6.397095920409659797, 31.55118611238502524 ) ) ;
#37863 = CARTESIAN_POINT ( 'NONE',  ( 266.9165763529819628, 192.0000000000000000, 128.9999999999999716 ) ) ;
#37864 = CARTESIAN_POINT ( 'NONE',  ( -18.89790202299209199, 62.20684691518605547, 43.58025477438756923 ) ) ;
#37865 = CONICAL_SURFACE ( 'NONE', #9815, 8.000000000000001776, 1.047197551196595855 ) ;
#37866 = CARTESIAN_POINT ( 'NONE',  ( 108.3753929817421096, 29.13179266688724312, -62.98785435523912213 ) ) ;
#37867 = CARTESIAN_POINT ( 'NONE',  ( 81.76092782665034520, 17.81692437267513540, 42.92251290309585698 ) ) ;
#37868 = VECTOR ( 'NONE', #61920, 1000.000000000000227 ) ;
#37869 = CARTESIAN_POINT ( 'NONE',  ( 63.49941241090380117, 13.81848793187417712, -50.72069083216975116 ) ) ;
#37870 = CARTESIAN_POINT ( 'NONE',  ( -119.1605144823340083, 43.39823405392971267, 34.80618779126584883 ) ) ;
#37872 = CARTESIAN_POINT ( 'NONE',  ( 444.9999999999999432, -35.00000000000000000, -2.000000000000000000 ) ) ;
#37871 = B_SPLINE_CURVE_WITH_KNOTS ( 'NONE', 3,
 ( #4059, #5760, #64517, #42709, #43045, #58880, #48307, #37093, #16670, #47632, #26197, #16326, #47290, #5429, #26543, #42025, #68745, #58532, #20918, #10693, #15642, #58203, #10023, #26882, #32169, #141, #48656, #32507, #31475, #53938, #69442, #64866, #53249, #20563, #53598, #42369, #59226, #37782, #63830, #27219, #21598, #15979, #11043, #25863, #21945, #10351, #69085, #31144 ),
 .UNSPECIFIED., .F., .F.,
 ( 4, 2, 2, 2, 2, 2, 2, 2, 2, 2, 2, 2, 2, 2, 2, 2, 2, 2, 2, 2, 2, 2, 2, 4 ),
 ( 0.02698595842317762922, 0.02784423243973404780, 0.02870250645629046637, 0.03041905448940321333, 0.03127732850595960068, 0.03213560252251598803, 0.03385215055562876274, 0.03471042457218512234, 0.03556869858874148888, 0.03728524662185418725, 0.03814352063841052604, 0.03900179465496686482, 0.03986006867152319666, 0.04071834268807953544, 0.04157661670463586728, 0.04243489072119220606, 0.04415143875430486975, 0.04500971277086120159, 0.04586798678741754037, 0.04758453482053021794, 0.04930108285364289550, 0.05101763088675557306, 0.05273417891986825756, 0.05445072695298092819 ),
 .UNSPECIFIED. ) ;
#37873 = EDGE_CURVE ( 'NONE', #59178, #36560, #64371, .T. ) ;
#37874 = ORIENTED_EDGE ( 'NONE', *, *, #47787, .T. ) ;
#37875 = CARTESIAN_POINT ( 'NONE',  ( -23.93895920923072396, 9.495000752338446759, 10.62982118334621617 ) ) ;
#37876 = ORIENTED_EDGE ( 'NONE', *, *, #24586, .F. ) ;
#37878 = AXIS2_PLACEMENT_3D ( 'NONE', #55412, #45211, #44522 ) ;
#37877 = CARTESIAN_POINT ( 'NONE',  ( -15.31363169557738324, 7.494880774891998776, -43.40552099073981651 ) ) ;
#37879 = CARTESIAN_POINT ( 'NONE',  ( 20.00000000000000000, 0.000000000000000000, 5.000000000000000000 ) ) ;
#37880 = ADVANCED_FACE ( 'NONE', ( #712 ), #21138, .F. ) ;
#37881 = DIRECTION ( 'NONE',  ( -0.000000000000000000, -0.000000000000000000, -1.000000000000000000 ) ) ;
#37882 = CARTESIAN_POINT ( 'NONE',  ( 150.2794558856210756, 52.26944788078747450, -14.57987070555832432 ) ) ;
#37883 = CARTESIAN_POINT ( 'NONE',  ( 31.90247004928963648, 8.563336936370815167, 10.06589353110114970 ) ) ;
#37884 = ADVANCED_FACE ( 'NONE', ( #42580 ), #6330, .F. ) ;
#37885 = DIRECTION ( 'NONE',  ( -0.2225209339563042066, -0.9749279121818259508, 0.000000000000000000 ) ) ;
#37886 = CARTESIAN_POINT ( 'NONE',  ( 15.55634918610396511, -46.66904755831214402, 0.000000000000000000 ) ) ;
#37887 = ORIENTED_EDGE ( 'NONE', *, *, #52804, .T. ) ;
#37888 = CARTESIAN_POINT ( 'NONE',  ( 212.0383651583489097, 116.9865343143054730, 88.79641243644768167 ) ) ;
#37889 = CARTESIAN_POINT ( 'NONE',  ( 266.9165763529819628, -2.000000000000001776, 108.9999999999999858 ) ) ;
#37890 = ORIENTED_EDGE ( 'NONE', *, *, #58215, .F. ) ;
#37891 = DIRECTION ( 'NONE',  ( -1.000000000000000000, 0.000000000000000000, 0.000000000000000000 ) ) ;
#37892 = CARTESIAN_POINT ( 'NONE',  ( 31.11269837220812562, 36.11269837220800838, 2.000000000000001776 ) ) ;
#37893 = DIRECTION ( 'NONE',  ( -0.000000000000000000, 1.000000000000000000, -0.000000000000000000 ) ) ;
#37894 = CARTESIAN_POINT ( 'NONE',  ( 46.84154678921881043, 10.51341196666389521, -70.94621687880534466 ) ) ;
#37895 = CARTESIAN_POINT ( 'NONE',  ( -0.3747453031323927930, 6.520267647591905913, 36.62717459950940935 ) ) ;
#37896 = PLANE ( 'NONE',  #3038 ) ;
#37897 = CARTESIAN_POINT ( 'NONE',  ( 92.99472202396344755, 22.76601925259606318, 86.92061487625339566 ) ) ;
#37898 = ORIENTED_EDGE ( 'NONE', *, *, #27397, .T. ) ;
#37899 = DIRECTION ( 'NONE',  ( 0.9998063756620099163, 0.01967768242440574161, -9.407213639798576407E-15 ) ) ;
#37900 = CARTESIAN_POINT ( 'NONE',  ( 0.000000000000000000, -2.000000000000000000, 378.0000000000000000 ) ) ;
#37901 = CARTESIAN_POINT ( 'NONE',  ( -132.4951995226845156, 50.99687809989499243, 7.706407028771845802 ) ) ;
#37902 = CARTESIAN_POINT ( 'NONE',  ( -173.1211646369891355, 88.63826465341152527, -34.71195716474998960 ) ) ;
#37903 = CARTESIAN_POINT ( 'NONE',  ( -179.9963635872885561, 95.12185477187962590, 88.99551518947737350 ) ) ;
#37904 = VERTEX_POINT ( 'NONE', #53115 ) ;
#37905 = CARTESIAN_POINT ( 'NONE',  ( 41.49663191311417165, -50.03028622612021792, 170.0000000000000000 ) ) ;
#37906 = CARTESIAN_POINT ( 'NONE',  ( 412.0000000000000000, 192.0000000000000000, 0.000000000000000000 ) ) ;
#37907 = AXIS2_PLACEMENT_3D ( 'NONE', #33772, #45357, #23565 ) ;
#37908 = EDGE_CURVE ( 'NONE', #25095, #22557, #37994, .T. ) ;
#37909 = CARTESIAN_POINT ( 'NONE',  ( 197.8588046850312878, 99.02485934465607897, -13.88803961789735375 ) ) ;
#37910 = CARTESIAN_POINT ( 'NONE',  ( -156.9749551707454316, 70.78135822687410439, 92.69151126661552098 ) ) ;
#37911 = AXIS2_PLACEMENT_3D ( 'NONE', #26732, #53096, #58385 ) ;
#37912 = CARTESIAN_POINT ( 'NONE',  ( 138.2204650371259618, 44.12203217345472694, 43.12867697710134962 ) ) ;
#37913 = ORIENTED_EDGE ( 'NONE', *, *, #33180, .T. ) ;
#37914 = DIRECTION ( 'NONE',  ( 0.000000000000000000, -1.000000000000000000, 0.000000000000000000 ) ) ;
#37915 = CARTESIAN_POINT ( 'NONE',  ( 81.04027388895738682, 18.64386073872848826, 15.39279842491352390 ) ) ;
#37916 = VECTOR ( 'NONE', #55721, 1000.000000000000000 ) ;
#37917 = CARTESIAN_POINT ( 'NONE',  ( 164.9540180502650628, 65.02981548735053252, 10.63337814117685198 ) ) ;
#37918 = CARTESIAN_POINT ( 'NONE',  ( -149.5074843970971301, -170.0000000000000000, 91.90992242082643315 ) ) ;
#37919 = VECTOR ( 'NONE', #68058, 1000.000000000000000 ) ;
#37920 = ORIENTED_EDGE ( 'NONE', *, *, #16884, .F. ) ;
#37921 = DIRECTION ( 'NONE',  ( 0.000000000000000000, 1.000000000000000000, -0.000000000000000000 ) ) ;
#37922 = ORIENTED_EDGE ( 'NONE', *, *, #6501, .F. ) ;
#37923 = CARTESIAN_POINT ( 'NONE',  ( -75.00168449119586001, 20.95943092127970431, -9.222782878067645740 ) ) ;
#37924 = DIRECTION ( 'NONE',  ( -0.000000000000000000, -6.405132834375902056E-16, 1.000000000000000000 ) ) ;
#37926 = ORIENTED_EDGE ( 'NONE', *, *, #46146, .F. ) ;
#37925 = LINE ( 'NONE', #31965, #41003 ) ;
#37927 = CARTESIAN_POINT ( 'NONE',  ( 159.2389084450350367, 59.03884018680376755, 44.21161777826668526 ) ) ;
#37928 = LINE ( 'NONE', #43539, #10502 ) ;
#37929 = DIRECTION ( 'NONE',  ( 0.000000000000000000, 0.000000000000000000, -1.000000000000000000 ) ) ;
#37930 = ORIENTED_EDGE ( 'NONE', *, *, #27151, .T. ) ;
#37931 = CARTESIAN_POINT ( 'NONE',  ( -102.2801239173131194, -170.0000000000000000, 45.51907450641513009 ) ) ;
#37932 = ADVANCED_FACE ( 'NONE', ( #17222 ), #10907, .T. ) ;
#37933 = CARTESIAN_POINT ( 'NONE',  ( -38.69577193929646342, 10.89562623693159971, -17.93097055276763641 ) ) ;
#37934 = EDGE_CURVE ( 'NONE', #8973, #51862, #53461, .T. ) ;
#37935 = CARTESIAN_POINT ( 'NONE',  ( -180.5954680880247167, 97.44843622358465041, 37.68151972413897255 ) ) ;
#37936 = CARTESIAN_POINT ( 'NONE',  ( -38.89042640463648581, 10.93374343663409398, -68.67378654700414131 ) ) ;
#37937 = VERTEX_POINT ( 'NONE', #4947 ) ;
#37938 = ORIENTED_EDGE ( 'NONE', *, *, #65352, .T. ) ;
#37939 = VERTEX_POINT ( 'NONE', #58739 ) ;
#37940 = FILL_AREA_STYLE_COLOUR ( '', #55345 ) ;
#37941 = LINE ( 'NONE', #43900, #67962 ) ;
#37942 = DIRECTION ( 'NONE',  ( -1.000000000000000000, 0.000000000000000000, 0.000000000000000000 ) ) ;
#37943 = CARTESIAN_POINT ( 'NONE',  ( 417.3372781065085633, 395.0000000000000568, -116.4497041420117824 ) ) ;
#37944 = VECTOR ( 'NONE', #55388, 1000.000000000000000 ) ;
#37945 = CARTESIAN_POINT ( 'NONE',  ( 68.58269726742371120, 14.03310040064105912, 85.96549742863071231 ) ) ;
#37946 = CARTESIAN_POINT ( 'NONE',  ( 445.3372781065086201, 0.000000000000000000, -1.353084311261909534E-13 ) ) ;
#37947 = CARTESIAN_POINT ( 'NONE',  ( 447.3372781065089043, 400.0000000000059117, -146.4497041420121377 ) ) ;
#37948 = FACE_BOUND ( 'NONE', #61800, .T. ) ;
#37949 = ORIENTED_EDGE ( 'NONE', *, *, #34175, .F. ) ;
#37950 = VECTOR ( 'NONE', #59935, 1000.000000000000000 ) ;
#37951 = CARTESIAN_POINT ( 'NONE',  ( 18.62350602913453201, 70.00000000000000000, 23.51946052065798298 ) ) ;
#37952 = ORIENTED_EDGE ( 'NONE', *, *, #41161, .F. ) ;
#37953 = DIRECTION ( 'NONE',  ( 1.000000000000000000, 0.000000000000000000, -0.000000000000000000 ) ) ;
#37954 = EDGE_CURVE ( 'NONE', #49516, #11433, #64036, .T. ) ;
#37955 = CARTESIAN_POINT ( 'NONE',  ( 210.6475357757682048, 114.8748261044496104, -75.24406005627064076 ) ) ;
#37956 = DIRECTION ( 'NONE',  ( -1.000000000000000000, 0.000000000000000000, 0.000000000000000000 ) ) ;
#37957 = VECTOR ( 'NONE', #8686, 1000.000000000000000 ) ;
#37958 = ADVANCED_FACE ( 'NONE', ( #32722 ), #27084, .F. ) ;
#37959 = B_SPLINE_CURVE_WITH_KNOTS ( 'NONE', 3,
 ( #409, #43657, #27486, #1116, #65485, #6024, #60196, #48572, #37694, #44360, #32773, #6734, #17643, #49278, #22915, #21864, #64783, #33129, #48925, #64431, #1460, #44008, #27140, #54201, #59144, #59491, #65844, #43307, #54561, #16242, #65136, #38752, #53860, #22565, #33487, #17278, #16930, #16590, #38394, #32432, #11301, #38046, #59834, #6387 ),
 .UNSPECIFIED., .F., .F.,
 ( 4, 2, 2, 2, 2, 2, 2, 2, 2, 2, 2, 2, 2, 2, 2, 2, 2, 2, 2, 2, 2, 4 ),
 ( 6.938893903907228378E-18, 0.001473754749730493913, 0.002210632124595742713, 0.002947509499460991729, 0.004421264249191470680, 0.005895018998921949631, 0.007368773748652429449, 0.008105651123517656348, 0.008842528498382884114, 0.01031628324811332230, 0.01179003799784375875, 0.01252691537270898825, 0.01326379274757421428, 0.01473754749730467328, 0.01547442487216991146, 0.01621130224703514963, 0.01768505699676562598, 0.01915881174649610233, 0.01989568912136134224, 0.02063256649622657868, 0.02210632124595707237, 0.02358007599568756954 ),
 .UNSPECIFIED. ) ;
#37960 = CARTESIAN_POINT ( 'NONE',  ( -78.66644367742111399, 22.32174330031319798, 18.57365054920947500 ) ) ;
#37961 = DIRECTION ( 'NONE',  ( -0.000000000000000000, -0.000000000000000000, -1.000000000000000000 ) ) ;
#37962 = DIRECTION ( 'NONE',  ( -4.270088556250601699E-16, -0.000000000000000000, -1.000000000000000000 ) ) ;
#37963 = DIRECTION ( 'NONE',  ( 0.000000000000000000, 0.000000000000000000, 1.000000000000000000 ) ) ;
#37964 = CARTESIAN_POINT ( 'NONE',  ( 157.4703587214989113, 57.65129005721575339, -36.12418429913763163 ) ) ;
#37965 = VECTOR ( 'NONE', #33972, 1000.000000000000000 ) ;
#37966 = CARTESIAN_POINT ( 'NONE',  ( 162.0812592823604916, 62.62783216273700049, -64.53408560632756519 ) ) ;
#37967 = ORIENTED_EDGE ( 'NONE', *, *, #21372, .T. ) ;
#37968 = CARTESIAN_POINT ( 'NONE',  ( 32.02161712141799654, -16.09918303830818687, 30.00000000000000000 ) ) ;
#37969 = FACE_OUTER_BOUND ( 'NONE', #20954, .T. ) ;
#37970 = ORIENTED_EDGE ( 'NONE', *, *, #64818, .T. ) ;
#37971 = VERTEX_POINT ( 'NONE', #27787 ) ;
#37972 = DIRECTION ( 'NONE',  ( 0.000000000000000000, 1.000000000000000000, 0.000000000000000000 ) ) ;
#37973 = CARTESIAN_POINT ( 'NONE',  ( -25.49247221749737236, 9.706368398275719400, -65.06484043158185671 ) ) ;
#37974 = CARTESIAN_POINT ( 'NONE',  ( 41.34269507549201705, 9.685203600174697058, 30.15284864378948981 ) ) ;
#37975 = CARTESIAN_POINT ( 'NONE',  ( -25.81763596640060499, 8.735969132042857410, 59.59007064553521360 ) ) ;
#37976 = VECTOR ( 'NONE', #7609, 1000.000000000000000 ) ;
#37977 = CARTESIAN_POINT ( 'NONE',  ( 132.9485794245231602, 40.87843215479635717, -9.220194473094281307 ) ) ;
#37978 = B_SPLINE_CURVE_WITH_KNOTS ( 'NONE', 3,
 ( #14341, #35795, #4469, #4804, #6188, #64593, #212, #48051, #22024, #5834, #21671, #27643, #47706, #53324, #49083, #59639, #69166, #42774, #10086, #36830, #63558, #26270, #26950, #64946, #64240, #58268, #10771, #21326, #32923, #15367, #59304, #37159, #54362, #5154, #922, #16400, #11453, #48729, #48377, #573, #20992, #16739, #42441, #22371 ),
 .UNSPECIFIED., .F., .F.,
 ( 4, 2, 2, 2, 2, 2, 2, 2, 2, 2, 2, 2, 2, 2, 2, 2, 2, 2, 2, 2, 2, 4 ),
 ( 0.02495775893651561855, 0.02650251144344301785, 0.02804726395037042061, 0.02959201645729781990, 0.03113676896422521920, 0.03268152147115262196, 0.03345389772461633549, 0.03422627397808004207, 0.03577102648500748300, 0.03654340273847120346, 0.03731577899193493086, 0.03808815524539864439, 0.03886053149886237179, 0.04040528400578980578, 0.04117766025925351236, 0.04195003651271722589, 0.04349478901964463212, 0.04503954152657204529, 0.04581191778003575188, 0.04658429403349946540, 0.04812904654042689245, 0.04967379904735433338 ),
 .UNSPECIFIED. ) ;
#37979 = ORIENTED_EDGE ( 'NONE', *, *, #28759, .T. ) ;
#37980 = ORIENTED_EDGE ( 'NONE', *, *, #48793, .F. ) ;
#37981 = CARTESIAN_POINT ( 'NONE',  ( -128.7724923851857284, 49.63576597317771899, 45.04931761937589840 ) ) ;
#37982 = ORIENTED_EDGE ( 'NONE', *, *, #33358, .T. ) ;
#37983 = PLANE ( 'NONE',  #24528 ) ;
#37984 = CARTESIAN_POINT ( 'NONE',  ( 185.7556003757505323, 84.93464887485406223, -91.53351864259758486 ) ) ;
#37985 = CARTESIAN_POINT ( 'NONE',  ( 62.53328835682432896, 12.56090025569836754, 56.65751152968496029 ) ) ;
#37986 = LINE ( 'NONE', #5285, #55402 ) ;
#37987 = CARTESIAN_POINT ( 'NONE',  ( -29.75554431712551917, 10.33961951730130124, -89.19458633079901233 ) ) ;
#37988 = DIRECTION ( 'NONE',  ( -0.000000000000000000, 1.000000000000000000, -0.000000000000000000 ) ) ;
#37989 = B_SPLINE_CURVE_WITH_KNOTS ( 'NONE', 3,
 ( #38437, #64474, #48612, #59526 ),
 .UNSPECIFIED., .F., .F.,
 ( 4, 4 ),
 ( 0.1259919275528358362, 0.1829744153748746327 ),
 .UNSPECIFIED. ) ;
#37990 = DIRECTION ( 'NONE',  ( 0.000000000000000000, 0.000000000000000000, 1.000000000000000000 ) ) ;
#37991 = ORIENTED_EDGE ( 'NONE', *, *, #28172, .T. ) ;
#37992 = ORIENTED_EDGE ( 'NONE', *, *, #34796, .F. ) ;
#37993 = FACE_OUTER_BOUND ( 'NONE', #11346, .T. ) ;
#37994 = LINE ( 'NONE', #53804, #66520 ) ;
#37995 = CARTESIAN_POINT ( 'NONE',  ( 432.4999999999999432, -18.06806526123148160, 378.0000000000000000 ) ) ;
#37996 = CARTESIAN_POINT ( 'NONE',  ( 138.1919700334460401, 44.10401742531043823, -76.50577590848440934 ) ) ;
#37997 = CARTESIAN_POINT ( 'NONE',  ( -5.000000000000000000, 0.000000000000000000, 2.000000000000000000 ) ) ;
#37998 = VERTEX_POINT ( 'NONE', #5 ) ;
#37999 = CARTESIAN_POINT ( 'NONE',  ( 83.38067517854669575, 18.33799117207142260, 3.603261572607144636 ) ) ;
#38000 = DIRECTION ( 'NONE',  ( 0.000000000000000000, 0.000000000000000000, 1.000000000000000000 ) ) ;
#38001 = CARTESIAN_POINT ( 'NONE',  ( 32.64241757152704793, 7.194141534430333884, 6.893342931793793760 ) ) ;
#38002 = ORIENTED_EDGE ( 'NONE', *, *, #23457, .T. ) ;
#38003 = AXIS2_PLACEMENT_3D ( 'NONE', #41294, #51839, #9277 ) ;
#38004 = ORIENTED_EDGE ( 'NONE', *, *, #67198, .T. ) ;
#38005 = CARTESIAN_POINT ( 'NONE',  ( -25.00000000000000000, 0.000000000000000000, 30.00000000000000000 ) ) ;
#38006 = CARTESIAN_POINT ( 'NONE',  ( 93.61951000632933528, 21.92572933971851512, 7.638221738897885693 ) ) ;
#38007 = EDGE_CURVE ( 'NONE', #27768, #19247, #21463, .T. ) ;
#38008 = VECTOR ( 'NONE', #12609, 1000.000000000000000 ) ;
#38009 = DIRECTION ( 'NONE',  ( 1.000000000000000000, -0.000000000000000000, -0.000000000000000000 ) ) ;
#38010 = ORIENTED_EDGE ( 'NONE', *, *, #2975, .F. ) ;
#38011 = CARTESIAN_POINT ( 'NONE',  ( -1.121471622164693649E-15, -6.534749472788167424, -4.681481898396976149 ) ) ;
#38012 = EDGE_CURVE ( 'NONE', #2785, #49177, #54146, .T. ) ;
#38013 = FACE_OUTER_BOUND ( 'NONE', #4497, .T. ) ;
#38014 = CARTESIAN_POINT ( 'NONE',  ( 152.6560521232696317, 54.00248515670892857, 31.15348575667133701 ) ) ;
#38015 = CARTESIAN_POINT ( 'NONE',  ( 65.39792658623289867, 14.27332852928128126, 44.42870172783316463 ) ) ;
#38016 = ADVANCED_FACE ( 'NONE', ( #49226 ), #59091, .T. ) ;
#38017 = CARTESIAN_POINT ( 'NONE',  ( -51.84164840787185113, 39.21024726209461875, 170.0000000000000000 ) ) ;
#38018 = DIRECTION ( 'NONE',  ( 0.000000000000000000, 1.000000000000000000, 0.000000000000000000 ) ) ;
#38019 = CARTESIAN_POINT ( 'NONE',  ( 63.00000000000000000, 7.715274834628325378E-15, 40.82842712474622004 ) ) ;
#38020 = EDGE_LOOP ( 'NONE', ( #38459, #42285, #57750, #43237 ) ) ;
#38021 = CARTESIAN_POINT ( 'NONE',  ( 136.7507824285648326, 44.38599729999913279, -63.44489443287879027 ) ) ;
#38022 = CARTESIAN_POINT ( 'NONE',  ( -22.50000000000003197, 207.5000000000000284, 0.000000000000000000 ) ) ;
#38023 = VERTEX_POINT ( 'NONE', #43251 ) ;
#38024 = EDGE_CURVE ( 'NONE', #28877, #19323, #64730, .T. ) ;
#38025 = FACE_BOUND ( 'NONE', #47245, .T. ) ;
#38026 = CARTESIAN_POINT ( 'NONE',  ( -61.29635759142615115, 21.66977272663494958, 41.38025477438755928 ) ) ;
#38027 =( LENGTH_UNIT ( ) NAMED_UNIT ( * ) SI_UNIT ( .MILLI., .METRE. ) );
#38028 = CARTESIAN_POINT ( 'NONE',  ( 10.55634918610400419, -15.55634918610406103, 2.000000000000000000 ) ) ;
#38029 = CARTESIAN_POINT ( 'NONE',  ( 35.54014968547473785, 66.04466488925542933, 0.000000000000000000 ) ) ;
#38030 = CARTESIAN_POINT ( 'NONE',  ( -85.35172689181705152, 26.07142112926218758, 7.637577235932388575 ) ) ;
#38031 = CARTESIAN_POINT ( 'NONE',  ( -20.00000000000002842, -6.319444444444441089, 4.000000000000000000 ) ) ;
#38032 = DIRECTION ( 'NONE',  ( -1.000000000000000000, 0.000000000000000000, 0.000000000000000000 ) ) ;
#38033 = CARTESIAN_POINT ( 'NONE',  ( -120.4666325602655945, 44.20829586446608062, -74.44071530592697172 ) ) ;
#38034 = FACE_OUTER_BOUND ( 'NONE', #68349, .T. ) ;
#38035 = CARTESIAN_POINT ( 'NONE',  ( 116.6734749296699505, 31.97209464358270026, 14.15860144538439336 ) ) ;
#38036 = CARTESIAN_POINT ( 'NONE',  ( 94.06699947028482711, 23.17027898120149487, -17.47450249519500787 ) ) ;
#38037 = ORIENTED_EDGE ( 'NONE', *, *, #33051, .T. ) ;
#38038 = CYLINDRICAL_SURFACE ( 'NONE', #22865, 5.000000000000000000 ) ;
#38039 = ORIENTED_EDGE ( 'NONE', *, *, #3663, .T. ) ;
#38040 = CARTESIAN_POINT ( 'NONE',  ( -737.6000277536880958, -694.2189502691660437, 10.00000000000000000 ) ) ;
#38041 = EDGE_CURVE ( 'NONE', #36640, #30444, #59437, .T. ) ;
#38042 = CARTESIAN_POINT ( 'NONE',  ( 80.73462811483980772, 18.54763808182592300, -74.83009348606147171 ) ) ;
#38043 = CARTESIAN_POINT ( 'NONE',  ( 103.2255776213605714, 26.86235640255825174, 93.47014144773791600 ) ) ;
#38044 = DIRECTION ( 'NONE',  ( -0.000000000000000000, 1.000000000000000000, -0.000000000000000000 ) ) ;
#38045 = PLANE ( 'NONE',  #37852 ) ;
#38046 = CARTESIAN_POINT ( 'NONE',  ( -30.46002654261637943, 10.45132580906818021, -50.26895622567106869 ) ) ;
#38047 = CARTESIAN_POINT ( 'NONE',  ( -48.58279704072702287, 14.07632445131079635, -65.75936485380451302 ) ) ;
#38048 = CARTESIAN_POINT ( 'NONE',  ( -74.63254191291112249, 21.89590985985097760, -89.97802660070999536 ) ) ;
#38049 = CARTESIAN_POINT ( 'NONE',  ( -120.4666325602655945, 44.20829586446606640, -20.75161412499960178 ) ) ;
#38050 = VERTEX_POINT ( 'NONE', #22167 ) ;
#38051 = EDGE_LOOP ( 'NONE', ( #11014, #55234, #62885, #3760 ) ) ;
#38052 = CARTESIAN_POINT ( 'NONE',  ( 37.46876540261052924, 9.179568636624027889, 57.00768069096702817 ) ) ;
#38053 = CARTESIAN_POINT ( 'NONE',  ( 133.8566784816069060, 42.60093787723656789, -89.71241211332301191 ) ) ;
#38054 = VECTOR ( 'NONE', #12147, 1000.000000000000000 ) ;
#38055 = PRODUCT_DEFINITION_CONTEXT ( 'detailed design', #64648, 'design' ) ;
#38056 = LINE ( 'NONE', #4663, #16034 ) ;
#38057 = ORIENTED_EDGE ( 'NONE', *, *, #42870, .F. ) ;
#38058 =( GEOMETRIC_REPRESENTATION_CONTEXT ( 3 ) GLOBAL_UNCERTAINTY_ASSIGNED_CONTEXT ( ( #29675 ) ) GLOBAL_UNIT_ASSIGNED_CONTEXT ( ( #49218, #31674, #6322 ) ) REPRESENTATION_CONTEXT ( 'NONE', 'WORKASPACE' ) );
#38059 = PLANE ( 'NONE',  #61474 ) ;
#38060 = CARTESIAN_POINT ( 'NONE',  ( 186.7642514597452532, 86.02880938169742819, -11.97657000041078490 ) ) ;
#38061 = CARTESIAN_POINT ( 'NONE',  ( 212.0803491126036704, 118.9047894217573003, 11.22770652852349293 ) ) ;
#38062 =( NAMED_UNIT ( * ) PLANE_ANGLE_UNIT ( ) SI_UNIT ( $, .RADIAN. ) );
#38063 = B_SPLINE_CURVE_WITH_KNOTS ( 'NONE', 3,
 ( #66697, #51548, #2321, #19526, #12518, #55782, #7603, #2663, #33979, #29389, #50845, #20552, #25167, #42017, #63476, #58193, #36748, #46596 ),
 .UNSPECIFIED., .F., .F.,
 ( 4, 2, 2, 2, 2, 2, 2, 2, 4 ),
 ( 0.01001195649024165871, 0.01126366347862624989, 0.01251537046701084281, 0.01376707745539543573, 0.01501878444378002692, 0.01627049143216461810, 0.01752219842054920929, 0.01877390540893380394, 0.02002561239731839512 ),
 .UNSPECIFIED. ) ;
#38064 = DIRECTION ( 'NONE',  ( 0.000000000000000000, 1.000000000000000000, -0.000000000000000000 ) ) ;
#38065 = LINE ( 'NONE', #48943, #32941 ) ;
#38066 = FACE_OUTER_BOUND ( 'NONE', #49050, .T. ) ;
#38067 = DIRECTION ( 'NONE',  ( 0.000000000000000000, 0.000000000000000000, -1.000000000000000000 ) ) ;
#38068 = DIRECTION ( 'NONE',  ( -0.000000000000000000, 1.000000000000000000, -0.000000000000000000 ) ) ;
#38069 = VERTEX_POINT ( 'NONE', #43608 ) ;
#38070 = PLANE ( 'NONE',  #54865 ) ;
#38071 = CARTESIAN_POINT ( 'NONE',  ( 86.62931800182293784, 20.48449268398423584, -35.82156419891171595 ) ) ;
#38072 = CARTESIAN_POINT ( 'NONE',  ( -50.14523569787233725, 14.45648954445650780, 58.96871617340304539 ) ) ;
#38073 = CARTESIAN_POINT ( 'NONE',  ( 290.0000000000000568, 0.000000000000000000, 0.000000000000000000 ) ) ;
#38074 = DIRECTION ( 'NONE',  ( 0.000000000000000000, -1.000000000000000000, 0.000000000000000000 ) ) ;
#38075 = CARTESIAN_POINT ( 'NONE',  ( -14.61007982266178651, 8.438780854740821624, 88.09163706110108194 ) ) ;
#38076 = ADVANCED_FACE ( 'NONE', ( #65078 ), #62025, .T. ) ;
#38077 = ORIENTED_EDGE ( 'NONE', *, *, #66408, .T. ) ;
#38078 = LINE ( 'NONE', #12400, #31443 ) ;
#38079 = CARTESIAN_POINT ( 'NONE',  ( -57.43251939610648549, 15.33203492375495003, 57.53293398456845864 ) ) ;
#38080 = ORIENTED_EDGE ( 'NONE', *, *, #54919, .T. ) ;
#38081 = EDGE_LOOP ( 'NONE', ( #54629, #58652, #68148, #11681 ) ) ;
#38082 = DIRECTION ( 'NONE',  ( -0.000000000000000000, 1.000000000000000000, -0.000000000000000000 ) ) ;
#38083 = DIRECTION ( 'NONE',  ( 0.7818314824680311359, -0.6234898018587319291, 0.000000000000000000 ) ) ;
#38084 = CARTESIAN_POINT ( 'NONE',  ( 107.0477776024378755, 27.43148174916615645, 30.32163195193443883 ) ) ;
#38085 = VERTEX_POINT ( 'NONE', #59781 ) ;
#38086 = CARTESIAN_POINT ( 'NONE',  ( -61.75629144857964548, 16.58190704077737720, -66.18821733435061105 ) ) ;
#38087 = CYLINDRICAL_SURFACE ( 'NONE', #39780, 7.500000000000013323 ) ;
#38088 = CARTESIAN_POINT ( 'NONE',  ( 179.0091171455097481, 77.94933395983140656, -50.94517210893256731 ) ) ;
#38089 = CARTESIAN_POINT ( 'NONE',  ( 63.72039997003709999, 12.83396383267841401, 170.0000000000000000 ) ) ;
#38090 = DIRECTION ( 'NONE',  ( 0.000000000000000000, 0.000000000000000000, -1.000000000000000000 ) ) ;
#38091 = CARTESIAN_POINT ( 'NONE',  ( 91.13361825170458985, 21.00701373666981198, 43.22864410637488675 ) ) ;
#38092 = VERTEX_POINT ( 'NONE', #29521 ) ;
#38093 = EDGE_CURVE ( 'NONE', #57773, #42528, #46305, .T. ) ;
#38094 = CARTESIAN_POINT ( 'NONE',  ( 104.7042813665017178, 27.49927371769996753, -11.49719868635148146 ) ) ;
#38095 = DIRECTION ( 'NONE',  ( 0.000000000000000000, -0.000000000000000000, -1.000000000000000000 ) ) ;
#38096 = LINE ( 'NONE', #10327, #23982 ) ;
#38097 = CARTESIAN_POINT ( 'NONE',  ( 66.18991464235057265, 13.43011255454270980, -90.06529977466986736 ) ) ;
#38098 = B_SPLINE_CURVE_WITH_KNOTS ( 'NONE', 3,
 ( #45499, #60988, #66630, #50439 ),
 .UNSPECIFIED., .F., .F.,
 ( 4, 4 ),
 ( 9.900409499167601085E-07, 0.05658314289920116785 ),
 .UNSPECIFIED. ) ;
#38099 = CIRCLE ( 'NONE', #66216, 2.999999999999999112 ) ;
#38100 = CARTESIAN_POINT ( 'NONE',  ( 0.000000000000000000, 0.000000000000000000, 40.00000000000003553 ) ) ;
#38102 = EDGE_LOOP ( 'NONE', ( #67279, #19344, #35939, #8203, #1696, #30074, #12632, #38928, #34964, #35501 ) ) ;
#38101 = DIRECTION ( 'NONE',  ( -0.000000000000000000, -0.000000000000000000, -1.000000000000000000 ) ) ;
#38103 = ORIENTED_EDGE ( 'NONE', *, *, #48319, .T. ) ;
#38104 = ADVANCED_FACE ( 'NONE', ( #54857 ), #23908, .T. ) ;
#38105 = ORIENTED_EDGE ( 'NONE', *, *, #6886, .T. ) ;
#38106 = CARTESIAN_POINT ( 'NONE',  ( -8.807541152391509698, 6.956521193351524524, -8.622092021015157925 ) ) ;
#38107 = CARTESIAN_POINT ( 'NONE',  ( -173.7786140196550662, 89.37941604754422542, 84.53550708663692603 ) ) ;
#38108 = DIRECTION ( 'NONE',  ( 0.04486483035051862939, -0.9989930665413143673, -1.037707659396819425E-17 ) ) ;
#38109 = CARTESIAN_POINT ( 'NONE',  ( 290.0000000000000568, 0.000000000000000000, 19.99999999999998934 ) ) ;
#38110 = CARTESIAN_POINT ( 'NONE',  ( -60.98168946575806615, 17.40090852531919907, -38.09669203216598987 ) ) ;
#38111 = CARTESIAN_POINT ( 'NONE',  ( -7.825402957745083654, 7.899365992529244984, -8.573520141480125645 ) ) ;
#38112 = CARTESIAN_POINT ( 'NONE',  ( 0.000000000000000000, 0.000000000000000000, 133.5802547743875550 ) ) ;
#38113 = CARTESIAN_POINT ( 'NONE',  ( 20.74852474914888489, 6.709938988646748648, -10.52766966389744496 ) ) ;
#38114 = ORIENTED_EDGE ( 'NONE', *, *, #64306, .F. ) ;
#38115 = DIRECTION ( 'NONE',  ( 1.000000000000000000, 0.000000000000000000, 0.000000000000000000 ) ) ;
#38116 = ORIENTED_EDGE ( 'NONE', *, *, #48990, .F. ) ;
#38117 = VERTEX_POINT ( 'NONE', #29188 ) ;
#38118 = EDGE_CURVE ( 'NONE', #53998, #61117, #1372, .T. ) ;
#38119 = CARTESIAN_POINT ( 'NONE',  ( -142.3260422482980800, 59.60034523324938505, 13.61095042684088341 ) ) ;
#38120 = LINE ( 'NONE', #54645, #40557 ) ;
#38121 = CARTESIAN_POINT ( 'NONE',  ( -24.32220005085346770, 9.546215986458923553, 89.01704716004896056 ) ) ;
#38122 = AXIS2_PLACEMENT_3D ( 'NONE', #43890, #17516, #55146 ) ;
#38124 = EDGE_CURVE ( 'NONE', #8304, #3538, #14873, .T. ) ;
#38123 = CARTESIAN_POINT ( 'NONE',  ( 112.1009898303695707, 30.86414810229296535, -9.296667012977504641 ) ) ;
#38125 = FACE_OUTER_BOUND ( 'NONE', #53777, .T. ) ;
#38126 = LINE ( 'NONE', #59568, #59517 ) ;
#38127 = CARTESIAN_POINT ( 'NONE',  ( -155.0388735873032147, 70.37329702672087706, 86.80759492728509485 ) ) ;
#38128 = ORIENTED_EDGE ( 'NONE', *, *, #17361, .T. ) ;
#38129 = ORIENTED_EDGE ( 'NONE', *, *, #52416, .T. ) ;
#38130 = EDGE_LOOP ( 'NONE', ( #8143, #18506, #7685, #53121 ) ) ;
#38131 = DIRECTION ( 'NONE',  ( 0.000000000000000000, -1.000000000000000000, 0.000000000000000000 ) ) ;
#38132 = CARTESIAN_POINT ( 'NONE',  ( -154.6085044440278580, 69.98390342970670019, -20.97153785029703599 ) ) ;
#38133 = CARTESIAN_POINT ( 'NONE',  ( 32.89501968360929851, 8.663558833820816929, -39.35812473969490810 ) ) ;
#38134 = APPLICATION_CONTEXT ( 'automotive_design' ) ;
#38135 = CARTESIAN_POINT ( 'NONE',  ( -32.41627406084104734, 9.753381371531505195, 72.01291641558607637 ) ) ;
#38136 = AXIS2_PLACEMENT_3D ( 'NONE', #28528, #50336, #66188 ) ;
#38137 = CARTESIAN_POINT ( 'NONE',  ( 26.11269837220803325, -15.55634918610409656, 0.000000000000000000 ) ) ;
#38138 = ORIENTED_EDGE ( 'NONE', *, *, #17953, .T. ) ;
#38139 = LINE ( 'NONE', #1211, #64926 ) ;
#38140 = DIRECTION ( 'NONE',  ( 0.000000000000000000, 0.000000000000000000, 1.000000000000000000 ) ) ;
#38141 =( NAMED_UNIT ( * ) SI_UNIT ( $, .STERADIAN. ) SOLID_ANGLE_UNIT ( ) );
#38142 = CARTESIAN_POINT ( 'NONE',  ( -5.412684891282530941, 7.753215344827982136, -50.03639412057999181 ) ) ;
#38143 = CARTESIAN_POINT ( 'NONE',  ( 107.9362503323352769, 27.82881837607801856, 17.41909339002288348 ) ) ;
#38144 = FACE_OUTER_BOUND ( 'NONE', #34301, .T. ) ;
#38145 = CARTESIAN_POINT ( 'NONE',  ( -443.1918329948323390, 394.9767458440207974, -132.2549152767664964 ) ) ;
#38146 = CARTESIAN_POINT ( 'NONE',  ( 0.000000000000000000, 0.000000000000000000, 170.0000000000000000 ) ) ;
#38147 = PLANE ( 'NONE',  #31007 ) ;
#38148 = CARTESIAN_POINT ( 'NONE',  ( 13.83281508467570831, 7.452090093180181896, 17.92762544713185946 ) ) ;
#38149 = AXIS2_PLACEMENT_3D ( 'NONE', #11017, #69059, #53225 ) ;
#38150 = ORIENTED_EDGE ( 'NONE', *, *, #50125, .F. ) ;
#38151 = DIRECTION ( 'NONE',  ( 0.7530714660036196273, -0.6579387259397027066, 0.000000000000000000 ) ) ;
#38152 = CARTESIAN_POINT ( 'NONE',  ( -132.4951995226845156, 50.99687809989497822, -72.82724474261920022 ) ) ;
#38153 = DIRECTION ( 'NONE',  ( -1.000000000000000000, 0.000000000000000000, 0.000000000000000000 ) ) ;
#38154 = CARTESIAN_POINT ( 'NONE',  ( 45.34143264614440483, 9.256465810451187437, -74.55058974195040378 ) ) ;
#38155 = AXIS2_PLACEMENT_3D ( 'NONE', #68135, #29797, #8351 ) ;
#38156 = CARTESIAN_POINT ( 'NONE',  ( 58.08938767906772682, 12.61185010801509954, -64.38876158233470903 ) ) ;
#38157 = ORIENTED_EDGE ( 'NONE', *, *, #6269, .F. ) ;
#38158 = ADVANCED_FACE ( 'NONE', ( #34479, #23566 ), #49933, .T. ) ;
#38159 = ORIENTED_EDGE ( 'NONE', *, *, #38284, .F. ) ;
#38160 = CARTESIAN_POINT ( 'NONE',  ( 0.000000000000000000, 0.000000000000000000, 15.70156211871650775 ) ) ;
#38161 = CARTESIAN_POINT ( 'NONE',  ( 188.4992282969374742, 86.43939134553235704, 89.35533139977708572 ) ) ;
#38162 = ORIENTED_EDGE ( 'NONE', *, *, #41374, .F. ) ;
#38163 = ADVANCED_FACE ( 'NONE', ( #2454 ), #45003, .F. ) ;
#38164 = EDGE_LOOP ( 'NONE', ( #4441, #20405 ) ) ;
#38165 = CARTESIAN_POINT ( 'NONE',  ( 188.0094179620990928, 87.39792407168454247, 33.91549744460515825 ) ) ;
#38166 = DIRECTION ( 'NONE',  ( 1.000000000000000000, 0.000000000000000000, 0.000000000000000000 ) ) ;
#38167 = VERTEX_POINT ( 'NONE', #23223 ) ;
#38168 = CARTESIAN_POINT ( 'NONE',  ( 117.6853163455684808, 33.60747889659833731, 65.01678748886072867 ) ) ;
#38169 = B_SPLINE_CURVE_WITH_KNOTS ( 'NONE', 3,
 ( #21230, #48276, #59187, #48616, #69414, #25830, #21911, #58847, #20525, #20882, #15948, #9988, #47257, #64832, #63801, #53905, #37058, #105, #5726, #15264, #68716, #10660, #16294, #11009, #27185, #9646, #58172, #32128, #32473, #5397, #16631, #5044, #31107, #36726, #31441, #53215, #457, #26506, #28225, #65177, #17692, #6070, #49326, #34220, #11350 ),
 .UNSPECIFIED., .F., .F.,
 ( 4, 2, 2, 2, 2, 2, 2, 2, 1, 2, 2, 2, 2, 2, 2, 2, 2, 2, 2, 2, 2, 2, 4 ),
 ( 0.000000000000000000, 0.001470449819620649103, 0.002205674729430984280, 0.002940899639241319891, 0.004411349458861969428, 0.005881799278482619832, 0.007352249098103270236, 0.008087474007913597607, 0.008822698917723924977, 0.009557923827534252348, 0.01029314873734457798, 0.01176359855696523446, 0.01249882346677556183, 0.01323404837658588920, 0.01470449819620655608, 0.01543972310601688866, 0.01617494801582721950, 0.01764539783544789506, 0.01911584765506857062, 0.01985107256487890146, 0.02058629747468922883, 0.02205674729430989398, 0.02352719711393055219 ),
 .UNSPECIFIED. ) ;
#38170 = CARTESIAN_POINT ( 'NONE',  ( 139.6150621148398443, 46.20856238844173447, 68.68618430425954102 ) ) ;
#38171 = CARTESIAN_POINT ( 'NONE',  ( 32.02161712141799654, -16.09918303830818687, 30.00000000000000000 ) ) ;
#38172 = AXIS2_PLACEMENT_3D ( 'NONE', #50671, #61234, #43991 ) ;
#38173 = CARTESIAN_POINT ( 'NONE',  ( -74.58602291351368763, 7.967916035251061402, 170.0000000000000000 ) ) ;
#38174 = CARTESIAN_POINT ( 'NONE',  ( 88.28780346671264567, 19.99350429399659390, -50.63982961935722926 ) ) ;
#38175 = CARTESIAN_POINT ( 'NONE',  ( -189.8071159312682425, 107.8771087123619594, 35.54271035159577252 ) ) ;
#38176 = EDGE_CURVE ( 'NONE', #64281, #34186, #29443, .T. ) ;
#38177 = ORIENTED_EDGE ( 'NONE', *, *, #41241, .T. ) ;
#38179 = ORIENTED_EDGE ( 'NONE', *, *, #51126, .T. ) ;
#38178 = EDGE_CURVE ( 'NONE', #22871, #51605, #28844, .T. ) ;
#38180 = CARTESIAN_POINT ( 'NONE',  ( 110.7114632166111932, 29.09878355652111281, -50.92243756565373047 ) ) ;
#38181 = FACE_BOUND ( 'NONE', #37650, .T. ) ;
#38182 = CARTESIAN_POINT ( 'NONE',  ( -144.2155061717025717, 61.10843690942980544, -36.99245134645610733 ) ) ;
#38183 = EDGE_CURVE ( 'NONE', #57137, #26420, #18282, .T. ) ;
#38184 = FACE_OUTER_BOUND ( 'NONE', #5231, .T. ) ;
#38186 = ORIENTED_EDGE ( 'NONE', *, *, #44865, .T. ) ;
#38185 = CARTESIAN_POINT ( 'NONE',  ( -147.3641864666714696, 62.38213854487952403, -49.51360668648376162 ) ) ;
#38187 = DIRECTION ( 'NONE',  ( 0.000000000000000000, 1.000000000000000000, 0.000000000000000000 ) ) ;
#38188 = ADVANCED_FACE ( 'NONE', ( #13019 ), #50780, .T. ) ;
#38189 = VECTOR ( 'NONE', #7949, 1000.000000000000000 ) ;
#38190 = ORIENTED_EDGE ( 'NONE', *, *, #7555, .T. ) ;
#38191 = CARTESIAN_POINT ( 'NONE',  ( -131.6508182719823594, 50.40277850441008667, 33.28679821686808538 ) ) ;
#38192 = DIRECTION ( 'NONE',  ( -0.000000000000000000, 1.000000000000000000, -0.000000000000000000 ) ) ;
#38193 = CARTESIAN_POINT ( 'NONE',  ( -452.6627218934915504, 399.9999999999998863, -146.4497041420118251 ) ) ;
#38194 = CARTESIAN_POINT ( 'NONE',  ( 91.50468583833760761, 22.21368636549395248, 31.49154984481617703 ) ) ;
#38195 = CARTESIAN_POINT ( 'NONE',  ( 84.28078136020373279, 18.63296074526051527, -9.350161758405024059 ) ) ;
#38196 = CARTESIAN_POINT ( 'NONE',  ( 92.21267147730745251, 21.40196534721315658, -65.13473199430346483 ) ) ;
#38197 = CARTESIAN_POINT ( 'NONE',  ( 197.3054165770396651, 96.72615186924556951, 8.555290693686146142 ) ) ;
#38198 = FACE_OUTER_BOUND ( 'NONE', #55039, .T. ) ;
#38199 = CARTESIAN_POINT ( 'NONE',  ( -1.224646799147352468E-15, 0.000000000000000000, 0.000000000000000000 ) ) ;
#38200 = VERTEX_POINT ( 'NONE', #61196 ) ;
#38201 = ORIENTED_EDGE ( 'NONE', *, *, #63616, .T. ) ;
#38202 = ADVANCED_FACE ( 'NONE', ( #12661 ), #40086, .F. ) ;
#38203 = CARTESIAN_POINT ( 'NONE',  ( 46.50704915687943242, 9.440294391580035693, 39.82807691976670839 ) ) ;
#38204 = CARTESIAN_POINT ( 'NONE',  ( 15.78827728214693416, 6.500811158483284835, 30.01470767270522089 ) ) ;
#38205 = CARTESIAN_POINT ( 'NONE',  ( 181.0840389613909736, -170.0000000000000000, -16.88050707541594164 ) ) ;
#38207 = EDGE_CURVE ( 'NONE', #26073, #30106, #22709, .T. ) ;
#38206 = FACE_BOUND ( 'NONE', #63415, .T. ) ;
#38208 = EDGE_CURVE ( 'NONE', #43433, #52438, #7389, .T. ) ;
#38209 = AXIS2_PLACEMENT_3D ( 'NONE', #16296, #4368, #26852 ) ;
#38210 = ADVANCED_FACE ( 'NONE', ( #45358 ), #12312, .T. ) ;
#38211 = CARTESIAN_POINT ( 'NONE',  ( 211.7357196141371674, 118.3691710715567211, -41.21681032355412100 ) ) ;
#38212 = CARTESIAN_POINT ( 'NONE',  ( -72.77296415263757012, 21.23032531836537373, -74.12506392022689283 ) ) ;
#38213 = PLANE ( 'NONE',  #21318 ) ;
#38214 = CARTESIAN_POINT ( 'NONE',  ( 45.76405797021010358, 10.34101216371941767, -39.14056405445984410 ) ) ;
#38215 = CARTESIAN_POINT ( 'NONE',  ( 205.1049299651096476, 106.9023875785546522, 71.05227132923316447 ) ) ;
#38216 = ORIENTED_EDGE ( 'NONE', *, *, #4233, .F. ) ;
#38217 = CARTESIAN_POINT ( 'NONE',  ( -103.2169245450825201, 33.25885825286819397, -23.12591867443444471 ) ) ;
#38218 = VERTEX_POINT ( 'NONE', #38696 ) ;
#38219 = FACE_OUTER_BOUND ( 'NONE', #58207, .T. ) ;
#38220 = CARTESIAN_POINT ( 'NONE',  ( 94.14197829520114169, 23.19876121754314369, 64.06685891365469843 ) ) ;
#38221 = CARTESIAN_POINT ( 'NONE',  ( 153.2282895792479280, 54.42637815496160414, -22.96929501619974445 ) ) ;
#38222 = CARTESIAN_POINT ( 'NONE',  ( 444.9999999999999432, 225.0000000000000000, 0.000000000000000000 ) ) ;
#38223 = CARTESIAN_POINT ( 'NONE',  ( -101.8187363387487210, 33.67461140603126069, -76.85912785543963821 ) ) ;
#38224 = AXIS2_PLACEMENT_3D ( 'NONE', #13570, #62453, #68089 ) ;
#38225 = LINE ( 'NONE', #5521, #51760 ) ;
#38226 = CARTESIAN_POINT ( 'NONE',  ( 212.1900147491068651, 117.2197345096297312, 90.80498426450013483 ) ) ;
#38227 = DIRECTION ( 'NONE',  ( -1.850371928290090422E-16, 1.000000000000000000, 1.110223024625156294E-16 ) ) ;
#38228 = ORIENTED_EDGE ( 'NONE', *, *, #60925, .F. ) ;
#38229 = CARTESIAN_POINT ( 'NONE',  ( 55.51528220483957909, 12.08323518953685927, 64.39593437836721534 ) ) ;
#38230 = DIRECTION ( 'NONE',  ( 0.2225209339563184452, -0.9749279121818226201, 0.000000000000000000 ) ) ;
#38231 = CARTESIAN_POINT ( 'NONE',  ( -11.56945424397728139, 8.173256823723106024, 4.267794400975877700 ) ) ;
#38232 = ADVANCED_BREP_SHAPE_REPRESENTATION ( '', ( #17204, #66832 ), #24189 ) ;
#38233 = CARTESIAN_POINT ( 'NONE',  ( 46.12582897016704209, 10.39833982076225105, -66.63266472015294539 ) ) ;
#38234 = CARTESIAN_POINT ( 'NONE',  ( 283.7689755057785987, -21.75207715352313542, 3.301879156304023510 ) ) ;
#38235 = CARTESIAN_POINT ( 'NONE',  ( -107.7743374187917311, 35.66028478413596048, -64.23029970060920846 ) ) ;
#38236 = CARTESIAN_POINT ( 'NONE',  ( 93.88165567369813402, 23.09997474706427667, 92.84299207529174680 ) ) ;
#38237 = VERTEX_POINT ( 'NONE', #60141 ) ;
#38238 = DIRECTION ( 'NONE',  ( -9.747901923620128589E-15, 4.064941510336539763E-15, -0.9999999999999998890 ) ) ;
#38239 = AXIS2_PLACEMENT_3D ( 'NONE', #29844, #13666, #56577 ) ;
#38240 = CARTESIAN_POINT ( 'NONE',  ( 432.4999999999999432, 207.5000000000000284, 1.999999999999998224 ) ) ;
#38241 = CARTESIAN_POINT ( 'NONE',  ( -133.3765738414514885, 51.62252165471732468, 11.85205414610034680 ) ) ;
#38242 = CARTESIAN_POINT ( 'NONE',  ( 15.55634918610397399, -31.11269837220809364, 85.00100000000000477 ) ) ;
#38243 = CARTESIAN_POINT ( 'NONE',  ( -68.06184294702700299, -31.38946074233465211, 41.38025477438755928 ) ) ;
#38244 = EDGE_LOOP ( 'NONE', ( #45118, #32637, #16207 ) ) ;
#38245 = CARTESIAN_POINT ( 'NONE',  ( 0.000000000000000000, 0.000000000000000000, -7.000000000000000000 ) ) ;
#38246 = CARTESIAN_POINT ( 'NONE',  ( -5.401648928593179910, 6.744888135494083947, -8.959184697842486500 ) ) ;
#38247 = CARTESIAN_POINT ( 'NONE',  ( 199.3764173596862008, 100.9540560740992277, -22.29103892941747134 ) ) ;
#38248 = CARTESIAN_POINT ( 'NONE',  ( -153.2300806271756528, 67.40240937773886287, 85.39292924717106814 ) ) ;
#38249 = EDGE_CURVE ( 'NONE', #56564, #38457, #33773, .T. ) ;
#38250 = DIRECTION ( 'NONE',  ( 1.000000000000000000, -4.174438572590588592E-14, 0.000000000000000000 ) ) ;
#38251 = ORIENTED_EDGE ( 'NONE', *, *, #25659, .F. ) ;
#38252 = LINE ( 'NONE', #11508, #25624 ) ;
#38253 = DIRECTION ( 'NONE',  ( 1.000000000000000000, 1.748184826783646563E-16, 0.000000000000000000 ) ) ;
#38254 = CARTESIAN_POINT ( 'NONE',  ( -101.8187363387486926, 33.67461140603126779, 30.51907450641510167 ) ) ;
#38255 = CARTESIAN_POINT ( 'NONE',  ( -29.70166638324966968, 57.83280658984257627, 170.0000000000000000 ) ) ;
#38256 = EDGE_LOOP ( 'NONE', ( #4790, #35354, #39604, #12535 ) ) ;
#38257 = EDGE_CURVE ( 'NONE', #61707, #29751, #7031, .T. ) ;
#38258 = DIRECTION ( 'NONE',  ( 0.000000000000000000, 0.000000000000000000, 1.000000000000000000 ) ) ;
#38259 = EDGE_CURVE ( 'NONE', #59483, #54103, #60920, .T. ) ;
#38260 = ORIENTED_EDGE ( 'NONE', *, *, #21740, .F. ) ;
#38261 = ORIENTED_EDGE ( 'NONE', *, *, #65597, .T. ) ;
#38262 = CARTESIAN_POINT ( 'NONE',  ( -120.3886177497181507, 42.97447856924565457, -91.00427280143986764 ) ) ;
#38263 = DIRECTION ( 'NONE',  ( -0.000000000000000000, 1.000000000000000000, -0.000000000000000000 ) ) ;
#38264 = EDGE_CURVE ( 'NONE', #62436, #54950, #52697, .T. ) ;
#38266 = ORIENTED_EDGE ( 'NONE', *, *, #44386, .T. ) ;
#38265 = CARTESIAN_POINT ( 'NONE',  ( 63.72039997003725631, -12.83396383267754182, 170.0000000000000000 ) ) ;
#38267 = CARTESIAN_POINT ( 'NONE',  ( 157.4703587214989113, 57.65129005721575339, 44.40946747225338953 ) ) ;
#38268 = VECTOR ( 'NONE', #24505, 1000.000000000000114 ) ;
#38269 = DIRECTION ( 'NONE',  ( 0.000000000000000000, 1.000000000000000000, 0.000000000000000000 ) ) ;
#38270 = FACE_OUTER_BOUND ( 'NONE', #31677, .T. ) ;
#38271 = PRODUCT_DEFINITION_SHAPE ( 'NONE', 'NONE',  #69620 ) ;
#38272 = ORIENTED_EDGE ( 'NONE', *, *, #32234, .F. ) ;
#38273 = MECHANICAL_DESIGN_GEOMETRIC_PRESENTATION_REPRESENTATION (  '', ( #65357 ), #11449 ) ;
#38274 = CARTESIAN_POINT ( 'NONE',  ( -39.87467016056562841, -12.30144018097216119, 13.79046412299627455 ) ) ;
#38275 = VECTOR ( 'NONE', #56448, 1000.000000000000000 ) ;
#38276 = DIRECTION ( 'NONE',  ( -0.000000000000000000, 1.000000000000000000, -0.000000000000000000 ) ) ;
#38277 = CARTESIAN_POINT ( 'NONE',  ( 0.000000000000000000, 0.000000000000000000, 30.00000000000000000 ) ) ;
#38278 = CARTESIAN_POINT ( 'NONE',  ( 126.3681350380370674, 38.23508791628619008, 64.34750091452772836 ) ) ;
#38279 = ORIENTED_EDGE ( 'NONE', *, *, #9196, .F. ) ;
#38280 = ORIENTED_EDGE ( 'NONE', *, *, #37038, .T. ) ;
#38281 = ORIENTED_EDGE ( 'NONE', *, *, #4240, .F. ) ;
#38282 = VECTOR ( 'NONE', #54183, 1000.000000000000000 ) ;
#38284 = EDGE_CURVE ( 'NONE', #57393, #34477, #8429, .T. ) ;
#38283 = DIRECTION ( 'NONE',  ( -1.000000000000000000, 0.000000000000000000, 0.000000000000000000 ) ) ;
#38285 = B_SPLINE_CURVE_WITH_KNOTS ( 'NONE', 3,
 ( #66797, #56563, #18936, #8740, #45313, #2758, #19980, #24911, #62183, #46343, #67822, #18585, #8387, #40043, #51641, #30188, #34776, #24573, #68174, #19622, #35458, #40725, #29831, #14688, #3449, #56213, #51301, #46009, #56922, #51976, #29483, #46696, #62886, #41431, #41082, #40385, #23869, #3112, #61502, #62544, #24222, #14355, #30528, #45670 ),
 .UNSPECIFIED., .F., .F.,
 ( 4, 2, 2, 2, 2, 2, 2, 2, 2, 2, 2, 2, 2, 2, 2, 2, 2, 2, 2, 2, 2, 4 ),
 ( 0.02477387709520258857, 0.02633314402883776828, 0.02711277749565535120, 0.02789241096247293758, 0.02945167789610813810, 0.03023131136292572449, 0.03101094482974331434, 0.03257021176337850099, 0.03334984523019608044, 0.03412947869701365988, 0.03568874563064881184, 0.03646837909746639128, 0.03724801256428397073, 0.03802764603110154323, 0.03880727949791912268, 0.04036654643155427463, 0.04192581336518942658, 0.04348508029882458548, 0.04504434723245973743, 0.04660361416609488938, 0.04816288109973004827, 0.04972214803336520023 ),
 .UNSPECIFIED. ) ;
#38286 = CARTESIAN_POINT ( 'NONE',  ( -439.4229916354185548, 400.0000000000021032, 91.05029585799266556 ) ) ;
#38287 = CARTESIAN_POINT ( 'NONE',  ( 0.000000000000000000, 0.000000000000000000, 30.00000000000000000 ) ) ;
#38288 = FACE_OUTER_BOUND ( 'NONE', #588, .T. ) ;
#38289 = CARTESIAN_POINT ( 'NONE',  ( -109.5141185504297283, 36.61008623467700573, 93.79613039457322543 ) ) ;
#38290 = EDGE_CURVE ( 'NONE', #49963, #14782, #62222, .T. ) ;
#38291 = LINE ( 'NONE', #5250, #32517 ) ;
#38292 = DIRECTION ( 'NONE',  ( -0.000000000000000000, -0.000000000000000000, -1.000000000000000000 ) ) ;
#38293 = CARTESIAN_POINT ( 'NONE',  ( -58.13254984326171382, 16.57438752089402456, 84.66073699768521976 ) ) ;
#38294 = CARTESIAN_POINT ( 'NONE',  ( 79.53408731553405175, 17.12082763744059122, 66.53775872133530811 ) ) ;
#38295 = ORIENTED_EDGE ( 'NONE', *, *, #27629, .F. ) ;
#38296 = CARTESIAN_POINT ( 'NONE',  ( -3.306248862503413655, 500.0000000000000000, -51.64566090791306863 ) ) ;
#38297 = EDGE_LOOP ( 'NONE', ( #11534, #18186, #61811, #42813 ) ) ;
#38298 = LINE ( 'NONE', #49181, #50933 ) ;
#38299 = CARTESIAN_POINT ( 'NONE',  ( 212.1983751099433562, 117.2326047784726768, -70.52915068856044911 ) ) ;
#38300 = CARTESIAN_POINT ( 'NONE',  ( 1.499999999999989564, 4.499999999999984901, -46.99999999999997158 ) ) ;
#38301 = CARTESIAN_POINT ( 'NONE',  ( -28.32746765835526048, 69.45586423092609607, 43.58025477438756212 ) ) ;
#38302 = CARTESIAN_POINT ( 'NONE',  ( -37.73701155674110197, 10.71027364713581065, -92.42797313720504349 ) ) ;
#38303 = CARTESIAN_POINT ( 'NONE',  ( -54.09522495088363314, 14.42642983673693102, 3.518423213031079744 ) ) ;
#38304 = LINE ( 'NONE', #16507, #12446 ) ;
#38305 = CARTESIAN_POINT ( 'NONE',  ( 164.9706294237034001, 65.04392654036657007, -70.74285660430801670 ) ) ;
#38306 = ORIENTED_EDGE ( 'NONE', *, *, #6580, .F. ) ;
#38307 = DIRECTION ( 'NONE',  ( 0.7071067811865474617, 0.7071067811865474617, -0.000000000000000000 ) ) ;
#38308 = CARTESIAN_POINT ( 'NONE',  ( -7.486743542469090684, -64.58150799671139453, 170.0000000000000000 ) ) ;
#38309 = EDGE_LOOP ( 'NONE', ( #62646, #42555, #27903, #33429 ) ) ;
#38310 = CARTESIAN_POINT ( 'NONE',  ( 29.86848256228606502, -58.14280299503694494, 41.38025477438755928 ) ) ;
#38311 = ORIENTED_EDGE ( 'NONE', *, *, #15180, .F. ) ;
#38312 = CARTESIAN_POINT ( 'NONE',  ( -81.90020664963797969, 23.57971581008656514, 31.14685346508889907 ) ) ;
#38313 = CARTESIAN_POINT ( 'NONE',  ( -28.81071653159242274, 10.19258396314334902, -62.63311570043980936 ) ) ;
#38314 = LINE ( 'NONE', #11229, #67019 ) ;
#38315 = CARTESIAN_POINT ( 'NONE',  ( 129.5193594945039308, 38.86618897895343139, -10.54188000187672003 ) ) ;
#38316 = VERTEX_POINT ( 'NONE', #56604 ) ;
#38317 = VECTOR ( 'NONE', #40586, 999.9999999999998863 ) ;
#38318 = ORIENTED_EDGE ( 'NONE', *, *, #2303, .T. ) ;
#38319 = DIRECTION ( 'NONE',  ( 0.000000000000000000, 0.000000000000000000, 1.000000000000000000 ) ) ;
#38320 = PRODUCT_DEFINITION ( 'UNKNOWN', '', #24285, #64797 ) ;
#38321 = ORIENTED_EDGE ( 'NONE', *, *, #58649, .F. ) ;
#38322 = CARTESIAN_POINT ( 'NONE',  ( 207.4867844023103487, 110.2451255333963189, 16.83735121052653838 ) ) ;
#38323 = CARTESIAN_POINT ( 'NONE',  ( -146.5230751932348596, 62.99205605665031271, 31.32563957384398279 ) ) ;
#38324 = AXIS2_PLACEMENT_3D ( 'NONE', #44041, #65886, #39475 ) ;
#38325 = CARTESIAN_POINT ( 'NONE',  ( 55.57657751403269231, 11.06944050856661832, 63.17132437929140565 ) ) ;
#38326 = CARTESIAN_POINT ( 'NONE',  ( -4.072522659361696107, 7.683023425615343349, 57.96194782726411887 ) ) ;
#38327 = PRODUCT ( 'hex bolt gradeab_iso_ISO 4014 - M10 x 45 x 26-N', 'hex bolt gradeab_iso_ISO 4014 - M10 x 45 x 26-N', '', ( #28382 ) ) ;
#38328 = EDGE_CURVE ( 'NONE', #59151, #35681, #24613, .T. ) ;
#38329 = CARTESIAN_POINT ( 'NONE',  ( -26.37645167493199949, 9.831227391966869789, -90.95605343330562675 ) ) ;
#38330 = VECTOR ( 'NONE', #31370, 1000.000000000000000 ) ;
#38332 = COLOUR_RGB ( '',0.7921568627450980005, 0.8196078431372548767, 0.9333333333333333481 ) ;
#38331 = DIRECTION ( 'NONE',  ( 0.000000000000000000, 0.000000000000000000, 1.000000000000000000 ) ) ;
#38333 = ORIENTED_EDGE ( 'NONE', *, *, #59308, .F. ) ;
#38334 = EDGE_CURVE ( 'NONE', #9333, #36739, #68547, .T. ) ;
#38335 = DIRECTION ( 'NONE',  ( -0.000000000000000000, -0.000000000000000000, 1.000000000000000000 ) ) ;
#38336 = ORIENTED_EDGE ( 'NONE', *, *, #68683, .F. ) ;
#38337 = ORIENTED_EDGE ( 'NONE', *, *, #8812, .F. ) ;
#38338 = DIRECTION ( 'NONE',  ( -0.000000000000000000, 1.000000000000000000, -0.000000000000000000 ) ) ;
#38339 = CARTESIAN_POINT ( 'NONE',  ( -439.4229916354183842, 388.0000000000064801, -128.9497041420121093 ) ) ;
#38340 = CARTESIAN_POINT ( 'NONE',  ( 0.000000000000000000, 0.000000000000000000, 2.499999999999999556 ) ) ;
#38341 = FACE_OUTER_BOUND ( 'NONE', #59465, .T. ) ;
#38342 = AXIS2_PLACEMENT_3D ( 'NONE', #25782, #4996, #4318 ) ;
#38343 = EDGE_LOOP ( 'NONE', ( #11263, #15502 ) ) ;
#38344 = ADVANCED_FACE ( 'NONE', ( #4184 ), #46047, .F. ) ;
#38345 = CARTESIAN_POINT ( 'NONE',  ( 81.04675113612957205, 17.59091904316107247, 15.40005626147305229 ) ) ;
#38346 = DIRECTION ( 'NONE',  ( 1.000000000000000000, 0.000000000000000000, 0.000000000000000000 ) ) ;
#38347 = CARTESIAN_POINT ( 'NONE',  ( -72.21652659655759976, 19.96855882996548459, 34.05819120719318249 ) ) ;
#38348 = ORIENTED_EDGE ( 'NONE', *, *, #27455, .T. ) ;
#38349 = DIRECTION ( 'NONE',  ( 0.000000000000000000, 0.000000000000000000, 1.000000000000000000 ) ) ;
#38350 = EDGE_CURVE ( 'NONE', #35601, #40482, #28487, .T. ) ;
#38351 = EDGE_CURVE ( 'NONE', #44335, #33511, #8105, .T. ) ;
#38352 = ORIENTED_EDGE ( 'NONE', *, *, #45821, .F. ) ;
#38353 = CARTESIAN_POINT ( 'NONE',  ( -149.0782809666403921, 63.81577337591401289, -76.65738112195566600 ) ) ;
#38354 = PLANE ( 'NONE',  #48347 ) ;
#38355 = DIRECTION ( 'NONE',  ( 0.000000000000000000, 0.000000000000000000, 1.000000000000000000 ) ) ;
#38356 = ORIENTED_EDGE ( 'NONE', *, *, #14857, .F. ) ;
#38357 = DIRECTION ( 'NONE',  ( -0.5128992774058949156, -0.8584487936018728726, 5.102127870520020458E-18 ) ) ;
#38358 = CARTESIAN_POINT ( 'NONE',  ( -443.1918329948321684, 394.9767458440207974, 99.35550699274327258 ) ) ;
#38359 = CARTESIAN_POINT ( 'NONE',  ( 311.0133388548732114, 190.0000000000000000, -153.4166086460792826 ) ) ;
#38360 = CARTESIAN_POINT ( 'NONE',  ( -173.5422248620773189, 89.11126078969418529, -34.71195716474998960 ) ) ;
#38361 = CARTESIAN_POINT ( 'NONE',  ( -131.1078488676298832, 50.02394948559179255, -10.17272884446006742 ) ) ;
#38362 = CARTESIAN_POINT ( 'NONE',  ( 70.60157554497457966, 25.16207943727196295, 41.38025477438755928 ) ) ;
#38363 = DIRECTION ( 'NONE',  ( -1.000000000000000000, -0.000000000000000000, -0.000000000000000000 ) ) ;
#38364 = EDGE_LOOP ( 'NONE', ( #31694, #16951, #54456, #50515, #36928, #64829, #47853, #48516 ) ) ;
#38365 = CARTESIAN_POINT ( 'NONE',  ( 141.3556389957210513, 47.34429831367557284, -70.07195742417799522 ) ) ;
#38366 = DIRECTION ( 'NONE',  ( -0.000000000000000000, -0.000000000000000000, -1.000000000000000000 ) ) ;
#38367 = VERTEX_POINT ( 'NONE', #64653 ) ;
#38368 = CIRCLE ( 'NONE', #17016, 5.000000000000000888 ) ;
#38369 = FACE_BOUND ( 'NONE', #3966, .T. ) ;
#38370 = CARTESIAN_POINT ( 'NONE',  ( -7.336760511143401331, 6.859209474528210393, -77.26262132240756841 ) ) ;
#38371 = CARTESIAN_POINT ( 'NONE',  ( -173.1211646369891355, 88.63826465341151106, 57.66624519710472185 ) ) ;
#38373 = DIRECTION ( 'NONE',  ( 0.000000000000000000, 0.000000000000000000, 1.000000000000000000 ) ) ;
#38372 = VECTOR ( 'NONE', #51603, 1000.000000000000000 ) ;
#38374 = LINE ( 'NONE', #53500, #31211 ) ;
#38375 = CARTESIAN_POINT ( 'NONE',  ( -85.96384504792884229, 26.32782846176032976, 12.82352473700630924 ) ) ;
#38376 = FACE_OUTER_BOUND ( 'NONE', #19529, .T. ) ;
#38377 = EDGE_CURVE ( 'NONE', #52626, #48419, #63619, .T. ) ;
#38378 = CARTESIAN_POINT ( 'NONE',  ( 55.14772863908675049, -34.40534879854660488, 40.00000000000003553 ) ) ;
#38379 = DIRECTION ( 'NONE',  ( -1.000000000000000000, 0.000000000000000000, 0.000000000000000000 ) ) ;
#38381 = CARTESIAN_POINT ( 'NONE',  ( -8.320534640989464492, 7.931748412542457771, 45.11558103944722120 ) ) ;
#38380 = AXIS2_PLACEMENT_3D ( 'NONE', #35362, #56118, #40979 ) ;
#38382 = COLOUR_RGB ( '',0.7921568627450980005, 0.8196078431372548767, 0.9333333333333333481 ) ;
#38383 = CARTESIAN_POINT ( 'NONE',  ( 112.1012908502484891, 29.75117929736501310, 2.996681463395355127 ) ) ;
#38384 = CARTESIAN_POINT ( 'NONE',  ( 87.11239765416380010, 20.65008247340817249, -8.977013608448023874 ) ) ;
#38385 = ORIENTED_EDGE ( 'NONE', *, *, #47258, .T. ) ;
#38386 = DIRECTION ( 'NONE',  ( -0.000000000000000000, -1.000000000000000000, -0.000000000000000000 ) ) ;
#38387 = ORIENTED_EDGE ( 'NONE', *, *, #53101, .F. ) ;
#38388 = DIRECTION ( 'NONE',  ( 1.000000000000000000, 0.000000000000000000, 0.000000000000000000 ) ) ;
#38389 = CARTESIAN_POINT ( 'NONE',  ( 141.0229350107040887, -170.0000000000000000, -95.00000000000133582 ) ) ;
#38390 = CARTESIAN_POINT ( 'NONE',  ( 117.7510257530316551, 33.64085080140208817, 90.74181468113641813 ) ) ;
#38391 = CARTESIAN_POINT ( 'NONE',  ( -142.0860844253783171, 59.41107357617636353, 63.94597921072897861 ) ) ;
#38392 = CARTESIAN_POINT ( 'NONE',  ( 26.11269837220800127, -31.11269837220812562, 85.00100000000000477 ) ) ;
#38393 = CLOSED_SHELL ( 'NONE', ( #69037, #28089, #17067, #62092, #47733, #64765, #43846, #47620, #20644, #29996, #44953, #11723, #372, #66413, #33353, #34145, #27537, #955 ) ) ;
#38394 = CARTESIAN_POINT ( 'NONE',  ( -28.35957743809534648, 10.12373109553627692, -49.66019367601061418 ) ) ;
#38395 = CARTESIAN_POINT ( 'NONE',  ( 210.6475351020683604, 116.6976423915685785, -92.93013880689109385 ) ) ;
#38396 = DIRECTION ( 'NONE',  ( -0.000000000000000000, -0.000000000000000000, 1.000000000000000000 ) ) ;
#38397 = FACE_OUTER_BOUND ( 'NONE', #54835, .T. ) ;
#38398 = ORIENTED_EDGE ( 'NONE', *, *, #2696, .T. ) ;
#38399 = VERTEX_POINT ( 'NONE', #53041 ) ;
#38400 = CARTESIAN_POINT ( 'NONE',  ( 32.37980458033285203, 8.611076697115697343, 66.90419927267225830 ) ) ;
#38401 = LINE ( 'NONE', #1467, #25440 ) ;
#38402 = CARTESIAN_POINT ( 'NONE',  ( 442.3372781065085633, 399.9999999999998863, 83.55029585798818914 ) ) ;
#38403 = CARTESIAN_POINT ( 'NONE',  ( -125.8938041572051389, 46.49392987655490828, -8.069153307770243089 ) ) ;
#38404 = ORIENTED_EDGE ( 'NONE', *, *, #63637, .T. ) ;
#38405 = CARTESIAN_POINT ( 'NONE',  ( 94.06699947028484132, 23.17027898120147711, 9.370048095268675326 ) ) ;
#38406 = ADVANCED_FACE ( 'NONE', ( #10141 ), #26331, .F. ) ;
#38407 = CARTESIAN_POINT ( 'NONE',  ( -13.78293860383720038, 7.352367295275509029, 69.04280783764355078 ) ) ;
#38408 = FACE_OUTER_BOUND ( 'NONE', #54498, .T. ) ;
#38409 = DIRECTION ( 'NONE',  ( -8.673617379884037937E-17, -1.033681467326434969E-16, -1.000000000000000000 ) ) ;
#38410 = CARTESIAN_POINT ( 'NONE',  ( 46.13320811200731697, 9.380653113584065395, -19.61926706393606068 ) ) ;
#38412 = DIRECTION ( 'NONE',  ( 0.3090169943749446757, 0.9510565162951544194, 0.000000000000000000 ) ) ;
#38411 = B_SPLINE_CURVE_WITH_KNOTS ( 'NONE', 3,
 ( #9529, #3552, #2868, #2522, #24680, #24337 ),
 .UNSPECIFIED., .F., .F.,
 ( 4, 2, 4 ),
 ( 1.095770181098114466E-06, 0.03239442681617710901, 0.06478775786217311206 ),
 .UNSPECIFIED. ) ;
#38413 = FACE_BOUND ( 'NONE', #64640, .T. ) ;
#38414 = CARTESIAN_POINT ( 'NONE',  ( -60.65612136648953623, 16.25551606627059442, -37.70714318869556791 ) ) ;
#38415 = ADVANCED_FACE ( 'NONE', ( #20696 ), #21726, .F. ) ;
#38416 =( BOUNDED_CURVE ( )  B_SPLINE_CURVE ( 3, ( #29905, #67893, #14757, #30947 ),
 .UNSPECIFIED., .F., .F. ) 
 B_SPLINE_CURVE_WITH_KNOTS ( ( 4, 4 ),
 ( -8.881784197001252323E-16, 1.570796326794896336 ),
 .UNSPECIFIED. ) 
 CURVE ( )  GEOMETRIC_REPRESENTATION_ITEM ( )  RATIONAL_B_SPLINE_CURVE ( ( 1.000000000000000000, 0.8047378541243649375, 0.8047378541243649375, 1.000000000000000000 ) ) 
 REPRESENTATION_ITEM ( '' )  );
#38417 = EDGE_CURVE ( 'NONE', #24527, #36942, #53382, .T. ) ;
#38418 = B_SPLINE_CURVE_WITH_KNOTS ( 'NONE', 3,
 ( #11644, #64423, #28171, #22556, #22908, #6016, #59134, #5343, #32424, #54902, #38745, #32765, #27475, #10604, #44000, #42952, #12006, #398, #59482, #44353, #60188, #6726, #49622, #53510, #15891, #48223, #17270, #16233, #37336, #37686, #5668, #58788, #32074, #22212, #10956, #53850, #64774, #21855, #16582, #27131, #48918, #48563, #11293 ),
 .UNSPECIFIED., .F., .F.,
 ( 4, 2, 2, 2, 2, 2, 2, 2, 2, 2, 2, 2, 1, 2, 2, 2, 2, 2, 2, 2, 2, 4 ),
 ( 0.02358007599568756260, 0.02505677178601662183, 0.02579511968118114104, 0.02653346757634566025, 0.02801016336667471601, 0.02948685915700377178, 0.03022520705216829792, 0.03096355494733282407, 0.03244025073766187983, 0.03391694652799093213, 0.03539364231831998442, 0.03613199021348451057, 0.03687033810864903671, 0.03760868600381356980, 0.03834703389897809594, 0.03982372968930714824, 0.04130042547963619359, 0.04277712126996524589, 0.04351546916512977203, 0.04425381706029428430, 0.04573051285062330884, 0.04720720864095233338 ),
 .UNSPECIFIED. ) ;
#38419 = ORIENTED_EDGE ( 'NONE', *, *, #380, .T. ) ;
#38420 = DIRECTION ( 'NONE',  ( 0.000000000000000000, 0.000000000000000000, 1.000000000000000000 ) ) ;
#38421 = DIRECTION ( 'NONE',  ( 0.000000000000000000, 0.000000000000000000, -1.000000000000000000 ) ) ;
#38422 = EDGE_CURVE ( 'NONE', #42704, #42164, #6684, .T. ) ;
#38423 = VECTOR ( 'NONE', #51680, 1000.000000000000000 ) ;
#38424 = CARTESIAN_POINT ( 'NONE',  ( -50.14440374537738876, 14.45628984983894938, 70.35385673637195225 ) ) ;
#38425 = DIRECTION ( 'NONE',  ( -1.000000000000000000, -0.000000000000000000, -0.000000000000000000 ) ) ;
#38426 = CARTESIAN_POINT ( 'NONE',  ( -15.55634918610405748, -10.55634918610400597, 2.000000000000001776 ) ) ;
#38427 = DIRECTION ( 'NONE',  ( 0.000000000000000000, 0.000000000000000000, 1.000000000000000000 ) ) ;
#38428 = AXIS2_PLACEMENT_3D ( 'NONE', #49865, #16811, #59029 ) ;
#38429 = ORIENTED_EDGE ( 'NONE', *, *, #68516, .F. ) ;
#38430 = CARTESIAN_POINT ( 'NONE',  ( 58.48209831743720599, 11.66636741727082160, 16.46295100624673680 ) ) ;
#38431 = CARTESIAN_POINT ( 'NONE',  ( 65.35403040894466642, 1.250000000000021982, 3.125053320693567160E-16 ) ) ;
#38432 = EDGE_LOOP ( 'NONE', ( #49546, #49035, #39058, #19573 ) ) ;
#38433 = VECTOR ( 'NONE', #40061, 1000.000000000000227 ) ;
#38434 = CIRCLE ( 'NONE', #8117, 63.00000000000000000 ) ;
#38435 = ORIENTED_EDGE ( 'NONE', *, *, #62169, .T. ) ;
#38436 = FACE_OUTER_BOUND ( 'NONE', #1869, .T. ) ;
#38437 = CARTESIAN_POINT ( 'NONE',  ( 0.1285234777254253835, 24.99966963213046611, 0.000000000000000000 ) ) ;
#38438 = CARTESIAN_POINT ( 'NONE',  ( 104.3931729003987243, 26.26823401847090977, 41.83091430256712329 ) ) ;
#38439 = EDGE_CURVE ( 'NONE', #65498, #37573, #39591, .T. ) ;
#38440 = ORIENTED_EDGE ( 'NONE', *, *, #57725, .F. ) ;
#38441 = EDGE_CURVE ( 'NONE', #22088, #24194, #17135, .T. ) ;
#38442 = EDGE_CURVE ( 'NONE', #32410, #16320, #45302, .T. ) ;
#38443 = AXIS2_PLACEMENT_3D ( 'NONE', #25228, #47342, #31195 ) ;
#38444 = VERTEX_POINT ( 'NONE', #44927 ) ;
#38445 = DIRECTION ( 'NONE',  ( -0.000000000000000000, -0.000000000000000000, -1.000000000000000000 ) ) ;
#38446 = CARTESIAN_POINT ( 'NONE',  ( 161.1112535418156710, 61.83422628788726172, 43.47046046015263698 ) ) ;
#38447 = CARTESIAN_POINT ( 'NONE',  ( -155.2836587093738956, 70.59655508952971559, -73.94790389774894379 ) ) ;
#38448 = CARTESIAN_POINT ( 'NONE',  ( 64.69738688745243849, 14.10375742873389449, 17.78141051354113245 ) ) ;
#38449 = CARTESIAN_POINT ( 'NONE',  ( 90.31682503704259091, 20.71196693118261933, 43.76113064241335593 ) ) ;
#38450 = CARTESIAN_POINT ( 'NONE',  ( -53.38065169970958834, 15.27943072477081543, -35.40114938969493608 ) ) ;
#38451 = PLANE ( 'NONE',  #12309 ) ;
#38452 = B_SPLINE_CURVE_WITH_KNOTS ( 'NONE', 3,
 ( #58632, #53351, #60021, #48759 ),
 .UNSPECIFIED., .F., .F.,
 ( 4, 4 ),
 ( 0.1259919275528360583, 0.1829744153748753543 ),
 .UNSPECIFIED. ) ;
#38453 = CARTESIAN_POINT ( 'NONE',  ( -149.5074843970971017, 65.50121172469320641, -88.50193171241930656 ) ) ;
#38454 = DIRECTION ( 'NONE',  ( 0.000000000000000000, 1.000000000000000000, -0.000000000000000000 ) ) ;
#38455 = DIRECTION ( 'NONE',  ( -0.000000000000000000, -0.000000000000000000, -1.000000000000000000 ) ) ;
#38457 = VERTEX_POINT ( 'NONE', #66412 ) ;
#38456 = CARTESIAN_POINT ( 'NONE',  ( -5.204170427930393515E-14, 6.000000000000000000, -29.99999999999986855 ) ) ;
#38458 = ORIENTED_EDGE ( 'NONE', *, *, #54565, .T. ) ;
#38459 = ORIENTED_EDGE ( 'NONE', *, *, #8011, .F. ) ;
#38460 = CARTESIAN_POINT ( 'NONE',  ( -14.32241591711281892, 7.401556312061829956, -12.31863017529175863 ) ) ;
#38461 = CARTESIAN_POINT ( 'NONE',  ( -166.1407022362849091, 81.12296115130531859, 89.24429516090893344 ) ) ;
#38462 = CARTESIAN_POINT ( 'NONE',  ( 48.11816970607299027, -43.69944786993949748, 40.00000000000003553 ) ) ;
#38463 = DIRECTION ( 'NONE',  ( 0.000000000000000000, -1.000000000000000000, 0.000000000000000000 ) ) ;
#38464 = CARTESIAN_POINT ( 'NONE',  ( -61.77164219855451677, 17.63686644795248171, -39.34642791434716003 ) ) ;
#38465 = CARTESIAN_POINT ( 'NONE',  ( -12.77550690612892481, 8.273784096785060882, -21.72907486570559854 ) ) ;
#38466 = DIRECTION ( 'NONE',  ( -0.000000000000000000, -0.000000000000000000, 1.000000000000000000 ) ) ;
#38467 = CARTESIAN_POINT ( 'NONE',  ( 0.000000000000000000, 0.000000000000000000, 170.0000000000000000 ) ) ;
#38468 = ORIENTED_EDGE ( 'NONE', *, *, #20631, .T. ) ;
#38469 = CARTESIAN_POINT ( 'NONE',  ( 5.737557066527558369, 200.0000000000000000, 2.275957463600584596 ) ) ;
#38470 = ORIENTED_EDGE ( 'NONE', *, *, #39838, .F. ) ;
#38471 = VERTEX_POINT ( 'NONE', #18201 ) ;
#38472 = CARTESIAN_POINT ( 'NONE',  ( -143.4048679855200987, 60.45763799613828837, 15.74344414432664330 ) ) ;
#38473 = VECTOR ( 'NONE', #12403, 1000.000000000000000 ) ;
#38474 = PLANE ( 'NONE',  #46227 ) ;
#38475 = PLANE ( 'NONE',  #17757 ) ;
#38476 = CARTESIAN_POINT ( 'NONE',  ( 144.4165763529819344, 225.8585178651493663, 129.0000000000000000 ) ) ;
#38477 = CARTESIAN_POINT ( 'NONE',  ( -149.5074843970971301, -170.0000000000000000, -34.81283053149196149 ) ) ;
#38478 = DIRECTION ( 'NONE',  ( 0.000000000000000000, 0.000000000000000000, -1.000000000000000000 ) ) ;
#38480 = CARTESIAN_POINT ( 'NONE',  ( 140.5958192060901411, 46.84598876498522912, -19.98049072836446527 ) ) ;
#38479 = B_SPLINE_CURVE_WITH_KNOTS ( 'NONE', 3,
 ( #42472, #30894, #31577, #67843, #47739, #69203, #20328, #9785, #30209, #26310, #68192, #3812, #35479, #52344, #10120, #41451, #19997, #62904, #3467, #21028, #51996, #68522 ),
 .UNSPECIFIED., .F., .F.,
 ( 4, 2, 2, 2, 2, 2, 2, 2, 2, 2, 4 ),
 ( 7.867692934960096083E-17, 0.001318139496345244275, 0.001977209244517810684, 0.002636278992690376660, 0.003954418489035485193, 0.005272557985380592858, 0.005931627733553143655, 0.006590697481725694452, 0.007908836978070800383, 0.009226976474415907181, 0.01054511597076101398 ),
 .UNSPECIFIED. ) ;
#38481 = ORIENTED_EDGE ( 'NONE', *, *, #39579, .F. ) ;
#38482 = VERTEX_POINT ( 'NONE', #55124 ) ;
#38483 = ORIENTED_EDGE ( 'NONE', *, *, #69377, .T. ) ;
#38484 = AXIS2_PLACEMENT_3D ( 'NONE', #21026, #26980, #69201 ) ;
#38485 = CARTESIAN_POINT ( 'NONE',  ( -11.14880195267007323, 7.129907723790828378, 17.51241905048560810 ) ) ;
#38486 = CARTESIAN_POINT ( 'NONE',  ( 32.67604581760325289, 7.629767527669979010, -66.63679567754731181 ) ) ;
#38487 = CARTESIAN_POINT ( 'NONE',  ( -190.6985136298601731, 109.1272424661242582, 94.99999999999866418 ) ) ;
#38488 = AXIS2_PLACEMENT_3D ( 'NONE', #8899, #19795, #8556 ) ;
#38489 = CARTESIAN_POINT ( 'NONE',  ( -38.84150381976580491, 10.92416363971238624, 63.33002578833360730 ) ) ;
#38490 = CARTESIAN_POINT ( 'NONE',  ( 199.3764470687682717, 100.9548044849099142, 68.84309499164012891 ) ) ;
#38491 = ORIENTED_EDGE ( 'NONE', *, *, #60364, .T. ) ;
#38492 = CARTESIAN_POINT ( 'NONE',  ( 187.8973304652192837, 87.27378997243174297, 60.50620952073695946 ) ) ;
#38493 = CARTESIAN_POINT ( 'NONE',  ( -151.2410113808308552, 65.66338888995507261, 57.75535393765130721 ) ) ;
#38494 = CARTESIAN_POINT ( 'NONE',  ( 0.000000000000000000, 70.00000000000000000, 0.000000000000000000 ) ) ;
#38495 = CARTESIAN_POINT ( 'NONE',  ( 112.3013380801408658, 400.0000000000066507, -128.9497041420121093 ) ) ;
#38496 = CARTESIAN_POINT ( 'NONE',  ( -452.6627218934915504, 399.9999999999998863, -146.4497041420118251 ) ) ;
#38497 = CARTESIAN_POINT ( 'NONE',  ( -85.45399718454962112, 25.02415453493131636, -39.41511587279529749 ) ) ;
#38498 = CARTESIAN_POINT ( 'NONE',  ( 10.00000000000000178, 35.26862320190615208, 5.000000000000000000 ) ) ;
#38499 = DIRECTION ( 'NONE',  ( 1.000000000000000000, 0.000000000000000000, 0.000000000000000000 ) ) ;
#38500 = CARTESIAN_POINT ( 'NONE',  ( 8.670103207226929953, 6.377073801252345575, -72.27660206952214139 ) ) ;
#38501 = ADVANCED_FACE ( 'NONE', ( #39655 ), #34037, .F. ) ;
#38502 = ORIENTED_EDGE ( 'NONE', *, *, #37476, .F. ) ;
#38503 = DIRECTION ( 'NONE',  ( 0.000000000000000000, 1.000000000000000000, 0.000000000000000000 ) ) ;
#38504 = EDGE_CURVE ( 'NONE', #33511, #29971, #48529, .T. ) ;
#38505 = CARTESIAN_POINT ( 'NONE',  ( -126.8005235842505840, 47.09307471149451629, -61.79966952219996301 ) ) ;
#38506 = LINE ( 'NONE', #65602, #32046 ) ;
#38507 = LINE ( 'NONE', #6142, #53661 ) ;
#38508 = CARTESIAN_POINT ( 'NONE',  ( 57.39233401791015154, 12.46575990788836563, -65.07837685070954592 ) ) ;
#38509 = VERTEX_POINT ( 'NONE', #45272 ) ;
#38510 = ORIENTED_EDGE ( 'NONE', *, *, #15301, .T. ) ;
#38511 = DIRECTION ( 'NONE',  ( -0.000000000000000000, -1.000000000000000000, -0.000000000000000000 ) ) ;
#38512 = CARTESIAN_POINT ( 'NONE',  ( 180.6638663192742342, 78.18175084954954457, 83.00395592035752657 ) ) ;
#38513 = EDGE_LOOP ( 'NONE', ( #21191, #43908, #68918, #355 ) ) ;
#38514 = EDGE_LOOP ( 'NONE', ( #29159, #37926 ) ) ;
#38515 = VECTOR ( 'NONE', #35394, 1000.000000000000000 ) ;
#38516 = CARTESIAN_POINT ( 'NONE',  ( 179.4207200232661421, 76.93724985992179199, -36.36109878936809281 ) ) ;
#38517 = DIRECTION ( 'NONE',  ( 1.000000000000000000, 0.000000000000000000, 0.000000000000000000 ) ) ;
#38518 = ADVANCED_FACE ( 'NONE', ( #40000 ), #13279, .T. ) ;
#38519 = VERTEX_POINT ( 'NONE', #20270 ) ;
#38520 = CARTESIAN_POINT ( 'NONE',  ( 115.0606351894211201, 32.29586232625067765, 58.18666269473403219 ) ) ;
#38521 = CARTESIAN_POINT ( 'NONE',  ( 140.2200249818744453, 46.60103563593126808, 59.87699706130887023 ) ) ;
#38522 = LINE ( 'NONE', #1588, #7268 ) ;
#38523 = CIRCLE ( 'NONE', #8209, 4.999999999999997335 ) ;
#38524 = CARTESIAN_POINT ( 'NONE',  ( 79.40386128751609363, 17.08093333150470627, -95.00000000000133582 ) ) ;
#38525 = CARTESIAN_POINT ( 'NONE',  ( 87.59061758233885087, 19.75077892934019275, -35.86783240150010954 ) ) ;
#38526 = VECTOR ( 'NONE', #16749, 1000.000000000000114 ) ;
#38527 = CARTESIAN_POINT ( 'NONE',  ( -189.9554299271397895, 108.0836897899587825, 41.65156110337591144 ) ) ;
#38528 = VERTEX_POINT ( 'NONE', #19227 ) ;
#38529 = VECTOR ( 'NONE', #10128, 1000.000000000000000 ) ;
#38530 = DIRECTION ( 'NONE',  ( 0.000000000000000000, 0.000000000000000000, 1.000000000000000000 ) ) ;
#38531 = CIRCLE ( 'NONE', #27273, 2.999999999999981792 ) ;
#38532 = CARTESIAN_POINT ( 'NONE',  ( -78.66644367742111399, 23.39876645725285798, 18.57365054920947500 ) ) ;
#38533 = CARTESIAN_POINT ( 'NONE',  ( -142.8492950481058870, 60.01492924994602163, -45.77552445218916688 ) ) ;
#38534 = DIRECTION ( 'NONE',  ( 1.000000000000000000, 0.000000000000000000, -0.000000000000000000 ) ) ;
#38536 = ORIENTED_EDGE ( 'NONE', *, *, #15570, .F. ) ;
#38535 = DIRECTION ( 'NONE',  ( -1.020422603260505347E-14, 1.000000000000000000, 5.551115123125782702E-17 ) ) ;
#38537 = CARTESIAN_POINT ( 'NONE',  ( 57.09527843067913722, 12.40436368789086430, 5.857540484044117868 ) ) ;
#38538 = VECTOR ( 'NONE', #66370, 1000.000000000000000 ) ;
#38539 = ORIENTED_EDGE ( 'NONE', *, *, #35980, .T. ) ;
#38540 = CARTESIAN_POINT ( 'NONE',  ( -144.3945994505580757, 59.96115386701887928, 59.57298621908066849 ) ) ;
#38541 = B_SPLINE_CURVE_WITH_KNOTS ( 'NONE', 3,
 ( #57449, #68359, #30723, #19466, #14199, #25798, #61685, #13509, #34965, #56408, #56762, #8584, #35657, #57112, #8925, #47914, #54219, #53183, #37357, #9959, #42648, #10627, #32445, #43323, #4664, #426, #53874, #11318, #31412, #5012, #15582, #52842, #58141, #58816 ),
 .UNSPECIFIED., .F., .F.,
 ( 4, 2, 2, 2, 2, 2, 2, 2, 2, 2, 2, 2, 2, 2, 2, 2, 4 ),
 ( 0.01568356594869772802, 0.01666352729433782584, 0.01764348863997792019, 0.01862344998561801801, 0.01960341133125811236, 0.02058337267689821018, 0.02156333402253830800, 0.02254329536817840235, 0.02352325671381850017, 0.02450321805945859799, 0.02548317940509869234, 0.02646314075073879016, 0.02744310209637888798, 0.02842306344201898233, 0.02940302478765908015, 0.03038298613329917797, 0.03136294747893927232 ),
 .UNSPECIFIED. ) ;
#38542 = CARTESIAN_POINT ( 'NONE',  ( 110.2429982417149574, -170.0000000000000000, 10.26666361527366078 ) ) ;
#38543 = LINE ( 'NONE', #6541, #27608 ) ;
#38544 = FACE_OUTER_BOUND ( 'NONE', #36176, .T. ) ;
#38545 = CARTESIAN_POINT ( 'NONE',  ( 80.16939877002758408, 17.31693935407228935, -12.63458944764736636 ) ) ;
#38546 = PLANE ( 'NONE',  #53312 ) ;
#38547 = CARTESIAN_POINT ( 'NONE',  ( -21.95369412746257254, 11.95973721106814835, 0.000000000000000000 ) ) ;
#38548 = CARTESIAN_POINT ( 'NONE',  ( -24.17914301452584169, 8.511888984123499924, -94.57447209120040554 ) ) ;
#38549 = DIRECTION ( 'NONE',  ( 0.000000000000000000, 0.000000000000000000, 1.000000000000000000 ) ) ;
#38550 = ORIENTED_EDGE ( 'NONE', *, *, #59382, .T. ) ;
#38551 = VERTEX_POINT ( 'NONE', #13613 ) ;
#38552 = LINE ( 'NONE', #59997, #66443 ) ;
#38553 = CARTESIAN_POINT ( 'NONE',  ( 181.0840389613909736, -170.0000000000000000, 63.65314469597510794 ) ) ;
#38554 = DIRECTION ( 'NONE',  ( -0.000000000000000000, 1.000000000000000000, -0.000000000000000000 ) ) ;
#38555 = DIRECTION ( 'NONE',  ( -1.000000000000000000, 0.000000000000000000, 0.000000000000000000 ) ) ;
#38556 = CARTESIAN_POINT ( 'NONE',  ( 31.11269837220809364, 15.55634918610396866, 2.000000000000001776 ) ) ;
#38557 = EDGE_CURVE ( 'NONE', #67458, #24702, #45970, .T. ) ;
#38558 = CARTESIAN_POINT ( 'NONE',  ( 0.000000000000000000, 0.000000000000000000, 170.0000000000000000 ) ) ;
#38559 = DIRECTION ( 'NONE',  ( 0.000000000000000000, 0.000000000000000000, 1.000000000000000000 ) ) ;
#38560 = CARTESIAN_POINT ( 'NONE',  ( 45.04020069093783007, 10.22779424730543418, -38.14995898565744170 ) ) ;
#38561 = CARTESIAN_POINT ( 'NONE',  ( 442.3372781065085633, 399.9999999999998863, 103.5502958579881891 ) ) ;
#38562 = ORIENTED_EDGE ( 'NONE', *, *, #59931, .F. ) ;
#38563 = CARTESIAN_POINT ( 'NONE',  ( -104.1342612728951309, 33.73231160250195160, -22.95220324455834415 ) ) ;
#38564 = ORIENTED_EDGE ( 'NONE', *, *, #22627, .F. ) ;
#38565 = EDGE_CURVE ( 'NONE', #43150, #10057, #56405, .T. ) ;
#38566 = LINE ( 'NONE', #33310, #3787 ) ;
#38567 = CARTESIAN_POINT ( 'NONE',  ( -85.98021075183530115, 25.24360504037805342, 89.91407000372294078 ) ) ;
#38568 = CARTESIAN_POINT ( 'NONE',  ( 0.000000000000000000, 0.000000000000000000, 10.00000000000000000 ) ) ;
#38569 = CARTESIAN_POINT ( 'NONE',  ( -15.55634918610411077, -46.66904755831208718, 2.000000000000001776 ) ) ;
#38570 = LINE ( 'NONE', #8310, #52331 ) ;
#38571 = B_SPLINE_CURVE_WITH_KNOTS ( 'NONE', 3,
 ( #27526, #43694, #16964, #51771, #13786, #30319, #8168, #66931, #19064, #29615, #40179, #2205, #7828, #56016, #8523, #13449, #46138, #61632, #3576, #66583, #25049, #51434, #62321, #23657, #50725, #24358, #51082, #3245, #29972, #14139, #2898, #45449, #18373, #45097, #45802, #39828, #61288, #67609, #13109, #34910, #56348, #67280, #34575, #18723, #35597, #24703, #19408 ),
 .UNSPECIFIED., .F., .F.,
 ( 4, 2, 2, 2, 2, 2, 2, 2, 2, 2, 2, 2, 1, 2, 2, 2, 2, 2, 2, 2, 2, 2, 2, 4 ),
 ( 0.000000000000000000, 0.001520400357569040442, 0.002280600536353578119, 0.003040800715138115579, 0.004561201072707176188, 0.005321401251491689362, 0.006081601430276202536, 0.007602001787845172505, 0.008362201966629670066, 0.009122402145414166760, 0.01064280250298316188, 0.01140300268176763950, 0.01216320286055211537, 0.01292340303933659298, 0.01368360321812107060, 0.01520400357569003102, 0.01596420375447449302, 0.01672440393325895155, 0.01824480429082784433, 0.01976520464839674057, 0.02052540482718119563, 0.02128560500596565069, 0.02280600536353454000, 0.02432640572110343277 ),
 .UNSPECIFIED. ) ;
#38572 = CARTESIAN_POINT ( 'NONE',  ( -65.36598343705435354, 0.000000000000000000, 41.38025477438755928 ) ) ;
#38573 = CONICAL_SURFACE ( 'NONE', #28485, 65.00000000000000000, 0.7853981633974497223 ) ;
#38574 = DIRECTION ( 'NONE',  ( 0.5409654940743039431, 0.000000000000000000, 0.8410447872859947438 ) ) ;
#38575 = VECTOR ( 'NONE', #28723, 1000.000000000000227 ) ;
#38576 = CARTESIAN_POINT ( 'NONE',  ( -5.000000000000000000, 0.000000000000000000, 85.00100000000000477 ) ) ;
#38577 = CARTESIAN_POINT ( 'NONE',  ( -46.95151367498729655, -47.29862477898760176, 34.48241795236666718 ) ) ;
#38578 = CYLINDRICAL_SURFACE ( 'NONE', #57817, 4.999999999999990230 ) ;
#38579 = ORIENTED_EDGE ( 'NONE', *, *, #11924, .F. ) ;
#38580 = DIRECTION ( 'NONE',  ( -0.000000000000000000, 0.000000000000000000, -1.000000000000000000 ) ) ;
#38581 = DIRECTION ( 'NONE',  ( 1.000000000000000000, 0.000000000000000000, 0.000000000000000000 ) ) ;
#38582 = CARTESIAN_POINT ( 'NONE',  ( 15.55634918610409656, 31.11269837220803325, 85.00100000000000477 ) ) ;
#38584 = EDGE_CURVE ( 'NONE', #9181, #40644, #27216, .T. ) ;
#38583 = AXIS2_PLACEMENT_3D ( 'NONE', #52067, #8824, #46434 ) ;
#38585 = DIRECTION ( 'NONE',  ( 0.7227948638273978821, -0.6910626489868580968, 2.500042656554810340E-16 ) ) ;
#38586 = CARTESIAN_POINT ( 'NONE',  ( -62.21428173307536724, 16.71931747086482289, -94.13522999573226002 ) ) ;
#38587 = CARTESIAN_POINT ( 'NONE',  ( 49.76301652092226391, -41.81676920493045202, 40.00000000000003553 ) ) ;
#38588 = AXIS2_PLACEMENT_3D ( 'NONE', #3056, #24166, #24518 ) ;
#38589 = EDGE_CURVE ( 'NONE', #33967, #34424, #45630, .T. ) ;
#38590 = CARTESIAN_POINT ( 'NONE',  ( 81.80567187957538522, 18.88678701137715876, 85.11920350517479505 ) ) ;
#38591 = EDGE_LOOP ( 'NONE', ( #32038, #27561, #5903, #45807 ) ) ;
#38593 = AXIS2_PLACEMENT_3D ( 'NONE', #45329, #34454, #41698 ) ;
#38592 = DIRECTION ( 'NONE',  ( 1.000000000000000000, 0.000000000000000000, 0.000000000000000000 ) ) ;
#38594 = EDGE_CURVE ( 'NONE', #913, #8504, #67783, .T. ) ;
#38595 = DIRECTION ( 'NONE',  ( 1.000000000000000000, 1.110223024625155594E-14, -1.110223024625155594E-14 ) ) ;
#38596 = DIRECTION ( 'NONE',  ( -0.000000000000000000, 0.000000000000000000, -1.000000000000000000 ) ) ;
#38597 = CARTESIAN_POINT ( 'NONE',  ( -166.2053056899075045, 81.18967388993343093, -45.12821780567188057 ) ) ;
#38598 = CARTESIAN_POINT ( 'NONE',  ( -130.5811943660945076, 50.88295841537571818, -48.28834053933531578 ) ) ;
#38599 = EDGE_LOOP ( 'NONE', ( #13458, #37287, #24657, #985 ) ) ;
#38600 = CARTESIAN_POINT ( 'NONE',  ( -124.3331814159187445, 45.47486189329071493, -49.75303911620572705 ) ) ;
#38601 = CARTESIAN_POINT ( 'NONE',  ( 86.62931800182293784, -170.0000000000000000, -43.32156419891173016 ) ) ;
#38602 = DIRECTION ( 'NONE',  ( -1.000000000000000000, 0.000000000000000000, 0.000000000000000000 ) ) ;
#38603 = CARTESIAN_POINT ( 'NONE',  ( -3.255961059272210800, 7.643453059677442596, -63.79517828393875334 ) ) ;
#38604 = DIRECTION ( 'NONE',  ( -1.000000000000000000, 0.000000000000000000, 0.000000000000000000 ) ) ;
#38605 = ADVANCED_FACE ( 'NONE', ( #29793 ), #20494, .T. ) ;
#38606 = VERTEX_POINT ( 'NONE', #62503 ) ;
#38607 = LINE ( 'NONE', #7989, #26706 ) ;
#38608 = CARTESIAN_POINT ( 'NONE',  ( 197.9847015768255289, 97.56951352050454318, -40.46952643750044132 ) ) ;
#38609 = CARTESIAN_POINT ( 'NONE',  ( -151.6648563624118822, 67.36546864992756412, 31.02422955355707046 ) ) ;
#38610 = ADVANCED_FACE ( 'NONE', ( #14649 ), #53065, .T. ) ;
#38611 = EDGE_CURVE ( 'NONE', #43052, #28243, #10396, .T. ) ;
#38612 = CARTESIAN_POINT ( 'NONE',  ( -44.99999999999998579, -22.99999999999998579, 4.000000000000000000 ) ) ;
#38614 = ORIENTED_EDGE ( 'NONE', *, *, #65252, .F. ) ;
#38613 = DIRECTION ( 'NONE',  ( 1.000000000000000000, 0.000000000000000000, 0.000000000000000000 ) ) ;
#38615 = CARTESIAN_POINT ( 'NONE',  ( -417.6627218934913230, 179.4906275429376308, -146.4497041420118819 ) ) ;
#38616 = ORIENTED_EDGE ( 'NONE', *, *, #68602, .T. ) ;
#38617 = ORIENTED_EDGE ( 'NONE', *, *, #55086, .T. ) ;
#38618 = CARTESIAN_POINT ( 'NONE',  ( -71.41745561414265353, 19.69148172991711832, -13.78189858334474671 ) ) ;
#38619 = FACE_OUTER_BOUND ( 'NONE', #68727, .T. ) ;
#38620 = CIRCLE ( 'NONE', #48735, 65.36598343705435354 ) ;
#38622 = ORIENTED_EDGE ( 'NONE', *, *, #62766, .F. ) ;
#38621 = CARTESIAN_POINT ( 'NONE',  ( -15.07235766390728493, 8.482541916553472561, -71.71007873016166911 ) ) ;
#38623 = CARTESIAN_POINT ( 'NONE',  ( 164.8407099662995563, 63.61629583487393802, 35.49381950204995917 ) ) ;
#38624 = DIRECTION ( 'NONE',  ( 0.000000000000000000, 0.000000000000000000, 1.000000000000000000 ) ) ;
#38625 = CARTESIAN_POINT ( 'NONE',  ( -75.00636493611887090, 22.03142602679956852, -36.05143679334967999 ) ) ;
#38626 = AXIS2_PLACEMENT_3D ( 'NONE', #25871, #4067, #25533 ) ;
#38627 = ORIENTED_EDGE ( 'NONE', *, *, #48017, .T. ) ;
#38628 = DIRECTION ( 'NONE',  ( -1.000000000000000000, 0.000000000000000000, 0.000000000000000000 ) ) ;
#38629 = VECTOR ( 'NONE', #5353, 1000.000000000000000 ) ;
#38630 = VECTOR ( 'NONE', #64814, 1000.000000000000000 ) ;
#38631 = CARTESIAN_POINT ( 'NONE',  ( -34.74740905761646559, 10.15745573515589406, -9.223982854342375859 ) ) ;
#38632 = LINE ( 'NONE', #11893, #52727 ) ;
#38633 = VECTOR ( 'NONE', #56608, 1000.000000000000114 ) ;
#38634 = CARTESIAN_POINT ( 'NONE',  ( -37.79601571721868680, 10.72155118426296738, -65.67424366896023002 ) ) ;
#38635 = CARTESIAN_POINT ( 'NONE',  ( 23.23965501943001044, 7.861749956303023978, 63.37552610149469956 ) ) ;
#38636 = ORIENTED_EDGE ( 'NONE', *, *, #30665, .F. ) ;
#38637 = VERTEX_POINT ( 'NONE', #62141 ) ;
#38638 = VERTEX_POINT ( 'NONE', #40682 ) ;
#38639 = CIRCLE ( 'NONE', #12799, 20.00000000000001066 ) ;
#38640 = CARTESIAN_POINT ( 'NONE',  ( 207.9985316690167565, 110.9796440870787393, -90.77140804177048494 ) ) ;
#38641 = CARTESIAN_POINT ( 'NONE',  ( -48.13019811071813336, 12.93401924038758288, 94.41062383682593406 ) ) ;
#38642 = FACE_OUTER_BOUND ( 'NONE', #3867, .T. ) ;
#38643 = CARTESIAN_POINT ( 'NONE',  ( -38.26732153931118319, 10.81230693396214093, -45.92944804569359007 ) ) ;
#38644 = EDGE_CURVE ( 'NONE', #18346, #10603, #9976, .T. ) ;
#38645 = CARTESIAN_POINT ( 'NONE',  ( -101.7332236082777257, 32.50383353354374805, 84.22225394076856730 ) ) ;
#38646 = LINE ( 'NONE', #60086, #56127 ) ;
#38647 = LINE ( 'NONE', #48470, #32811 ) ;
#38648 = CARTESIAN_POINT ( 'NONE',  ( -77.71801202538870257, 23.03755222122951452, -8.316084935337491046 ) ) ;
#38649 = CARTESIAN_POINT ( 'NONE',  ( 84.28078136020376121, 18.63296074526051527, 71.18349001298599887 ) ) ;
#38650 = ORIENTED_EDGE ( 'NONE', *, *, #68543, .T. ) ;
#38651 = ADVANCED_FACE ( 'NONE', ( #17683 ), #3681, .T. ) ;
#38652 = CARTESIAN_POINT ( 'NONE',  ( -36.11269837220804391, 15.55634918610408945, 85.00100000000000477 ) ) ;
#38653 = DIRECTION ( 'NONE',  ( 1.697894969632810155E-16, -1.110223024625155801E-16, 1.000000000000000000 ) ) ;
#38654 = ORIENTED_EDGE ( 'NONE', *, *, #40988, .T. ) ;
#38655 = CARTESIAN_POINT ( 'NONE',  ( 204.6977192012829789, 106.3443248447423457, -63.17048162308526571 ) ) ;
#38656 = LINE ( 'NONE', #38300, #21996 ) ;
#38657 = CARTESIAN_POINT ( 'NONE',  ( -75.00168449119588843, 20.95943092127969720, 17.62176771239603568 ) ) ;
#38658 = CARTESIAN_POINT ( 'NONE',  ( -118.3948752128398496, 42.92869324237091178, 65.26186531831542936 ) ) ;
#38659 = CARTESIAN_POINT ( 'NONE',  ( -53.14475157111026249, 14.17819596930906911, 3.715487147916443522 ) ) ;
#38660 = CARTESIAN_POINT ( 'NONE',  ( 152.3102623290679674, 53.74757787434987222, -38.17601757745164548 ) ) ;
#38661 = PLANE ( 'NONE',  #38895 ) ;
#38662 = ORIENTED_EDGE ( 'NONE', *, *, #40848, .T. ) ;
#38663 = DIRECTION ( 'NONE',  ( -1.000000000000000000, -0.000000000000000000, -0.000000000000000000 ) ) ;
#38664 = FACE_OUTER_BOUND ( 'NONE', #19018, .T. ) ;
#38665 = ORIENTED_EDGE ( 'NONE', *, *, #7644, .T. ) ;
#38666 = DIRECTION ( 'NONE',  ( -0.000000000000000000, -0.000000000000000000, 1.000000000000000000 ) ) ;
#38667 = ORIENTED_EDGE ( 'NONE', *, *, #35754, .F. ) ;
#38668 = EDGE_CURVE ( 'NONE', #50651, #52456, #58245, .T. ) ;
#38669 = CARTESIAN_POINT ( 'NONE',  ( -84.23431294393863311, 24.52078568147202731, 32.86922510554116172 ) ) ;
#38670 = CARTESIAN_POINT ( 'NONE',  ( -26.49928411671542605, 9.848831533840670005, -63.99709101584238624 ) ) ;
#38671 = CARTESIAN_POINT ( 'NONE',  ( 46.51679720856117228, 10.46086439153924807, 34.99061173750302345 ) ) ;
#38672 = ADVANCED_FACE ( 'NONE', ( #47333 ), #20607, .T. ) ;
#38673 = AXIS2_PLACEMENT_3D ( 'NONE', #51870, #19513, #64753 ) ;
#38674 = CARTESIAN_POINT ( 'NONE',  ( -146.7345109736526751, 61.86270848728300109, 18.34836298419372014 ) ) ;
#38675 = EDGE_CURVE ( 'NONE', #63625, #47023, #55341, .T. ) ;
#38676 = ORIENTED_EDGE ( 'NONE', *, *, #18278, .T. ) ;
#38677 = CIRCLE ( 'NONE', #31790, 21.50000000000000000 ) ;
#38678 = EDGE_LOOP ( 'NONE', ( #47343, #48973, #30945, #21754 ) ) ;
#38679 = DIRECTION ( 'NONE',  ( 0.000000000000000000, 0.000000000000000000, -1.000000000000000000 ) ) ;
#38680 = ORIENTED_EDGE ( 'NONE', *, *, #54016, .T. ) ;
#38681 = LINE ( 'NONE', #41806, #5373 ) ;
#38682 = CARTESIAN_POINT ( 'NONE',  ( 0.000000000000000000, 0.000000000000000000, 41.38025477438755928 ) ) ;
#38683 = CARTESIAN_POINT ( 'NONE',  ( -55.05276343752910151, 15.72344139423345588, -88.90542517938717992 ) ) ;
#38684 = CARTESIAN_POINT ( 'NONE',  ( 140.7150918341941122, 46.92378309712762530, 93.81823441900311877 ) ) ;
#38685 = VECTOR ( 'NONE', #11655, 1000.000000000000000 ) ;
#38686 = CARTESIAN_POINT ( 'NONE',  ( 198.8948370720704588, 100.3380403442581752, -92.75881832202279043 ) ) ;
#38687 = CIRCLE ( 'NONE', #11708, 8.000000000000000000 ) ;
#38688 = SURFACE_STYLE_USAGE ( .BOTH. , #65422 ) ;
#38689 = VERTEX_POINT ( 'NONE', #44403 ) ;
#38690 = VECTOR ( 'NONE', #52957, 1000.000000000000000 ) ;
#38691 = B_SPLINE_CURVE_WITH_KNOTS ( 'NONE', 3,
 ( #28401, #49491, #34040, #44930, #60052, #18204, #60416, #2375, #66415, #29109, #55479, #1324, #22779, #17856, #23834, #67106, #39658, #18549, #33349, #45277, #54780, #61113, #12937, #12234, #2721, #13283, #6605, #23490, #65707, #33699, #50214, #49846, #7303, #56177, #50558, #17497, #34398, #55126, #1675, #7663, #23139, #44585, #66065, #55842, #39316 ),
 .UNSPECIFIED., .F., .F.,
 ( 4, 2, 2, 1, 2, 2, 2, 2, 2, 2, 2, 2, 2, 2, 2, 2, 2, 2, 2, 2, 2, 2, 4 ),
 ( 0.02345095402629350512, 0.02491692321306678351, 0.02564990780645342791, 0.02638289239984007578, 0.02711587699322672018, 0.02784886158661336458, 0.02931483077338667073, 0.03004781536677332901, 0.03078079996015999076, 0.03224676914693330732, 0.03297975374031995865, 0.03371273833370660306, 0.03517870752047990573, 0.03664467670725320148, 0.03737766130063985281, 0.03811064589402650415, 0.03957661508079981377, 0.04104258426757313033, 0.04250855345434643995, 0.04324153804773309823, 0.04397452264111975651, 0.04544049182789306612, 0.04690646101466638268 ),
 .UNSPECIFIED. ) ;
#38692 = CARTESIAN_POINT ( 'NONE',  ( -121.5921196778231774, 43.72569502503143468, -75.42000096489594796 ) ) ;
#38693 = ORIENTED_EDGE ( 'NONE', *, *, #4757, .F. ) ;
#38694 = ORIENTED_EDGE ( 'NONE', *, *, #39300, .T. ) ;
#38695 = DIRECTION ( 'NONE',  ( 1.000000000000000000, 0.000000000000000000, -0.000000000000000000 ) ) ;
#38696 = CARTESIAN_POINT ( 'NONE',  ( 110.2429982417149432, 28.88204397445229077, -35.92243756565368784 ) ) ;
#38697 = LINE ( 'NONE', #43952, #21800 ) ;
#38698 = FACE_OUTER_BOUND ( 'NONE', #68739, .T. ) ;
#38699 = CARTESIAN_POINT ( 'NONE',  ( -41.50537345350708307, 50.04124777106294886, 0.000000000000000000 ) ) ;
#38700 = ADVANCED_FACE ( 'NONE', ( #31522 ), #45255, .T. ) ;
#38701 = ADVANCED_FACE ( 'NONE', ( #4777, #58579, #58926 ), #26247, .F. ) ;
#38702 = VERTEX_POINT ( 'NONE', #32551 ) ;
#38703 = EDGE_CURVE ( 'NONE', #65008, #3292, #48022, .T. ) ;
#38704 = PLANE ( 'NONE',  #49610 ) ;
#38705 = ORIENTED_EDGE ( 'NONE', *, *, #12189, .T. ) ;
#38706 = CARTESIAN_POINT ( 'NONE',  ( -74.17694007417655655, 20.66176641130876135, 43.94577668441134222 ) ) ;
#38707 = EDGE_LOOP ( 'NONE', ( #46746, #57844, #6303, #68519 ) ) ;
#38708 = CARTESIAN_POINT ( 'NONE',  ( 133.1039262992642591, 40.97158229895780579, -89.74086916301752126 ) ) ;
#38709 = VERTEX_POINT ( 'NONE', #52618 ) ;
#38710 = CARTESIAN_POINT ( 'NONE',  ( -144.3945994505580757, 59.96115386701888639, -74.64976673323776879 ) ) ;
#38711 = CARTESIAN_POINT ( 'NONE',  ( 7.484861546145031852, 64.56761454192836425, 40.00000000000003553 ) ) ;
#38712 = CYLINDRICAL_SURFACE ( 'NONE', #68746, 7.500000000000013323 ) ;
#38713 = VERTEX_POINT ( 'NONE', #53646 ) ;
#38714 = DIRECTION ( 'NONE',  ( 0.6910626489868580968, 0.7227948638273978821, -0.000000000000000000 ) ) ;
#38715 = CARTESIAN_POINT ( 'NONE',  ( -443.6249203811465804, 394.9114286947786354, 98.78386141483146332 ) ) ;
#38716 = CARTESIAN_POINT ( 'NONE',  ( 32.15284246740100116, 8.588257691344876932, 39.35317935462418859 ) ) ;
#38717 = VECTOR ( 'NONE', #27810, 1000.000000000000000 ) ;
#38718 = CARTESIAN_POINT ( 'NONE',  ( -180.4651598106648294, 97.28730001475658185, -40.66035573052959506 ) ) ;
#38719 = CARTESIAN_POINT ( 'NONE',  ( -127.6992109187852265, 47.69334801994797601, -22.86298476009724467 ) ) ;
#38720 = DIRECTION ( 'NONE',  ( 0.000000000000000000, 0.000000000000000000, -1.000000000000000000 ) ) ;
#38721 = CARTESIAN_POINT ( 'NONE',  ( -442.6627218934912662, 389.9999999999998295, 113.5502958579881465 ) ) ;
#38722 = B_SPLINE_CURVE_WITH_KNOTS ( 'NONE', 3,
 ( #7774, #24651, #23607, #24307, #8113, #34858, #7433, #2494, #51378, #3194, #14084, #39774, #55962, #39425, #12699, #2152, #29563, #40465, #66876, #13059, #35191, #23947, #51027, #55247, #66528, #49976, #45045, #60876, #56646, #45749, #61235, #61909, #34165, #8466, #2841, #67229, #13733, #29918, #18674, #61584, #46086, #7070, #44708 ),
 .UNSPECIFIED., .F., .F.,
 ( 4, 2, 2, 2, 2, 2, 2, 2, 2, 2, 2, 2, 1, 2, 2, 2, 2, 2, 2, 2, 2, 4 ),
 ( 0.02390068823634510647, 0.02538837671117073411, 0.02613222094858354966, 0.02687606518599636521, 0.02836375366082197896, 0.02985144213564758925, 0.03059528637306041521, 0.03133913061047324117, 0.03282681908529890696, 0.03431450756012456582, 0.03580219603495023162, 0.03654604027236305064, 0.03728988450977585578, 0.03803372874718866786, 0.03877757298460147994, 0.04026526145942714574, 0.04175294993425280460, 0.04324063840907846346, 0.04398448264649129635, 0.04472832688390412231, 0.04621601535872980893, 0.04770370383355549554 ),
 .UNSPECIFIED. ) ;
#38723 = ORIENTED_EDGE ( 'NONE', *, *, #28685, .T. ) ;
#38724 = DIRECTION ( 'NONE',  ( 0.000000000000000000, -0.000000000000000000, 1.000000000000000000 ) ) ;
#38725 = CARTESIAN_POINT ( 'NONE',  ( 10.55634918610406281, 20.55634918610400064, 85.00100000000000477 ) ) ;
#38726 = ORIENTED_EDGE ( 'NONE', *, *, #6103, .T. ) ;
#38727 = FACE_BOUND ( 'NONE', #17557, .T. ) ;
#38728 = CARTESIAN_POINT ( 'NONE',  ( -4.070918861171934466, 6.675509947362631813, -63.26537528929446097 ) ) ;
#38729 = AXIS2_PLACEMENT_3D ( 'NONE', #25963, #35830, #9439 ) ;
#38730 = CARTESIAN_POINT ( 'NONE',  ( -176.3763474213711220, 92.36993073950279154, 58.39546644310473766 ) ) ;
#38731 = CARTESIAN_POINT ( 'NONE',  ( 51.00231672172485275, 42.89951318340155240, 34.48241795236666718 ) ) ;
#38732 = CARTESIAN_POINT ( 'NONE',  ( 0.000000000000000000, 0.000000000000000000, 41.38025477438755928 ) ) ;
#38733 = LINE ( 'NONE', #60177, #34418 ) ;
#38734 = DIRECTION ( 'NONE',  ( -1.850550996349095901E-16, 1.000000000000000000, -5.551115123125781470E-17 ) ) ;
#38735 = AXIS2_PLACEMENT_3D ( 'NONE', #49195, #58716, #6651 ) ;
#38736 = CARTESIAN_POINT ( 'NONE',  ( -151.6716822472524200, 66.03661194063732864, 4.181547750986519318 ) ) ;
#38737 = CARTESIAN_POINT ( 'NONE',  ( -74.62027799914388027, 20.82126111774559618, -89.97495102220065633 ) ) ;
#38738 = VECTOR ( 'NONE', #50391, 1000.000000000000000 ) ;
#38739 = CARTESIAN_POINT ( 'NONE',  ( -15.13211202216340645, 8.488266782358815377, 35.90622617973726705 ) ) ;
#38740 = CARTESIAN_POINT ( 'NONE',  ( 114.4640969196985765, 30.88424258798502109, 4.062649201705831103 ) ) ;
#38741 = CARTESIAN_POINT ( 'NONE',  ( 93.87111289824407834, 23.09598275302506210, -14.46140212872976960 ) ) ;
#38742 = ORIENTED_EDGE ( 'NONE', *, *, #60364, .F. ) ;
#38743 = B_SPLINE_CURVE_WITH_KNOTS ( 'NONE', 3,
 ( #62261, #56641, #7770, #7427 ),
 .UNSPECIFIED., .F., .F.,
 ( 4, 4 ),
 ( 9.900409499076797036E-07, 0.05658314289920116785 ),
 .UNSPECIFIED. ) ;
#38744 = EDGE_CURVE ( 'NONE', #937, #58062, #42069, .T. ) ;
#38745 = CARTESIAN_POINT ( 'NONE',  ( -36.37229078872273647, 11.47648211215765279, 5.201659389993076310 ) ) ;
#38746 = ORIENTED_EDGE ( 'NONE', *, *, #1768, .T. ) ;
#38747 = CARTESIAN_POINT ( 'NONE',  ( -78.66644367742111399, -170.0000000000000000, 91.60730232060049616 ) ) ;
#38748 = CARTESIAN_POINT ( 'NONE',  ( 79.14113188808480004, 18.05280674635441684, -69.67520535789378755 ) ) ;
#38749 = CARTESIAN_POINT ( 'NONE',  ( 107.1638638624856554, 28.58522774667099853, 83.95379775939885292 ) ) ;
#38750 = CARTESIAN_POINT ( 'NONE',  ( 69.36122620657974380, -170.0000000000000000, 94.99999999999866418 ) ) ;
#38751 = CARTESIAN_POINT ( 'NONE',  ( -15.30012024911653334, 7.493578574797995273, 90.60732787615089023 ) ) ;
#38752 = CARTESIAN_POINT ( 'NONE',  ( -25.48750459758502629, 9.705678256319565378, -47.40729988162036079 ) ) ;
#38753 = CARTESIAN_POINT ( 'NONE',  ( -15.76129977463529563, 63.43731725181438463, 41.38025477438755928 ) ) ;
#38754 = DIRECTION ( 'NONE',  ( -0.000000000000000000, -0.000000000000000000, 1.000000000000000000 ) ) ;
#38755 = DIRECTION ( 'NONE',  ( -0.7071067811865475727, -2.220446049250312341E-16, 0.7071067811865474617 ) ) ;
#38756 = ORIENTED_EDGE ( 'NONE', *, *, #17570, .T. ) ;
#38757 = B_SPLINE_CURVE_WITH_KNOTS ( 'NONE', 3,
 ( #55088, #29412, #2679, #60721, #49455, #11835 ),
 .UNSPECIFIED., .F., .F.,
 ( 4, 2, 4 ),
 ( 0.01291313371729459550, 0.01525081363757311778, 0.01758849355785164006 ),
 .UNSPECIFIED. ) ;
#38758 = VERTEX_POINT ( 'NONE', #48352 ) ;
#38759 = EDGE_CURVE ( 'NONE', #27523, #38117, #185, .T. ) ;
#38760 = CARTESIAN_POINT ( 'NONE',  ( 32.66883187925818532, 8.640402022338117050, 60.91819067178263225 ) ) ;
#38761 = CARTESIAN_POINT ( 'NONE',  ( 177.5945652320814077, 75.14951358071817822, 70.29580567297929861 ) ) ;
#38762 = CARTESIAN_POINT ( 'NONE',  ( 0.000000000000000000, 0.000000000000000000, 0.000000000000000000 ) ) ;
#38763 = EDGE_CURVE ( 'NONE', #9201, #10179, #41943, .T. ) ;
#38764 = CARTESIAN_POINT ( 'NONE',  ( 15.55634918610400241, -10.55634918610406281, 85.00100000000000477 ) ) ;
#38765 = EDGE_CURVE ( 'NONE', #53581, #50424, #13107, .T. ) ;
#38766 = EDGE_CURVE ( 'NONE', #50285, #7511, #56699, .T. ) ;
#38767 = LINE ( 'NONE', #54216, #47613 ) ;
#38768 = EDGE_LOOP ( 'NONE', ( #54195, #59206, #698, #32325 ) ) ;
#38769 = EDGE_CURVE ( 'NONE', #21122, #64911, #2545, .T. ) ;
#38770 = CARTESIAN_POINT ( 'NONE',  ( 92.95016907945944240, 22.74936990452175678, 6.323048487394066441 ) ) ;
#38771 = CARTESIAN_POINT ( 'NONE',  ( -15.32520546926282989, 7.495995523981874520, 64.95300774305263758 ) ) ;
#38772 = DIRECTION ( 'NONE',  ( 0.000000000000000000, 1.000000000000000000, -1.224646799147353207E-16 ) ) ;
#38773 = CARTESIAN_POINT ( 'NONE',  ( -80.35638419094748031, 24.05227397169793591, -88.98511473825129769 ) ) ;
#38774 = CARTESIAN_POINT ( 'NONE',  ( 39.40195752203892710, 8.409560354027398432, -23.77526687496409608 ) ) ;
#38775 = DIRECTION ( 'NONE',  ( 0.000000000000000000, 1.000000000000000000, 0.000000000000000000 ) ) ;
#38776 = FACE_BOUND ( 'NONE', #41591, .T. ) ;
#38777 = CARTESIAN_POINT ( 'NONE',  ( 6.933333333333328241, 8.000000000000000000, -11.86666666666666536 ) ) ;
#38778 = CIRCLE ( 'NONE', #66860, 65.00000000000000000 ) ;
#38779 = ORIENTED_EDGE ( 'NONE', *, *, #1411, .F. ) ;
#38780 = CARTESIAN_POINT ( 'NONE',  ( 133.8566784816069060, 42.60093787723655367, 17.66579024853170310 ) ) ;
#38781 = CARTESIAN_POINT ( 'NONE',  ( 91.50468583833760761, 22.21368636549395248, -49.04210192657487255 ) ) ;
#38782 = CONICAL_SURFACE ( 'NONE', #15225, 74.95140232871122521, 0.8777644062502172329 ) ;
#38783 = CARTESIAN_POINT ( 'NONE',  ( -47.65155309726505095, 13.85482731128118061, 63.42320367329789832 ) ) ;
#38784 = CARTESIAN_POINT ( 'NONE',  ( -180.5234362879039622, 97.35934147644941561, 12.72465163773038377 ) ) ;
#38785 = CARTESIAN_POINT ( 'NONE',  ( 211.3710169359754332, 117.8057917113659840, 60.11802606744021915 ) ) ;
#38786 = CARTESIAN_POINT ( 'NONE',  ( 86.62931800182293784, 19.42108912189599579, -62.66611478937537782 ) ) ;
#38787 = AXIS2_PLACEMENT_3D ( 'NONE', #53632, #59951, #33246 ) ;
#38788 = ORIENTED_EDGE ( 'NONE', *, *, #30254, .F. ) ;
#38789 = AXIS2_PLACEMENT_3D ( 'NONE', #13847, #29681, #56767 ) ;
#38790 = EDGE_CURVE ( 'NONE', #9869, #68905, #24000, .T. ) ;
#38791 = CARTESIAN_POINT ( 'NONE',  ( 61.09275639403234237, 12.23448398202909182, 3.202934752445754096 ) ) ;
#38792 = VECTOR ( 'NONE', #4200, 1000.000000000000000 ) ;
#38793 = CARTESIAN_POINT ( 'NONE',  ( -61.75956139478100226, 16.58288496614412111, 61.29573688743341364 ) ) ;
#38794 = ORIENTED_EDGE ( 'NONE', *, *, #5705, .F. ) ;
#38795 = ORIENTED_EDGE ( 'NONE', *, *, #48172, .T. ) ;
#38796 = VECTOR ( 'NONE', #22021, 1000.000000000000000 ) ;
#38797 = DIRECTION ( 'NONE',  ( 0.000000000000000000, 0.000000000000000000, -1.000000000000000000 ) ) ;
#38798 = CARTESIAN_POINT ( 'NONE',  ( 50.98853755884157835, 388.0000000000065370, -133.9497041420122798 ) ) ;
#38799 = CARTESIAN_POINT ( 'NONE',  ( 103.5588133492864813, 25.91050225236390858, 33.67192454186398010 ) ) ;
#38800 = ORIENTED_EDGE ( 'NONE', *, *, #10248, .F. ) ;
#38801 = ORIENTED_EDGE ( 'NONE', *, *, #3364, .F. ) ;
#38802 = CARTESIAN_POINT ( 'NONE',  ( 2.112947028648761272, 24.91054906769654664, 0.000000000000000000 ) ) ;
#38803 = CARTESIAN_POINT ( 'NONE',  ( 157.4703587214989113, 58.92748579479261650, 29.40946747225336466 ) ) ;
#38804 = CARTESIAN_POINT ( 'NONE',  ( 103.5849290181279088, 27.01613348792539071, 6.804909383962445268 ) ) ;
#38805 = CARTESIAN_POINT ( 'NONE',  ( 70.50376765786472788, 15.57629333413342998, 9.978129533752355229 ) ) ;
#38806 = CARTESIAN_POINT ( 'NONE',  ( 204.6977192012829789, 106.3443248447423315, 17.36317014830577321 ) ) ;
#38807 = CARTESIAN_POINT ( 'NONE',  ( 102.7414208686707582, 26.65627265923296818, -16.08848679405983262 ) ) ;
#38808 = CARTESIAN_POINT ( 'NONE',  ( -47.79955240516186876, 13.88975739862082470, 9.000507506480387221 ) ) ;
#38809 = CARTESIAN_POINT ( 'NONE',  ( -133.0835080491124813, 52.64966140620841628, -17.72071528858218059 ) ) ;
#38810 = FACE_OUTER_BOUND ( 'NONE', #46314, .T. ) ;
#38811 = CARTESIAN_POINT ( 'NONE',  ( 68.22258291815838049, 13.94003497920737011, -91.44893492023997794 ) ) ;
#38812 = CARTESIAN_POINT ( 'NONE',  ( 93.99232916046767627, 22.06612048408747384, 89.43417854994513050 ) ) ;
#38814 = ORIENTED_EDGE ( 'NONE', *, *, #21285, .F. ) ;
#38813 = LINE ( 'NONE', #38456, #1740 ) ;
#38815 = VERTEX_POINT ( 'NONE', #45446 ) ;
#38817 = VERTEX_POINT ( 'NONE', #39826 ) ;
#38816 = EDGE_CURVE ( 'NONE', #65087, #14549, #39477, .T. ) ;
#38818 = DIRECTION ( 'NONE',  ( 0.000000000000000000, 1.000000000000000000, -0.000000000000000000 ) ) ;
#38819 = CARTESIAN_POINT ( 'NONE',  ( 390.9212159716611836, 188.0000000000000000, 0.000000000000000000 ) ) ;
#38820 = CARTESIAN_POINT ( 'NONE',  ( -53.38256734720887664, 14.24001356352779979, -23.18744243301667751 ) ) ;
#38821 = CARTESIAN_POINT ( 'NONE',  ( 108.3906473026529653, 28.03385344351496400, -9.295257895322684760 ) ) ;
#38822 = EDGE_CURVE ( 'NONE', #24193, #6711, #24356, .T. ) ;
#38823 = CARTESIAN_POINT ( 'NONE',  ( -57.43883374585512769, 16.37892664338858850, -35.60189161719256390 ) ) ;
#38824 = ADVANCED_FACE ( 'NONE', ( #7826 ), #40516, .T. ) ;
#38825 = CARTESIAN_POINT ( 'NONE',  ( 204.6977192012829789, -170.0000000000000000, 63.55227132923313604 ) ) ;
#38826 = CARTESIAN_POINT ( 'NONE',  ( -71.21970990337018748, 19.62334883444993494, -70.48616352051527656 ) ) ;
#38827 = CARTESIAN_POINT ( 'NONE',  ( 23.23895241123074840, 6.853530908437178937, -17.16259189106778749 ) ) ;
#38828 = VERTEX_POINT ( 'NONE', #12753 ) ;
#38829 = AXIS2_PLACEMENT_3D ( 'NONE', #9486, #68233, #13718 ) ;
#38830 = ADVANCED_FACE ( 'NONE', ( #55654, #50032 ), #55302, .T. ) ;
#38831 = CARTESIAN_POINT ( 'NONE',  ( 74.62299871641508275, -5.461138973197948943, 43.58025477438756923 ) ) ;
#38832 = VERTEX_POINT ( 'NONE', #7122 ) ;
#38833 = EDGE_LOOP ( 'NONE', ( #47826, #18051, #19539, #26595, #50482, #14247, #2061, #13967, #46435 ) ) ;
#38834 = CARTESIAN_POINT ( 'NONE',  ( -142.1332311300252798, 59.44822332309657043, 9.980626331248242167 ) ) ;
#38835 = CIRCLE ( 'NONE', #21942, 5.000000000000000888 ) ;
#38836 = CARTESIAN_POINT ( 'NONE',  ( -57.76231208694425590, 16.46985661704315618, -89.40870754664922515 ) ) ;
#38837 = CARTESIAN_POINT ( 'NONE',  ( -24.01966911771076241, 9.505735805909457881, 92.54941079593402264 ) ) ;
#38838 = CARTESIAN_POINT ( 'NONE',  ( -95.05546640093035649, 29.25972325950978004, -44.59432911818360168 ) ) ;
#38839 = VECTOR ( 'NONE', #15163, 1000.000000000000000 ) ;
#38840 = CARTESIAN_POINT ( 'NONE',  ( -106.6781182590523542, 35.07133425426477658, 17.26811540876042983 ) ) ;
#38841 = CYLINDRICAL_SURFACE ( 'NONE', #15752, 63.00000000000000000 ) ;
#38842 = CARTESIAN_POINT ( 'NONE',  ( 136.1215428813736708, 43.99260314811118633, -23.84356242264301784 ) ) ;
#38843 = ORIENTED_EDGE ( 'NONE', *, *, #48079, .F. ) ;
#38844 = EDGE_LOOP ( 'NONE', ( #36239, #68645, #51551, #57807 ) ) ;
#38845 = VECTOR ( 'NONE', #36389, 1000.000000000000114 ) ;
#38846 = ORIENTED_EDGE ( 'NONE', *, *, #30279, .F. ) ;
#38847 = SHAPE_REPRESENTATION ( 'stator', ( #66832 ), #19703 ) ;
#38848 = DIRECTION ( 'NONE',  ( -1.000000000000000000, 3.552713678800500929E-15, 0.000000000000000000 ) ) ;
#38849 = AXIS2_PLACEMENT_3D ( 'NONE', #49697, #65923, #27911 ) ;
#38850 = CARTESIAN_POINT ( 'NONE',  ( -13.47230132170245120, 7.324574289401432736, 15.73105565795967031 ) ) ;
#38851 = CARTESIAN_POINT ( 'NONE',  ( 32.28603806442398394, 7.590310383548725781, -72.38435536236562484 ) ) ;
#38852 = CARTESIAN_POINT ( 'NONE',  ( 60.40277045393653310, 12.08176563382369828, -9.341763661136180730 ) ) ;
#38853 = EDGE_CURVE ( 'NONE', #9471, #36296, #66581, .T. ) ;
#38854 = EDGE_CURVE ( 'NONE', #22781, #9333, #47696, .T. ) ;
#38855 = UNCERTAINTY_MEASURE_WITH_UNIT (LENGTH_MEASURE( 1.000000000000000082E-05 ), #27409, 'distance_accuracy_value', 'NONE');
#38856 = LINE ( 'NONE', #7183, #31524 ) ;
#38857 = DIRECTION ( 'NONE',  ( 0.000000000000000000, 0.000000000000000000, -1.000000000000000000 ) ) ;
#38858 = VERTEX_POINT ( 'NONE', #61630 ) ;
#38859 = CARTESIAN_POINT ( 'NONE',  ( 188.2950976467627697, 87.71503060978560029, 65.73591284412599123 ) ) ;
#38860 = CARTESIAN_POINT ( 'NONE',  ( -154.7934364910360330, 68.79594655117534785, 70.39161810400815966 ) ) ;
#38861 = CARTESIAN_POINT ( 'NONE',  ( -1.866625526081663322, 7.583073082893621475, -38.33698315850279670 ) ) ;
#38862 = CARTESIAN_POINT ( 'NONE',  ( 102.8518012651273494, 25.61025413220826863, 11.56502006215868050 ) ) ;
#38863 = CARTESIAN_POINT ( 'NONE',  ( -170.4515722736647092, 84.20506723175657271, -88.88108375465611743 ) ) ;
#38864 = CARTESIAN_POINT ( 'NONE',  ( -79.62258606008209938, 22.68765733708495347, -50.06947209741141336 ) ) ;
#38865 = FACE_BOUND ( 'NONE', #48005, .T. ) ;
#38866 = DIRECTION ( 'NONE',  ( 0.000000000000000000, 0.000000000000000000, 1.000000000000000000 ) ) ;
#38867 = ORIENTED_EDGE ( 'NONE', *, *, #56052, .T. ) ;
#38868 = DIRECTION ( 'NONE',  ( -0.000000000000000000, -1.000000000000000000, -0.000000000000000000 ) ) ;
#38869 = CARTESIAN_POINT ( 'NONE',  ( 181.0840389613909736, 78.60582251573003987, 29.30859410551139277 ) ) ;
#38870 = CYLINDRICAL_SURFACE ( 'NONE', #41044, 5.000000000000018652 ) ;
#38871 = CARTESIAN_POINT ( 'NONE',  ( -8.712114576423529044, -23.56346432108879441, 3.061616997868437868E-16 ) ) ;
#38872 = CARTESIAN_POINT ( 'NONE',  ( 60.61895554631706062, 13.15982272268127851, -62.94199435588256364 ) ) ;
#38873 = ORIENTED_EDGE ( 'NONE', *, *, #26299, .T. ) ;
#38874 = PRODUCT_DEFINITION_SHAPE ( 'NONE', 'NONE',  #69622 ) ;
#38875 = ORIENTED_EDGE ( 'NONE', *, *, #40667, .F. ) ;
#38876 = CARTESIAN_POINT ( 'NONE',  ( -36.11269837220806522, 0.000000000000000000, 2.000000000000000000 ) ) ;
#38877 = CARTESIAN_POINT ( 'NONE',  ( 183.1997226035582003, 80.77024518673746911, 83.29662567210579027 ) ) ;
#38878 = ORIENTED_EDGE ( 'NONE', *, *, #4241, .F. ) ;
#38879 = VECTOR ( 'NONE', #41165, 1000.000000000000000 ) ;
#38880 = ORIENTED_EDGE ( 'NONE', *, *, #49509, .F. ) ;
#38881 = DIRECTION ( 'NONE',  ( -1.000000000000000000, 0.000000000000000000, 0.000000000000000000 ) ) ;
#38882 = CARTESIAN_POINT ( 'NONE',  ( -15.55634918610403439, 5.000000000000028422, 0.000000000000000000 ) ) ;
#38883 = ORIENTED_EDGE ( 'NONE', *, *, #45649, .F. ) ;
#38884 = PLANE ( 'NONE',  #5366 ) ;
#38885 = CARTESIAN_POINT ( 'NONE',  ( 56.42997683260148278, -32.25922681454192542, 170.0000000000000000 ) ) ;
#38886 = CARTESIAN_POINT ( 'NONE',  ( -74.79002408692173276, 20.88280597089421420, -36.19028926828421078 ) ) ;
#38887 = DIRECTION ( 'NONE',  ( 0.8345732537213079727, -0.5508969814520945363, 2.500042656554809847E-16 ) ) ;
#38888 = AXIS2_PLACEMENT_3D ( 'NONE', #16785, #59351, #42818 ) ;
#38890 = CARTESIAN_POINT ( 'NONE',  ( -29.51272929882557250, 10.30144624948894361, -8.720126078648599233 ) ) ;
#38889 = VECTOR ( 'NONE', #57654, 999.9999999999998863 ) ;
#38891 = CARTESIAN_POINT ( 'NONE',  ( -50.14440374537738876, 14.45628984983895471, -10.17979503501909022 ) ) ;
#38892 = PRODUCT_DEFINITION_FORMATION_WITH_SPECIFIED_SOURCE ( 'ANY', '', #43365, .NOT_KNOWN. ) ;
#38893 = ORIENTED_EDGE ( 'NONE', *, *, #62660, .F. ) ;
#38894 = CARTESIAN_POINT ( 'NONE',  ( 111.8699272271189216, 29.64190505307780299, -50.74762732561652712 ) ) ;
#38895 = AXIS2_PLACEMENT_3D ( 'NONE', #60106, #44636, #66120 ) ;
#38896 = CARTESIAN_POINT ( 'NONE',  ( 111.9975424824652634, 20.00000000000003197, 401.6295345748407613 ) ) ;
#38897 = CARTESIAN_POINT ( 'NONE',  ( 41.09671232177015554, 8.635892912882335182, -50.42995035429531470 ) ) ;
#38898 = CARTESIAN_POINT ( 'NONE',  ( 412.3372781065087906, 400.0000000000065938, -111.4497041420121093 ) ) ;
#38900 = VERTEX_POINT ( 'NONE', #56346 ) ;
#38899 = CARTESIAN_POINT ( 'NONE',  ( -120.2252778751027478, 42.87312880338508592, 86.88807202166155719 ) ) ;
#38901 = CARTESIAN_POINT ( 'NONE',  ( 8.000000000000007105, 249.8719672152120381, -95.00000000000133582 ) ) ;
#38902 = EDGE_CURVE ( 'NONE', #61262, #51470, #42972, .T. ) ;
#38903 = ORIENTED_EDGE ( 'NONE', *, *, #36532, .T. ) ;
#38904 = CARTESIAN_POINT ( 'NONE',  ( -129.4098618459772467, 48.85263848239745244, 31.49111774146622622 ) ) ;
#38905 = FACE_OUTER_BOUND ( 'NONE', #61943, .T. ) ;
#38906 = DIRECTION ( 'NONE',  ( -2.126200446592111359E-16, 0.6427876096865404731, -0.7660444431189771253 ) ) ;
#38907 = CARTESIAN_POINT ( 'NONE',  ( 93.72687053612523300, 23.04134601640627622, 34.73706976770577626 ) ) ;
#38908 = EDGE_CURVE ( 'NONE', #48854, #65404, #8165, .T. ) ;
#38909 = CARTESIAN_POINT ( 'NONE',  ( -120.1497954511983295, 42.82624472369556656, 60.11543276227916266 ) ) ;
#38910 = DIRECTION ( 'NONE',  ( -1.000000000000000000, 0.000000000000000000, 0.000000000000000000 ) ) ;
#38911 = CARTESIAN_POINT ( 'NONE',  ( 93.92280655489130936, 22.03989931749464404, -71.93211272359918951 ) ) ;
#38912 = ADVANCED_FACE ( 'NONE', ( #13784 ), #29970, .F. ) ;
#38913 = CARTESIAN_POINT ( 'NONE',  ( -19.56458807131831890, -15.75959024859417390, 3.061616997868437868E-16 ) ) ;
#38914 = DIRECTION ( 'NONE',  ( -0.000000000000000000, -0.000000000000000000, -1.000000000000000000 ) ) ;
#38915 = VERTEX_POINT ( 'NONE', #51432 ) ;
#38916 = VERTEX_POINT ( 'NONE', #24701 ) ;
#38917 = ADVANCED_FACE ( 'NONE', ( #45095 ), #8867, .F. ) ;
#38918 = CARTESIAN_POINT ( 'NONE',  ( 46.13320811200730276, 9.380653113584042302, 34.06983411699128794 ) ) ;
#38919 = CARTESIAN_POINT ( 'NONE',  ( 200.4600337307565781, 100.7087439352120981, -10.77597343189907342 ) ) ;
#38920 = DIRECTION ( 'NONE',  ( -0.000000000000000000, -0.000000000000000000, -1.000000000000000000 ) ) ;
#38921 = CARTESIAN_POINT ( 'NONE',  ( -190.3074740493607351, 108.5764897054613414, 61.38473446933937794 ) ) ;
#38922 = CARTESIAN_POINT ( 'NONE',  ( 211.1046732743773191, 117.3965485104337461, -39.91724935795743789 ) ) ;
#38923 = CARTESIAN_POINT ( 'NONE',  ( -71.42007367207963853, 20.75704712149297393, -71.45956786119569415 ) ) ;
#38924 = CARTESIAN_POINT ( 'NONE',  ( 39.54205320694412507, -51.58901073076707888, 170.0000000000000000 ) ) ;
#38925 = CARTESIAN_POINT ( 'NONE',  ( -25.48237668717800375, 8.689083390666773710, -38.23367346561963132 ) ) ;
#38926 = CARTESIAN_POINT ( 'NONE',  ( 163.1265310614426767, 62.18610413911356716, -75.40005345542890325 ) ) ;
#38927 = PRODUCT_DEFINITION_SHAPE ( 'NONE', 'NONE',  #69598 ) ;
#38928 = ORIENTED_EDGE ( 'NONE', *, *, #39192, .T. ) ;
#38929 = CARTESIAN_POINT ( 'NONE',  ( -28.13128612339709633, 10.08889185338652084, 17.62085998369287054 ) ) ;
#38930 = ORIENTED_EDGE ( 'NONE', *, *, #59049, .T. ) ;
#38931 = VECTOR ( 'NONE', #9414, 1000.000000000000000 ) ;
#38932 = CARTESIAN_POINT ( 'NONE',  ( 16.78635691501517613, 0.000000000000000000, -9.435653166495500344 ) ) ;
#38933 = CARTESIAN_POINT ( 'NONE',  ( -82.77834200299112410, 23.92990355093956012, 85.30423727294719072 ) ) ;
#38934 = CARTESIAN_POINT ( 'NONE',  ( -85.75222301046098039, 25.14826148333819233, 67.27150280759872203 ) ) ;
#38935 = EDGE_CURVE ( 'NONE', #56347, #58835, #8314, .T. ) ;
#38936 = CARTESIAN_POINT ( 'NONE',  ( 126.4633682455861816, 38.28837286275646790, 38.29824169173695481 ) ) ;
#38937 = LINE ( 'NONE', #28014, #44498 ) ;
#38938 = VECTOR ( 'NONE', #13581, 1000.000000000000000 ) ;
#38939 = CARTESIAN_POINT ( 'NONE',  ( 0.000000000000000000, 0.000000000000000000, 0.000000000000000000 ) ) ;
#38940 = CARTESIAN_POINT ( 'NONE',  ( -100.4440683050664802, 32.98184228837414622, -8.383530731465961949 ) ) ;
#38941 = AXIS2_PLACEMENT_3D ( 'NONE', #49398, #7202, #28662 ) ;
#38942 = DIRECTION ( 'NONE',  ( 0.000000000000000000, 0.000000000000000000, 1.000000000000000000 ) ) ;
#38943 = CARTESIAN_POINT ( 'NONE',  ( 211.8283568324397095, 116.6646490157212810, 92.73083172464008328 ) ) ;
#38944 = DIRECTION ( 'NONE',  ( 0.000000000000000000, -0.09748146057682104126, -0.9952373409613456401 ) ) ;
#38945 = VERTEX_POINT ( 'NONE', #15523 ) ;
#38946 = CARTESIAN_POINT ( 'NONE',  ( -128.7650348665116837, 48.41336321950710442, 71.89692748193580485 ) ) ;
#38947 = CARTESIAN_POINT ( 'NONE',  ( 0.000000000000000000, 200.0000000000000000, 0.000000000000000000 ) ) ;
#38948 = CARTESIAN_POINT ( 'NONE',  ( 11.20486344102687681, 7.403248964808831545, -63.90658810494937114 ) ) ;
#38949 = CARTESIAN_POINT ( 'NONE',  ( -9.779603649692305112, 8.034615131607072414, 18.02880719371939833 ) ) ;
#38950 = CARTESIAN_POINT ( 'NONE',  ( 282.5087422071486571, -21.56900326173647997, -4.337278505387078376 ) ) ;
#38951 = CARTESIAN_POINT ( 'NONE',  ( 6.400000000000000355, -4.618802153517016507, -8.000000000000000000 ) ) ;
#38952 = CARTESIAN_POINT ( 'NONE',  ( -94.87734348028330089, 29.17663635873013561, -95.00000000000133582 ) ) ;
#38953 = CONICAL_SURFACE ( 'NONE', #56925, 8.000000000000001776, 1.047197551196595855 ) ;
#38954 = ORIENTED_EDGE ( 'NONE', *, *, #54703, .T. ) ;
#38955 = DIRECTION ( 'NONE',  ( 0.9467895904119979500, 0.3218531831246678743, -7.920897705323217815E-15 ) ) ;
#38956 = CARTESIAN_POINT ( 'NONE',  ( 109.9975424824652777, 296.0000000000000000, 418.0000000000000000 ) ) ;
#38957 = CARTESIAN_POINT ( 'NONE',  ( -133.1527834403230202, 51.46311219732125153, 13.18024344451227492 ) ) ;
#38958 = CARTESIAN_POINT ( 'NONE',  ( -165.6215009671260532, 80.58889799860440917, -41.89784876661412483 ) ) ;
#38959 = LINE ( 'NONE', #12566, #40034 ) ;
#38960 = ORIENTED_EDGE ( 'NONE', *, *, #13682, .F. ) ;
#38961 = CARTESIAN_POINT ( 'NONE',  ( 125.0000000000000000, 1.530808498934191561E-14, -10.00000000000000000 ) ) ;
#38962 = CARTESIAN_POINT ( 'NONE',  ( 56.42997683260104225, 32.25922681454270702, 170.0000000000000000 ) ) ;
#38963 = CARTESIAN_POINT ( 'NONE',  ( -144.9439644317224349, 60.40328483334189258, -21.42479971859992460 ) ) ;
#38964 = CARTESIAN_POINT ( 'NONE',  ( -142.1403563221901436, 58.17414631827835336, 93.35838044322102292 ) ) ;
#38965 = DIRECTION ( 'NONE',  ( -1.000000000000000000, 0.000000000000000000, 0.000000000000000000 ) ) ;
#38966 = ORIENTED_EDGE ( 'NONE', *, *, #12159, .T. ) ;
#38967 = CARTESIAN_POINT ( 'NONE',  ( -59.95412189755934662, 17.09836075175410386, 5.275069537795150865 ) ) ;
#38968 = CARTESIAN_POINT ( 'NONE',  ( 200.4559562755961792, 100.7034888016685841, -50.02848380335337453 ) ) ;
#38969 = DIRECTION ( 'NONE',  ( 0.000000000000000000, 0.000000000000000000, -1.000000000000000000 ) ) ;
#38970 = CARTESIAN_POINT ( 'NONE',  ( 157.4703587214989113, 58.92748579479261650, 29.40946747225336466 ) ) ;
#38972 = ORIENTED_EDGE ( 'NONE', *, *, #64380, .F. ) ;
#38971 = CARTESIAN_POINT ( 'NONE',  ( -57.43251939610648549, 15.33203492375495891, 3.843832803641082041 ) ) ;
#38973 = ADVANCED_FACE ( 'NONE', ( #30661, #14137, #26419 ), #58411, .T. ) ;
#38974 = CARTESIAN_POINT ( 'NONE',  ( 0.000000000000000000, 0.000000000000000000, 0.000000000000000000 ) ) ;
#38975 = ORIENTED_EDGE ( 'NONE', *, *, #64965, .T. ) ;
#38976 = VERTEX_POINT ( 'NONE', #57053 ) ;
#38977 = VECTOR ( 'NONE', #67241, 1000.000000000000000 ) ;
#38978 = CARTESIAN_POINT ( 'NONE',  ( -121.0374639672267989, 43.37850281258126728, -90.38315847734473607 ) ) ;
#38979 = LINE ( 'NONE', #5897, #32713 ) ;
#38980 = VECTOR ( 'NONE', #6928, 1000.000000000000114 ) ;
#38982 = EDGE_LOOP ( 'NONE', ( #11830, #15151, #67102, #68483 ) ) ;
#38981 = CARTESIAN_POINT ( 'NONE',  ( -15.27733754929849752, 8.502213909106947298, -68.78387266333825778 ) ) ;
#38983 = DIRECTION ( 'NONE',  ( -0.000000000000000000, -0.000000000000000000, -1.000000000000000000 ) ) ;
#38984 = PLANE ( 'NONE',  #49823 ) ;
#38985 = LINE ( 'NONE', #44237, #60871 ) ;
#38986 = AXIS2_PLACEMENT_3D ( 'NONE', #68038, #62402, #36014 ) ;
#38987 = ORIENTED_EDGE ( 'NONE', *, *, #23377, .T. ) ;
#38988 = VECTOR ( 'NONE', #30973, 1000.000000000000000 ) ;
#38989 = CARTESIAN_POINT ( 'NONE',  ( 65.13282190615461786, 1.839221433318906476E-12, -5.000000000000000000 ) ) ;
#38990 = ADVANCED_FACE ( 'NONE', ( #41217 ), #25047, .F. ) ;
#38991 = AXIS2_PLACEMENT_3D ( 'NONE', #57163, #4040, #46947 ) ;
#38992 = CARTESIAN_POINT ( 'NONE',  ( -37.92511097250854846, 10.74631978746600680, -12.19873838909606256 ) ) ;
#38993 = CARTESIAN_POINT ( 'NONE',  ( 32.06997139192709056, 56.95813133885486934, 41.38025477438755928 ) ) ;
#38994 = CARTESIAN_POINT ( 'NONE',  ( -128.1282195935087316, 49.19720162550163423, 4.112327430167169062 ) ) ;
#38995 = DIRECTION ( 'NONE',  ( 0.5111246509603011301, 0.000000000000000000, 0.8595065975201763298 ) ) ;
#38996 = ORIENTED_EDGE ( 'NONE', *, *, #7402, .T. ) ;
#38997 = ORIENTED_EDGE ( 'NONE', *, *, #41939, .T. ) ;
#38998 = ORIENTED_EDGE ( 'NONE', *, *, #15515, .F. ) ;
#38999 = EDGE_CURVE ( 'NONE', #60543, #11940, #26762, .T. ) ;
#39000 = CARTESIAN_POINT ( 'NONE',  ( -4.250000000000000000, 5.204748896376250699E-16, -0.5251556536572842271 ) ) ;
#39001 = CARTESIAN_POINT ( 'NONE',  ( 311.9975424824652350, 170.0000000000000284, 354.1673509436691347 ) ) ;
#39002 = FACE_OUTER_BOUND ( 'NONE', #58351, .T. ) ;
#39003 = CARTESIAN_POINT ( 'NONE',  ( -33.83558513595455963, 9.996963989836508802, -35.70617816557648894 ) ) ;
#39004 = CARTESIAN_POINT ( 'NONE',  ( -102.9107985116279451, 33.10231825923204241, 84.22887737053727619 ) ) ;
#39005 = CARTESIAN_POINT ( 'NONE',  ( -143.8794621588508278, 59.54894433207190474, 33.25729526067438968 ) ) ;
#39006 = CARTESIAN_POINT ( 'NONE',  ( -132.4951995226845156, 50.99687809989501375, 61.39550820969922285 ) ) ;
#39007 = CARTESIAN_POINT ( 'NONE',  ( -72.77296415263757012, 21.23032531836539150, -20.43596273929950513 ) ) ;
#39008 = ORIENTED_EDGE ( 'NONE', *, *, #8036, .F. ) ;
#39009 = CARTESIAN_POINT ( 'NONE',  ( 0.000000000000000000, 35.26862320190615208, -9.999999999999998224 ) ) ;
#39010 = ORIENTED_EDGE ( 'NONE', *, *, #54069, .T. ) ;
#39011 = CARTESIAN_POINT ( 'NONE',  ( 37.46254810722764717, 8.164772623042713562, 30.15249803224812197 ) ) ;
#39012 = CARTESIAN_POINT ( 'NONE',  ( 51.39999999999999858, 0.000000000000000000, 0.000000000000000000 ) ) ;
#39013 = CARTESIAN_POINT ( 'NONE',  ( 49.42891955109325153, 30.98851943060457614, 27.58472369397437163 ) ) ;
#39014 = EDGE_CURVE ( 'NONE', #44762, #65087, #20023, .T. ) ;
#39015 = DIRECTION ( 'NONE',  ( 0.000000000000000000, 1.000000000000000000, -0.000000000000000000 ) ) ;
#39016 = DIRECTION ( 'NONE',  ( -1.020422603260505347E-14, 1.000000000000000000, 5.551115123125782702E-17 ) ) ;
#39017 = CARTESIAN_POINT ( 'NONE',  ( -120.1346137380982242, 44.00127440773566434, 60.15369630792869771 ) ) ;
#39018 = CARTESIAN_POINT ( 'NONE',  ( -52.68007207639879397, 14.05813534436551215, 3.853851446599284358 ) ) ;
#39019 = EDGE_CURVE ( 'NONE', #38482, #32583, #60148, .T. ) ;
#39020 = CARTESIAN_POINT ( 'NONE',  ( 150.2794558856211040, 52.26944788078748161, -41.42442129602201106 ) ) ;
#39021 = EDGE_CURVE ( 'NONE', #54785, #27416, #2533, .T. ) ;
#39022 = LINE ( 'NONE', #50262, #64795 ) ;
#39023 = ORIENTED_EDGE ( 'NONE', *, *, #5625, .F. ) ;
#39024 = CARTESIAN_POINT ( 'NONE',  ( -109.5949300668648476, 36.65467447298198067, -94.53065599267198138 ) ) ;
#39025 = FACE_OUTER_BOUND ( 'NONE', #52803, .T. ) ;
#39026 = EDGE_LOOP ( 'NONE', ( #12048, #14249, #64102, #39850 ) ) ;
#39027 = CARTESIAN_POINT ( 'NONE',  ( -3.816391647148975608E-14, -9.237604307034022355, -8.785468820183664818 ) ) ;
#39028 = CARTESIAN_POINT ( 'NONE',  ( -24.51966494718099909, -5.470267094204724678, 0.000000000000000000 ) ) ;
#39029 = ORIENTED_EDGE ( 'NONE', *, *, #24217, .T. ) ;
#39030 = CARTESIAN_POINT ( 'NONE',  ( -85.75947274862033964, 25.15128705015479227, 35.42982735500162050 ) ) ;
#39031 = CARTESIAN_POINT ( 'NONE',  ( 19.71799482800335923, -15.56722426018171035, 3.061616997868437868E-16 ) ) ;
#39032 = CARTESIAN_POINT ( 'NONE',  ( 41.33434189587760699, 9.684413566891869607, 44.66476443964724297 ) ) ;
#39033 = AXIS2_PLACEMENT_3D ( 'NONE', #42219, #38942, #49817 ) ;
#39034 = ORIENTED_EDGE ( 'NONE', *, *, #356, .T. ) ;
#39035 = ORIENTED_EDGE ( 'NONE', *, *, #38644, .F. ) ;
#39036 = DIRECTION ( 'NONE',  ( -1.000000000000000000, 0.000000000000000000, 0.000000000000000000 ) ) ;
#39037 = AXIS2_PLACEMENT_3D ( 'NONE', #6529, #65986, #37839 ) ;
#39038 = VERTEX_POINT ( 'NONE', #11259 ) ;
#39039 = DIRECTION ( 'NONE',  ( -0.000000000000000000, 1.000000000000000000, -0.000000000000000000 ) ) ;
#39040 = FACE_OUTER_BOUND ( 'NONE', #23860, .T. ) ;
#39041 = CARTESIAN_POINT ( 'NONE',  ( -1.866625526081660880, 7.583073082893622363, 15.35211802242455725 ) ) ;
#39042 = CARTESIAN_POINT ( 'NONE',  ( 138.8350590320874574, 45.70671380708321863, 85.08020996455034890 ) ) ;
#39043 = VECTOR ( 'NONE', #56282, 999.9999999999998863 ) ;
#39044 = PLANE ( 'NONE',  #44808 ) ;
#39045 = DIRECTION ( 'NONE',  ( 1.000000000000000000, 0.000000000000000000, 0.000000000000000000 ) ) ;
#39046 = AXIS2_PLACEMENT_3D ( 'NONE', #48723, #54000, #915 ) ;
#39047 = ORIENTED_EDGE ( 'NONE', *, *, #58052, .F. ) ;
#39048 = FACE_OUTER_BOUND ( 'NONE', #41047, .T. ) ;
#39049 = ORIENTED_EDGE ( 'NONE', *, *, #4701, .T. ) ;
#39050 = VERTEX_POINT ( 'NONE', #6691 ) ;
#39051 = CARTESIAN_POINT ( 'NONE',  ( 161.7209903610255424, 61.03262545641851489, -10.58304253588356936 ) ) ;
#39052 = DIRECTION ( 'NONE',  ( -1.000000000000000000, 0.000000000000000000, -0.000000000000000000 ) ) ;
#39053 = FACE_OUTER_BOUND ( 'NONE', #64205, .T. ) ;
#39054 = CARTESIAN_POINT ( 'NONE',  ( 138.5684226926155702, 45.53585076428270639, 16.02087130590416564 ) ) ;
#39055 = DIRECTION ( 'NONE',  ( 0.000000000000000000, 0.000000000000000000, 1.000000000000000000 ) ) ;
#39056 = ORIENTED_EDGE ( 'NONE', *, *, #61247, .F. ) ;
#39057 = EDGE_CURVE ( 'NONE', #57934, #21309, #28137, .T. ) ;
#39058 = ORIENTED_EDGE ( 'NONE', *, *, #16264, .T. ) ;
#39059 = DIRECTION ( 'NONE',  ( -1.240128853613758897E-16, 0.000000000000000000, 1.000000000000000000 ) ) ;
#39060 = ORIENTED_EDGE ( 'NONE', *, *, #34578, .F. ) ;
#39061 = EDGE_CURVE ( 'NONE', #22304, #32549, #16198, .T. ) ;
#39062 = LINE ( 'NONE', #52377, #67933 ) ;
#39063 = ORIENTED_EDGE ( 'NONE', *, *, #4704, .T. ) ;
#39064 = CARTESIAN_POINT ( 'NONE',  ( -147.7860806339124906, 62.73248524776228408, -76.47009865734850109 ) ) ;
#39065 = CARTESIAN_POINT ( 'NONE',  ( 88.28780346671261725, 19.99350429399657969, 3.049271561570116251 ) ) ;
#39066 = CARTESIAN_POINT ( 'NONE',  ( -9.964117946889912147, 64.24592483216710548, 170.0000000000000000 ) ) ;
#39067 = ORIENTED_EDGE ( 'NONE', *, *, #26906, .T. ) ;
#39068 = VECTOR ( 'NONE', #18811, 1000.000000000000000 ) ;
#39069 = FACE_OUTER_BOUND ( 'NONE', #52973, .T. ) ;
#39070 = EDGE_CURVE ( 'NONE', #26725, #9754, #52758, .T. ) ;
#39071 = ADVANCED_FACE ( 'NONE', ( #55219 ), #2809, .F. ) ;
#39072 = CARTESIAN_POINT ( 'NONE',  ( 70.10996765587415780, 15.47155867340926960, 88.54573586507250127 ) ) ;
#39073 = VECTOR ( 'NONE', #44994, 1000.000000000000000 ) ;
#39074 = CARTESIAN_POINT ( 'NONE',  ( 36.30999198706540199, 9.040534725358950752, 44.25116645233489265 ) ) ;
#39075 = CARTESIAN_POINT ( 'NONE',  ( -180.0154536325056540, 96.73346874014738717, -39.24493656227331684 ) ) ;
#39076 = CARTESIAN_POINT ( 'NONE',  ( -132.4819073909166320, 50.98736898418876251, -11.94662083526208285 ) ) ;
#39077 = DIRECTION ( 'NONE',  ( -1.000000000000000000, 0.000000000000000000, -0.000000000000000000 ) ) ;
#39078 =( REPRESENTATION_RELATIONSHIP ('NONE','NONE', #40274, #50551 ) REPRESENTATION_RELATIONSHIP_WITH_TRANSFORMATION ( #21374 )SHAPE_REPRESENTATION_RELATIONSHIP( ) );
#39079 = FACE_OUTER_BOUND ( 'NONE', #44402, .T. ) ;
#39081 = ORIENTED_EDGE ( 'NONE', *, *, #69057, .F. ) ;
#39080 = ADVANCED_FACE ( 'NONE', ( #50998 ), #55570, .F. ) ;
#39082 = FACE_OUTER_BOUND ( 'NONE', #16114, .T. ) ;
#39083 = VECTOR ( 'NONE', #7565, 1000.000000000000114 ) ;
#39084 = DIRECTION ( 'NONE',  ( -1.000000000000000000, 0.000000000000000000, 0.000000000000000000 ) ) ;
#39085 = ORIENTED_EDGE ( 'NONE', *, *, #38439, .F. ) ;
#39086 = EDGE_CURVE ( 'NONE', #55507, #68666, #61202, .T. ) ;
#39087 = CARTESIAN_POINT ( 'NONE',  ( 444.9999999999999432, 225.0000000000000000, 380.0000000000000000 ) ) ;
#39088 = AXIS2_PLACEMENT_3D ( 'NONE', #56360, #61299, #13796 ) ;
#39089 = CARTESIAN_POINT ( 'NONE',  ( -5.401648928593175469, 6.744888135494086612, -62.64828587876987598 ) ) ;
#39090 = CARTESIAN_POINT ( 'NONE',  ( -34.06637338149494099, 11.05895377318623218, 30.68749078464274760 ) ) ;
#39091 = CARTESIAN_POINT ( 'NONE',  ( 14.11945145860287809, 7.458327016560931000, -89.34736952536303534 ) ) ;
#39092 = DIRECTION ( 'NONE',  ( 0.000000000000000000, 0.000000000000000000, 1.000000000000000000 ) ) ;
#39093 = DIRECTION ( 'NONE',  ( -2.509494923690479143E-16, -1.000000000000000000, -1.496132621402170665E-16 ) ) ;
#39094 = CARTESIAN_POINT ( 'NONE',  ( 10.73115448446713494, 22.57968829347503714, 0.000000000000000000 ) ) ;
#39095 = CARTESIAN_POINT ( 'NONE',  ( 114.8388692023054318, 21.96385131419673442, -1.300671796277839354 ) ) ;
#39096 = DIRECTION ( 'NONE',  ( 1.000000000000000000, 0.000000000000000000, -0.000000000000000000 ) ) ;
#39097 = CARTESIAN_POINT ( 'NONE',  ( 25.09133896793782981, -1.250000000000021982, 0.000000000000000000 ) ) ;
#39098 = CARTESIAN_POINT ( 'NONE',  ( 164.9709596662455908, 63.72607097915132357, 10.32857681705704067 ) ) ;
#39099 = CARTESIAN_POINT ( 'NONE',  ( -49.66729301550846998, 14.33905798229759121, -91.16771365468441957 ) ) ;
#39100 = ORIENTED_EDGE ( 'NONE', *, *, #57409, .T. ) ;
#39101 = VECTOR ( 'NONE', #62876, 1000.000000000000000 ) ;
#39102 = CYLINDRICAL_SURFACE ( 'NONE', #357, 5.000000000000018652 ) ;
#39103 = VERTEX_POINT ( 'NONE', #34829 ) ;
#39104 = CARTESIAN_POINT ( 'NONE',  ( -444.3843108123961656, 394.6949978562683441, 95.33065306861280419 ) ) ;
#39105 = ADVANCED_FACE ( 'NONE', ( #13027 ), #7396, .F. ) ;
#39106 = CARTESIAN_POINT ( 'NONE',  ( 83.59652366361575559, 19.46709838196858655, -63.30246192554085383 ) ) ;
#39107 = CARTESIAN_POINT ( 'NONE',  ( 115.2886225100560438, 32.40839894504812690, 85.24140403135865540 ) ) ;
#39108 = CARTESIAN_POINT ( 'NONE',  ( 230.9999999999999432, 0.000000000000000000, 72.99999999999998579 ) ) ;
#39109 = CARTESIAN_POINT ( 'NONE',  ( -14.35185884954381308, 7.404296649871966451, 94.99999999999866418 ) ) ;
#39110 = EDGE_CURVE ( 'NONE', #56653, #31511, #45367, .T. ) ;
#39111 = EDGE_CURVE ( 'NONE', #31650, #67324, #35956, .T. ) ;
#39112 = ADVANCED_FACE ( 'NONE', ( #64248 ), #53329, .T. ) ;
#39113 = CARTESIAN_POINT ( 'NONE',  ( -2.699999999999990408, 0.000000000000000000, 0.000000000000000000 ) ) ;
#39114 = DIRECTION ( 'NONE',  ( 1.000000000000000000, 0.000000000000000000, -0.000000000000000000 ) ) ;
#39115 = CARTESIAN_POINT ( 'NONE',  ( -118.8392474096542344, 43.20060570451234838, -18.16838627151736674 ) ) ;
#39116 = ORIENTED_EDGE ( 'NONE', *, *, #57723, .T. ) ;
#39117 = ORIENTED_EDGE ( 'NONE', *, *, #56296, .T. ) ;
#39118 = CARTESIAN_POINT ( 'NONE',  ( 35.65622260226242446, 8.964590916200315007, 70.76066538983499754 ) ) ;
#39119 = LINE ( 'NONE', #33494, #43373 ) ;
#39120 = CARTESIAN_POINT ( 'NONE',  ( -1.734723475976807094E-15, 9.237604307034022355, -8.785468820183664818 ) ) ;
#39121 = CARTESIAN_POINT ( 'NONE',  ( 64.38365952014046911, -38.46744580544211800, 43.58025477438756212 ) ) ;
#39122 = CARTESIAN_POINT ( 'NONE',  ( -20.00000000000002842, 3.680555555555560243, 4.000000000000000000 ) ) ;
#39123 = LINE ( 'NONE', #779, #7220 ) ;
#39124 = ORIENTED_EDGE ( 'NONE', *, *, #21271, .T. ) ;
#39125 = CARTESIAN_POINT ( 'NONE',  ( 94.02861641584117081, 23.15570573563316259, 9.116654949391469032 ) ) ;
#39126 = CARTESIAN_POINT ( 'NONE',  ( 149.6041652118227603, -64.71860240360767591, 1.657799476683943007 ) ) ;
#39127 = CARTESIAN_POINT ( 'NONE',  ( 31.11269837220800127, -31.11269837220812562, 0.000000000000000000 ) ) ;
#39128 = FACE_OUTER_BOUND ( 'NONE', #2464, .T. ) ;
#39129 = CARTESIAN_POINT ( 'NONE',  ( 211.5066273949819617, 116.1727691518061789, -20.17497244266030165 ) ) ;
#39130 = FACE_BOUND ( 'NONE', #3761, .T. ) ;
#39131 = CARTESIAN_POINT ( 'NONE',  ( -56.96214175905166854, 15.20165595797839941, -35.45940458566272468 ) ) ;
#39132 = AXIS2_PLACEMENT_3D ( 'NONE', #36352, #13268, #42319 ) ;
#39133 = EDGE_LOOP ( 'NONE', ( #45024, #7333 ) ) ;
#39134 = CIRCLE ( 'NONE', #42481, 65.00000000000000000 ) ;
#39135 = CARTESIAN_POINT ( 'NONE',  ( -39.29440389294403246, 17.09499999999999886, 0.000000000000000000 ) ) ;
#39136 = LINE ( 'NONE', #39467, #33921 ) ;
#39137 = CARTESIAN_POINT ( 'NONE',  ( 0.000000000000000000, 5.000000000000000000, 0.000000000000000000 ) ) ;
#39138 = CARTESIAN_POINT ( 'NONE',  ( 432.4999999999999432, -18.06806526123148160, 0.000000000000000000 ) ) ;
#39139 = CARTESIAN_POINT ( 'NONE',  ( 208.9583973663598329, 114.1615900753670729, 57.36381220210540022 ) ) ;
#39140 = CARTESIAN_POINT ( 'NONE',  ( -22.50000000000003197, -18.06806526123148160, -2.000000000000000000 ) ) ;
#39141 = AXIS2_PLACEMENT_3D ( 'NONE', #16729, #7238, #59632 ) ;
#39142 = VERTEX_POINT ( 'NONE', #26619 ) ;
#39143 = CARTESIAN_POINT ( 'NONE',  ( 60.62939143133406361, 12.13148391928980629, 3.341460604810993384 ) ) ;
#39144 = DIRECTION ( 'NONE',  ( 0.000000000000000000, 0.000000000000000000, 1.000000000000000000 ) ) ;
#39145 = VERTEX_POINT ( 'NONE', #21677 ) ;
#39146 = CARTESIAN_POINT ( 'NONE',  ( 213.7150814747576817, 0.000000000000000000, 277.7615984639418798 ) ) ;
#39147 = VERTEX_POINT ( 'NONE', #27648 ) ;
#39148 = EDGE_CURVE ( 'NONE', #49636, #62220, #43471, .T. ) ;
#39149 = DIRECTION ( 'NONE',  ( 0.000000000000000000, 0.000000000000000000, 1.000000000000000000 ) ) ;
#39150 = CARTESIAN_POINT ( 'NONE',  ( -55.05276343752909440, 15.72344139423348430, -23.37177340799619785 ) ) ;
#39151 = CARTESIAN_POINT ( 'NONE',  ( 106.6192711434718632, 27.24117154335862523, 30.54033420133337628 ) ) ;
#39152 = ORIENTED_EDGE ( 'NONE', *, *, #13497, .T. ) ;
#39153 = ORIENTED_EDGE ( 'NONE', *, *, #51305, .F. ) ;
#39154 = DIRECTION ( 'NONE',  ( -1.000000000000000000, 0.000000000000000000, 0.000000000000000000 ) ) ;
#39155 = CARTESIAN_POINT ( 'NONE',  ( 162.0862735437576134, 62.63196145447164298, 30.97879343093337212 ) ) ;
#39156 = DIRECTION ( 'NONE',  ( -0.000000000000000000, -0.000000000000000000, 1.000000000000000000 ) ) ;
#39157 = CARTESIAN_POINT ( 'NONE',  ( -84.49322488516129681, 0.000000000000000000, 43.58025477438756212 ) ) ;
#39158 = DIRECTION ( 'NONE',  ( 1.000000000000000000, 0.000000000000000000, -0.000000000000000000 ) ) ;
#39159 = ADVANCED_FACE ( 'NONE', ( #11122 ), #65291, .F. ) ;
#39160 = CARTESIAN_POINT ( 'NONE',  ( 65.00000000000000000, 0.000000000000000000, 55.00000000000000711 ) ) ;
#39161 = CARTESIAN_POINT ( 'NONE',  ( -50.14523569787235147, 14.45648954445650602, 5.279614992475671897 ) ) ;
#39162 = CARTESIAN_POINT ( 'NONE',  ( -132.6092625803567273, 52.31125232006262138, -12.21942496479799800 ) ) ;
#39163 = ADVANCED_FACE ( 'NONE', ( #17442 ), #17085, .F. ) ;
#39164 = CARTESIAN_POINT ( 'NONE',  ( 15.55634918610396511, -46.66904755831214402, 0.000000000000000000 ) ) ;
#39165 = DIRECTION ( 'NONE',  ( -1.000000000000000000, 0.000000000000000000, 0.000000000000000000 ) ) ;
#39166 = EDGE_CURVE ( 'NONE', #11439, #38858, #14922, .T. ) ;
#39167 = LINE ( 'NONE', #66599, #21956 ) ;
#39169 = EDGE_LOOP ( 'NONE', ( #29567, #396, #30022, #17406, #55695, #50027, #11741, #33814 ) ) ;
#39168 = CARTESIAN_POINT ( 'NONE',  ( -5.000000000000026645, -15.55634918610403616, 2.000000000000000000 ) ) ;
#39170 = VERTEX_POINT ( 'NONE', #43126 ) ;
#39171 = ORIENTED_EDGE ( 'NONE', *, *, #36787, .F. ) ;
#39172 = CARTESIAN_POINT ( 'NONE',  ( 0.000000000000000000, -6.928203230275503444, 4.000000000000010658 ) ) ;
#39173 = CARTESIAN_POINT ( 'NONE',  ( -48.56549579811112238, 13.03742088415615896, 41.61317450176976251 ) ) ;
#39174 = DIRECTION ( 'NONE',  ( -1.000000000000000000, -0.000000000000000000, -0.000000000000000000 ) ) ;
#39175 = CARTESIAN_POINT ( 'NONE',  ( -44.26023579658873075, -48.10138582123835249, 41.38025477438755928 ) ) ;
#39176 = CARTESIAN_POINT ( 'NONE',  ( -60.64199216239839529, 17.30050036439945060, -47.72342124229984250 ) ) ;
#39177 = LINE ( 'NONE', #56041, #25402 ) ;
#39178 = FACE_OUTER_BOUND ( 'NONE', #59307, .T. ) ;
#39179 = CARTESIAN_POINT ( 'NONE',  ( -10.46803069297986788, 7.077485182625209426, 44.63888823349410018 ) ) ;
#39180 = ORIENTED_EDGE ( 'NONE', *, *, #4436, .F. ) ;
#39181 = CARTESIAN_POINT ( 'NONE',  ( -3.364862276287834408, -74.92447999059862696, 0.000000000000000000 ) ) ;
#39182 = ORIENTED_EDGE ( 'NONE', *, *, #68866, .F. ) ;
#39183 = VERTEX_POINT ( 'NONE', #42780 ) ;
#39184 = AXIS2_PLACEMENT_3D ( 'NONE', #28045, #49841, #61108 ) ;
#39185 = CARTESIAN_POINT ( 'NONE',  ( -144.3939084932120807, 61.25241660819418144, 16.86807984998707255 ) ) ;
#39186 = CARTESIAN_POINT ( 'NONE',  ( -166.3205068063721512, 81.30869308872871670, 35.14705211311118660 ) ) ;
#39187 = CARTESIAN_POINT ( 'NONE',  ( 4.000000000000012434, 6.928203230275504332, -9.500000000000000000 ) ) ;
#39188 = EDGE_CURVE ( 'NONE', #9126, #59383, #54159, .T. ) ;
#39189 = CIRCLE ( 'NONE', #17843, 19.99999999999998934 ) ;
#39190 = CARTESIAN_POINT ( 'NONE',  ( -102.7502407665687372, 33.01985383847076605, 18.67452391595144690 ) ) ;
#39191 = CARTESIAN_POINT ( 'NONE',  ( 444.9999999999999432, 225.0000000000000000, 0.000000000000000000 ) ) ;
#39192 = EDGE_CURVE ( 'NONE', #38713, #26166, #49441, .T. ) ;
#39193 = DIRECTION ( 'NONE',  ( 1.000000000000000000, 0.000000000000000000, 0.000000000000000000 ) ) ;
#39194 = EDGE_LOOP ( 'NONE', ( #6390, #66279, #27964, #32857 ) ) ;
#39195 = ORIENTED_EDGE ( 'NONE', *, *, #7472, .T. ) ;
#39196 = VERTEX_POINT ( 'NONE', #22728 ) ;
#39197 = LINE ( 'NONE', #22654, #43945 ) ;
#39198 = CARTESIAN_POINT ( 'NONE',  ( -15.13254930056756642, 7.477527548005403091, 12.47888104443209123 ) ) ;
#39199 = CARTESIAN_POINT ( 'NONE',  ( 36.08729376665095145, 8.001156100723207487, -63.21872957073706800 ) ) ;
#39200 = CARTESIAN_POINT ( 'NONE',  ( 59.29615173875419032, 11.84060224810187911, -22.89344993205446244 ) ) ;
#39201 = CARTESIAN_POINT ( 'NONE',  ( -47.68743014591520080, 12.82957810971108081, 39.29583277014084786 ) ) ;
#39202 = LINE ( 'NONE', #2265, #26139 ) ;
#39203 = VERTEX_POINT ( 'NONE', #44165 ) ;
#39204 = CARTESIAN_POINT ( 'NONE',  ( 204.6977192012829789, -170.0000000000000000, 17.36317014830577321 ) ) ;
#39205 = CARTESIAN_POINT ( 'NONE',  ( 31.11269837220800127, -26.11269837220812562, 85.00100000000000477 ) ) ;
#39206 = CARTESIAN_POINT ( 'NONE',  ( 279.3447482101068431, -21.43190799616912656, -4.967656235065410542 ) ) ;
#39207 =( NAMED_UNIT ( * ) SI_UNIT ( $, .STERADIAN. ) SOLID_ANGLE_UNIT ( ) );
#39208 = CARTESIAN_POINT ( 'NONE',  ( -165.9986675144415358, 79.53506019208352029, 13.84447030584273364 ) ) ;
#39209 = CARTESIAN_POINT ( 'NONE',  ( -31.11269837220812207, -31.11269837220801193, 85.00100000000000477 ) ) ;
#39210 = FACE_BOUND ( 'NONE', #51078, .T. ) ;
#39211 = CARTESIAN_POINT ( 'NONE',  ( -189.4814416122051455, 107.4245629773156594, 90.19736142070722451 ) ) ;
#39212 = EDGE_LOOP ( 'NONE', ( #34876, #27499, #59433, #37979 ) ) ;
#39213 = CARTESIAN_POINT ( 'NONE',  ( 447.3372781065085633, 399.9999999999998863, 83.55029585798818914 ) ) ;
#39214 = CARTESIAN_POINT ( 'NONE',  ( -130.5740389938243311, 49.65308610043482673, -63.37811513693232257 ) ) ;
#39215 = CARTESIAN_POINT ( 'NONE',  ( 4.549306917177319498, -73.43672186181514405, 133.5802547743875550 ) ) ;
#39216 = CARTESIAN_POINT ( 'NONE',  ( 42.71504753277074684, 8.863481902720376837, -63.23136117686474478 ) ) ;
#39217 = CARTESIAN_POINT ( 'NONE',  ( -5.000000000000073719, -46.66904755831211560, 0.000000000000000000 ) ) ;
#39218 = VERTEX_POINT ( 'NONE', #59310 ) ;
#39219 = PRODUCT_DEFINITION ( 'UNKNOWN', '', #4042, #59846 ) ;
#39220 = ORIENTED_EDGE ( 'NONE', *, *, #65705, .T. ) ;
#39221 = FACE_OUTER_BOUND ( 'NONE', #48055, .T. ) ;
#39222 = EDGE_CURVE ( 'NONE', #33172, #52626, #32248, .T. ) ;
#39223 = CARTESIAN_POINT ( 'NONE',  ( 186.9579425186612696, 84.75281520165634674, 85.82254035461609476 ) ) ;
#39224 = ORIENTED_EDGE ( 'NONE', *, *, #60836, .T. ) ;
#39225 = ORIENTED_EDGE ( 'NONE', *, *, #18804, .T. ) ;
#39226 = EDGE_CURVE ( 'NONE', #56202, #39748, #23972, .T. ) ;
#39227 = DIRECTION ( 'NONE',  ( 0.000000000000000000, 0.000000000000000000, 1.000000000000000000 ) ) ;
#39228 = CARTESIAN_POINT ( 'NONE',  ( 152.1153500913667642, 54.85403770686899350, 42.16645570227397855 ) ) ;
#39229 = CARTESIAN_POINT ( 'NONE',  ( 204.6977192012829789, 106.3443248447423315, -36.32593103262158252 ) ) ;
#39230 = ORIENTED_EDGE ( 'NONE', *, *, #12281, .F. ) ;
#39231 = CARTESIAN_POINT ( 'NONE',  ( 117.6924004117966263, 33.61107268965019301, 62.94190954259333637 ) ) ;
#39232 = VECTOR ( 'NONE', #52966, 1000.000000000000000 ) ;
#39233 = CARTESIAN_POINT ( 'NONE',  ( -179.0654441437003186, 93.99779465816536117, 6.897009515522955603 ) ) ;
#39234 = CARTESIAN_POINT ( 'NONE',  ( -72.21652659655764239, 19.96855882996549170, -46.47546056419784577 ) ) ;
#39235 = CARTESIAN_POINT ( 'NONE',  ( 80.22637088046110421, 17.33468451430266200, -93.08378292954130018 ) ) ;
#39236 = CONICAL_SURFACE ( 'NONE', #66219, 200.0000000000000000, 1.279339532317029793 ) ;
#39237 = CARTESIAN_POINT ( 'NONE',  ( 23.09119322872580682, 6.844329382916375160, -95.00000000000133582 ) ) ;
#39238 = CARTESIAN_POINT ( 'NONE',  ( -48.71337292867759317, 14.10768470390588902, -11.85640319484388705 ) ) ;
#39239 = ADVANCED_FACE ( 'NONE', ( #10776 ), #53681, .F. ) ;
#39240 = ORIENTED_EDGE ( 'NONE', *, *, #46454, .T. ) ;
#39241 = LINE ( 'NONE', #6164, #60369 ) ;
#39242 = FACE_OUTER_BOUND ( 'NONE', #24391, .T. ) ;
#39243 = ADVANCED_FACE ( 'NONE', ( #48737 ), #33297, .F. ) ;
#39244 = CARTESIAN_POINT ( 'NONE',  ( -142.5042386072304623, 59.74110826975217492, -45.04988858504612637 ) ) ;
#39245 = EDGE_CURVE ( 'NONE', #41662, #13740, #57430, .T. ) ;
#39246 = PLANE ( 'NONE',  #56718 ) ;
#39248 = ORIENTED_EDGE ( 'NONE', *, *, #60618, .F. ) ;
#39247 = CARTESIAN_POINT ( 'NONE',  ( -132.6811329440527061, 51.12842468617797920, 94.99999999999866418 ) ) ;
#39249 = CARTESIAN_POINT ( 'NONE',  ( 84.28078136020374700, 18.63296074526051882, -36.19471234886871969 ) ) ;
#39250 = VECTOR ( 'NONE', #32403, 1000.000000000000000 ) ;
#39251 = VERTEX_POINT ( 'NONE', #46521 ) ;
#39252 = CARTESIAN_POINT ( 'NONE',  ( -125.8938041572051389, 46.49392987655492249, 30.61994787315706290 ) ) ;
#39253 = CARTESIAN_POINT ( 'NONE',  ( 81.57915404881516963, 18.81499384983930767, 31.66182794264046763 ) ) ;
#39254 = CARTESIAN_POINT ( 'NONE',  ( -439.4229916354183842, 400.0000000000065370, -128.9497041420121093 ) ) ;
#39255 = CARTESIAN_POINT ( 'NONE',  ( 187.5272808203428099, 85.37192123373904451, -20.75736303806692007 ) ) ;
#39256 =( BOUNDED_CURVE ( )  B_SPLINE_CURVE ( 3, ( #3458, #4156, #8396, #25620 ),
 .UNSPECIFIED., .F., .F. ) 
 B_SPLINE_CURVE_WITH_KNOTS ( ( 4, 4 ),
 ( 1.570796326794896558, 3.141592653589793116 ),
 .UNSPECIFIED. ) 
 CURVE ( )  GEOMETRIC_REPRESENTATION_ITEM ( )  RATIONAL_B_SPLINE_CURVE ( ( 1.000000000000000000, 0.8047378541243649375, 0.8047378541243649375, 1.000000000000000000 ) ) 
 REPRESENTATION_ITEM ( '' )  );
#39257 = CARTESIAN_POINT ( 'NONE',  ( -125.8938041572051105, 46.49392987655492959, 57.46449846362076386 ) ) ;
#39258 = CARTESIAN_POINT ( 'NONE',  ( 42.71247067544613429, 9.879726907348448606, 3.834988087375502008 ) ) ;
#39259 = CARTESIAN_POINT ( 'NONE',  ( 93.32502112557681073, 21.81526022999038261, -73.58157134791495935 ) ) ;
#39260 = CARTESIAN_POINT ( 'NONE',  ( -36.11269837220801548, 31.11269837220812207, 0.000000000000000000 ) ) ;
#39261 = ORIENTED_EDGE ( 'NONE', *, *, #41915, .T. ) ;
#39262 = ORIENTED_EDGE ( 'NONE', *, *, #1043, .T. ) ;
#39263 = CARTESIAN_POINT ( 'NONE',  ( 43.35980717318837208, 8.957244490220908517, 43.78924419203700324 ) ) ;
#39264 = CARTESIAN_POINT ( 'NONE',  ( 204.6977192012829789, 106.3443248447423173, -9.481380442157895772 ) ) ;
#39265 = CYLINDRICAL_SURFACE ( 'NONE', #45868, 7.500000000000013323 ) ;
#39266 = AXIS2_PLACEMENT_3D ( 'NONE', #33374, #50236, #22802 ) ;
#39267 = CARTESIAN_POINT ( 'NONE',  ( 311.9975424824652350, 296.0000000000000000, 420.0000000000000000 ) ) ;
#39268 = CARTESIAN_POINT ( 'NONE',  ( 207.2640160519426331, 111.6867652229576464, -50.87616464366998770 ) ) ;
#39269 = CARTESIAN_POINT ( 'NONE',  ( -77.71490760329790248, 23.03637365463982078, -76.91457645186844161 ) ) ;
#39270 = CARTESIAN_POINT ( 'NONE',  ( -149.5074843970971301, -170.0000000000000000, -88.50193171241930656 ) ) ;
#39271 = CARTESIAN_POINT ( 'NONE',  ( -28.13852122803040601, 9.072484007196647937, -49.56943753559436061 ) ) ;
#39272 = EDGE_CURVE ( 'NONE', #65661, #13467, #39682, .T. ) ;
#39273 = DIRECTION ( 'NONE',  ( -1.000000000000000000, 0.000000000000000000, 0.000000000000000000 ) ) ;
#39274 = ORIENTED_EDGE ( 'NONE', *, *, #9797, .T. ) ;
#39275 = ORIENTED_EDGE ( 'NONE', *, *, #37038, .F. ) ;
#39276 = B_SPLINE_CURVE_WITH_KNOTS ( 'NONE', 3,
 ( #10761, #5486, #58259, #48038, #38185, #53309, #63889, #37491, #15699, #69497, #11105, #11438, #21315, #69157, #32568, #31881, #58942, #20979, #53995, #42763, #53663, #48717, #64226, #198, #32910, #559, #26940, #42431, #10411, #48367, #22013, #15359, #16040, #37149, #21660, #43110, #31537, #64579, #58594, #16391, #43453, #52969, #4460, #64932, #47348, #25919, #36819, #26261 ),
 .UNSPECIFIED., .F., .F.,
 ( 4, 2, 2, 2, 2, 2, 2, 2, 2, 2, 2, 2, 2, 2, 2, 2, 2, 2, 2, 2, 2, 2, 2, 4 ),
 ( 0.02746511744866864460, 0.02914922134997091976, 0.03083332525127319146, 0.03251742915257545274, 0.03335948110322661808, 0.03420153305387777648, 0.03504358500452893488, 0.03588563695518009328, 0.03756974085648236844, 0.03841179280713351296, 0.03925384475778465748, 0.04009589670843580200, 0.04093794865908693958, 0.04262205256038922863, 0.04430615646169151767, 0.04514820841234267607, 0.04599026036299384140, 0.04767436426429616514, 0.04935846816559849581, 0.05020052011624965421, 0.05104257206690081261, 0.05272667596820312941, 0.05356872791885426699, 0.05441077986950541151 ),
 .UNSPECIFIED. ) ;
#39277 = CARTESIAN_POINT ( 'NONE',  ( 442.3372781065085633, 399.9999999999998863, 83.55029585798818914 ) ) ;
#39278 = CARTESIAN_POINT ( 'NONE',  ( 183.2136430849847955, 6.000000000000000000, -36.68900338898718871 ) ) ;
#39279 = CARTESIAN_POINT ( 'NONE',  ( 7.533997733928869067, 64.93035244659017735, 41.38025477438755928 ) ) ;
#39280 = DIRECTION ( 'NONE',  ( 0.8465179929926601732, 0.5323601107705934199, -0.000000000000000000 ) ) ;
#39281 = CARTESIAN_POINT ( 'NONE',  ( -7.825402957745085430, -170.0000000000000000, 56.96013162991089018 ) ) ;
#39282 = VECTOR ( 'NONE', #8273, 1000.000000000000000 ) ;
#39283 = DIRECTION ( 'NONE',  ( 0.000000000000000000, -1.000000000000000000, 0.000000000000000000 ) ) ;
#39284 = CARTESIAN_POINT ( 'NONE',  ( -97.48179118242302366, 31.52606332398821110, -21.45542205896860466 ) ) ;
#39285 = CARTESIAN_POINT ( 'NONE',  ( 62.53356220515464514, 13.59349015304564112, 29.81296093922127000 ) ) ;
#39286 = CARTESIAN_POINT ( 'NONE',  ( -37.04655464516766727, -53.85410457537912521, 43.58025477438756212 ) ) ;
#39287 = LINE ( 'NONE', #12549, #53317 ) ;
#39288 = ORIENTED_EDGE ( 'NONE', *, *, #29169, .F. ) ;
#39289 = DIRECTION ( 'NONE',  ( 0.000000000000000000, 1.000000000000000000, 0.000000000000000000 ) ) ;
#39290 = CARTESIAN_POINT ( 'NONE',  ( -10.92576759990585700, 8.121994053275065184, 17.60457009605725887 ) ) ;
#39291 = DIRECTION ( 'NONE',  ( 0.000000000000000000, 1.000000000000000000, 0.000000000000000000 ) ) ;
#39292 = LINE ( 'NONE', #35399, #4131 ) ;
#39293 = CARTESIAN_POINT ( 'NONE',  ( 130.3035708464390154, 40.48418876551455980, -10.05640674831288806 ) ) ;
#39294 = ORIENTED_EDGE ( 'NONE', *, *, #61914, .F. ) ;
#39295 = APPLICATION_PROTOCOL_DEFINITION ( 'draft international standard', 'automotive_design', 1998, #61055 ) ;
#39296 = VECTOR ( 'NONE', #33384, 1000.000000000000000 ) ;
#39297 = DIRECTION ( 'NONE',  ( -0.000000000000000000, -1.000000000000000000, -0.000000000000000000 ) ) ;
#39298 = CARTESIAN_POINT ( 'NONE',  ( -34.74563762132952149, 11.17960945723135602, -36.08099439004806186 ) ) ;
#39299 = LINE ( 'NONE', #33335, #48036 ) ;
#39300 = EDGE_CURVE ( 'NONE', #30808, #40134, #35285, .T. ) ;
#39301 = LINE ( 'NONE', #55828, #32145 ) ;
#39302 = VERTEX_POINT ( 'NONE', #40904 ) ;
#39303 = DIRECTION ( 'NONE',  ( 1.000000000000000000, 2.117582368135750246E-20, -1.697742017499683849E-16 ) ) ;
#39304 = CARTESIAN_POINT ( 'NONE',  ( -7.825402957745085430, 6.891034867348157178, -8.573520141480125645 ) ) ;
#39305 = DIRECTION ( 'NONE',  ( 0.000000000000000000, 0.000000000000000000, -1.000000000000000000 ) ) ;
#39306 = EDGE_CURVE ( 'NONE', #35856, #56740, #64480, .T. ) ;
#39307 = CARTESIAN_POINT ( 'NONE',  ( -7.825402957745087207, 7.899365992529248537, -62.26262132240749736 ) ) ;
#39308 = EDGE_CURVE ( 'NONE', #21223, #20719, #63621, .T. ) ;
#39309 = CARTESIAN_POINT ( 'NONE',  ( 63.01563776193091826, -170.0000000000000000, -70.06524142263343435 ) ) ;
#39310 = VERTEX_POINT ( 'NONE', #44533 ) ;
#39311 = CARTESIAN_POINT ( 'NONE',  ( 160.3272647999154401, 61.19822819988351625, -90.36850820003876095 ) ) ;
#39312 = CARTESIAN_POINT ( 'NONE',  ( 198.2545923567585362, 97.90679023593578734, -47.67529484694221509 ) ) ;
#39313 = EDGE_CURVE ( 'NONE', #32720, #56407, #49793, .T. ) ;
#39314 = CARTESIAN_POINT ( 'NONE',  ( -95.60805465865863084, 30.63099276904602775, 34.55587408256688775 ) ) ;
#39315 = AXIS2_PLACEMENT_3D ( 'NONE', #37946, #33385, #44258 ) ;
#39316 = CARTESIAN_POINT ( 'NONE',  ( 15.78827728214693416, 6.500811158483327468, -35.51894409868578606 ) ) ;
#39318 = ORIENTED_EDGE ( 'NONE', *, *, #55049, .F. ) ;
#39317 = DIRECTION ( 'NONE',  ( 0.000000000000000000, 1.000000000000000000, -0.000000000000000000 ) ) ;
#39319 = CARTESIAN_POINT ( 'NONE',  ( 59.08638499266955080, 11.79550614876701609, 30.91997476302164927 ) ) ;
#39320 = ORIENTED_EDGE ( 'NONE', *, *, #63368, .F. ) ;
#39321 = ORIENTED_EDGE ( 'NONE', *, *, #41912, .F. ) ;
#39322 = CARTESIAN_POINT ( 'NONE',  ( -71.16770070143911653, 19.60548673929831054, -16.29567994807987219 ) ) ;
#39323 = ADVANCED_FACE ( 'NONE', ( #62004 ), #33987, .F. ) ;
#39324 = CARTESIAN_POINT ( 'NONE',  ( -39.29440389294403246, 17.09499999999999886, 0.000000000000000000 ) ) ;
#39326 = ORIENTED_EDGE ( 'NONE', *, *, #68893, .T. ) ;
#39325 = CARTESIAN_POINT ( 'NONE',  ( -7.825402957745081878, 7.899365992529270741, -77.26262132240753999 ) ) ;
#39327 = CARTESIAN_POINT ( 'NONE',  ( -94.81218273889635384, 30.25676132809585894, 92.47620566321978686 ) ) ;
#39328 = CARTESIAN_POINT ( 'NONE',  ( 3.000000000000002665, 0.000000000000000000, -24.69999999999999929 ) ) ;
#39329 = VECTOR ( 'NONE', #36632, 1000.000000000000000 ) ;
#39330 = FACE_BOUND ( 'NONE', #52835, .T. ) ;
#39331 = VERTEX_POINT ( 'NONE', #15893 ) ;
#39332 = CARTESIAN_POINT ( 'NONE',  ( 211.4997502125519304, 118.0043045815490643, -73.84422742146547591 ) ) ;
#39333 = CARTESIAN_POINT ( 'NONE',  ( -38.15923928782688535, 10.79140400702259406, -12.63341888148066694 ) ) ;
#39334 = CARTESIAN_POINT ( 'NONE',  ( -179.5186635612083705, 96.12511541314941610, 42.27427310839760111 ) ) ;
#39335 = CARTESIAN_POINT ( 'NONE',  ( -132.9227230387960503, 52.53474289881227577, 13.90519458082851756 ) ) ;
#39336 = CARTESIAN_POINT ( 'NONE',  ( 18.20314211955701467, 7.596739727129570241, 57.24165582558227783 ) ) ;
#39337 = ORIENTED_EDGE ( 'NONE', *, *, #31587, .F. ) ;
#39338 = ORIENTED_EDGE ( 'NONE', *, *, #5474, .F. ) ;
#39339 = ORIENTED_EDGE ( 'NONE', *, *, #8676, .T. ) ;
#39340 = CIRCLE ( 'NONE', #47162, 242.4895526022646379 ) ;
#39341 = CARTESIAN_POINT ( 'NONE',  ( 210.1083934089977276, 114.0683883068361979, -92.30473204684062694 ) ) ;
#39342 = CARTESIAN_POINT ( 'NONE',  ( -108.6944271866238694, 37.30738480893075604, 15.09322670349537887 ) ) ;
#39343 = FACE_OUTER_BOUND ( 'NONE', #11657, .T. ) ;
#39344 = CARTESIAN_POINT ( 'NONE',  ( -38.69408084385329261, 10.89529537250242797, -40.85159504354631821 ) ) ;
#39345 = CARTESIAN_POINT ( 'NONE',  ( -94.82654088125009650, 29.15296007446479365, 90.81183754180923984 ) ) ;
#39346 = DIRECTION ( 'NONE',  ( -1.000000000000000000, 0.000000000000000000, 0.000000000000000000 ) ) ;
#39347 = LINE ( 'NONE', #12614, #56417 ) ;
#39348 = CARTESIAN_POINT ( 'NONE',  ( -71.42007367207961011, 20.75704712149298103, -17.77046668026834553 ) ) ;
#39349 = ORIENTED_EDGE ( 'NONE', *, *, #60161, .F. ) ;
#39350 = CARTESIAN_POINT ( 'NONE',  ( 80.17205177205137545, 17.31791394718355193, 60.23348464139676395 ) ) ;
#39351 = ORIENTED_EDGE ( 'NONE', *, *, #2469, .T. ) ;
#39352 = CARTESIAN_POINT ( 'NONE',  ( 31.91375106836931508, 7.553354707452896832, 36.92584114580535726 ) ) ;
#39353 = CARTESIAN_POINT ( 'NONE',  ( -439.4229916354182706, 388.0000000000064233, 91.05029585798840230 ) ) ;
#39354 = CARTESIAN_POINT ( 'NONE',  ( 184.0013086981203116, 81.60415045669144263, 43.73133913719384225 ) ) ;
#39355 = DIRECTION ( 'NONE',  ( -0.000000000000000000, -0.000000000000000000, -1.000000000000000000 ) ) ;
#39356 = PLANE ( 'NONE',  #25313 ) ;
#39357 = CARTESIAN_POINT ( 'NONE',  ( -118.4106078162223241, 42.93830006159887347, 65.53424955688741704 ) ) ;
#39358 = CARTESIAN_POINT ( 'NONE',  ( -47.56463531432803649, 12.80077789972091118, 11.46294120578592413 ) ) ;
#39359 = CARTESIAN_POINT ( 'NONE',  ( 442.3372781065085633, 392.9289321881387878, 108.5502958579838548 ) ) ;
#39360 = CARTESIAN_POINT ( 'NONE',  ( 157.9121974517528599, 59.27335488206247049, -77.96873488960137877 ) ) ;
#39361 = EDGE_LOOP ( 'NONE', ( #31989, #15933 ) ) ;
#39362 = EDGE_CURVE ( 'NONE', #51848, #37385, #57777, .T. ) ;
#39363 = CARTESIAN_POINT ( 'NONE',  ( -109.6445876100719801, 36.68207583875867073, -94.76434699328210343 ) ) ;
#39364 = LINE ( 'NONE', #48490, #40856 ) ;
#39365 = EDGE_LOOP ( 'NONE', ( #53221, #59036, #34925, #6627 ) ) ;
#39366 = CARTESIAN_POINT ( 'NONE',  ( 183.2136430849848239, 6.000000000000000000, -4.435653166495524324 ) ) ;
#39367 = CARTESIAN_POINT ( 'NONE',  ( 0.1285234777257801275, -24.99966963213046611, 0.000000000000000000 ) ) ;
#39368 = DIRECTION ( 'NONE',  ( 0.000000000000000000, -0.000000000000000000, -1.000000000000000000 ) ) ;
#39369 = VERTEX_POINT ( 'NONE', #4315 ) ;
#39370 = CARTESIAN_POINT ( 'NONE',  ( -59.89379335984659747, -45.06047301136921135, 41.38025477438755928 ) ) ;
#39371 = CARTESIAN_POINT ( 'NONE',  ( 157.0316110297313514, 58.58403635656377872, -62.96873488960130771 ) ) ;
#39372 = CARTESIAN_POINT ( 'NONE',  ( 62.53328835682435738, 12.56090025569837287, -50.72069083216976537 ) ) ;
#39373 = CARTESIAN_POINT ( 'NONE',  ( 136.3292018078238925, 42.93753790426541883, -50.60784358443687125 ) ) ;
#39374 = ORIENTED_EDGE ( 'NONE', *, *, #40268, .F. ) ;
#39375 = CARTESIAN_POINT ( 'NONE',  ( 420.5071894358209761, 1005.591584617514741, 586.5068267248775555 ) ) ;
#39376 = VECTOR ( 'NONE', #39834, 1000.000000000000000 ) ;
#39377 = CARTESIAN_POINT ( 'NONE',  ( 24.39800339187844003, 60.26242556095705538, 170.0000000000000000 ) ) ;
#39378 = ORIENTED_EDGE ( 'NONE', *, *, #4681, .T. ) ;
#39379 = FACE_OUTER_BOUND ( 'NONE', #32914, .T. ) ;
#39380 = CARTESIAN_POINT ( 'NONE',  ( -5.767955557622883589E-14, -31.11269837220806878, 2.000000000000001776 ) ) ;
#39381 = CARTESIAN_POINT ( 'NONE',  ( -1.455067768715152310, 7.566780179921177130, 14.73709619961304540 ) ) ;
#39382 = CARTESIAN_POINT ( 'NONE',  ( -2.172839205444464739, 7.595638683704374117, 59.50596416994952875 ) ) ;
#39383 = CARTESIAN_POINT ( 'NONE',  ( -200.0000000000000000, 2.449293598294706434E-14, -10.00000000000000000 ) ) ;
#39384 = EDGE_CURVE ( 'NONE', #22341, #14469, #21179, .T. ) ;
#39385 = CARTESIAN_POINT ( 'NONE',  ( 313.9975424824652350, 296.0000000000000000, 529.9060149868646477 ) ) ;
#39386 = ORIENTED_EDGE ( 'NONE', *, *, #64362, .F. ) ;
#39387 = LINE ( 'NONE', #28480, #31298 ) ;
#39388 = EDGE_LOOP ( 'NONE', ( #38814, #34914, #43692, #58320, #29668, #68818, #15484, #19334, #62132 ) ) ;
#39389 = CARTESIAN_POINT ( 'NONE',  ( 162.6190874793280159, 61.76782592053312726, -22.23833498129200237 ) ) ;
#39390 = CARTESIAN_POINT ( 'NONE',  ( 0.000000000000000000, 0.000000000000000000, 0.000000000000000000 ) ) ;
#39391 = PLANE ( 'NONE',  #12843 ) ;
#39392 = CARTESIAN_POINT ( 'NONE',  ( 141.2894128405439460, 46.09731134920845363, -69.33034730996990902 ) ) ;
#39393 = EDGE_CURVE ( 'NONE', #50834, #28516, #67766, .T. ) ;
#39394 = CARTESIAN_POINT ( 'NONE',  ( 0.000000000000000000, 0.000000000000000000, 10.00000000000000000 ) ) ;
#39395 = VERTEX_POINT ( 'NONE', #69360 ) ;
#39396 = ORIENTED_EDGE ( 'NONE', *, *, #38816, .T. ) ;
#39397 = VECTOR ( 'NONE', #64392, 1000.000000000000000 ) ;
#39398 = DIRECTION ( 'NONE',  ( 0.000000000000000000, 1.000000000000000000, -0.000000000000000000 ) ) ;
#39399 = EDGE_LOOP ( 'NONE', ( #63403, #56000, #17688, #47693 ) ) ;
#39400 = CARTESIAN_POINT ( 'NONE',  ( -60.97727891098332975, 16.35024395194892222, -74.18606411768185183 ) ) ;
#39401 = LINE ( 'NONE', #60850, #24093 ) ;
#39402 = EDGE_CURVE ( 'NONE', #14285, #53742, #64081, .T. ) ;
#39403 = ORIENTED_EDGE ( 'NONE', *, *, #65884, .T. ) ;
#39404 = CARTESIAN_POINT ( 'NONE',  ( -142.5211356634642073, 58.47296527616903461, -71.89897564660120111 ) ) ;
#39405 = CARTESIAN_POINT ( 'NONE',  ( 26.69682282325707945, 59.27986298182226221, 170.0000000000000000 ) ) ;
#39406 = CARTESIAN_POINT ( 'NONE',  ( 0.000000000000000000, 0.000000000000000000, -10.00000000000000000 ) ) ;
#39407 = ORIENTED_EDGE ( 'NONE', *, *, #69004, .T. ) ;
#39408 = DIRECTION ( 'NONE',  ( -1.000000000000000000, 0.000000000000000000, 0.000000000000000000 ) ) ;
#39409 = CARTESIAN_POINT ( 'NONE',  ( 56.65085722429434156, 12.31291088688619872, 87.02077204420697853 ) ) ;
#39410 = DIRECTION ( 'NONE',  ( 0.000000000000000000, 1.000000000000000000, 0.000000000000000000 ) ) ;
#39411 = CARTESIAN_POINT ( 'NONE',  ( -180.5200658187031308, 97.35517482626556784, -43.47889771769175127 ) ) ;
#39412 = CARTESIAN_POINT ( 'NONE',  ( -129.6001310305488801, 48.98284622040321068, -9.044787352631615818 ) ) ;
#39413 = CARTESIAN_POINT ( 'NONE',  ( -2.775557561562891351E-14, 2.999999999999969802, -50.00000000000000000 ) ) ;
#39414 = CARTESIAN_POINT ( 'NONE',  ( 127.6144785300460143, 37.78099129859913319, -74.53306838336926887 ) ) ;
#39415 = ORIENTED_EDGE ( 'NONE', *, *, #2380, .T. ) ;
#39416 = CARTESIAN_POINT ( 'NONE',  ( 140.8855094313932739, 47.03549517811092784, -67.73839220523630900 ) ) ;
#39417 = CARTESIAN_POINT ( 'NONE',  ( 86.62931800182293784, -170.0000000000000000, -23.97701360844805407 ) ) ;
#39418 = VERTEX_POINT ( 'NONE', #37688 ) ;
#39419 = CARTESIAN_POINT ( 'NONE',  ( -155.7457403566965866, 71.01814553754117298, -46.50655860890988436 ) ) ;
#39420 = CARTESIAN_POINT ( 'NONE',  ( -3.816391647148975608E-14, -9.237604307034022355, -0.7145311798163346273 ) ) ;
#39421 = CARTESIAN_POINT ( 'NONE',  ( -32.41898580403139363, 10.77423026598440003, 45.16838497460151558 ) ) ;
#39422 = CARTESIAN_POINT ( 'NONE',  ( 55.14772863908626732, 34.40534879854737227, 40.00000000000003553 ) ) ;
#39423 = CARTESIAN_POINT ( 'NONE',  ( -7.825402957745085430, 7.899365992529246761, 45.11558103944722120 ) ) ;
#39424 = CARTESIAN_POINT ( 'NONE',  ( 2.700000000000004619, 0.000000000000000000, 0.000000000000000000 ) ) ;
#39425 = CARTESIAN_POINT ( 'NONE',  ( -49.14234466229832776, 13.17605306081208383, -74.18447387590266828 ) ) ;
#39426 = CARTESIAN_POINT ( 'NONE',  ( -2.869721780807579226, 7.625909776230887616, -10.42278629837480075 ) ) ;
#39427 = CARTESIAN_POINT ( 'NONE',  ( -11.14668121284976543, 8.139398342256731311, 44.34457400782481074 ) ) ;
#39428 = CARTESIAN_POINT ( 'NONE',  ( -31.11269837220804035, 15.55634918610408945, 0.000000000000000000 ) ) ;
#39429 = CARTESIAN_POINT ( 'NONE',  ( -51.75505017849845757, 14.85991436727098680, -89.65576684818640274 ) ) ;
#39430 = ORIENTED_EDGE ( 'NONE', *, *, #57130, .T. ) ;
#39431 = CARTESIAN_POINT ( 'NONE',  ( -98.67557579989349392, 32.10670856967969655, -49.10905532852981281 ) ) ;
#39432 = EDGE_LOOP ( 'NONE', ( #37423, #30262, #64445, #40659 ) ) ;
#39433 = DIRECTION ( 'NONE',  ( -0.000000000000000000, 1.000000000000000000, -0.000000000000000000 ) ) ;
#39434 = B_SPLINE_CURVE_WITH_KNOTS ( 'NONE', 3,
 ( #32900, #43443, #42071, #32218, #31525, #15689, #58930, #37136, #37481, #16714, #11092, #58248, #21645, #10064, #69138, #37834, #20611, #5125 ),
 .UNSPECIFIED., .F., .F.,
 ( 4, 2, 2, 2, 2, 2, 2, 2, 4 ),
 ( 0.000000000000000000, 0.001383361344168719618, 0.002075042016253087016, 0.002766722688337454415, 0.004150084032506189645, 0.005533445376674925309, 0.006916806720843658371, 0.008300168065012393168, 0.01106689075334992868 ),
 .UNSPECIFIED. ) ;
#39435 = CARTESIAN_POINT ( 'NONE',  ( 85.68197636629476222, 20.16141071296262055, -77.62144078439391137 ) ) ;
#39436 = DIRECTION ( 'NONE',  ( 1.000000000000000000, -0.000000000000000000, 0.000000000000000000 ) ) ;
#39437 = CARTESIAN_POINT ( 'NONE',  ( 3.000000000000004441, 6.000000000000000000, -46.99999999999997158 ) ) ;
#39438 = LINE ( 'NONE', #17642, #49081 ) ;
#39439 = VECTOR ( 'NONE', #33907, 1000.000000000000000 ) ;
#39440 = DIRECTION ( 'NONE',  ( -0.000000000000000000, -1.000000000000000000, -0.000000000000000000 ) ) ;
#39441 = CIRCLE ( 'NONE', #22613, 5.000000000000004441 ) ;
#39442 = ADVANCED_FACE ( 'NONE', ( #52495 ), #14855, .T. ) ;
#39443 = CYLINDRICAL_SURFACE ( 'NONE', #30813, 7.500000000000013323 ) ;
#39444 = CARTESIAN_POINT ( 'NONE',  ( -120.1346137380982526, 44.00127440773566434, -20.37995546346237674 ) ) ;
#39445 = ORIENTED_EDGE ( 'NONE', *, *, #58330, .F. ) ;
#39446 = ORIENTED_EDGE ( 'NONE', *, *, #60345, .T. ) ;
#39447 = DIRECTION ( 'NONE',  ( 0.008343357611899119078, 0.000000000000000000, 0.9999651935861366692 ) ) ;
#39448 = CARTESIAN_POINT ( 'NONE',  ( 173.6020601204682237, 71.36108012062135231, 64.25024514119610330 ) ) ;
#39450 = LINE ( 'NONE', #40150, #13222 ) ;
#39449 = CIRCLE ( 'NONE', #9124, 4.999999999999990230 ) ;
#39451 = CIRCLE ( 'NONE', #60834, 10.00000000000000000 ) ;
#39452 = ADVANCED_FACE ( 'NONE', ( #16236 ), #42286, .F. ) ;
#39453 = CARTESIAN_POINT ( 'NONE',  ( 103.0124792097646775, 26.77148435100180635, 61.89731518363151253 ) ) ;
#39454 = CARTESIAN_POINT ( 'NONE',  ( -165.6215009671260816, 80.58889799860442338, -15.05329817615042742 ) ) ;
#39455 = LINE ( 'NONE', #60209, #17295 ) ;
#39456 = ORIENTED_EDGE ( 'NONE', *, *, #12388, .T. ) ;
#39457 = CARTESIAN_POINT ( 'NONE',  ( 90.30840373526895348, 21.77864858272153725, 3.827423155247575703 ) ) ;
#39458 = CARTESIAN_POINT ( 'NONE',  ( -8.811275908848678284, 6.956777180392053062, 57.00910973746761812 ) ) ;
#39459 = CARTESIAN_POINT ( 'NONE',  ( 14.08810621383466710, 7.458732232275135487, 57.05035383895328494 ) ) ;
#39460 = CYLINDRICAL_SURFACE ( 'NONE', #19542, 65.36598343705435354 ) ;
#39461 = CARTESIAN_POINT ( 'NONE',  ( -15.55634918610396866, 31.11269837220809009, 0.000000000000000000 ) ) ;
#39462 = FACE_BOUND ( 'NONE', #28558, .T. ) ;
#39463 = EDGE_CURVE ( 'NONE', #60279, #1408, #15558, .T. ) ;
#39464 = EDGE_CURVE ( 'NONE', #62549, #69370, #69002, .T. ) ;
#39465 = VERTEX_POINT ( 'NONE', #53512 ) ;
#39466 = DIRECTION ( 'NONE',  ( 0.000000000000000000, 0.000000000000000000, 1.000000000000000000 ) ) ;
#39467 = CARTESIAN_POINT ( 'NONE',  ( 444.9999999999999432, -35.00000000000000000, 378.0000000000000000 ) ) ;
#39468 = CARTESIAN_POINT ( 'NONE',  ( 31.90170717962885405, 8.563261373066634263, -69.72421537717313811 ) ) ;
#39469 = CARTESIAN_POINT ( 'NONE',  ( 63.74253542338254164, 39.54050679744534591, 170.0000000000000000 ) ) ;
#39470 = EDGE_CURVE ( 'NONE', #16594, #54975, #63749, .T. ) ;
#39471 = CARTESIAN_POINT ( 'NONE',  ( 211.7318474105134101, 118.3631723164074430, 60.93285753849514919 ) ) ;
#39472 = CARTESIAN_POINT ( 'NONE',  ( 51.04335988554098691, -7.992588018875752098, 26.66469066592269144 ) ) ;
#39473 = ORIENTED_EDGE ( 'NONE', *, *, #19296, .T. ) ;
#39474 = CARTESIAN_POINT ( 'NONE',  ( 55.57657751403270652, 11.06944050856661654, 9.482223198364021499 ) ) ;
#39475 = DIRECTION ( 'NONE',  ( 1.000000000000000000, 0.000000000000000000, 0.000000000000000000 ) ) ;
#39476 = ORIENTED_EDGE ( 'NONE', *, *, #19380, .T. ) ;
#39477 = LINE ( 'NONE', #18721, #4779 ) ;
#39478 = ORIENTED_EDGE ( 'NONE', *, *, #47800, .T. ) ;
#39479 = LINE ( 'NONE', #44765, #62232 ) ;
#39480 = CARTESIAN_POINT ( 'NONE',  ( -54.64247910309503453, -38.15499993216875652, 34.48241795236666007 ) ) ;
#39481 = CARTESIAN_POINT ( 'NONE',  ( 93.87111289824406413, 23.09598275302505854, -68.15050330965711112 ) ) ;
#39482 =( REPRESENTATION_RELATIONSHIP ('NONE','NONE', #40274, #2894 ) REPRESENTATION_RELATIONSHIP_WITH_TRANSFORMATION ( #5454 )SHAPE_REPRESENTATION_RELATIONSHIP( ) );
#39484 = ORIENTED_EDGE ( 'NONE', *, *, #11120, .T. ) ;
#39483 = EDGE_CURVE ( 'NONE', #38758, #4696, #4072, .T. ) ;
#39485 = VECTOR ( 'NONE', #50109, 1000.000000000000000 ) ;
#39486 = ORIENTED_EDGE ( 'NONE', *, *, #45037, .F. ) ;
#39487 = CARTESIAN_POINT ( 'NONE',  ( -78.66644367742109978, 23.39876645725289706, 57.26275173013680586 ) ) ;
#39488 = EDGE_CURVE ( 'NONE', #58835, #48695, #5345, .T. ) ;
#39490 = EDGE_CURVE ( 'NONE', #57773, #30714, #58447, .T. ) ;
#39489 = CARTESIAN_POINT ( 'NONE',  ( 160.9097745014957752, 61.67033591969550343, 43.57822560071761586 ) ) ;
#39491 = ADVANCED_FACE ( 'NONE', ( #10265 ), #9356, .T. ) ;
#39492 = CARTESIAN_POINT ( 'NONE',  ( -149.5074843970970733, 65.50121172469317798, -61.65738112195564469 ) ) ;
#39493 = CARTESIAN_POINT ( 'NONE',  ( 70.45451534980409747, 15.56315969138428734, 9.480703485068785241 ) ) ;
#39494 = CARTESIAN_POINT ( 'NONE',  ( 6.689127551062003185, 5.375634714784618851, -9.182649155111345607 ) ) ;
#39495 = CIRCLE ( 'NONE', #65349, 65.36598343705435354 ) ;
#39496 = ORIENTED_EDGE ( 'NONE', *, *, #234, .F. ) ;
#39497 = PRODUCT_DEFINITION_SHAPE ( 'NONE', 'NONE',  #69591 ) ;
#39498 = AXIS2_PLACEMENT_3D ( 'NONE', #18143, #44156, #32919 ) ;
#39499 = AXIS2_PLACEMENT_3D ( 'NONE', #50437, #41271, #14533 ) ;
#39500 = CARTESIAN_POINT ( 'NONE',  ( -188.8754233303960746, 108.3048424661242137, 94.99999999999866418 ) ) ;
#39501 = DIRECTION ( 'NONE',  ( 0.000000000000000000, -1.000000000000000000, 0.000000000000000000 ) ) ;
#39502 = CARTESIAN_POINT ( 'NONE',  ( -11.12071801323846820, 8.136093035169569276, -89.81606957978225125 ) ) ;
#39503 = CARTESIAN_POINT ( 'NONE',  ( 15.78827728214693416, 7.507518794609575608, 45.01470767270524931 ) ) ;
#39504 = CARTESIAN_POINT ( 'NONE',  ( 117.0065308422768453, 32.13872219870571456, -19.82875574738446289 ) ) ;
#39505 = CARTESIAN_POINT ( 'NONE',  ( 92.40591237198245267, 21.47348772973007769, 86.10604474285490539 ) ) ;
#39507 = ORIENTED_EDGE ( 'NONE', *, *, #6461, .T. ) ;
#39506 = CARTESIAN_POINT ( 'NONE',  ( 0.000000000000000000, 6.928203230275505220, -4.000000000000007994 ) ) ;
#39508 = ORIENTED_EDGE ( 'NONE', *, *, #54789, .T. ) ;
#39509 = ORIENTED_EDGE ( 'NONE', *, *, #61693, .F. ) ;
#39510 = CARTESIAN_POINT ( 'NONE',  ( 43.96465529479667822, 9.046527005589322101, 4.596442995059748071 ) ) ;
#39511 = CARTESIAN_POINT ( 'NONE',  ( -179.5301766695108086, 96.13943360322242881, 88.10265356730171504 ) ) ;
#39512 = FACE_OUTER_BOUND ( 'NONE', #45205, .T. ) ;
#39513 = CARTESIAN_POINT ( 'NONE',  ( 104.3931729003987243, 26.26823401847090977, -11.85818687836022889 ) ) ;
#39514 = CARTESIAN_POINT ( 'NONE',  ( 140.3489479654237186, 45.48511634645607415, -93.43377705359233687 ) ) ;
#39515 = CARTESIAN_POINT ( 'NONE',  ( 197.4179691534359904, 98.47175324380101813, 88.57974532536528045 ) ) ;
#39516 = CARTESIAN_POINT ( 'NONE',  ( 111.9975424824653487, 18.00000000000002842, 256.6193948016162381 ) ) ;
#39517 = CARTESIAN_POINT ( 'NONE',  ( -78.66644367742111399, 22.32174330031318377, -76.96000122218160300 ) ) ;
#39518 = CARTESIAN_POINT ( 'NONE',  ( -9.525868120571905351, 7.007646177566256185, 44.92434374916574313 ) ) ;
#39519 = VERTEX_POINT ( 'NONE', #32426 ) ;
#39520 = FACE_OUTER_BOUND ( 'NONE', #28580, .T. ) ;
#39521 = ORIENTED_EDGE ( 'NONE', *, *, #21135, .F. ) ;
#39522 = ORIENTED_EDGE ( 'NONE', *, *, #35015, .F. ) ;
#39523 = CARTESIAN_POINT ( 'NONE',  ( -64.97888516016269023, -7.103257987406330187, 3.125053320693569132E-16 ) ) ;
#39524 = CARTESIAN_POINT ( 'NONE',  ( 181.9411407973024666, 80.91291802046382031, -63.06960825634326540 ) ) ;
#39525 = CARTESIAN_POINT ( 'NONE',  ( -166.5742238910466142, 81.57147158222490191, 34.65224386300440074 ) ) ;
#39526 = CARTESIAN_POINT ( 'NONE',  ( 117.4396227366912626, 32.35611529020199129, -95.00000000000133582 ) ) ;
#39527 = CARTESIAN_POINT ( 'NONE',  ( -107.0584934212648420, 35.27493744466471526, 16.97611379505483953 ) ) ;
#39528 = CARTESIAN_POINT ( 'NONE',  ( 63.01563776193091826, 13.70579113808095251, 56.65751152968497451 ) ) ;
#39529 = CARTESIAN_POINT ( 'NONE',  ( 133.8566784816069060, 42.60093787723653236, -24.17876034193199786 ) ) ;
#39530 = ORIENTED_EDGE ( 'NONE', *, *, #28336, .F. ) ;
#39531 = ORIENTED_EDGE ( 'NONE', *, *, #61218, .F. ) ;
#39532 = ORIENTED_EDGE ( 'NONE', *, *, #68515, .F. ) ;
#39533 = ADVANCED_FACE ( 'NONE', ( #68665 ), #31798, .T. ) ;
#39534 = CARTESIAN_POINT ( 'NONE',  ( 53.32245423372616244, -37.19594572654634845, 43.58025477438756923 ) ) ;
#39535 = CARTESIAN_POINT ( 'NONE',  ( -15.07200981767290848, 7.471751903425209562, 12.71961635690741765 ) ) ;
#39536 = CARTESIAN_POINT ( 'NONE',  ( 25.00000000000763478, -65.13282190615278466, -5.000000000000000000 ) ) ;
#39537 = CARTESIAN_POINT ( 'NONE',  ( 57.08336938683662964, 11.37442068895388836, -11.76070366654272981 ) ) ;
#39538 = UNCERTAINTY_MEASURE_WITH_UNIT (LENGTH_MEASURE( 1.000000000000000082E-05 ), #37800, 'distance_accuracy_value', 'NONE');
#39539 = VECTOR ( 'NONE', #25809, 1000.000000000000114 ) ;
#39540 = CARTESIAN_POINT ( 'NONE',  ( -49.14234466229832776, 13.17605306081208028, 33.19372848595200054 ) ) ;
#39541 = LINE ( 'NONE', #17018, #58813 ) ;
#39542 = ORIENTED_EDGE ( 'NONE', *, *, #63706, .T. ) ;
#39543 = CARTESIAN_POINT ( 'NONE',  ( 21.27121078971695312, -61.42097029141944375, 170.0000000000000000 ) ) ;
#39544 = LINE ( 'NONE', #39205, #34927 ) ;
#39545 =( NAMED_UNIT ( * ) PLANE_ANGLE_UNIT ( ) SI_UNIT ( $, .RADIAN. ) );
#39546 = DIRECTION ( 'NONE',  ( -0.5877852522924802425, 0.8090169943749422332, 0.000000000000000000 ) ) ;
#39547 = CARTESIAN_POINT ( 'NONE',  ( 6.381648866512449558, -37.79907605652034874, 13.32819299319722539 ) ) ;
#39548 = DIRECTION ( 'NONE',  ( 0.000000000000000000, -1.000000000000000000, 0.000000000000000000 ) ) ;
#39549 = FACE_OUTER_BOUND ( 'NONE', #35770, .T. ) ;
#39550 = FACE_BOUND ( 'NONE', #12474, .T. ) ;
#39551 = ADVANCED_FACE ( 'NONE', ( #63050 ), #41937, .F. ) ;
#39552 = DIRECTION ( 'NONE',  ( 0.000000000000000000, 0.000000000000000000, 1.000000000000000000 ) ) ;
#39553 = EDGE_CURVE ( 'NONE', #30998, #4775, #51903, .T. ) ;
#39554 = EDGE_CURVE ( 'NONE', #22933, #36104, #28537, .T. ) ;
#39555 = AXIS2_PLACEMENT_3D ( 'NONE', #42517, #15783, #37229 ) ;
#39556 = CARTESIAN_POINT ( 'NONE',  ( -4.070918861171935355, 6.675509947362632701, 70.95737766302396210 ) ) ;
#39557 = EDGE_CURVE ( 'NONE', #64281, #23906, #54554, .T. ) ;
#39558 = VERTEX_POINT ( 'NONE', #6382 ) ;
#39559 = CARTESIAN_POINT ( 'NONE',  ( 264.4165763529819628, -27.00000000000000355, 138.9999999999999716 ) ) ;
#39560 = AXIS2_PLACEMENT_3D ( 'NONE', #359, #38000, #38346 ) ;
#39561 = CARTESIAN_POINT ( 'NONE',  ( 178.1903523079567435, 75.72906488635187827, 29.87569773046720201 ) ) ;
#39562 = FACE_OUTER_BOUND ( 'NONE', #67114, .T. ) ;
#39563 = CARTESIAN_POINT ( 'NONE',  ( 73.57152302639913444, -14.62167909564502821, 170.0000000000000000 ) ) ;
#39564 = CARTESIAN_POINT ( 'NONE',  ( 133.8566784816069344, -170.0000000000000000, 71.35489142945907304 ) ) ;
#39565 = VERTEX_POINT ( 'NONE', #12008 ) ;
#39566 = CARTESIAN_POINT ( 'NONE',  ( -130.9137245142390498, 49.88865066924345371, -90.51337433235501351 ) ) ;
#39567 = CARTESIAN_POINT ( 'NONE',  ( 188.3360522968598616, 86.25934009027517391, 88.57512505238727840 ) ) ;
#39568 = VERTEX_POINT ( 'NONE', #33815 ) ;
#39569 = ORIENTED_EDGE ( 'NONE', *, *, #27350, .T. ) ;
#39570 = CARTESIAN_POINT ( 'NONE',  ( 173.9413349464227281, 71.67637800842359752, -46.02999054611672847 ) ) ;
#39571 = CARTESIAN_POINT ( 'NONE',  ( -179.8996803435689174, 95.00451760716444483, -65.83508346284071422 ) ) ;
#39572 = DIRECTION ( 'NONE',  ( -0.000000000000000000, 0.000000000000000000, 1.000000000000000000 ) ) ;
#39573 = VERTEX_POINT ( 'NONE', #59829 ) ;
#39574 = LINE ( 'NONE', #1586, #37944 ) ;
#39575 = CARTESIAN_POINT ( 'NONE',  ( -179.9014775667593540, 95.00669833041662571, 8.259492724175739653 ) ) ;
#39576 = CARTESIAN_POINT ( 'NONE',  ( -6.126800896373024052, 6.786243985899683473, 3.461768403377602610 ) ) ;
#39577 = ADVANCED_FACE ( 'NONE', ( #27478 ), #59484, .F. ) ;
#39579 = EDGE_CURVE ( 'NONE', #49951, #59826, #23272, .T. ) ;
#39578 = DIRECTION ( 'NONE',  ( -0.000000000000000000, 1.000000000000000000, -0.000000000000000000 ) ) ;
#39580 = FACE_OUTER_BOUND ( 'NONE', #47638, .T. ) ;
#39581 = CARTESIAN_POINT ( 'NONE',  ( -47.80251179448167420, 13.89045662648309509, -13.88776572326466230 ) ) ;
#39582 = EDGE_CURVE ( 'NONE', #55128, #62781, #49986, .T. ) ;
#39583 = ORIENTED_EDGE ( 'NONE', *, *, #55831, .F. ) ;
#39584 = CARTESIAN_POINT ( 'NONE',  ( 13.56909401489539846, -65.06753427964257241, 73.58025477438755502 ) ) ;
#39585 = CARTESIAN_POINT ( 'NONE',  ( -71.97658551692140350, 20.95070248419153103, 7.673782731213468544 ) ) ;
#39586 = CARTESIAN_POINT ( 'NONE',  ( 0.000000000000000000, 0.000000000000000000, 0.000000000000000000 ) ) ;
#39587 = CARTESIAN_POINT ( 'NONE',  ( -166.5742238910465858, 81.57147158222490191, -72.72595849885027519 ) ) ;
#39589 = EDGE_LOOP ( 'NONE', ( #32501, #27177, #132, #44797, #4144, #53380, #60108, #16741, #6904 ) ) ;
#39588 = CARTESIAN_POINT ( 'NONE',  ( 112.3013380801408232, 388.0000000000077307, 101.0502958579874644 ) ) ;
#39590 = CARTESIAN_POINT ( 'NONE',  ( 84.05098130332767425, 18.55728792516086401, -36.27452980240430946 ) ) ;
#39591 = CIRCLE ( 'NONE', #9259, 74.95140232871122521 ) ;
#39592 = EDGE_LOOP ( 'NONE', ( #8998, #16237, #4608, #30060 ) ) ;
#39593 = VECTOR ( 'NONE', #2750, 1000.000000000000114 ) ;
#39594 = CARTESIAN_POINT ( 'NONE',  ( 0.000000000000000000, 35.26862320190615208, 5.000000000000000000 ) ) ;
#39595 = CARTESIAN_POINT ( 'NONE',  ( 84.05289558242219528, 19.61733656419350069, 30.16443369323296864 ) ) ;
#39596 = CARTESIAN_POINT ( 'NONE',  ( 29.86848256228520526, 58.14280299503737837, 3.125053320693577513E-16 ) ) ;
#39597 = CARTESIAN_POINT ( 'NONE',  ( 183.3913492984167988, 80.96922346472078402, -24.02000789587866691 ) ) ;
#39598 = AXIS2_PLACEMENT_3D ( 'NONE', #18159, #28717, #13236 ) ;
#39599 = CARTESIAN_POINT ( 'NONE',  ( 141.2811136745703209, 46.09188267874203149, -17.77400908926494694 ) ) ;
#39600 = FACE_OUTER_BOUND ( 'NONE', #56873, .T. ) ;
#39601 = CARTESIAN_POINT ( 'NONE',  ( -177.1514380519393512, 93.28180884530866024, -9.027143560223994001 ) ) ;
#39602 = LINE ( 'NONE', #66359, #39657 ) ;
#39603 = ORIENTED_EDGE ( 'NONE', *, *, #15240, .F. ) ;
#39604 = ORIENTED_EDGE ( 'NONE', *, *, #19720, .T. ) ;
#39605 = CARTESIAN_POINT ( 'NONE',  ( -27.00000000000000355, 26.99999999999999645, 12.00000000000000000 ) ) ;
#39606 = AXIS2_PLACEMENT_3D ( 'NONE', #41402, #3759, #62856 ) ;
#39607 = LINE ( 'NONE', #61742, #67234 ) ;
#39608 = CARTESIAN_POINT ( 'NONE',  ( 417.3372781065085633, 400.0000000000000568, -141.4497041420118251 ) ) ;
#39609 = CARTESIAN_POINT ( 'NONE',  ( 207.8398359204633152, 112.5208221429021478, -50.63919247862472162 ) ) ;
#39610 = CARTESIAN_POINT ( 'NONE',  ( -74.79539698934958381, 21.95498232236882785, -75.88833620473140229 ) ) ;
#39611 = CARTESIAN_POINT ( 'NONE',  ( -107.7743374187917169, 35.66028478413597469, 69.99245325170923593 ) ) ;
#39612 = CARTESIAN_POINT ( 'NONE',  ( 39.40195752203892710, 9.424259417798134919, -50.61981746542779348 ) ) ;
#39613 = CARTESIAN_POINT ( 'NONE',  ( 159.2319614735956463, 59.03334608081211599, -77.77237424278591504 ) ) ;
#39614 = ORIENTED_EDGE ( 'NONE', *, *, #16669, .F. ) ;
#39615 = VERTEX_POINT ( 'NONE', #60886 ) ;
#39616 = ORIENTED_EDGE ( 'NONE', *, *, #68784, .F. ) ;
#39617 = CARTESIAN_POINT ( 'NONE',  ( -8.811275908848687166, 6.956777180392055726, -50.36909262438710755 ) ) ;
#39618 = ADVANCED_FACE ( 'NONE', ( #32767 ), #17636, .F. ) ;
#39619 = PLANE ( 'NONE',  #24079 ) ;
#39620 = CARTESIAN_POINT ( 'NONE',  ( -78.66644367742109978, 22.32174330031321574, 72.26275173013684139 ) ) ;
#39621 = CARTESIAN_POINT ( 'NONE',  ( 127.2358066117907072, 38.72257733469226082, 33.44959100710425304 ) ) ;
#39622 = LINE ( 'NONE', #61424, #15326 ) ;
#39623 = DIRECTION ( 'NONE',  ( 1.000000000000000000, 0.000000000000000000, 0.000000000000000000 ) ) ;
#39624 = CARTESIAN_POINT ( 'NONE',  ( -101.3502439362134737, 33.43728945125136676, -23.12672091462772883 ) ) ;
#39625 = CARTESIAN_POINT ( 'NONE',  ( 59.73312635112156244, 12.96464920523511033, 30.55208854348506975 ) ) ;
#39626 = CARTESIAN_POINT ( 'NONE',  ( 34.55331630735146575, 7.828237636019207635, 85.37150955030359967 ) ) ;
#39627 = CARTESIAN_POINT ( 'NONE',  ( 311.9975424824652350, 20.00000000000003197, 256.6193948016162381 ) ) ;
#39628 = ORIENTED_EDGE ( 'NONE', *, *, #31320, .F. ) ;
#39629 = DIRECTION ( 'NONE',  ( 0.000000000000000000, 0.000000000000000000, 1.000000000000000000 ) ) ;
#39630 = FACE_OUTER_BOUND ( 'NONE', #5355, .T. ) ;
#39631 = CARTESIAN_POINT ( 'NONE',  ( -189.5329886872042948, 107.4958891766010964, -44.24249695867173671 ) ) ;
#39632 = ADVANCED_FACE ( 'NONE', ( #60190 ), #33482, .F. ) ;
#39633 = CARTESIAN_POINT ( 'NONE',  ( -94.87734348028330089, -170.0000000000000000, -95.00000000000133582 ) ) ;
#39634 = CARTESIAN_POINT ( 'NONE',  ( 197.8572563162090887, 97.41072138832258531, 66.64235681249728316 ) ) ;
#39635 = CARTESIAN_POINT ( 'NONE',  ( 127.2107679985236217, 38.70844091144998345, -13.16384531823007897 ) ) ;
#39636 = ADVANCED_FACE ( 'NONE', ( #54904 ), #28174, .T. ) ;
#39637 = EDGE_CURVE ( 'NONE', #31182, #46298, #400, .T. ) ;
#39638 = ORIENTED_EDGE ( 'NONE', *, *, #41836, .F. ) ;
#39639 = DIRECTION ( 'NONE',  ( 0.4127148655274873734, -0.9108602745606090290, -7.852085311506935167E-15 ) ) ;
#39640 = LINE ( 'NONE', #38956, #66680 ) ;
#39641 = CARTESIAN_POINT ( 'NONE',  ( -126.7989199172159260, 47.09198523267863834, 3.816158964292980738 ) ) ;
#39642 = CYLINDRICAL_SURFACE ( 'NONE', #22245, 4.999999999999990230 ) ;
#39643 = CONTEXT_DEPENDENT_SHAPE_REPRESENTATION ( #7229, #50115 ) ;
#39644 = DIRECTION ( 'NONE',  ( 0.3090169943749446757, 0.9510565162951544194, 0.000000000000000000 ) ) ;
#39645 = ORIENTED_EDGE ( 'NONE', *, *, #5193, .F. ) ;
#39646 = CARTESIAN_POINT ( 'NONE',  ( -123.6699087229881968, 45.04696784753414818, -49.58003572520509294 ) ) ;
#39647 = AXIS2_PLACEMENT_3D ( 'NONE', #34345, #55788, #33648 ) ;
#39648 = CARTESIAN_POINT ( 'NONE',  ( 26.99999999999999645, 26.99999999999999645, 12.00000000000000000 ) ) ;
#39649 = VECTOR ( 'NONE', #27320, 1000.000000000000114 ) ;
#39650 = CARTESIAN_POINT ( 'NONE',  ( -0.3740447803642789060, 7.527031846085010081, -70.74654756650022591 ) ) ;
#39651 = CIRCLE ( 'NONE', #35134, 25.12245591505646303 ) ;
#39652 = CARTESIAN_POINT ( 'NONE',  ( -35.00000000000002842, -35.00000000000000000, 380.0000000000000000 ) ) ;
#39653 = EDGE_LOOP ( 'NONE', ( #54132, #35407, #14471, #42482 ) ) ;
#39654 = CARTESIAN_POINT ( 'NONE',  ( -55.53456145826333312, 15.85318253404851774, 3.472777182467473356 ) ) ;
#39655 = FACE_OUTER_BOUND ( 'NONE', #52021, .T. ) ;
#39656 = CARTESIAN_POINT ( 'NONE',  ( -97.86516199987805464, 31.71158167298307617, 31.93729686093309184 ) ) ;
#39657 = VECTOR ( 'NONE', #23080, 1000.000000000000000 ) ;
#39658 = CARTESIAN_POINT ( 'NONE',  ( 22.29513692215317988, 6.796052026456506745, -46.78078019334662940 ) ) ;
#39660 = ORIENTED_EDGE ( 'NONE', *, *, #33419, .F. ) ;
#39659 = CARTESIAN_POINT ( 'NONE',  ( 116.0963032583228483, 32.80867113471310148, 5.551094412785531063 ) ) ;
#39661 = EDGE_CURVE ( 'NONE', #57513, #2845, #41891, .T. ) ;
#39662 = LINE ( 'NONE', #12942, #50800 ) ;
#39663 = ORIENTED_EDGE ( 'NONE', *, *, #47650, .T. ) ;
#39664 = ORIENTED_EDGE ( 'NONE', *, *, #13251, .T. ) ;
#39665 = CARTESIAN_POINT ( 'NONE',  ( 178.1888264190354505, 77.13727704498028004, 43.74063381377031590 ) ) ;
#39666 = CARTESIAN_POINT ( 'NONE',  ( 23.23895241123075550, 6.853530908437178049, -70.85169307199515742 ) ) ;
#39668 = EDGE_LOOP ( 'NONE', ( #63063, #17368, #852, #64172 ) ) ;
#39667 = PLANE ( 'NONE',  #48889 ) ;
#39669 = CARTESIAN_POINT ( 'NONE',  ( -95.54114085644955878, 30.59949910443587839, 94.99999999999866418 ) ) ;
#39670 = CARTESIAN_POINT ( 'NONE',  ( 141.9165763529819344, 242.0000000000000000, 108.9999999999999858 ) ) ;
#39671 = CARTESIAN_POINT ( 'NONE',  ( -72.21947956767114363, 21.03570528348187452, -46.45601792771012839 ) ) ;
#39672 = ORIENTED_EDGE ( 'NONE', *, *, #12713, .T. ) ;
#39673 = CARTESIAN_POINT ( 'NONE',  ( 208.5884523568772693, 113.6152425727545250, -64.24464719657447631 ) ) ;
#39674 = CARTESIAN_POINT ( 'NONE',  ( 139.3041645503688244, 46.00819478311335331, 31.84931363288263384 ) ) ;
#39676 = CARTESIAN_POINT ( 'NONE',  ( -175.9944734395086527, 91.92390745845763433, 45.26234191262543050 ) ) ;
#39675 = AXIS2_PLACEMENT_3D ( 'NONE', #56854, #19556, #41016 ) ;
#39677 = FACE_OUTER_BOUND ( 'NONE', #176, .T. ) ;
#39678 = FACE_OUTER_BOUND ( 'NONE', #64159, .T. ) ;
#39679 = ORIENTED_EDGE ( 'NONE', *, *, #32224, .F. ) ;
#39680 = VERTEX_POINT ( 'NONE', #66196 ) ;
#39681 = VERTEX_POINT ( 'NONE', #17989 ) ;
#39682 = CIRCLE ( 'NONE', #66671, 5.000000000000000888 ) ;
#39683 = CARTESIAN_POINT ( 'NONE',  ( -2.000000000000000000, -2.000000000000000000, 380.0000000000000000 ) ) ;
#39684 = EDGE_CURVE ( 'NONE', #38471, #69231, #11646, .T. ) ;
#39685 = CARTESIAN_POINT ( 'NONE',  ( -64.18058723658640474, -10.37664328995274055, 170.0000000000000000 ) ) ;
#39686 = AXIS2_PLACEMENT_3D ( 'NONE', #3118, #68180, #47381 ) ;
#39687 = CARTESIAN_POINT ( 'NONE',  ( -38.16002576456689610, 10.79155573432543314, -46.15488383467597089 ) ) ;
#39688 = DIRECTION ( 'NONE',  ( 1.000000000000000000, 0.000000000000000000, 0.000000000000000000 ) ) ;
#39689 = CARTESIAN_POINT ( 'NONE',  ( -142.0685766576042397, 58.11789490499574384, 39.33001764120334087 ) ) ;
#39691 = EDGE_CURVE ( 'NONE', #35756, #66616, #6018, .T. ) ;
#39690 = CIRCLE ( 'NONE', #68892, 24.99999999999985434 ) ;
#39692 = CARTESIAN_POINT ( 'NONE',  ( 55.61348889667009132, -50.24791103897046440, 41.38025477438755928 ) ) ;
#39693 = FACE_OUTER_BOUND ( 'NONE', #33001, .T. ) ;
#39695 = ORIENTED_EDGE ( 'NONE', *, *, #22422, .F. ) ;
#39694 = EDGE_CURVE ( 'NONE', #40482, #35601, #30119, .T. ) ;
#39697 = CARTESIAN_POINT ( 'NONE',  ( 84.74140601443113496, 18.78541996275572856, 71.31910537301371278 ) ) ;
#39696 = VECTOR ( 'NONE', #50973, 1000.000000000000000 ) ;
#39698 = EDGE_LOOP ( 'NONE', ( #6976, #46148, #42257, #48987 ) ) ;
#39699 = CARTESIAN_POINT ( 'NONE',  ( -95.15214927927195276, 30.41622044381585255, -93.85950614209359344 ) ) ;
#39700 = EDGE_CURVE ( 'NONE', #38482, #18908, #2162, .T. ) ;
#39701 = VECTOR ( 'NONE', #25465, 1000.000000000000000 ) ;
#39702 = FACE_OUTER_BOUND ( 'NONE', #7592, .T. ) ;
#39703 = DIRECTION ( 'NONE',  ( -0.000000000000000000, 1.000000000000000000, -0.000000000000000000 ) ) ;
#39704 = DIRECTION ( 'NONE',  ( 0.000000000000000000, 0.000000000000000000, -1.000000000000000000 ) ) ;
#39705 = LINE ( 'NONE', #23534, #25542 ) ;
#39706 = CARTESIAN_POINT ( 'NONE',  ( 163.5430354047457229, 63.84092878795252801, 94.99999999999866418 ) ) ;
#39707 = AXIS2_PLACEMENT_3D ( 'NONE', #46183, #68007, #2592 ) ;
#39708 = CARTESIAN_POINT ( 'NONE',  ( 99.99999999999997158, 0.000000000000000000, -25.00000000000000000 ) ) ;
#39709 = LINE ( 'NONE', #23540, #53530 ) ;
#39710 = ORIENTED_EDGE ( 'NONE', *, *, #19321, .T. ) ;
#39711 = LINE ( 'NONE', #8400, #34226 ) ;
#39712 = CARTESIAN_POINT ( 'NONE',  ( -156.9406434201984553, 70.74968524571475825, -14.31838670552433257 ) ) ;
#39713 = EDGE_LOOP ( 'NONE', ( #52115, #19097, #36125, #39815 ) ) ;
#39714 = DIRECTION ( 'NONE',  ( -0.8090169943749422332, -0.5877852522924802425, 0.000000000000000000 ) ) ;
#39715 = CARTESIAN_POINT ( 'NONE',  ( -62.30163634902125125, 17.79682011226253380, 62.67378655492601780 ) ) ;
#39716 = DIRECTION ( 'NONE',  ( -0.9959742939952384022, -0.08963930890344089242, 0.000000000000000000 ) ) ;
#39717 = VERTEX_POINT ( 'NONE', #24658 ) ;
#39718 = LINE ( 'NONE', #30211, #50223 ) ;
#39719 = CARTESIAN_POINT ( 'NONE',  ( 6.400000000000000355, -4.618802153517016507, -8.000000000000000000 ) ) ;
#39720 = CARTESIAN_POINT ( 'NONE',  ( -38.69577193929646342, 10.89562623693160326, 35.75813062815972643 ) ) ;
#39721 = CARTESIAN_POINT ( 'NONE',  ( 2.999999999999992450, 0.000000000000000000, -21.02499999999999858 ) ) ;
#39722 = EDGE_CURVE ( 'NONE', #5460, #31511, #55391, .T. ) ;
#39723 = EDGE_CURVE ( 'NONE', #67765, #16637, #68843, .T. ) ;
#39724 = ORIENTED_EDGE ( 'NONE', *, *, #68839, .F. ) ;
#39725 = DIRECTION ( 'NONE',  ( 0.000000000000000000, 0.000000000000000000, 1.000000000000000000 ) ) ;
#39726 = CARTESIAN_POINT ( 'NONE',  ( 329.1355598199468204, 190.0000000000000000, -129.5087625010780812 ) ) ;
#39727 = EDGE_LOOP ( 'NONE', ( #68161, #64170, #36644, #55034 ) ) ;
#39728 = LINE ( 'NONE', #18273, #26713 ) ;
#39729 = DIRECTION ( 'NONE',  ( 0.000000000000000000, -1.000000000000000000, 0.000000000000000000 ) ) ;
#39730 = CARTESIAN_POINT ( 'NONE',  ( 141.3476419847744694, 47.33903275097040364, 90.28850992081258653 ) ) ;
#39731 = CARTESIAN_POINT ( 'NONE',  ( -25.51439092786625906, 9.709553105505657200, -91.90258131718498191 ) ) ;
#39732 = PLANE ( 'NONE',  #66532 ) ;
#39733 = CIRCLE ( 'NONE', #30797, 23.50000000000000000 ) ;
#39734 = CARTESIAN_POINT ( 'NONE',  ( -17.90772993695113868, 72.84144224619130625, 170.0000000000000000 ) ) ;
#39735 = VERTEX_POINT ( 'NONE', #62633 ) ;
#39736 = CARTESIAN_POINT ( 'NONE',  ( -65.20298343242131978, -4.613322252418188718, 41.38025477438755928 ) ) ;
#39737 = CARTESIAN_POINT ( 'NONE',  ( -45.00000000000002132, 20.00000000000000355, 2.000000000000015543 ) ) ;
#39738 = VECTOR ( 'NONE', #53080, 1000.000000000000000 ) ;
#39739 = CARTESIAN_POINT ( 'NONE',  ( 437.3372781065085633, 400.0000000000000568, -141.4497041420118251 ) ) ;
#39740 = DIRECTION ( 'NONE',  ( -0.5508969814520944253, -0.8345732537213078617, 0.000000000000000000 ) ) ;
#39741 = LINE ( 'NONE', #44311, #26293 ) ;
#39742 = CIRCLE ( 'NONE', #13927, 25.00000000000000000 ) ;
#39743 = ORIENTED_EDGE ( 'NONE', *, *, #1694, .T. ) ;
#39744 = AXIS2_PLACEMENT_3D ( 'NONE', #16496, #27386, #1019 ) ;
#39745 = CARTESIAN_POINT ( 'NONE',  ( 158.3636111008086687, 59.62671916656141491, -9.279633708673955539 ) ) ;
#39746 = VECTOR ( 'NONE', #22677, 1000.000000000000000 ) ;
#39747 = DIRECTION ( 'NONE',  ( 0.000000000000000000, 0.000000000000000000, 1.000000000000000000 ) ) ;
#39748 = VERTEX_POINT ( 'NONE', #61917 ) ;
#39749 = CARTESIAN_POINT ( 'NONE',  ( -61.86845765289633192, 16.61548683002700599, -72.70064571127269915 ) ) ;
#39750 = CARTESIAN_POINT ( 'NONE',  ( 447.3372781065085064, 364.9999999999990905, 113.5502958579887007 ) ) ;
#39751 = VECTOR ( 'NONE', #48604, 1000.000000000000000 ) ;
#39752 = VECTOR ( 'NONE', #36598, 1000.000000000000114 ) ;
#39753 = ORIENTED_EDGE ( 'NONE', *, *, #12621, .T. ) ;
#39754 = CARTESIAN_POINT ( 'NONE',  ( -146.7345109736526183, 61.86270848728296556, -62.18528878719732944 ) ) ;
#39755 = DIRECTION ( 'NONE',  ( 0.000000000000000000, 0.000000000000000000, -1.000000000000000000 ) ) ;
#39756 = CARTESIAN_POINT ( 'NONE',  ( 44.99999999999999289, -20.00000000000000355, 2.000000000000015543 ) ) ;
#39757 = EDGE_LOOP ( 'NONE', ( #40573, #42331, #67465, #41830 ) ) ;
#39758 = CARTESIAN_POINT ( 'NONE',  ( -96.76336539645313906, 31.18045094643428428, 6.069607441441186246 ) ) ;
#39759 = CARTESIAN_POINT ( 'NONE',  ( 2.700000000000004619, 0.000000000000000000, 0.000000000000000000 ) ) ;
#39760 = CARTESIAN_POINT ( 'NONE',  ( 32.15613847490629240, 8.588587416860168133, 35.46206655629798377 ) ) ;
#39761 = CARTESIAN_POINT ( 'NONE',  ( -179.8926034784145713, 96.58272071140105197, -45.44813079124821797 ) ) ;
#39762 = CARTESIAN_POINT ( 'NONE',  ( -132.9109786433856186, 51.29129389542017492, -12.90849194883207041 ) ) ;
#39763 = CARTESIAN_POINT ( 'NONE',  ( 32.65658189266903122, 8.638786419050411780, -93.42454832150183108 ) ) ;
#39764 = PLANE ( 'NONE',  #42835 ) ;
#39765 = EDGE_LOOP ( 'NONE', ( #48662, #16821, #15305, #40563 ) ) ;
#39766 = FACE_OUTER_BOUND ( 'NONE', #7028, .T. ) ;
#39767 = CARTESIAN_POINT ( 'NONE',  ( -12.77550690612892481, 8.273784096785073316, 58.80457690568544393 ) ) ;
#39768 = EDGE_LOOP ( 'NONE', ( #51397, #9685, #23675, #26119 ) ) ;
#39769 = CARTESIAN_POINT ( 'NONE',  ( -152.5101325120253080, 68.10842280990927122, -35.42590201308884446 ) ) ;
#39770 = CARTESIAN_POINT ( 'NONE',  ( 4.000000000000011546, -6.928203230275505220, 0.000000000000000000 ) ) ;
#39771 = CARTESIAN_POINT ( 'NONE',  ( -31.43908319763709969, 10.61114334766716105, 45.21645440618919309 ) ) ;
#39772 = FACE_OUTER_BOUND ( 'NONE', #62147, .T. ) ;
#39773 = CARTESIAN_POINT ( 'NONE',  ( -85.35521056349260505, -170.0000000000000000, 94.99999999999866418 ) ) ;
#39774 = CARTESIAN_POINT ( 'NONE',  ( -49.62489392740899063, 13.29305723289024499, -74.74236697503437199 ) ) ;
#39775 = CARTESIAN_POINT ( 'NONE',  ( -4.071369321747700276, 7.682719369516286534, -9.562191003685860835 ) ) ;
#39776 = EDGE_CURVE ( 'NONE', #19186, #69231, #38523, .T. ) ;
#39777 = CARTESIAN_POINT ( 'NONE',  ( -13.45956523846225039, 8.333781915634245863, 32.65906174219168889 ) ) ;
#39778 = CARTESIAN_POINT ( 'NONE',  ( -61.39252081892701796, 16.47343302442960677, 6.958049073610734325 ) ) ;
#39779 = ORIENTED_EDGE ( 'NONE', *, *, #876, .F. ) ;
#39780 = AXIS2_PLACEMENT_3D ( 'NONE', #32820, #6438, #43699 ) ;
#39781 = CARTESIAN_POINT ( 'NONE',  ( -35.66505483122875120, 56.29927536160143831, 34.48241795236666007 ) ) ;
#39783 = ORIENTED_EDGE ( 'NONE', *, *, #55416, .F. ) ;
#39782 = EDGE_CURVE ( 'NONE', #27706, #61321, #23614, .T. ) ;
#39784 = CARTESIAN_POINT ( 'NONE',  ( 107.2672065034543039, 27.52931006625853172, -77.15546443931920351 ) ) ;
#39785 = CARTESIAN_POINT ( 'NONE',  ( 46.51377856795993893, 10.46037936279324576, -13.84377530420647240 ) ) ;
#39786 = STYLED_ITEM ( 'NONE', ( #20490 ), #40699 ) ;
#39787 = LINE ( 'NONE', #56658, #5793 ) ;
#39788 = CARTESIAN_POINT ( 'NONE',  ( 8.000000000000003553, -4.618802153517020948, -8.785468820183664818 ) ) ;
#39790 = MANIFOLD_SOLID_BREP ( 'Chamfer1', #15947 ) ;
#39789 = EDGE_CURVE ( 'NONE', #3161, #24241, #50679, .T. ) ;
#39791 = DIRECTION ( 'NONE',  ( 0.000000000000000000, 0.000000000000000000, 1.000000000000000000 ) ) ;
#39792 = CARTESIAN_POINT ( 'NONE',  ( 0.01688885742776611437, 6.535341423375590431, -4.680456609903974829 ) ) ;
#39793 = AXIS2_PLACEMENT_3D ( 'NONE', #36606, #5275, #26396 ) ;
#39794 = LINE ( 'NONE', #19370, #11707 ) ;
#39795 = CARTESIAN_POINT ( 'NONE',  ( -165.7699288023689519, 79.30174988963860017, 63.65066555552893846 ) ) ;
#39796 = ORIENTED_EDGE ( 'NONE', *, *, #52932, .T. ) ;
#39797 = AXIS2_PLACEMENT_3D ( 'NONE', #59749, #53778, #59066 ) ;
#39798 = ORIENTED_EDGE ( 'NONE', *, *, #51245, .T. ) ;
#39799 = AXIS2_PLACEMENT_3D ( 'NONE', #15431, #48696, #14729 ) ;
#39800 = LINE ( 'NONE', #50357, #24236 ) ;
#39801 = DIRECTION ( 'NONE',  ( -0.000000000000000000, -0.000000000000000000, 1.000000000000000000 ) ) ;
#39802 = CARTESIAN_POINT ( 'NONE',  ( 46.14647339926992231, 9.382387518671809090, -93.42281443246146466 ) ) ;
#39803 = CARTESIAN_POINT ( 'NONE',  ( -173.1211646369891355, 88.63826465341151106, 57.66624519710472185 ) ) ;
#39804 = CIRCLE ( 'NONE', #34192, 20.00000000000000000 ) ;
#39805 = CARTESIAN_POINT ( 'NONE',  ( -165.9154624515710168, 80.89088623112733956, -13.26577719977006531 ) ) ;
#39806 = EDGE_CURVE ( 'NONE', #50609, #23032, #61592, .T. ) ;
#39807 = DIRECTION ( 'NONE',  ( 0.000000000000000000, 0.000000000000000000, 1.000000000000000000 ) ) ;
#39808 = EDGE_LOOP ( 'NONE', ( #38281, #10191, #10365, #47507, #19731, #36761, #32736, #54689, #46650 ) ) ;
#39809 = CARTESIAN_POINT ( 'NONE',  ( 107.0447263249841541, 28.53200276018956671, -36.63432886298605240 ) ) ;
#39810 = CARTESIAN_POINT ( 'NONE',  ( 20.74561700410410836, 7.717362891868937425, -37.36968443880168422 ) ) ;
#39811 = CARTESIAN_POINT ( 'NONE',  ( -83.14462298835724141, 24.07775853418029044, -21.80647150814679947 ) ) ;
#39812 = DIRECTION ( 'NONE',  ( -0.000000000000000000, 1.000000000000000000, -0.000000000000000000 ) ) ;
#39813 = CARTESIAN_POINT ( 'NONE',  ( 0.000000000000000000, 0.000000000000000000, 40.00000000000003553 ) ) ;
#39814 = FACE_BOUND ( 'NONE', #64227, .T. ) ;
#39815 = ORIENTED_EDGE ( 'NONE', *, *, #22530, .F. ) ;
#39816 = DIRECTION ( 'NONE',  ( 0.2225209339563042066, 0.9749279121818259508, -0.000000000000000000 ) ) ;
#39817 = FACE_OUTER_BOUND ( 'NONE', #18634, .T. ) ;
#39818 = CARTESIAN_POINT ( 'NONE',  ( 32.29578462738147238, 8.602609172809795979, -67.55334439686617998 ) ) ;
#39819 = CARTESIAN_POINT ( 'NONE',  ( -179.8926034784146282, 96.58272071140106618, 8.240970389679118213 ) ) ;
#39820 = CARTESIAN_POINT ( 'NONE',  ( 212.1976655298228707, 119.0878071902807562, 63.37440967419005489 ) ) ;
#39821 = CARTESIAN_POINT ( 'NONE',  ( 3.306546357697853733E-15, 0.000000000000000000, 27.00000000000000000 ) ) ;
#39822 = ORIENTED_EDGE ( 'NONE', *, *, #2955, .T. ) ;
#39823 = CYLINDRICAL_SURFACE ( 'NONE', #2229, 5.000000000000004441 ) ;
#39824 = DIRECTION ( 'NONE',  ( 0.000000000000000000, -1.000000000000000000, 0.000000000000000000 ) ) ;
#39825 = ORIENTED_EDGE ( 'NONE', *, *, #66739, .F. ) ;
#39826 = CARTESIAN_POINT ( 'NONE',  ( -31.11269837220801193, 31.11269837220812207, 0.000000000000000000 ) ) ;
#39827 = EDGE_LOOP ( 'NONE', ( #21410, #26054, #18298, #64082 ) ) ;
#39828 = CARTESIAN_POINT ( 'NONE',  ( -84.23431294393864732, 24.52078568147204862, -74.50897725631355684 ) ) ;
#39829 = CARTESIAN_POINT ( 'NONE',  ( -62.30163634902124414, 17.79682011226252669, -17.85986521646501757 ) ) ;
#39830 = SPHERICAL_SURFACE ( 'NONE', #26860, 3.000000000000000000 ) ;
#39831 = VERTEX_POINT ( 'NONE', #20745 ) ;
#39832 = EDGE_LOOP ( 'NONE', ( #52393, #54427, #3004, #64580 ) ) ;
#39833 = CARTESIAN_POINT ( 'NONE',  ( 8.288451200428832877, 6.376395059685425082, -42.52704783185547655 ) ) ;
#39834 = DIRECTION ( 'NONE',  ( 0.000000000000000000, 0.000000000000000000, -1.000000000000000000 ) ) ;
#39835 = CARTESIAN_POINT ( 'NONE',  ( 109.3047140914111424, 29.55674059952507093, 17.72275918544008277 ) ) ;
#39836 = CIRCLE ( 'NONE', #57815, 74.95140232871122521 ) ;
#39837 = ORIENTED_EDGE ( 'NONE', *, *, #49312, .T. ) ;
#39838 = EDGE_CURVE ( 'NONE', #15039, #42011, #22495, .T. ) ;
#39839 = CIRCLE ( 'NONE', #3895, 21.00000000000000355 ) ;
#39840 = CONICAL_SURFACE ( 'NONE', #24139, 8.000000000000000000, 1.047197551196600296 ) ;
#39841 = LINE ( 'NONE', #34919, #22197 ) ;
#39842 = CARTESIAN_POINT ( 'NONE',  ( -52.68206656346372796, 15.09776187114412949, 18.09236373069973780 ) ) ;
#39843 = VECTOR ( 'NONE', #46226, 1000.000000000000000 ) ;
#39844 = DIRECTION ( 'NONE',  ( -0.000000000000000000, -0.000000000000000000, -1.000000000000000000 ) ) ;
#39845 = DIRECTION ( 'NONE',  ( -0.000000000000000000, -0.000000000000000000, -1.000000000000000000 ) ) ;
#39846 = CARTESIAN_POINT ( 'NONE',  ( 79.93911349260510235, 17.24571896967717777, 87.49448148412906789 ) ) ;
#39848 = VERTEX_POINT ( 'NONE', #3884 ) ;
#39847 = CARTESIAN_POINT ( 'NONE',  ( -167.0144425875893432, 82.02896103816512152, -91.51796402915401529 ) ) ;
#39849 = ORIENTED_EDGE ( 'NONE', *, *, #44651, .F. ) ;
#39850 = ORIENTED_EDGE ( 'NONE', *, *, #50642, .T. ) ;
#39851 = CARTESIAN_POINT ( 'NONE',  ( 44.86216938219160966, 9.182565662897500758, 5.421885990403858990 ) ) ;
#39852 = CARTESIAN_POINT ( 'NONE',  ( -178.4080989094417475, 94.78067157791448949, 86.68361982195993676 ) ) ;
#39853 = CARTESIAN_POINT ( 'NONE',  ( 0.000000000000000000, -6.928203230275505220, -4.000000000000007105 ) ) ;
#39854 = CARTESIAN_POINT ( 'NONE',  ( 102.7435092758397843, 25.56449004647816992, -16.30709162799740142 ) ) ;
#39855 = CARTESIAN_POINT ( 'NONE',  ( 197.5334904971815888, 97.00846725096930356, 12.10439990847099345 ) ) ;
#39856 = EDGE_CURVE ( 'NONE', #29971, #31797, #60458, .T. ) ;
#39857 = CARTESIAN_POINT ( 'NONE',  ( 199.0264175060451066, 100.5059091267551707, 85.47604204415401341 ) ) ;
#39858 = EDGE_CURVE ( 'NONE', #67200, #33912, #38298, .T. ) ;
#39859 = CARTESIAN_POINT ( 'NONE',  ( -38.02163356681019479, -170.0000000000000000, 94.99999999999866418 ) ) ;
#39860 = CARTESIAN_POINT ( 'NONE',  ( -77.02372450489328060, 21.70271995013165167, -76.78175660144862036 ) ) ;
#39861 = CARTESIAN_POINT ( 'NONE',  ( -15.22871623201694291, 7.486724405784661585, 36.39031658515959577 ) ) ;
#39862 = ORIENTED_EDGE ( 'NONE', *, *, #69144, .F. ) ;
#39863 = CARTESIAN_POINT ( 'NONE',  ( 14.81290967676422277, 7.477658233646008235, -23.62699843601409455 ) ) ;
#39864 = EDGE_LOOP ( 'NONE', ( #34025, #38116, #60982, #34442 ) ) ;
#39865 = EDGE_LOOP ( 'NONE', ( #48452, #64125, #12280 ) ) ;
#39866 = CARTESIAN_POINT ( 'NONE',  ( -147.7925265216585444, 64.04960911618972830, 4.071655134873576110 ) ) ;
#39867 = CARTESIAN_POINT ( 'NONE',  ( 186.5979919519638202, 85.84756789133379584, -65.47989607005200696 ) ) ;
#39868 = CARTESIAN_POINT ( 'NONE',  ( -35.68184644965160857, 11.34911992846755524, 85.21252114010754042 ) ) ;
#39869 = ADVANCED_FACE ( 'NONE', ( #22470 ), #64692, .F. ) ;
#39870 = FACE_OUTER_BOUND ( 'NONE', #67740, .T. ) ;
#39871 = DIRECTION ( 'NONE',  ( 0.000000000000000000, 1.000000000000000000, -0.000000000000000000 ) ) ;
#39872 = DIRECTION ( 'NONE',  ( -0.000000000000000000, -0.000000000000000000, -1.000000000000000000 ) ) ;
#39873 = CYLINDRICAL_SURFACE ( 'NONE', #39707, 63.00000000000000000 ) ;
#39874 = ORIENTED_EDGE ( 'NONE', *, *, #50598, .F. ) ;
#39875 = ORIENTED_EDGE ( 'NONE', *, *, #49221, .T. ) ;
#39876 = AXIS2_PLACEMENT_3D ( 'NONE', #36217, #58016, #52394 ) ;
#39877 = CARTESIAN_POINT ( 'NONE',  ( 188.2493301599116933, 87.66407108637575618, 92.74603266058126394 ) ) ;
#39878 = CARTESIAN_POINT ( 'NONE',  ( 0.3167204509598370299, 5.377136764700159333, 6.686525924292792133 ) ) ;
#39879 = FACE_OUTER_BOUND ( 'NONE', #36292, .T. ) ;
#39880 = CARTESIAN_POINT ( 'NONE',  ( 60.63507185982727066, 12.13307030573223777, -9.259813910333594578 ) ) ;
#39881 = ADVANCED_FACE ( 'NONE', ( #22121 ), #16838, .T. ) ;
#39882 = CARTESIAN_POINT ( 'NONE',  ( -55.05276343752909440, 14.68156374112638751, 30.31732777293113301 ) ) ;
#39883 = EDGE_CURVE ( 'NONE', #38638, #29482, #27388, .T. ) ;
#39884 = CARTESIAN_POINT ( 'NONE',  ( 203.1414537950835779, 105.9225671689748367, 70.89961707943172087 ) ) ;
#39885 = EDGE_CURVE ( 'NONE', #43775, #68312, #3777, .T. ) ;
#39886 = ORIENTED_EDGE ( 'NONE', *, *, #35993, .T. ) ;
#39887 = CARTESIAN_POINT ( 'NONE',  ( 10.55634918610397577, -31.11269837220809364, 0.000000000000000000 ) ) ;
#39888 = AXIS2_PLACEMENT_3D ( 'NONE', #41253, #2924, #24037 ) ;
#39889 = AXIS2_PLACEMENT_3D ( 'NONE', #18189, #40671, #29777 ) ;
#39890 = CARTESIAN_POINT ( 'NONE',  ( -61.53550548562874667, 17.56596194025585334, -65.75729484215656839 ) ) ;
#39891 = CARTESIAN_POINT ( 'NONE',  ( 197.2199569260504006, 98.22436319491369261, -70.00670125119623322 ) ) ;
#39892 = CARTESIAN_POINT ( 'NONE',  ( 275.1611065714564575, -21.96385652020510193, 1.300672318859845911 ) ) ;
#39893 = CARTESIAN_POINT ( 'NONE',  ( -165.7143741370937562, 79.24519349471960084, 10.25937150958397659 ) ) ;
#39894 = CARTESIAN_POINT ( 'NONE',  ( 111.9975424824652634, 296.0000000000000000, 529.9060149868646477 ) ) ;
#39895 = AXIS2_PLACEMENT_3D ( 'NONE', #59937, #11756, #60999 ) ;
#39896 = FACE_BOUND ( 'NONE', #40594, .T. ) ;
#39897 = CARTESIAN_POINT ( 'NONE',  ( 73.51344971438143716, -14.61114034329455258, 41.38025477438755928 ) ) ;
#39898 = CIRCLE ( 'NONE', #61237, 4.171999999999999709 ) ;
#39899 = VECTOR ( 'NONE', #49422, 1000.000000000000114 ) ;
#39900 = CARTESIAN_POINT ( 'NONE',  ( -2.355184675731021748, 6.596450510445358795, 59.32335353079142237 ) ) ;
#39901 = ORIENTED_EDGE ( 'NONE', *, *, #54213, .T. ) ;
#39902 = CARTESIAN_POINT ( 'NONE',  ( 276.0251321087873180, 21.78917327468806420, -3.050596224313125493 ) ) ;
#39903 = MANIFOLD_SOLID_BREP ( 'Cut-Extrude1', #28298 ) ;
#39904 = CARTESIAN_POINT ( 'NONE',  ( 209.3223706822284100, 0.000000000000000000, 276.7520087653757628 ) ) ;
#39905 = CARTESIAN_POINT ( 'NONE',  ( 410.0000000000000000, 190.0000000000000000, 174.3129005282752928 ) ) ;
#39906 = CARTESIAN_POINT ( 'NONE',  ( -3.769320398328897870, 0.000000000000000000, -1.941378477755967502 ) ) ;
#39907 = DIRECTION ( 'NONE',  ( -1.000000000000000000, 0.000000000000000000, 0.000000000000000000 ) ) ;
#39908 = ORIENTED_EDGE ( 'NONE', *, *, #16853, .T. ) ;
#39909 = DIRECTION ( 'NONE',  ( 1.000000000000000000, -0.000000000000000000, 0.000000000000000000 ) ) ;
#39910 = ORIENTED_EDGE ( 'NONE', *, *, #38902, .T. ) ;
#39911 = ORIENTED_EDGE ( 'NONE', *, *, #62681, .T. ) ;
#39912 = CARTESIAN_POINT ( 'NONE',  ( -7.825402957745087207, -170.0000000000000000, -16.07352014148014163 ) ) ;
#39913 = CARTESIAN_POINT ( 'NONE',  ( 153.8224167330181729, 56.12711234192239829, 43.46668491457897687 ) ) ;
#39914 = PLANE ( 'NONE',  #53753 ) ;
#39915 = ORIENTED_EDGE ( 'NONE', *, *, #65294, .T. ) ;
#39916 = CARTESIAN_POINT ( 'NONE',  ( 110.7117404013331026, 30.20916032354562120, 56.45576479620101651 ) ) ;
#39917 = CARTESIAN_POINT ( 'NONE',  ( -179.6470915626256897, 94.69856161161347075, 7.770636087711473294 ) ) ;
#39918 = CARTESIAN_POINT ( 'NONE',  ( -0.5158933718595621887, 6.525180340836104875, 12.46832194864746413 ) ) ;
#39919 = CARTESIAN_POINT ( 'NONE',  ( -81.00768240531206743, 24.30850321514431656, 30.78898729842287807 ) ) ;
#39920 = CARTESIAN_POINT ( 'NONE',  ( 91.13361825170457564, 21.00701373666980842, -37.30500766501614862 ) ) ;
#39921 = CARTESIAN_POINT ( 'NONE',  ( 311.9975424824652350, 20.00000000000003197, 256.6193948016162381 ) ) ;
#39922 = EDGE_CURVE ( 'NONE', #13679, #1714, #54459, .T. ) ;
#39923 = ORIENTED_EDGE ( 'NONE', *, *, #1597, .T. ) ;
#39925 = EDGE_CURVE ( 'NONE', #44925, #20626, #8261, .T. ) ;
#39924 = CARTESIAN_POINT ( 'NONE',  ( 444.9999999999999432, -35.00000000000000000, 2.000000000000000000 ) ) ;
#39926 = AXIS2_PLACEMENT_3D ( 'NONE', #17336, #39501, #1165 ) ;
#39927 = CARTESIAN_POINT ( 'NONE',  ( -72.78270026377323632, 21.23376443558118964, 15.75090436928392990 ) ) ;
#39928 = CARTESIAN_POINT ( 'NONE',  ( 46.85206196242846488, 9.495795933269471689, -44.11339331410427178 ) ) ;
#39929 = CARTESIAN_POINT ( 'NONE',  ( -168.0003605155415300, 83.06333427281272463, -74.54173236266500169 ) ) ;
#39931 = EDGE_LOOP ( 'NONE', ( #11144, #24312 ) ) ;
#39930 = CARTESIAN_POINT ( 'NONE',  ( -133.3755351667540481, 51.62178393940525467, 92.43199189059410514 ) ) ;
#39932 = CARTESIAN_POINT ( 'NONE',  ( 79.14129363775931836, 17.00055658855363205, -43.81460635687067651 ) ) ;
#39933 = VECTOR ( 'NONE', #51382, 999.9999999999998863 ) ;
#39934 = AXIS2_PLACEMENT_3D ( 'NONE', #64900, #43076, #38153 ) ;
#39935 = ORIENTED_EDGE ( 'NONE', *, *, #29471, .T. ) ;
#39936 = LINE ( 'NONE', #61393, #55957 ) ;
#39937 = CARTESIAN_POINT ( 'NONE',  ( 79.39764314491567632, 18.13166883367086868, 35.20801747820795669 ) ) ;
#39938 = DIRECTION ( 'NONE',  ( 1.000000000000000000, 0.000000000000000000, 0.000000000000000000 ) ) ;
#39939 = ADVANCED_FACE ( 'NONE', ( #5590 ), #11916, .F. ) ;
#39941 = CARTESIAN_POINT ( 'NONE',  ( -31.90315521289150524, 56.64813493366005304, 170.0000000000000000 ) ) ;
#39940 = AXIS2_PLACEMENT_3D ( 'NONE', #30164, #24882, #35786 ) ;
#39942 = ADVANCED_FACE ( 'NONE', ( #44627 ), #59401, .F. ) ;
#39943 = CARTESIAN_POINT ( 'NONE',  ( 141.2470358420065963, 46.06959063280893218, -15.37362590030078202 ) ) ;
#39944 = DIRECTION ( 'NONE',  ( 0.000000000000000000, -1.000000000000000000, -1.877893248421448789E-16 ) ) ;
#39945 = CARTESIAN_POINT ( 'NONE',  ( -175.9864315813574080, 91.91454246454361510, -22.31134190825564190 ) ) ;
#39946 = CIRCLE ( 'NONE', #59011, 30.00000000000000000 ) ;
#39947 = CARTESIAN_POINT ( 'NONE',  ( -47.94536219817737788, 13.92422159065987763, 35.37158188387844149 ) ) ;
#39948 = ORIENTED_EDGE ( 'NONE', *, *, #17132, .F. ) ;
#39949 = EDGE_LOOP ( 'NONE', ( #9483, #69491, #28259, #65574 ) ) ;
#39950 = ADVANCED_FACE ( 'NONE', ( #27044 ), #11552, .T. ) ;
#39951 = CARTESIAN_POINT ( 'NONE',  ( 107.0477776024378471, 27.43148174916615645, 57.16618254239813268 ) ) ;
#39952 = CARTESIAN_POINT ( 'NONE',  ( 162.0835148203877054, 61.32844276806160622, 57.82138791843907910 ) ) ;
#39953 = CARTESIAN_POINT ( 'NONE',  ( -28.30427060690108476, 69.40159203110296460, 41.38025477438755928 ) ) ;
#39954 = CARTESIAN_POINT ( 'NONE',  ( 11.98601804829804607, 14.28438006995819443, -11.98601804829804607 ) ) ;
#39955 = CARTESIAN_POINT ( 'NONE',  ( 185.1647878987786555, 82.82967084668432278, -50.03327312915156000 ) ) ;
#39956 = CARTESIAN_POINT ( 'NONE',  ( -106.6940984894957865, 35.07986071359381697, 58.78132469885891709 ) ) ;
#39957 = CARTESIAN_POINT ( 'NONE',  ( -26.49516976694650694, 8.831756547364872034, -37.15611514740469090 ) ) ;
#39958 = CARTESIAN_POINT ( 'NONE',  ( 0.000000000000000000, 50.00000000000000000, 0.000000000000000000 ) ) ;
#39959 = ORIENTED_EDGE ( 'NONE', *, *, #42105, .T. ) ;
#39960 = ORIENTED_EDGE ( 'NONE', *, *, #12616, .T. ) ;
#39961 = EDGE_LOOP ( 'NONE', ( #21409, #16363, #1319, #26688 ) ) ;
#39962 = DIRECTION ( 'NONE',  ( 0.000000000000000000, 0.000000000000000000, 1.000000000000000000 ) ) ;
#39963 = DIRECTION ( 'NONE',  ( 0.000000000000000000, 0.000000000000000000, 1.000000000000000000 ) ) ;
#39964 = DIRECTION ( 'NONE',  ( -0.000000000000000000, 1.000000000000000000, -0.000000000000000000 ) ) ;
#39965 = CARTESIAN_POINT ( 'NONE',  ( 127.4669243510812890, 38.85312661085428232, 40.96951064535277709 ) ) ;
#39966 = LINE ( 'NONE', #29078, #62530 ) ;
#39967 = CARTESIAN_POINT ( 'NONE',  ( -62.30163634902122993, 17.79682011226253380, 35.82923596446230619 ) ) ;
#39968 = DIRECTION ( 'NONE',  ( 1.000000000000000000, 0.000000000000000000, 0.000000000000000000 ) ) ;
#39969 = ADVANCED_FACE ( 'NONE', ( #54104 ), #1022, .F. ) ;
#39970 = EDGE_CURVE ( 'NONE', #66476, #23762, #24577, .T. ) ;
#39971 = CARTESIAN_POINT ( 'NONE',  ( 37.47081272996200596, 8.166145978397523209, 71.50965036819673060 ) ) ;
#39972 = CARTESIAN_POINT ( 'NONE',  ( -14.79841479960619921, -20.14961338137257840, 0.000000000000000000 ) ) ;
#39973 = ORIENTED_EDGE ( 'NONE', *, *, #69243, .T. ) ;
#39974 = CARTESIAN_POINT ( 'NONE',  ( 4.590321433069001422, -24.57496590315233931, 0.000000000000000000 ) ) ;
#39975 = CARTESIAN_POINT ( 'NONE',  ( 25.09133896793783336, 1.250000000000021982, 3.061616997868437868E-16 ) ) ;
#39977 = ADVANCED_FACE ( 'NONE', ( #12622 ), #55521, .T. ) ;
#39976 = CARTESIAN_POINT ( 'NONE',  ( -189.5325095384513645, 107.4952257375067433, -39.98148027700779750 ) ) ;
#39978 = CARTESIAN_POINT ( 'NONE',  ( -16.68907004672388084, 73.11959341363670717, 43.58025477438756212 ) ) ;
#39979 = CARTESIAN_POINT ( 'NONE',  ( 284.3366190915103857, -21.85805078441903504, -2.510101233139093502 ) ) ;
#39980 = CARTESIAN_POINT ( 'NONE',  ( 200.8410151090926661, 101.2014854111317419, 69.99904410503900465 ) ) ;
#39981 = CARTESIAN_POINT ( 'NONE',  ( 131.3924949472282719, 41.12442122814100998, -23.76614924233935611 ) ) ;
#39982 = AXIS2_PLACEMENT_3D ( 'NONE', #62945, #67891, #61567 ) ;
#39983 = ORIENTED_EDGE ( 'NONE', *, *, #18316, .F. ) ;
#39984 = CONICAL_SURFACE ( 'NONE', #36623, 8.000000000000000000, 1.047197551196600296 ) ;
#39985 = CARTESIAN_POINT ( 'NONE',  ( 129.4887940973039235, 40.01039828304090662, -37.40761579681454663 ) ) ;
#39986 = CARTESIAN_POINT ( 'NONE',  ( -128.7810612886106583, 48.42424427998342651, 4.349626167892300721 ) ) ;
#39987 = LINE ( 'NONE', #56504, #57059 ) ;
#39988 = ITEM_DEFINED_TRANSFORMATION ( 'NONE', 'NONE', #53469,  #66832 ) ;
#39989 = CARTESIAN_POINT ( 'NONE',  ( -190.6985136298601731, 109.1272424661242582, -46.56223028809779407 ) ) ;
#39990 = EDGE_LOOP ( 'NONE', ( #52110, #39180 ) ) ;
#39991 = CARTESIAN_POINT ( 'NONE',  ( -122.3745688183166180, 44.21964839958062043, -35.77374999016983281 ) ) ;
#39992 = VECTOR ( 'NONE', #65518, 1000.000000000000000 ) ;
#39993 = PRODUCT_DEFINITION_FORMATION_WITH_SPECIFIED_SOURCE ( 'ANY', '', #38327, .NOT_KNOWN. ) ;
#39994 = DIRECTION ( 'NONE',  ( -0.000000000000000000, -0.000000000000000000, -1.000000000000000000 ) ) ;
#39995 = CARTESIAN_POINT ( 'NONE',  ( 36.64089410029568228, 65.45232906116417837, 170.0000000000000000 ) ) ;
#39996 = VECTOR ( 'NONE', #11207, 1000.000000000000000 ) ;
#39997 = CARTESIAN_POINT ( 'NONE',  ( 163.6822386031149961, 63.95725419756645636, 86.38138517414357409 ) ) ;
#39998 = VERTEX_POINT ( 'NONE', #34780 ) ;
#39999 = LINE ( 'NONE', #29441, #3127 ) ;
#40000 = FACE_OUTER_BOUND ( 'NONE', #53960, .T. ) ;
#40001 = CARTESIAN_POINT ( 'NONE',  ( -153.1031717208032035, 68.63449618039560107, 31.63498310044917616 ) ) ;
#40002 = CARTESIAN_POINT ( 'NONE',  ( -4.164416015345870470, 64.86646004871185767, 170.0000000000000000 ) ) ;
#40003 = CARTESIAN_POINT ( 'NONE',  ( 84.05098130332766004, 18.55728792516086401, 17.41457137852304982 ) ) ;
#40005 = ORIENTED_EDGE ( 'NONE', *, *, #22530, .T. ) ;
#40004 = CARTESIAN_POINT ( 'NONE',  ( -58.10608953386396536, 15.52134062643865242, 4.118145803309525732 ) ) ;
#40006 = CARTESIAN_POINT ( 'NONE',  ( 55.61382797299287972, 11.07686102552914953, 36.07810415337662846 ) ) ;
#40007 = ORIENTED_EDGE ( 'NONE', *, *, #11514, .T. ) ;
#40008 = ORIENTED_EDGE ( 'NONE', *, *, #42505, .T. ) ;
#40010 = EDGE_CURVE ( 'NONE', #28072, #16942, #34123, .T. ) ;
#40009 = CARTESIAN_POINT ( 'NONE',  ( 175.8874477961784351, 74.89984466412603581, 42.23741952950327061 ) ) ;
#40011 = CARTESIAN_POINT ( 'NONE',  ( -31.86813133847536506, 10.68216487685447724, -89.01555078892404538 ) ) ;
#40013 = VERTEX_POINT ( 'NONE', #19625 ) ;
#40012 = CARTESIAN_POINT ( 'NONE',  ( 73.79471914489722906, 13.39176710989777952, 0.000000000000000000 ) ) ;
#40014 = FACE_OUTER_BOUND ( 'NONE', #36507, .T. ) ;
#40015 = MANIFOLD_SOLID_BREP ( 'Cut-Extrude1[1]', #40655 ) ;
#40016 = CARTESIAN_POINT ( 'NONE',  ( -24.60892750534350171, 9.584951112520229799, 34.60842798550392274 ) ) ;
#40017 = B_SPLINE_CURVE_WITH_KNOTS ( 'NONE', 3,
 ( #16085, #10458, #31932, #65325, #10811, #43502, #32279, #16775, #5532, #38234, #6220, #50186, #56154, #44194, #17834, #45600, #49469, #1304, #7971, #22755, #44908, #29426, #39979, #2695, #50876, #54753, #61438, #38950, #24159, #66041, #65681, #7638, #67086, #55102 ),
 .UNSPECIFIED., .F., .F.,
 ( 4, 2, 2, 2, 2, 2, 2, 2, 2, 2, 2, 2, 2, 2, 2, 2, 4 ),
 ( 0.007843851441979901237, 0.008823947846603227146, 0.009804044251226553056, 0.01078414065584987896, 0.01176423706047320487, 0.01274433346509653078, 0.01372442986971985669, 0.01470452627434318260, 0.01568462267896651025, 0.01666471908358983442, 0.01764481548821315859, 0.01862491189283648624, 0.01960500829745981388, 0.02058510470208313806, 0.02156520110670646223, 0.02254529751132978987, 0.02352539391595311752 ),
 .UNSPECIFIED. ) ;
#40018 = FACE_BOUND ( 'NONE', #2482, .T. ) ;
#40019 = EDGE_LOOP ( 'NONE', ( #54263, #61928, #63200, #37205, #25844, #46854 ) ) ;
#40020 = CARTESIAN_POINT ( 'NONE',  ( 205.5130322755755969, 109.1888880665735684, -63.17048162308527992 ) ) ;
#40021 = ADVANCED_FACE ( 'NONE', ( #7350 ), #7700, .F. ) ;
#40022 = B_SPLINE_CURVE_WITH_KNOTS ( 'NONE', 3,
 ( #63870, #53639, #16365, #535 ),
 .UNSPECIFIED., .F., .F.,
 ( 4, 4 ),
 ( 0.1259919275528361138, 0.1829744153748753543 ),
 .UNSPECIFIED. ) ;
#40023 = AXIS2_PLACEMENT_3D ( 'NONE', #52137, #41581, #25422 ) ;
#40024 = CARTESIAN_POINT ( 'NONE',  ( 136.9654665832768217, 44.52067472585215313, 43.83972285872444274 ) ) ;
#40025 = DIRECTION ( 'NONE',  ( -1.385490305291001461E-14, -1.000000000000000000, -1.110223024625132258E-16 ) ) ;
#40026 = CARTESIAN_POINT ( 'NONE',  ( -129.3970594949619795, 50.06339481638098476, 4.627477422553299746 ) ) ;
#40027 = ADVANCED_FACE ( 'NONE', ( #18589 ), #55883, .F. ) ;
#40028 = CARTESIAN_POINT ( 'NONE',  ( 22.72762739171800561, 7.830015800126070680, 67.23574744945879900 ) ) ;
#40029 = ORIENTED_EDGE ( 'NONE', *, *, #19360, .T. ) ;
#40030 = EDGE_CURVE ( 'NONE', #56454, #18878, #37453, .T. ) ;
#40031 = ORIENTED_EDGE ( 'NONE', *, *, #63782, .T. ) ;
#40032 = EDGE_LOOP ( 'NONE', ( #33576, #63367, #44175, #65950 ) ) ;
#40033 = DIRECTION ( 'NONE',  ( -0.000000000000000000, 1.000000000000000000, -0.000000000000000000 ) ) ;
#40034 = VECTOR ( 'NONE', #44918, 1000.000000000000000 ) ;
#40035 = DIRECTION ( 'NONE',  ( 0.000000000000000000, 0.000000000000000000, -1.000000000000000000 ) ) ;
#40036 = CARTESIAN_POINT ( 'NONE',  ( 48.79594039481688128, -16.97828768250229103, 26.66469066592269144 ) ) ;
#40037 = CARTESIAN_POINT ( 'NONE',  ( -96.88650755818751747, 30.12426815936638391, 86.48723326776581644 ) ) ;
#40038 = CARTESIAN_POINT ( 'NONE',  ( -17.50000000000002842, 207.5000000000000284, 0.000000000000000000 ) ) ;
#40039 = LINE ( 'NONE', #34772, #1090 ) ;
#40040 = CARTESIAN_POINT ( 'NONE',  ( 69.77839676787858991, 27.52340539440040956, 170.0000000000000000 ) ) ;
#40041 = CARTESIAN_POINT ( 'NONE',  ( -77.02112161466368434, 22.77583432622785864, -8.449775604031531273 ) ) ;
#40042 = ORIENTED_EDGE ( 'NONE', *, *, #66502, .F. ) ;
#40043 = CARTESIAN_POINT ( 'NONE',  ( -107.7677210873465867, 36.80113675102408877, 32.88384746470102016 ) ) ;
#40044 = ORIENTED_EDGE ( 'NONE', *, *, #39166, .T. ) ;
#40046 = AXIS2_PLACEMENT_3D ( 'NONE', #11303, #50351, #13071 ) ;
#40045 = CARTESIAN_POINT ( 'NONE',  ( 31.90184941268615759, 7.552181687745346927, 37.17179062719809224 ) ) ;
#40047 = SURFACE_STYLE_FILL_AREA ( #34445 ) ;
#40048 = ORIENTED_EDGE ( 'NONE', *, *, #54686, .F. ) ;
#40049 = CARTESIAN_POINT ( 'NONE',  ( 0.000000000000000000, 0.000000000000000000, 2.000000000000001776 ) ) ;
#40050 = DIRECTION ( 'NONE',  ( -0.000000000000000000, -0.5000000000000013323, -0.8660254037844379305 ) ) ;
#40051 = EDGE_CURVE ( 'NONE', #63684, #51410, #19885, .T. ) ;
#40052 = PLANE ( 'NONE',  #57225 ) ;
#40053 = CARTESIAN_POINT ( 'NONE',  ( -442.6627218934918915, 395.0000000000064801, -136.4497041420121661 ) ) ;
#40054 = CARTESIAN_POINT ( 'NONE',  ( -47.55235941796723154, 12.79790236059687558, 11.21044603464288869 ) ) ;
#40055 = CARTESIAN_POINT ( 'NONE',  ( 152.2940756559017927, 53.73566983921581652, -49.05695220847099591 ) ) ;
#40056 = EDGE_CURVE ( 'NONE', #12081, #21604, #8172, .T. ) ;
#40057 = ORIENTED_EDGE ( 'NONE', *, *, #48418, .T. ) ;
#40058 = DIRECTION ( 'NONE',  ( -0.7100673072878298520, -0.7041338076821838099, -0.000000000000000000 ) ) ;
#40059 = CARTESIAN_POINT ( 'NONE',  ( -151.2497169612548760, 65.66843968092747730, -8.119136368407126270 ) ) ;
#40060 = EDGE_LOOP ( 'NONE', ( #20872, #63405, #33413, #18555 ) ) ;
#40061 = DIRECTION ( 'NONE',  ( -0.9959742939952382912, -0.08963930890344087854, 0.000000000000000000 ) ) ;
#40062 = FACE_OUTER_BOUND ( 'NONE', #64147, .T. ) ;
#40064 = ADVANCED_FACE ( 'NONE', ( #26294 ), #69527, .F. ) ;
#40063 = DIRECTION ( 'NONE',  ( -0.000000000000000000, -0.000000000000000000, -1.000000000000000000 ) ) ;
#40065 = ORIENTED_EDGE ( 'NONE', *, *, #40758, .T. ) ;
#40066 = DIRECTION ( 'NONE',  ( -1.000000000000000000, -1.001918046209079887E-14, 9.729495617646301779E-15 ) ) ;
#40067 = CARTESIAN_POINT ( 'NONE',  ( 153.8224167330181729, 56.12711234192239829, -63.91151744727573458 ) ) ;
#40068 = CARTESIAN_POINT ( 'NONE',  ( -37.07602570886409410, 10.58457435034603300, 32.74454515178810965 ) ) ;
#40069 = CARTESIAN_POINT ( 'NONE',  ( 140.8984307802396643, 45.84194788389000763, -46.15581894915797534 ) ) ;
#40070 = EDGE_LOOP ( 'NONE', ( #31217, #60907, #14773, #40203, #47344, #68678, #44904, #58827, #62545 ) ) ;
#40071 =( NAMED_UNIT ( * ) PLANE_ANGLE_UNIT ( ) SI_UNIT ( $, .RADIAN. ) );
#40072 = LINE ( 'NONE', #64451, #49766 ) ;
#40073 = CARTESIAN_POINT ( 'NONE',  ( -119.2982054035570911, 42.30181775808006250, 34.54033407936248068 ) ) ;
#40074 = ORIENTED_EDGE ( 'NONE', *, *, #23531, .T. ) ;
#40075 = CARTESIAN_POINT ( 'NONE',  ( 32.30062460741315533, 8.603096374765343057, -18.70062496153113685 ) ) ;
#40076 = CARTESIAN_POINT ( 'NONE',  ( 183.1865184929770862, 80.75677158533827082, 2.761582280813896340 ) ) ;
#40077 = CARTESIAN_POINT ( 'NONE',  ( 89.87518614971251907, 20.55373388674512469, 57.27852128848381597 ) ) ;
#40078 = PRODUCT_DEFINITION_SHAPE ( 'NONE', 'NONE',  #69605 ) ;
#40079 = DIRECTION ( 'NONE',  ( -0.000000000000000000, 0.000000000000000000, -1.000000000000000000 ) ) ;
#40080 =( NAMED_UNIT ( * ) PLANE_ANGLE_UNIT ( ) SI_UNIT ( $, .RADIAN. ) );
#40081 = VECTOR ( 'NONE', #41597, 1000.000000000000000 ) ;
#40082 = B_SPLINE_CURVE_WITH_KNOTS ( 'NONE', 3,
 ( #60707, #66012, #59644, #60365, #28348, #27995, #577, #43816, #23083, #27296, #49792, #11458, #22028, #12523, #50156, #49440, #38918, #48736, #22727, #43470, #64950, #17441, #55424, #33296, #16745, #44164, #11820, #23442, #38203, #1619, #27647, #44881, #65290, #18152, #6892, #1984, #39263, #12181, #17809, #33644, #44532, #32927, #49088, #7250, #66362 ),
 .UNSPECIFIED., .F., .F.,
 ( 4, 2, 2, 2, 2, 2, 2, 2, 2, 2, 2, 2, 2, 1, 2, 2, 2, 2, 2, 2, 2, 2, 4 ),
 ( 0.02352719711393055912, 0.02499986300757017083, 0.02573619595438998708, 0.02647252890120980334, 0.02794519479484943586, 0.02941786068848907185, 0.03015419363530889157, 0.03089052658212870783, 0.03236319247576834035, 0.03309952542258814273, 0.03383585836940794511, 0.03530852426304757763, 0.03604485720986738695, 0.03678119015668719627, 0.03751752310350699865, 0.03825385605032680103, 0.03972652194396641273, 0.04119918783760602443, 0.04267185373124562919, 0.04340818667806543851, 0.04414451962488524783, 0.04561718551852484566, 0.04708985141216444348 ),
 .UNSPECIFIED. ) ;
#40083 = CYLINDRICAL_SURFACE ( 'NONE', #59344, 25.00000000000395772 ) ;
#40084 = EDGE_LOOP ( 'NONE', ( #63627, #31085, #53722, #31103 ) ) ;
#40085 = CARTESIAN_POINT ( 'NONE',  ( 162.7921669283191193, 61.91024532638674316, -22.07005389488237057 ) ) ;
#40086 = PLANE ( 'NONE',  #45207 ) ;
#40087 = VECTOR ( 'NONE', #58304, 1000.000000000000000 ) ;
#40088 = CARTESIAN_POINT ( 'NONE',  ( 68.95451040317567504, 14.12887482153123386, 68.76426114867949480 ) ) ;
#40089 = CARTESIAN_POINT ( 'NONE',  ( 141.2801018238827169, 47.29457739955284978, 11.26812789576816876 ) ) ;
#40090 = CARTESIAN_POINT ( 'NONE',  ( 7.762887554996211747E-14, 46.66904755831208718, 0.000000000000000000 ) ) ;
#40091 = CONICAL_SURFACE ( 'NONE', #25490, 74.95140232871122521, 0.8777644062502172329 ) ;
#40092 = ORIENTED_EDGE ( 'NONE', *, *, #52807, .T. ) ;
#40093 = AXIS2_PLACEMENT_3D ( 'NONE', #17005, #6472, #140 ) ;
#40094 = EDGE_CURVE ( 'NONE', #30890, #19565, #14691, .T. ) ;
#40095 = DIRECTION ( 'NONE',  ( 0.000000000000000000, 0.000000000000000000, 1.000000000000000000 ) ) ;
#40096 = CARTESIAN_POINT ( 'NONE',  ( 10.13846145460683701, 6.385368868491634764, 42.47142630253362228 ) ) ;
#40097 = ORIENTED_EDGE ( 'NONE', *, *, #38124, .F. ) ;
#40098 = VECTOR ( 'NONE', #5233, 1000.000000000000000 ) ;
#40100 = ADVANCED_FACE ( 'NONE', ( #47048 ), #4488, .T. ) ;
#40099 = CARTESIAN_POINT ( 'NONE',  ( 63.49941241090381538, 13.81848793187418600, 56.65751152968498161 ) ) ;
#40101 = CARTESIAN_POINT ( 'NONE',  ( 130.2154003102709225, 39.26869728108905377, -90.64406281561510070 ) ) ;
#40102 = ORIENTED_EDGE ( 'NONE', *, *, #45999, .F. ) ;
#40103 = CARTESIAN_POINT ( 'NONE',  ( 162.8034185388970627, 63.22443559329413176, -48.91927988040787056 ) ) ;
#40104 = DIRECTION ( 'NONE',  ( -1.000000000000000000, 0.000000000000000000, 0.000000000000000000 ) ) ;
#40105 = CYLINDRICAL_SURFACE ( 'NONE', #5688, 10.00000000000000000 ) ;
#40106 = DIRECTION ( 'NONE',  ( -0.000000000000000000, -0.000000000000000000, 1.000000000000000000 ) ) ;
#40107 = ORIENTED_EDGE ( 'NONE', *, *, #14208, .T. ) ;
#40108 = CARTESIAN_POINT ( 'NONE',  ( -99.98584758882478241, 32.75338129098886952, 4.018470313552430895 ) ) ;
#40109 = CARTESIAN_POINT ( 'NONE',  ( 66.50978889550178508, 14.54692747110987483, 84.35750253269495147 ) ) ;
#40110 = CARTESIAN_POINT ( 'NONE',  ( 151.2878525843655666, 54.24529526600250051, -93.06221793583787871 ) ) ;
#40111 = CARTESIAN_POINT ( 'NONE',  ( 86.62931800182292363, 20.48449268398422163, -8.977013608448025650 ) ) ;
#40112 = CARTESIAN_POINT ( 'NONE',  ( -165.7689197919845014, 79.30072199592278537, 39.83247271659003985 ) ) ;
#40113 = CARTESIAN_POINT ( 'NONE',  ( 33.57125916965274115, 8.734028988681728833, -92.01757106967839661 ) ) ;
#40114 = EDGE_CURVE ( 'NONE', #59570, #47824, #19983, .T. ) ;
#40115 = CYLINDRICAL_SURFACE ( 'NONE', #51847, 7.500000000000020428 ) ;
#40116 = VERTEX_POINT ( 'NONE', #15730 ) ;
#40117 = CARTESIAN_POINT ( 'NONE',  ( -49.42000000000000171, -36.09918303830819752, 10.41169613715280740 ) ) ;
#40119 = ADVANCED_FACE ( 'NONE', ( #63233 ), #38573, .T. ) ;
#40118 = LINE ( 'NONE', #56636, #34438 ) ;
#40120 = ORIENTED_EDGE ( 'NONE', *, *, #43245, .T. ) ;
#40121 = CYLINDRICAL_SURFACE ( 'NONE', #11500, 7.500000000000013323 ) ;
#40122 = CARTESIAN_POINT ( 'NONE',  ( 210.9608386442062624, 117.1762372255315654, -12.84724971893104062 ) ) ;
#40123 = CARTESIAN_POINT ( 'NONE',  ( 9.850262805259839993, 188.0000000000000000, -1.724042536399416070 ) ) ;
#40124 = DIRECTION ( 'NONE',  ( 0.8090169943749506709, -0.5877852522924686962, 0.000000000000000000 ) ) ;
#40125 = AXIS2_PLACEMENT_3D ( 'NONE', #16459, #53729, #6244 ) ;
#40126 = CARTESIAN_POINT ( 'NONE',  ( -9.914178172705819136, 7.035763242673981566, -89.39128270836016554 ) ) ;
#40127 = CARTESIAN_POINT ( 'NONE',  ( 0.000000000000000000, 0.000000000000000000, 73.58025477438756923 ) ) ;
#40128 = FACE_OUTER_BOUND ( 'NONE', #66244, .T. ) ;
#40129 = FACE_OUTER_BOUND ( 'NONE', #51563, .T. ) ;
#40130 = CARTESIAN_POINT ( 'NONE',  ( -56.02027488966933788, 14.94257193099085868, 18.42563833103987392 ) ) ;
#40131 = ORIENTED_EDGE ( 'NONE', *, *, #59715, .T. ) ;
#40132 = VECTOR ( 'NONE', #44724, 1000.000000000000000 ) ;
#40133 = CARTESIAN_POINT ( 'NONE',  ( -100.4347360276019145, 32.97716872911834685, -49.79891040578767303 ) ) ;
#40134 = VERTEX_POINT ( 'NONE', #10442 ) ;
#40135 = CARTESIAN_POINT ( 'NONE',  ( 0.000000000000000000, 0.000000000000000000, 43.58025477438756212 ) ) ;
#40136 = DIRECTION ( 'NONE',  ( -0.000000000000000000, -1.000000000000000000, -0.000000000000000000 ) ) ;
#40137 = AXIS2_PLACEMENT_3D ( 'NONE', #46191, #40925, #29678 ) ;
#40138 = CARTESIAN_POINT ( 'NONE',  ( 445.3372781065085633, 217.8591479523844612, -111.4497041420119388 ) ) ;
#40139 = FACE_OUTER_BOUND ( 'NONE', #55336, .T. ) ;
#40140 = MANIFOLD_SOLID_BREP ( 'Angle iron 35 X 35 X 5(2)', #45174 ) ;
#40141 = CARTESIAN_POINT ( 'NONE',  ( -15.32732096506169661, 7.496199110535271437, 91.58149418733879088 ) ) ;
#40142 = LINE ( 'NONE', #33822, #15341 ) ;
#40144 = VECTOR ( 'NONE', #14446, 1000.000000000000000 ) ;
#40143 = CARTESIAN_POINT ( 'NONE',  ( 200.0000000000000000, 2.999999999999969802, -46.99999999999997158 ) ) ;
#40145 = DIRECTION ( 'NONE',  ( 2.477416674922665047E-16, -3.355888904727913208E-17, 1.000000000000000000 ) ) ;
#40146 = ORIENTED_EDGE ( 'NONE', *, *, #64810, .T. ) ;
#40147 = EDGE_LOOP ( 'NONE', ( #58011, #43051 ) ) ;
#40148 = CARTESIAN_POINT ( 'NONE',  ( -31.11269837220809364, -15.55634918610397754, 2.000000000000001776 ) ) ;
#40149 = FACE_OUTER_BOUND ( 'NONE', #15597, .T. ) ;
#40150 = CARTESIAN_POINT ( 'NONE',  ( -25.99999999999999289, 0.000000000000000000, -33.00000000000000000 ) ) ;
#40151 = B_SPLINE_CURVE_WITH_KNOTS ( 'NONE', 3,
 ( #68147, #51613, #9393, #56896, #36468, #18912, #9740, #46319, #30852, #19594, #19955, #31203, #52298, #25234, #62154, #3423, #3764, #47022, #35083, #41057, #40696, #20285, #52635, #14662, #24198, #45984, #36124, #46672, #19242, #45641, #40358, #61806, #4117, #56535, #13974, #35436, #63205, #8363, #8712, #68478, #29811, #41744, #51273, #62517, #14329, #57235, #9050, #59289 ),
 .UNSPECIFIED., .F., .F.,
 ( 4, 2, 2, 2, 2, 2, 2, 2, 2, 2, 2, 2, 2, 2, 2, 2, 2, 2, 2, 2, 2, 2, 2, 4 ),
 ( 0.02554216173022670275, 0.02715505844859215229, 0.02796150680777490655, 0.02876795516695766428, 0.03038085188532323178, 0.03199374860368880275, 0.03360664532205437371, 0.03441309368123716267, 0.03521954204041995162, 0.03602599039960274058, 0.03683243875878554341, 0.03844533547715116295, 0.03925178383633396578, 0.04005823219551677555, 0.04086468055469958532, 0.04167112891388238816, 0.04247757727306519793, 0.04328402563224800770, 0.04489692235061367581, 0.04650981906897934393, 0.04731626742816219533, 0.04812271578734504673, 0.04973561250571066628, 0.05134850922407628582 ),
 .UNSPECIFIED. ) ;
#40152 = CARTESIAN_POINT ( 'NONE',  ( 106.6181401479172308, 28.34160787025144046, 70.52598296703905589 ) ) ;
#40153 = CIRCLE ( 'NONE', #37878, 246.3582898394606957 ) ;
#40154 = CARTESIAN_POINT ( 'NONE',  ( -51.66904755831210139, 6.635317295611287136E-14, 2.000000000000001776 ) ) ;
#40155 = CARTESIAN_POINT ( 'NONE',  ( 58.46823952472684027, 12.69204591816732730, -10.39183658609108996 ) ) ;
#40156 = VERTEX_POINT ( 'NONE', #11136 ) ;
#40157 = CARTESIAN_POINT ( 'NONE',  ( 109.3047140914111850, 29.55674059952507093, -35.96634199548729072 ) ) ;
#40158 = CARTESIAN_POINT ( 'NONE',  ( -31.43908319763710679, 10.61114334766716283, -8.472646774738153752 ) ) ;
#40159 = LINE ( 'NONE', #1841, #32701 ) ;
#40160 = LINE ( 'NONE', #28203, #344 ) ;
#40161 = FACE_BOUND ( 'NONE', #33463, .T. ) ;
#40162 = ORIENTED_EDGE ( 'NONE', *, *, #35882, .F. ) ;
#40163 = DIRECTION ( 'NONE',  ( 0.1342332658176667304, -0.9909497617679331460, 0.000000000000000000 ) ) ;
#40164 = DIRECTION ( 'NONE',  ( -0.000000000000000000, -0.000000000000000000, -1.000000000000000000 ) ) ;
#40165 = CARTESIAN_POINT ( 'NONE',  ( 34.83823433017388993, 8.871835168107978120, -75.93650321438980200 ) ) ;
#40166 = CARTESIAN_POINT ( 'NONE',  ( -180.5801285865471186, 97.42945596116098272, 10.67803447139740491 ) ) ;
#40167 = CARTESIAN_POINT ( 'NONE',  ( 211.5034924207027700, 118.0100795718634856, 66.71809058681080273 ) ) ;
#40168 = CARTESIAN_POINT ( 'NONE',  ( 86.15410276028859471, 19.25894675708890347, -77.66611478937541335 ) ) ;
#40169 = EDGE_CURVE ( 'NONE', #14795, #5765, #48070, .T. ) ;
#40170 = AXIS2_PLACEMENT_3D ( 'NONE', #17221, #69311, #58738 ) ;
#40171 = ORIENTED_EDGE ( 'NONE', *, *, #66424, .F. ) ;
#40172 = DIRECTION ( 'NONE',  ( 0.000000000000000000, 0.000000000000000000, 1.000000000000000000 ) ) ;
#40173 = CARTESIAN_POINT ( 'NONE',  ( 197.8598785550297521, 99.02620879292953759, -46.92193452575618551 ) ) ;
#40174 = EDGE_CURVE ( 'NONE', #36497, #43728, #22042, .T. ) ;
#40175 = VERTEX_POINT ( 'NONE', #232 ) ;
#40177 = DIRECTION ( 'NONE',  ( -0.000000000000000000, 1.000000000000000000, -0.000000000000000000 ) ) ;
#40176 = AXIS2_PLACEMENT_3D ( 'NONE', #65673, #22400, #6571 ) ;
#40178 = ORIENTED_EDGE ( 'NONE', *, *, #7256, .F. ) ;
#40179 = CARTESIAN_POINT ( 'NONE',  ( -83.12901536265223967, 24.07178615860086168, -63.42720624446700128 ) ) ;
#40180 = CARTESIAN_POINT ( 'NONE',  ( -62.41727141396690826, 17.83188754031768752, -14.38874286553851611 ) ) ;
#40181 = ADVANCED_FACE ( 'NONE', ( #48754 ), #59660, .F. ) ;
#40182 = B_SPLINE_CURVE_WITH_KNOTS ( 'NONE', 3,
 ( #65092, #17602, #6349, #39065, #60510, #59795, #34140, #23242, #43267, #33446, #54162, #27802, #11975, #49240, #6697, #17955, #12326, #38006, #33785, #11266, #48883, #1075, #66163, #16551, #22525, #28143, #729, #55224, #17239, #60853, #50311, #64747, #55577, #5986, #1779, #7042, #49588, #43967, #65446, #28505, #7406, #28861, #22179, #59453, #13036, #35519 ),
 .UNSPECIFIED., .F., .F.,
 ( 4, 2, 2, 2, 2, 2, 2, 2, 2, 2, 2, 2, 2, 2, 2, 2, 2, 2, 2, 2, 2, 2, 4 ),
 ( 0.02404638330965502141, 0.02555608299537558831, 0.02631093283823587523, 0.02706578268109615867, 0.02857548236681672904, 0.02933033220967700902, 0.03008518205253728900, 0.03159488173825784896, 0.03310458142397840892, 0.03385943126683869236, 0.03461428110969896887, 0.03612398079541952189, 0.03687883063827980534, 0.03763368048114007491, 0.03838853032400035142, 0.03914338016686062793, 0.04065307985258118095, 0.04216277953830172703, 0.04367247922402228699, 0.04518217890974284001, 0.04593702875260310958, 0.04669187859546338609, 0.04820157828118393911 ),
 .UNSPECIFIED. ) ;
#40183 = CARTESIAN_POINT ( 'NONE',  ( 92.53033045403536505, 22.59263332688196257, -74.82145947628868043 ) ) ;
#40184 = ORIENTED_EDGE ( 'NONE', *, *, #413, .T. ) ;
#40185 = VECTOR ( 'NONE', #23730, 1000.000000000000000 ) ;
#40186 = EDGE_CURVE ( 'NONE', #65701, #25560, #32994, .T. ) ;
#40187 = EDGE_LOOP ( 'NONE', ( #30168, #46137, #10530, #64349 ) ) ;
#40188 = DIRECTION ( 'NONE',  ( 0.000000000000000000, 0.000000000000000000, 1.000000000000000000 ) ) ;
#40189 = CARTESIAN_POINT ( 'NONE',  ( -109.4874964445488104, 37.74487348321786584, -94.07812955749422201 ) ) ;
#40190 = VECTOR ( 'NONE', #20531, 1000.000000000000000 ) ;
#40191 = DIRECTION ( 'NONE',  ( -1.000000000000000000, 0.000000000000000000, 0.000000000000000000 ) ) ;
#40192 = ORIENTED_EDGE ( 'NONE', *, *, #17513, .T. ) ;
#40193 = DIRECTION ( 'NONE',  ( 0.000000000000000000, 0.000000000000000000, 1.000000000000000000 ) ) ;
#40194 = AXIS2_PLACEMENT_3D ( 'NONE', #43472, #33298, #21678 ) ;
#40195 = CARTESIAN_POINT ( 'NONE',  ( -48.71337292867760027, 14.10768470390589435, 14.98814739561979437 ) ) ;
#40196 = CARTESIAN_POINT ( 'NONE',  ( -132.2286325684322037, 52.04087929935079870, -11.54593800350672872 ) ) ;
#40197 = ADVANCED_FACE ( 'NONE', ( #49102 ), #43124, .T. ) ;
#40198 = CARTESIAN_POINT ( 'NONE',  ( -46.66904755831210139, 6.635317295611287136E-14, 85.00100000000000477 ) ) ;
#40199 = CARTESIAN_POINT ( 'NONE',  ( 79.13041963748372609, 18.04952109592810672, -43.84177388801760600 ) ) ;
#40201 = ORIENTED_EDGE ( 'NONE', *, *, #33376, .T. ) ;
#40200 = CARTESIAN_POINT ( 'NONE',  ( -173.1211646369891355, -170.0000000000000000, 65.16624519710472896 ) ) ;
#40202 = ORIENTED_EDGE ( 'NONE', *, *, #30751, .T. ) ;
#40203 = ORIENTED_EDGE ( 'NONE', *, *, #61493, .T. ) ;
#40204 = DIRECTION ( 'NONE',  ( 0.000000000000000000, 0.000000000000000000, 1.000000000000000000 ) ) ;
#40205 = CARTESIAN_POINT ( 'NONE',  ( 74.94097818310312675, -1.250000000000021760, 41.38025477438755928 ) ) ;
#40206 = CARTESIAN_POINT ( 'NONE',  ( 117.4396227366912626, 33.48307633470226818, -95.00000000000133582 ) ) ;
#40207 = CARTESIAN_POINT ( 'NONE',  ( 11.05669727962759907, 70.00000000000000000, -27.88815958909220782 ) ) ;
#40208 = CARTESIAN_POINT ( 'NONE',  ( 197.2200752504830632, 96.62072041958359137, 10.52740617786156463 ) ) ;
#40209 = DIRECTION ( 'NONE',  ( 0.000000000000000000, 0.000000000000000000, 1.000000000000000000 ) ) ;
#40210 = CARTESIAN_POINT ( 'NONE',  ( 212.0690325386321433, 118.8871691880494836, 88.99556113406791269 ) ) ;
#40211 = CARTESIAN_POINT ( 'NONE',  ( 0.000000000000000000, 0.000000000000000000, 0.000000000000000000 ) ) ;
#40212 = CARTESIAN_POINT ( 'NONE',  ( -82.93126516400698733, 25.07709093823495650, 58.58861024883177038 ) ) ;
#40213 = CARTESIAN_POINT ( 'NONE',  ( 417.3372781065085633, 400.0000000000000568, -141.4497041420118251 ) ) ;
#40214 = ORIENTED_EDGE ( 'NONE', *, *, #35580, .T. ) ;
#40215 = DIRECTION ( 'NONE',  ( 0.000000000000000000, 0.000000000000000000, 1.000000000000000000 ) ) ;
#40216 = ORIENTED_EDGE ( 'NONE', *, *, #27399, .T. ) ;
#40217 = ORIENTED_EDGE ( 'NONE', *, *, #67129, .F. ) ;
#40218 = LINE ( 'NONE', #13485, #46656 ) ;
#40219 = CARTESIAN_POINT ( 'NONE',  ( -15.55634918610400597, 15.55634918610405748, 0.000000000000000000 ) ) ;
#40220 = CARTESIAN_POINT ( 'NONE',  ( -31.13302211571334155, 10.56067280572192146, 83.90492538947324874 ) ) ;
#40221 = CARTESIAN_POINT ( 'NONE',  ( -101.3492134984965389, 32.31003911421601771, -35.05777063899205359 ) ) ;
#40222 = DIRECTION ( 'NONE',  ( 1.000000000000000000, 0.000000000000000000, 0.000000000000000000 ) ) ;
#40224 = FACE_OUTER_BOUND ( 'NONE', #21940, .T. ) ;
#40223 = CIRCLE ( 'NONE', #61562, 5.000000000000004441 ) ;
#40225 = CARTESIAN_POINT ( 'NONE',  ( 8.763528846667099970, 7.383598436776582119, -40.38010197442696381 ) ) ;
#40226 = CARTESIAN_POINT ( 'NONE',  ( 126.5710838895481629, 37.19597237024176906, -45.32323354818519334 ) ) ;
#40227 = ORIENTED_EDGE ( 'NONE', *, *, #64054, .T. ) ;
#40228 = VERTEX_POINT ( 'NONE', #6910 ) ;
#40229 = AXIS2_PLACEMENT_3D ( 'NONE', #45428, #12731, #29257 ) ;
#40230 = CARTESIAN_POINT ( 'NONE',  ( 188.3911424972466193, 87.82183351239343949, 88.76307796285202301 ) ) ;
#40231 = CARTESIAN_POINT ( 'NONE',  ( -17.90772993695113868, 72.84144224619130625, 170.0000000000000000 ) ) ;
#40232 = CARTESIAN_POINT ( 'NONE',  ( -452.6627218934858661, 400.0000000000064801, -116.4497041420121377 ) ) ;
#40233 = CARTESIAN_POINT ( 'NONE',  ( -24.33435124463267130, 8.532637995283112176, -67.24644030340769518 ) ) ;
#40234 = VECTOR ( 'NONE', #2451, 1000.000000000000000 ) ;
#40235 = UNCERTAINTY_MEASURE_WITH_UNIT (LENGTH_MEASURE( 1.000000000000000082E-05 ), #47079, 'distance_accuracy_value', 'NONE');
#40236 = CARTESIAN_POINT ( 'NONE',  ( 11.21387192505586405, 6.397095920409661574, 4.706635521921354481 ) ) ;
#40237 = ORIENTED_EDGE ( 'NONE', *, *, #53979, .F. ) ;
#40238 = CIRCLE ( 'NONE', #52580, 35.00000000000000000 ) ;
#40239 = CARTESIAN_POINT ( 'NONE',  ( 41.34269507549201705, 9.685203600174695282, -77.22535371806525006 ) ) ;
#40240 = CARTESIAN_POINT ( 'NONE',  ( -60.95805269991218722, 17.39401718769329719, -74.19099977899746534 ) ) ;
#40241 = CARTESIAN_POINT ( 'NONE',  ( 197.3064269725219049, 98.33232022113060111, -69.35658200132850482 ) ) ;
#40242 = SHAPE_REPRESENTATION_RELATIONSHIP ( 'NONE' , 'NONE' ,  #7414, #56683 ) ;
#40243 = ADVANCED_FACE ( 'NONE', ( #54028 ), #28011, .T. ) ;
#40244 = CARTESIAN_POINT ( 'NONE',  ( 277.4937869665631069, -21.56868463414005177, -4.338918127843128580 ) ) ;
#40245 = CARTESIAN_POINT ( 'NONE',  ( -173.1211646369891071, 87.12891641440859303, 3.977144016177345254 ) ) ;
#40246 = CARTESIAN_POINT ( 'NONE',  ( 64.52696037203368462, -10.43950074664762262, 3.125053320693559764E-16 ) ) ;
#40247 = CARTESIAN_POINT ( 'NONE',  ( -55.05276343752909440, 14.68156374112638929, 57.16187836339483397 ) ) ;
#40248 = AXIS2_PLACEMENT_3D ( 'NONE', #6385, #37342, #32080 ) ;
#40249 = CARTESIAN_POINT ( 'NONE',  ( -0.5183605925911988210, 6.525266619725955231, 62.75222543575570455 ) ) ;
#40250 = ORIENTED_EDGE ( 'NONE', *, *, #51153, .F. ) ;
#40251 = CARTESIAN_POINT ( 'NONE',  ( 275.0001309909290512, 21.99997022933651891, 0.3293293811575784269 ) ) ;
#40252 = CARTESIAN_POINT ( 'NONE',  ( 150.0516754638056227, 53.34587188591231666, 62.61862363090603623 ) ) ;
#40253 = DIRECTION ( 'NONE',  ( 0.000000000000000000, 1.000000000000000000, 0.000000000000000000 ) ) ;
#40254 = CARTESIAN_POINT ( 'NONE',  ( -24.75616454008743972, 3.483147608716851806, 0.000000000000000000 ) ) ;
#40255 = LINE ( 'NONE', #50114, #65912 ) ;
#40256 = VERTEX_POINT ( 'NONE', #11474 ) ;
#40257 = DIRECTION ( 'NONE',  ( 0.000000000000000000, 0.000000000000000000, -1.000000000000000000 ) ) ;
#40258 = EDGE_CURVE ( 'NONE', #43258, #54206, #14888, .T. ) ;
#40259 = ORIENTED_EDGE ( 'NONE', *, *, #28925, .F. ) ;
#40260 = VERTEX_POINT ( 'NONE', #37879 ) ;
#40261 = DIRECTION ( 'NONE',  ( 0.000000000000000000, 1.000000000000000000, 0.000000000000000000 ) ) ;
#40262 = CARTESIAN_POINT ( 'NONE',  ( 152.8672128926848757, 55.41186463791521533, 30.98344588502664365 ) ) ;
#40263 = CARTESIAN_POINT ( 'NONE',  ( 311.8713128290285113, 2.000000000000001776, 346.5826552340383842 ) ) ;
#40264 = ORIENTED_EDGE ( 'NONE', *, *, #6902, .F. ) ;
#40265 = LINE ( 'NONE', #56435, #58144 ) ;
#40266 = CARTESIAN_POINT ( 'NONE',  ( -178.0658882571759989, 92.80593104957416983, 5.833208099788561363 ) ) ;
#40267 = DIRECTION ( 'NONE',  ( 0.000000000000000000, 0.000000000000000000, 1.000000000000000000 ) ) ;
#40268 = EDGE_CURVE ( 'NONE', #52035, #9829, #11510, .T. ) ;
#40269 = CARTESIAN_POINT ( 'NONE',  ( 55.77012379229939398, 12.13428856597101202, -41.26774091221908236 ) ) ;
#40270 = CARTESIAN_POINT ( 'NONE',  ( -85.10909119100207931, 25.97025675005452428, 34.04615563038053949 ) ) ;
#40271 = CARTESIAN_POINT ( 'NONE',  ( -27.70185240367226953, 10.02491413133431308, -22.47982293096844941 ) ) ;
#40272 = CARTESIAN_POINT ( 'NONE',  ( 134.3159642998340360, 41.70198410084977780, 2.665790248531664908 ) ) ;
#40273 = VERTEX_POINT ( 'NONE', #24496 ) ;
#40275 = B_SPLINE_CURVE_WITH_KNOTS ( 'NONE', 3,
 ( #67322, #62724, #9253, #7873, #34953, #19814, #57097, #66978, #29323, #61333, #18771, #52160, #51479, #68348, #35987, #40916, #24052, #3290, #51128, #24405, #8914, #45491, #61675, #40226, #29667, #57442, #13494, #56397, #67656, #24748, #30711, #19453, #8219, #3623, #8572, #30019, #3978, #2943, #45846, #19108, #62374, #25449, #40562, #62014, #13155, #56057 ),
 .UNSPECIFIED., .F., .F.,
 ( 4, 2, 2, 2, 2, 2, 2, 2, 2, 2, 2, 2, 2, 2, 2, 2, 2, 2, 2, 2, 2, 2, 4 ),
 ( 3.179800655392250756E-17, 0.001572224531395693828, 0.003144449062791355564, 0.004716673594187017517, 0.006288898125582679903, 0.007861122656978341422, 0.009433347188374002074, 0.01021945945407182026, 0.01100557171976963497, 0.01179168398546745315, 0.01257779625116526960, 0.01415002078256088341, 0.01493613304825867037, 0.01572224531395645733, 0.01650835757965424949, 0.01729446984535203818, 0.01886669437674766067, 0.01965280664244547365, 0.02043891890814329010, 0.02201114343953891606, 0.02358336797093454548, 0.02436948023663238969, 0.02515559250233023042 ),
 .UNSPECIFIED. ) ;
#40274 = SHAPE_REPRESENTATION ( 'MAT-053', ( #2942, #34331, #12993, #43273, #7412, #53415, #57915, #62440, #52289, #32107, #20856, #42195, #1785, #2889, #66925, #21950, #33217, #61280, #6237, #45560, #11864, #36581, #15237, #54521, #24242, #28797, #61332, #66977, #51251, #13040, #63591, #15286, #17531, #31010, #65872, #27623, #16434, #19812, #20905, #664, #34433, #47854, #33267, #48946, #64738, #7469, #53469, #9668, #22004, #42247, #60221, #29898, #45617, #56872, #26529, #1845, #59099, #50136, #54586, #35524, #8571 ), #44506 ) ;
#40276 = VECTOR ( 'NONE', #10822, 1000.000000000000000 ) ;
#40277 = DIRECTION ( 'NONE',  ( -0.7100673072878298520, -0.7041338076821838099, -0.000000000000000000 ) ) ;
#40278 = FACE_OUTER_BOUND ( 'NONE', #67348, .T. ) ;
#40279 = ADVANCED_FACE ( 'NONE', ( #34703 ), #18513, .F. ) ;
#40280 = CARTESIAN_POINT ( 'NONE',  ( 46.50704915687941821, 9.440294391580033917, -40.70557485162431988 ) ) ;
#40281 = AXIS2_PLACEMENT_3D ( 'NONE', #59607, #33609, #11781 ) ;
#40282 = CARTESIAN_POINT ( 'NONE',  ( 6.800000000000000711, 6.613092715395708453E-16, 5.400000000000001243 ) ) ;
#40284 = VERTEX_POINT ( 'NONE', #3033 ) ;
#40283 = CARTESIAN_POINT ( 'NONE',  ( 204.6977192012829789, -170.0000000000000000, -97.51503221354896311 ) ) ;
#40285 = CARTESIAN_POINT ( 'NONE',  ( 79.38459371357853911, 17.07499996355401706, -41.31674572369035303 ) ) ;
#40286 = ADVANCED_FACE ( 'NONE', ( #8307 ), #6069, .T. ) ;
#40287 = VERTEX_POINT ( 'NONE', #39278 ) ;
#40288 = CARTESIAN_POINT ( 'NONE',  ( -142.0685766576042113, 58.11789490499571542, 66.17456823166700985 ) ) ;
#40289 = CARTESIAN_POINT ( 'NONE',  ( 26.69682282325707945, 59.27986298182226221, 170.0000000000000000 ) ) ;
#40290 = LINE ( 'NONE', #1608, #60150 ) ;
#40291 = CARTESIAN_POINT ( 'NONE',  ( 187.9007786055418023, 85.78077355327275200, -13.74105984729973251 ) ) ;
#40292 = CARTESIAN_POINT ( 'NONE',  ( 140.8984307802396927, 45.84194788389002184, -19.31126835869425662 ) ) ;
#40293 = CARTESIAN_POINT ( 'NONE',  ( -84.21836162213168109, 25.60181819557223548, -20.83666508763759140 ) ) ;
#40294 = CARTESIAN_POINT ( 'NONE',  ( -177.5100621450480389, 93.70693725195823731, -21.46705021681216863 ) ) ;
#40295 = CARTESIAN_POINT ( 'NONE',  ( -49.43836229152577033, 14.28302414152159727, 32.81988602651634324 ) ) ;
#40296 = ORIENTED_EDGE ( 'NONE', *, *, #18646, .T. ) ;
#40297 = ORIENTED_EDGE ( 'NONE', *, *, #56822, .F. ) ;
#40298 = CARTESIAN_POINT ( 'NONE',  ( 103.1567541746301373, 25.73937982110321343, 61.44734176770268874 ) ) ;
#40299 = LINE ( 'NONE', #56126, #52586 ) ;
#40300 = CARTESIAN_POINT ( 'NONE',  ( -30.62628708973392122, 68.47330165179127448, 43.58025477438756923 ) ) ;
#40301 = CARTESIAN_POINT ( 'NONE',  ( 41.66904755831210849, -9.150666335777657423E-14, 0.000000000000000000 ) ) ;
#40302 = CARTESIAN_POINT ( 'NONE',  ( -452.6627218934859798, 390.0000000000064801, -141.4497041420121377 ) ) ;
#40303 = CARTESIAN_POINT ( 'NONE',  ( -24.70354720400822757, 8.582324684301863016, -39.48142304760889942 ) ) ;
#40304 = DIRECTION ( 'NONE',  ( -1.000000000000000000, 0.000000000000000000, 0.000000000000000000 ) ) ;
#40305 = VERTEX_POINT ( 'NONE', #29756 ) ;
#40306 = ORIENTED_EDGE ( 'NONE', *, *, #38249, .T. ) ;
#40307 = ORIENTED_EDGE ( 'NONE', *, *, #234, .T. ) ;
#40308 = FACE_OUTER_BOUND ( 'NONE', #18858, .T. ) ;
#40309 = CARTESIAN_POINT ( 'NONE',  ( -71.35455658117328426, 19.66980550601473254, 89.90639409444233365 ) ) ;
#40310 = CARTESIAN_POINT ( 'NONE',  ( -82.32750425780473336, 23.74963782027935721, 71.32606545563898237 ) ) ;
#40311 = CARTESIAN_POINT ( 'NONE',  ( 63.98009977735164000, 12.89803120691695959, -50.67432517864035901 ) ) ;
#40312 = DIRECTION ( 'NONE',  ( -0.000000000000000000, 1.000000000000000000, -0.000000000000000000 ) ) ;
#40313 = CARTESIAN_POINT ( 'NONE',  ( -61.52761555060400411, 17.56359742150279146, 34.00003020467226378 ) ) ;
#40314 = LINE ( 'NONE', #23461, #21412 ) ;
#40315 = CARTESIAN_POINT ( 'NONE',  ( 55.91494169499918598, 12.16343363043255899, 39.74022306742683952 ) ) ;
#40316 = DIRECTION ( 'NONE',  ( 0.9578262852211514300, 1.172998894335282758E-16, -0.2873478855663451625 ) ) ;
#40318 = ORIENTED_EDGE ( 'NONE', *, *, #51620, .T. ) ;
#40317 = ADVANCED_FACE ( 'NONE', ( #60720 ), #30113, .F. ) ;
#40319 = CARTESIAN_POINT ( 'NONE',  ( -7.336760511143403107, 6.859209474528211281, -50.41807073194384969 ) ) ;
#40320 = CARTESIAN_POINT ( 'NONE',  ( -35.00000000000002842, 225.0000000000000000, 0.000000000000000000 ) ) ;
#40321 = CARTESIAN_POINT ( 'NONE',  ( -190.3074740493607067, 108.5764897054613414, -45.99346789251534773 ) ) ;
#40322 = FACE_OUTER_BOUND ( 'NONE', #49663, .T. ) ;
#40323 = CARTESIAN_POINT ( 'NONE',  ( 0.000000000000000000, 65.13282190615278466, 5.000000000000000000 ) ) ;
#40324 = CARTESIAN_POINT ( 'NONE',  ( -109.3553681454883844, 36.52260784104394986, -71.89925778247966548 ) ) ;
#40325 = CARTESIAN_POINT ( 'NONE',  ( 132.9453095272139649, 42.04754713161464963, -9.178760341931969435 ) ) ;
#40326 = ADVANCED_FACE ( 'NONE', ( #50171 ), #55800, .F. ) ;
#40327 = AXIS2_PLACEMENT_3D ( 'NONE', #20961, #42412, #25902 ) ;
#40328 = ORIENTED_EDGE ( 'NONE', *, *, #27929, .T. ) ;
#40329 = CARTESIAN_POINT ( 'NONE',  ( 126.4633682455862100, 38.28837286275646790, -42.23541007965406635 ) ) ;
#40330 = CARTESIAN_POINT ( 'NONE',  ( -38.54712373114178092, 11.89174538567467643, -45.26023169000558255 ) ) ;
#40331 = CARTESIAN_POINT ( 'NONE',  ( 0.000000000000000000, -6.928203230275509661, -3.999999999999999112 ) ) ;
#40332 = STYLED_ITEM ( 'NONE', ( #21799 ), #64301 ) ;
#40333 = CARTESIAN_POINT ( 'NONE',  ( -170.7765859439901419, 84.55522338090253243, 84.86709083567915002 ) ) ;
#40334 = EDGE_LOOP ( 'NONE', ( #18726, #27477, #41702, #11099, #28631, #4228, #51302, #830, #67447 ) ) ;
#40335 = CARTESIAN_POINT ( 'NONE',  ( 132.2818448028687897, 41.65267246304668447, 2.829438630737001859 ) ) ;
#40336 = EDGE_CURVE ( 'NONE', #44250, #61065, #1635, .T. ) ;
#40337 = DIRECTION ( 'NONE',  ( 0.000000000000000000, 0.000000000000000000, 1.000000000000000000 ) ) ;
#40338 = DIRECTION ( 'NONE',  ( -1.000000000000000000, 0.000000000000000000, 0.000000000000000000 ) ) ;
#40339 = ADVANCED_FACE ( 'NONE', ( #7624 ), #33999, .F. ) ;
#40340 = ORIENTED_EDGE ( 'NONE', *, *, #52512, .T. ) ;
#40341 = CARTESIAN_POINT ( 'NONE',  ( 164.6219598329275868, 64.74833093291276498, 88.30847154703400292 ) ) ;
#40342 = ADVANCED_FACE ( 'NONE', ( #18168 ), #39619, .F. ) ;
#40343 = ORIENTED_EDGE ( 'NONE', *, *, #28772, .T. ) ;
#40344 = LINE ( 'NONE', #57905, #66054 ) ;
#40345 = CARTESIAN_POINT ( 'NONE',  ( 126.8015497489690091, 37.32461426945042859, 34.45213346083535555 ) ) ;
#40346 = DIRECTION ( 'NONE',  ( 2.220446049250313081E-16, 0.000000000000000000, 1.000000000000000000 ) ) ;
#40347 = EDGE_CURVE ( 'NONE', #21319, #52293, #59948, .T. ) ;
#40348 = FACE_OUTER_BOUND ( 'NONE', #29114, .T. ) ;
#40349 = DIRECTION ( 'NONE',  ( 1.000000000000000000, 0.000000000000000000, 0.000000000000000000 ) ) ;
#40351 = ORIENTED_EDGE ( 'NONE', *, *, #58265, .T. ) ;
#40350 = CARTESIAN_POINT ( 'NONE',  ( 15.68296563925498965, 63.09411298019766434, 3.061616997868437868E-16 ) ) ;
#40352 = CARTESIAN_POINT ( 'NONE',  ( -6.972379992530896686, 7.843576898687570242, -89.10717191287119476 ) ) ;
#40353 = ORIENTED_EDGE ( 'NONE', *, *, #47633, .T. ) ;
#40354 = VERTEX_POINT ( 'NONE', #25184 ) ;
#40355 = CARTESIAN_POINT ( 'NONE',  ( -166.9992034932275544, 82.01285191063136892, 15.83985853835711488 ) ) ;
#40356 = EDGE_CURVE ( 'NONE', #11740, #20027, #26274, .T. ) ;
#40357 = CARTESIAN_POINT ( 'NONE',  ( 20.74852474914887068, 6.709938988646750424, -64.21677084482480780 ) ) ;
#40359 = ORIENTED_EDGE ( 'NONE', *, *, #20532, .F. ) ;
#40358 = CARTESIAN_POINT ( 'NONE',  ( -132.8257891167039588, 52.46553896898736724, 67.83950217250055914 ) ) ;
#40360 = CARTESIAN_POINT ( 'NONE',  ( -94.77353847196663139, 30.23867427826260013, 91.81396056268231121 ) ) ;
#40361 = MANIFOLD_SOLID_BREP ( 'Boss-Extrude1', #58612 ) ;
#40362 = ADVANCED_FACE ( 'NONE', ( #69099 ), #50988, .T. ) ;
#40363 = EDGE_CURVE ( 'NONE', #242, #57624, #38620, .T. ) ;
#40364 = CARTESIAN_POINT ( 'NONE',  ( -71.23176719684943237, 20.69188312694500453, -41.59565793431328729 ) ) ;
#40365 = EDGE_CURVE ( 'NONE', #1408, #52352, #68095, .T. ) ;
#40366 = ORIENTED_EDGE ( 'NONE', *, *, #13583, .T. ) ;
#40367 = CARTESIAN_POINT ( 'NONE',  ( -20.00000000000000000, 2.449293598294706513E-15, -5.000000000000000888 ) ) ;
#40368 = B_SPLINE_CURVE_WITH_KNOTS ( 'NONE', 3,
 ( #63577, #3454, #15391, #10108, #30533, #35817, #24915, #46349, #14360, #57269, #51982, #3799, #30884, #25267, #52328, #58977, #10791, #15731, #49103, #48071, #37181, #942 ),
 .UNSPECIFIED., .F., .F.,
 ( 4, 2, 2, 2, 2, 2, 2, 2, 2, 2, 4 ),
 ( 0.01079565252593830092, 0.01215565516365934261, 0.01351565780138038603, 0.01487566043910142771, 0.01555566175796195202, 0.01623566307682247287, 0.01759566571454351802, 0.01827566703340402846, 0.01895566835226453889, 0.02031567098998559445, 0.02167567362770664655 ),
 .UNSPECIFIED. ) ;
#40369 = DIRECTION ( 'NONE',  ( 0.000000000000000000, 0.000000000000000000, 1.000000000000000000 ) ) ;
#40370 = CARTESIAN_POINT ( 'NONE',  ( 113.8626313173125766, 31.71036178495293001, 43.69715942616913651 ) ) ;
#40371 = DIRECTION ( 'NONE',  ( 0.000000000000000000, 0.000000000000000000, 1.000000000000000000 ) ) ;
#40372 = DIRECTION ( 'NONE',  ( 1.000000000000000000, 1.387778780781442471E-16, 0.000000000000000000 ) ) ;
#40373 = VERTEX_POINT ( 'NONE', #52916 ) ;
#40374 = CIRCLE ( 'NONE', #53802, 65.00000000000000000 ) ;
#40375 = ORIENTED_EDGE ( 'NONE', *, *, #26205, .F. ) ;
#40376 = CARTESIAN_POINT ( 'NONE',  ( -142.8492950481059154, 60.01492924994602873, -18.93097386172547303 ) ) ;
#40377 = CARTESIAN_POINT ( 'NONE',  ( 427.4999999999999432, 207.5000000000000284, 1.999999999999998224 ) ) ;
#40378 = PRESENTATION_LAYER_ASSIGNMENT (  '', '', ( #53859 ) ) ;
#40379 = CYLINDRICAL_SURFACE ( 'NONE', #59133, 7.500000000000020428 ) ;
#40380 = DIRECTION ( 'NONE',  ( -1.000000000000000000, -0.000000000000000000, -0.000000000000000000 ) ) ;
#40381 = CARTESIAN_POINT ( 'NONE',  ( -142.5211356634642073, 58.47296527616907014, 35.47922671525356009 ) ) ;
#40382 = CARTESIAN_POINT ( 'NONE',  ( -132.9409505933031426, 51.31241517713429801, 62.34483324402277304 ) ) ;
#40383 = CARTESIAN_POINT ( 'NONE',  ( -171.4814970982679654, 85.32124710276286805, -61.72613384226752942 ) ) ;
#40384 = ORIENTED_EDGE ( 'NONE', *, *, #24554, .F. ) ;
#40385 = CARTESIAN_POINT ( 'NONE',  ( -107.0809603157386647, 36.42942792191063717, 43.80174314235760846 ) ) ;
#40386 = ORIENTED_EDGE ( 'NONE', *, *, #46887, .T. ) ;
#40387 = CARTESIAN_POINT ( 'NONE',  ( 36.09137906183516264, 8.001963043161765654, 30.67956151840819246 ) ) ;
#40388 = ORIENTED_EDGE ( 'NONE', *, *, #41395, .T. ) ;
#40389 = CARTESIAN_POINT ( 'NONE',  ( 10.55634918610409656, 31.11269837220803325, 2.000000000000000000 ) ) ;
#40390 = LINE ( 'NONE', #46350, #53520 ) ;
#40391 = CARTESIAN_POINT ( 'NONE',  ( -1.683356153842345604, -65.34430428700412108, 3.125053320693568639E-16 ) ) ;
#40392 = CARTESIAN_POINT ( 'NONE',  ( 41.66904755831212981, 20.55634918610394379, 85.00100000000000477 ) ) ;
#40393 = CARTESIAN_POINT ( 'NONE',  ( -8.320534640989466268, 7.931748412542452442, -35.41807073194379996 ) ) ;
#40394 = CIRCLE ( 'NONE', #10063, 74.95140232871122521 ) ;
#40395 = CARTESIAN_POINT ( 'NONE',  ( 153.2282895792479280, 54.42637815496157572, -49.81384560666342054 ) ) ;
#40396 = EDGE_LOOP ( 'NONE', ( #64094, #24258 ) ) ;
#40397 = DIRECTION ( 'NONE',  ( 9.109522253334654429E-16, 1.000000000000000000, 1.305497313003906699E-14 ) ) ;
#40398 = ORIENTED_EDGE ( 'NONE', *, *, #65765, .T. ) ;
#40399 = DIRECTION ( 'NONE',  ( -0.000000000000000000, 0.000000000000000000, -1.000000000000000000 ) ) ;
#40400 = CARTESIAN_POINT ( 'NONE',  ( -58.97243502469714826, 16.81420332340175605, 71.06078827025896771 ) ) ;
#40401 = LINE ( 'NONE', #35127, #15085 ) ;
#40402 = ORIENTED_EDGE ( 'NONE', *, *, #25498, .F. ) ;
#40403 = CARTESIAN_POINT ( 'NONE',  ( 266.9165763529819628, 242.0000000000000000, 128.9999999999999716 ) ) ;
#40404 = CARTESIAN_POINT ( 'NONE',  ( -8.807541152391513251, 6.956521193351525412, -62.31119320194252964 ) ) ;
#40405 = CARTESIAN_POINT ( 'NONE',  ( -95.63568360745013308, 29.53168204475775482, -19.15801658276413377 ) ) ;
#40406 = CARTESIAN_POINT ( 'NONE',  ( 136.1310312718401860, 42.81430973242786564, -36.36153061589796920 ) ) ;
#40407 = EDGE_CURVE ( 'NONE', #21788, #671, #30447, .T. ) ;
#40408 =( REPRESENTATION_RELATIONSHIP ('NONE','NONE', #40274, #7414 ) REPRESENTATION_RELATIONSHIP_WITH_TRANSFORMATION ( #63400 )SHAPE_REPRESENTATION_RELATIONSHIP( ) );
#40409 = ORIENTED_EDGE ( 'NONE', *, *, #38441, .F. ) ;
#40410 = AXIS2_PLACEMENT_3D ( 'NONE', #58698, #32673, #43206 ) ;
#40411 = CARTESIAN_POINT ( 'NONE',  ( -152.2873556200144378, 67.91256772393730046, 58.09607398853111704 ) ) ;
#40412 = CARTESIAN_POINT ( 'NONE',  ( -118.9468627709229054, 42.08677365399181269, 40.95864189269519784 ) ) ;
#40413 = CARTESIAN_POINT ( 'NONE',  ( -61.75956139478098805, 16.58288496614411756, -46.08246547442131202 ) ) ;
#40414 = ORIENTED_EDGE ( 'NONE', *, *, #67158, .T. ) ;
#40415 = CARTESIAN_POINT ( 'NONE',  ( -177.5100621450479537, 93.70693725195826573, -75.15615139773954922 ) ) ;
#40416 = CARTESIAN_POINT ( 'NONE',  ( 129.7308524360012427, 40.15101741188608742, 84.42769425744016587 ) ) ;
#40417 = EDGE_CURVE ( 'NONE', #27957, #25366, #19898, .T. ) ;
#40419 = EDGE_CURVE ( 'NONE', #59923, #4530, #41355, .T. ) ;
#40418 = LINE ( 'NONE', #41469, #1007 ) ;
#40420 = DIRECTION ( 'NONE',  ( -0.000000000000000000, 1.000000000000000000, -0.000000000000000000 ) ) ;
#40421 = EDGE_CURVE ( 'NONE', #23357, #68876, #14952, .T. ) ;
#40422 = CARTESIAN_POINT ( 'NONE',  ( 390.9212159716611836, 95.00000000000000000, 0.000000000000000000 ) ) ;
#40423 = AXIS2_PLACEMENT_3D ( 'NONE', #26857, #48283, #5735 ) ;
#40424 = EDGE_CURVE ( 'NONE', #33190, #44118, #37565, .T. ) ;
#40425 = ORIENTED_EDGE ( 'NONE', *, *, #17860, .F. ) ;
#40426 = CARTESIAN_POINT ( 'NONE',  ( 162.8142581494936394, 61.92799983924231810, -11.49565247231627119 ) ) ;
#40427 = CARTESIAN_POINT ( 'NONE',  ( 115.7561705820729117, 31.51689401996055651, -75.37479631241809841 ) ) ;
#40428 = LINE ( 'NONE', #45359, #7208 ) ;
#40429 = CARTESIAN_POINT ( 'NONE',  ( 138.5943620234099001, 45.55242290395132443, 4.331259207765530306 ) ) ;
#40430 = CARTESIAN_POINT ( 'NONE',  ( -12.71198166530320606, 21.52685583500265665, 0.000000000000000000 ) ) ;
#40431 = ADVANCED_FACE ( 'NONE', ( #59234 ), #49370, .F. ) ;
#40432 = VECTOR ( 'NONE', #65168, 1000.000000000000227 ) ;
#40433 = EDGE_LOOP ( 'NONE', ( #22336, #19691, #32778, #47601 ) ) ;
#40434 = LINE ( 'NONE', #3162, #32819 ) ;
#40435 = ORIENTED_EDGE ( 'NONE', *, *, #19770, .T. ) ;
#40436 = DIRECTION ( 'NONE',  ( 1.000000000000000000, 8.881784197001252323E-16, 0.000000000000000000 ) ) ;
#40437 = CARTESIAN_POINT ( 'NONE',  ( 141.3651931500070305, 46.14690144103921199, 90.63982096354233420 ) ) ;
#40438 = B_SPLINE_CURVE_WITH_KNOTS ( 'NONE', 3,
 ( #44212, #55119, #28391, #17128, #23127, #17849, #60044, #6596, #65696, #38963, #55471, #50549, #7651, #60407, #44577, #66405, #28754, #28043, #66055, #50202, #23483, #18195, #61106, #12928, #34388, #55832, #63183, #62841, #36446, #8690, #19930, #61785, #3065, #29437, #20264, #2711, #67098, #30144, #8340, #51594, #62493, #4099, #46648, #24173, #9031, #18887, #35063, #25216 ),
 .UNSPECIFIED., .F., .F.,
 ( 4, 2, 2, 2, 2, 2, 2, 2, 2, 2, 2, 2, 2, 2, 2, 2, 2, 2, 2, 2, 2, 2, 2, 4 ),
 ( 0.02746511744866863072, 0.02914922134997089548, 0.03083332525127316023, 0.03251742915257541111, 0.03335948110322656951, 0.03420153305387772097, 0.03504358500452887937, 0.03588563695518003083, 0.03756974085648229905, 0.03841179280713343663, 0.03925384475778457422, 0.04009589670843571874, 0.04093794865908685632, 0.04262205256038914536, 0.04430615646169143440, 0.04514820841234259974, 0.04599026036299375814, 0.04767436426429607493, 0.04935846816559839867, 0.05020052011624956401, 0.05104257206690072934, 0.05272667596820305308, 0.05356872791885422536, 0.05441077986950540457 ),
 .UNSPECIFIED. ) ;
#40439 = ORIENTED_EDGE ( 'NONE', *, *, #7943, .F. ) ;
#40440 = CARTESIAN_POINT ( 'NONE',  ( -147.7845268487069177, 62.73119438705056439, -61.84506813724533458 ) ) ;
#40442 = DIRECTION ( 'NONE',  ( 0.000000000000000000, 0.000000000000000000, 1.000000000000000000 ) ) ;
#40441 = AXIS2_PLACEMENT_3D ( 'NONE', #33109, #53148, #64070 ) ;
#40443 = FACE_OUTER_BOUND ( 'NONE', #28989, .T. ) ;
#40444 = EDGE_CURVE ( 'NONE', #937, #42059, #66768, .T. ) ;
#40445 = CARTESIAN_POINT ( 'NONE',  ( 163.2886151008987667, 62.32020850087170771, -48.36354064594853952 ) ) ;
#40446 = ORIENTED_EDGE ( 'NONE', *, *, #4574, .F. ) ;
#40447 = ADVANCED_FACE ( 'NONE', ( #27228 ), #10705, .F. ) ;
#40448 = CARTESIAN_POINT ( 'NONE',  ( -74.75133697335800775, -5.472689625387135770, 41.38025477438755928 ) ) ;
#40449 = CARTESIAN_POINT ( 'NONE',  ( 70.43355351840769174, 15.55757160495454983, 89.84466342665578509 ) ) ;
#40450 = CARTESIAN_POINT ( 'NONE',  ( 153.6141452268275884, 55.97027600123225000, -90.86889088305335349 ) ) ;
#40451 = CARTESIAN_POINT ( 'NONE',  ( 84.74089592029042706, 19.84571403269345424, -23.73936403045067678 ) ) ;
#40452 = CARTESIAN_POINT ( 'NONE',  ( -17.50000000000000000, -17.50000000000000000, 20.00000000000000000 ) ) ;
#40453 = CARTESIAN_POINT ( 'NONE',  ( 38.57561400113527839, 9.317436507016033431, -89.34323513843901310 ) ) ;
#40454 = CARTESIAN_POINT ( 'NONE',  ( 126.4083787442700242, 37.10531539900951969, -71.39317657368648895 ) ) ;
#40455 = VERTEX_POINT ( 'NONE', #53258 ) ;
#40456 = CARTESIAN_POINT ( 'NONE',  ( -97.48179118242298102, 31.52606332398822531, 59.07822971242244137 ) ) ;
#40457 = CARTESIAN_POINT ( 'NONE',  ( -15.32495246574475267, 8.506829480038508251, 63.95817259830450752 ) ) ;
#40458 = ORIENTED_EDGE ( 'NONE', *, *, #34342, .F. ) ;
#40459 = AXIS2_PLACEMENT_3D ( 'NONE', #55347, #17008, #38478 ) ;
#40460 = CARTESIAN_POINT ( 'NONE',  ( -157.0069571479806996, 72.18154199622277645, -42.61338853642176616 ) ) ;
#40461 = CARTESIAN_POINT ( 'NONE',  ( 210.0122310839192323, 115.7355030290288198, -11.66628312975793413 ) ) ;
#40462 = CARTESIAN_POINT ( 'NONE',  ( -37.07436112751819479, 11.60822760208521842, 42.68967068761850214 ) ) ;
#40463 = CARTESIAN_POINT ( 'NONE',  ( -155.2912910578197057, 69.24479901948498650, -64.37611446947235549 ) ) ;
#40464 = CARTESIAN_POINT ( 'NONE',  ( 57.23318867907233454, 11.40538244752438857, 86.21413257773676264 ) ) ;
#40465 = CARTESIAN_POINT ( 'NONE',  ( -47.95193882091085413, 12.89180642785319364, -72.02524729475207721 ) ) ;
#40466 = CARTESIAN_POINT ( 'NONE',  ( -3.255961059272217462, 7.643453059677442596, -10.10607710301138518 ) ) ;
#40467 = CARTESIAN_POINT ( 'NONE',  ( 174.2469308602414912, 71.96142024047681218, 6.869062816487226719 ) ) ;
#40468 = CARTESIAN_POINT ( 'NONE',  ( -61.38706483483512244, 16.47181058798475917, 14.99613853738705771 ) ) ;
#40469 = ORIENTED_EDGE ( 'NONE', *, *, #39782, .T. ) ;
#40470 = CARTESIAN_POINT ( 'NONE',  ( -97.48179118242302366, 31.52606332398818267, -48.29997264943230562 ) ) ;
#40471 = ORIENTED_EDGE ( 'NONE', *, *, #24858, .F. ) ;
#40472 = CARTESIAN_POINT ( 'NONE',  ( 108.3819860115547300, 28.02992728837240577, -77.54759093648532087 ) ) ;
#40473 = CARTESIAN_POINT ( 'NONE',  ( -3.000000000000006217, 0.000000000000000000, -23.97499999999999787 ) ) ;
#40474 = CARTESIAN_POINT ( 'NONE',  ( 41.80536115778105710, 8.734184316430663841, 57.14969185523772666 ) ) ;
#40475 = LINE ( 'NONE', #7444, #50342 ) ;
#40476 = CARTESIAN_POINT ( 'NONE',  ( -3.023885888100138697, 6.625757189166515460, 85.53385992682667904 ) ) ;
#40477 = VECTOR ( 'NONE', #30671, 1000.000000000000000 ) ;
#40478 = CARTESIAN_POINT ( 'NONE',  ( -106.4728934171453858, 36.10295170132724962, -21.89315576262807639 ) ) ;
#40479 = DIRECTION ( 'NONE',  ( -1.000000000000000000, -0.000000000000000000, -0.000000000000000000 ) ) ;
#40480 = CARTESIAN_POINT ( 'NONE',  ( -165.6398193834831716, 79.16932278174803628, 64.55551728305448478 ) ) ;
#40481 = ORIENTED_EDGE ( 'NONE', *, *, #25098, .T. ) ;
#40482 = VERTEX_POINT ( 'NONE', #22310 ) ;
#40483 = EDGE_CURVE ( 'NONE', #9471, #61817, #49256, .T. ) ;
#40484 = CARTESIAN_POINT ( 'NONE',  ( 0.000000000000000000, 0.000000000000000000, -5.000000000000000000 ) ) ;
#40485 = DIRECTION ( 'NONE',  ( 0.000000000000000000, 0.000000000000000000, 1.000000000000000000 ) ) ;
#40486 = CARTESIAN_POINT ( 'NONE',  ( -23.03840347525633447, -9.707315041312391202, 0.000000000000000000 ) ) ;
#40487 = CARTESIAN_POINT ( 'NONE',  ( 104.4006536356073980, 27.36759527624477073, 59.22638815182622807 ) ) ;
#40488 = EDGE_CURVE ( 'NONE', #59075, #48432, #12456, .T. ) ;
#40489 = CARTESIAN_POINT ( 'NONE',  ( -439.4229916354184411, 394.9999999999955094, 101.0502958579930066 ) ) ;
#40490 = AXIS2_PLACEMENT_3D ( 'NONE', #28081, #49524, #61146 ) ;
#40491 = CARTESIAN_POINT ( 'NONE',  ( 55.56634333706183781, 12.09342294753930069, -17.37762842755674342 ) ) ;
#40492 = ORIENTED_EDGE ( 'NONE', *, *, #10875, .F. ) ;
#40493 = DIRECTION ( 'NONE',  ( -2.377681859532289471E-16, -7.725556675377533209E-17, 1.000000000000000000 ) ) ;
#40494 = CARTESIAN_POINT ( 'NONE',  ( 15.78827728214693416, 7.507518794609576496, -35.51894409868578606 ) ) ;
#40495 = CARTESIAN_POINT ( 'NONE',  ( 8.679939806240504652, 7.383357464882123189, 66.76383109117342940 ) ) ;
#40496 = CARTESIAN_POINT ( 'NONE',  ( 141.9165763529819344, 242.0000000000000000, 129.0000000000000000 ) ) ;
#40497 = CARTESIAN_POINT ( 'NONE',  ( 12.92334181113699465, 6.425676190254471010, -89.76395520566100572 ) ) ;
#40498 = EDGE_CURVE ( 'NONE', #4244, #27145, #7877, .T. ) ;
#40499 = ADVANCED_FACE ( 'NONE', ( #61679 ), #28635, .F. ) ;
#40500 = ORIENTED_EDGE ( 'NONE', *, *, #49772, .T. ) ;
#40501 = EDGE_CURVE ( 'NONE', #67714, #20392, #12810, .T. ) ;
#40502 = ORIENTED_EDGE ( 'NONE', *, *, #32277, .T. ) ;
#40503 = CARTESIAN_POINT ( 'NONE',  ( -55.15976438495108169, -34.41253982194112382, 41.38025477438755928 ) ) ;
#40504 = CARTESIAN_POINT ( 'NONE',  ( 39.40195752203892710, 8.409560354027384221, 71.75838489642698903 ) ) ;
#40505 = CARTESIAN_POINT ( 'NONE',  ( -742.9236288613935812, -685.7537703392392814, 0.000000000000000000 ) ) ;
#40506 = CARTESIAN_POINT ( 'NONE',  ( 133.8566784816069344, -170.0000000000000000, 63.85489142945905172 ) ) ;
#40507 = CARTESIAN_POINT ( 'NONE',  ( 8.286608610395276742, 6.376392877433615602, 90.91779146060531502 ) ) ;
#40508 = VECTOR ( 'NONE', #15738, 1000.000000000000000 ) ;
#40509 = CARTESIAN_POINT ( 'NONE',  ( 79.23200707685334976, 17.02828389812517784, -68.90372702717917264 ) ) ;
#40510 = EDGE_CURVE ( 'NONE', #48379, #47772, #21610, .T. ) ;
#40511 = B_SPLINE_CURVE_WITH_KNOTS ( 'NONE', 3,
 ( #1699, #11531, #33008, #60777, #28784, #55866, #23509, #7680, #22104, #6621, #43544, #54440, #28069, #49161, #1000, #44245, #22452, #12253 ),
 .UNSPECIFIED., .F., .F.,
 ( 4, 2, 2, 2, 2, 2, 2, 2, 4 ),
 ( 0.01106689075334992868, 0.01242473758491097549, 0.01378258441647202230, 0.01514043124803306911, 0.01649827807959411766, 0.01785612491115516273, 0.01921397174271621128, 0.02057181857427725635, 0.02192966540583830490 ),
 .UNSPECIFIED. ) ;
#40512 = ORIENTED_EDGE ( 'NONE', *, *, #56797, .T. ) ;
#40513 = CARTESIAN_POINT ( 'NONE',  ( 141.9165763529819344, 242.0000000000000000, 108.9999999999999858 ) ) ;
#40514 = CARTESIAN_POINT ( 'NONE',  ( 197.6341357773624452, 98.74251867088339907, -41.28717180241687146 ) ) ;
#40515 = ORIENTED_EDGE ( 'NONE', *, *, #17860, .T. ) ;
#40516 = CYLINDRICAL_SURFACE ( 'NONE', #25036, 5.000000000000004441 ) ;
#40517 = EDGE_LOOP ( 'NONE', ( #60442, #40402, #5609, #61827 ) ) ;
#40518 = LINE ( 'NONE', #61965, #2796 ) ;
#40519 = CARTESIAN_POINT ( 'NONE',  ( -58.97243502469712695, 16.81420332340174895, -9.472863501132078312 ) ) ;
#40520 = CARTESIAN_POINT ( 'NONE',  ( 0.000000000000000000, 190.0000000000000000, 2.000000000000000000 ) ) ;
#40521 = ORIENTED_EDGE ( 'NONE', *, *, #8963, .T. ) ;
#40522 = ORIENTED_EDGE ( 'NONE', *, *, #29394, .T. ) ;
#40523 = CARTESIAN_POINT ( 'NONE',  ( 46.85361596800671435, 10.51535167202354693, 65.24308912524901416 ) ) ;
#40524 = CARTESIAN_POINT ( 'NONE',  ( -102.4897449030618333, 34.01725961887433414, -88.70367844590327877 ) ) ;
#40525 = CARTESIAN_POINT ( 'NONE',  ( 103.1695711638930675, 26.83837309506526481, 7.722913913205804448 ) ) ;
#40526 = ORIENTED_EDGE ( 'NONE', *, *, #63643, .F. ) ;
#40527 = EDGE_CURVE ( 'NONE', #49554, #61455, #5654, .T. ) ;
#40528 = CARTESIAN_POINT ( 'NONE',  ( 99.99999999999997158, 0.000000000000000000, -25.00000000000000000 ) ) ;
#40529 = CARTESIAN_POINT ( 'NONE',  ( -17.72433019600386217, 0.000000000000000000, -35.39385180692614341 ) ) ;
#40530 = CARTESIAN_POINT ( 'NONE',  ( 8.485361335568063268, 7.382900357301075189, -95.00000000000133582 ) ) ;
#40531 = CARTESIAN_POINT ( 'NONE',  ( 113.8748103246145575, 30.59837980920002565, -9.998117947202244338 ) ) ;
#40532 = CARTESIAN_POINT ( 'NONE',  ( 82.73618382051374454, 19.18661415186669217, -36.90649579248486845 ) ) ;
#40533 = DIRECTION ( 'NONE',  ( -9.109522253334613014E-16, -1.000000000000000000, 3.889846672687432470E-31 ) ) ;
#40534 = ORIENTED_EDGE ( 'NONE', *, *, #27524, .F. ) ;
#40535 = AXIS2_PLACEMENT_3D ( 'NONE', #6043, #43327, #37714 ) ;
#40536 = ORIENTED_EDGE ( 'NONE', *, *, #61857, .T. ) ;
#40537 = CARTESIAN_POINT ( 'NONE',  ( 181.0840389613909736, 80.03940679743416808, 2.464043515047717570 ) ) ;
#40539 = DIRECTION ( 'NONE',  ( 0.8465179929926601732, 0.5323601107705934199, -0.000000000000000000 ) ) ;
#40538 = VECTOR ( 'NONE', #40420, 1000.000000000000000 ) ;
#40540 = DIRECTION ( 'NONE',  ( -1.000000000000000000, 0.000000000000000000, 0.000000000000000000 ) ) ;
#40541 = CARTESIAN_POINT ( 'NONE',  ( -22.50000000000000355, 207.5000000000000284, 0.000000000000000000 ) ) ;
#40542 = CARTESIAN_POINT ( 'NONE',  ( 127.1040286383415037, 37.49395136275128237, 6.891878244443025103 ) ) ;
#40543 = CARTESIAN_POINT ( 'NONE',  ( 0.000000000000000000, 188.0000000000000000, 0.000000000000000000 ) ) ;
#40544 = CARTESIAN_POINT ( 'NONE',  ( 208.5412688739946248, 113.5467507967246945, 83.95023641488762678 ) ) ;
#40546 = DIRECTION ( 'NONE',  ( -0.000000000000000000, -0.000000000000000000, -1.000000000000000000 ) ) ;
#40545 = AXIS2_PLACEMENT_3D ( 'NONE', #16804, #66075, #23498 ) ;
#40547 = PLANE ( 'NONE',  #33161 ) ;
#40548 = CARTESIAN_POINT ( 'NONE',  ( -13.78293860383719327, 7.352367295275509029, 42.19825724717986759 ) ) ;
#40549 = ORIENTED_EDGE ( 'NONE', *, *, #2948, .F. ) ;
#40550 = CARTESIAN_POINT ( 'NONE',  ( 9.689943677145720358, 7.388265075009365468, -20.54709311085173695 ) ) ;
#40551 = ORIENTED_EDGE ( 'NONE', *, *, #7740, .F. ) ;
#40552 = CARTESIAN_POINT ( 'NONE',  ( 0.06809871960542752956, 6.146186931204407067, 5.354491962338127742 ) ) ;
#40553 = EDGE_LOOP ( 'NONE', ( #53801, #56890, #14322, #21952, #3896 ) ) ;
#40554 = CARTESIAN_POINT ( 'NONE',  ( -142.3187766126154941, 59.59460822661997526, 9.166696566367921406 ) ) ;
#40555 = CARTESIAN_POINT ( 'NONE',  ( 184.9757174666827382, 84.09845285279331506, -76.98475161410866008 ) ) ;
#40556 = CARTESIAN_POINT ( 'NONE',  ( -166.7050147108375029, 81.70694330787517856, 42.24510784831770138 ) ) ;
#40557 = VECTOR ( 'NONE', #6107, 1000.000000000000114 ) ;
#40558 = CARTESIAN_POINT ( 'NONE',  ( 44.99999999999999289, -20.00000000000000355, 4.000000000000000000 ) ) ;
#40559 = CARTESIAN_POINT ( 'NONE',  ( 31.96227686234409049, 7.558148489540042370, -44.10090099851916534 ) ) ;
#40560 = DIRECTION ( 'NONE',  ( 0.000000000000000000, 0.000000000000000000, -1.000000000000000000 ) ) ;
#40561 = CARTESIAN_POINT ( 'NONE',  ( 13.83281508467570475, 7.452090093180183672, -35.76147573379551403 ) ) ;
#40562 = CARTESIAN_POINT ( 'NONE',  ( 132.9440032680862771, 40.87616997986733480, -50.97107703778330290 ) ) ;
#40563 = ORIENTED_EDGE ( 'NONE', *, *, #1009, .F. ) ;
#40564 = ORIENTED_EDGE ( 'NONE', *, *, #45878, .F. ) ;
#40565 = EDGE_CURVE ( 'NONE', #26863, #65415, #34957, .T. ) ;
#40566 = DIRECTION ( 'NONE',  ( 0.000000000000000000, 1.000000000000000000, -0.000000000000000000 ) ) ;
#40567 = CARTESIAN_POINT ( 'NONE',  ( -15.31363169557738679, 7.494880774892000552, 10.28358019018753389 ) ) ;
#40568 = CARTESIAN_POINT ( 'NONE',  ( 1.313474075707213196, 8.479269695850863542, -0.3167204509598407491 ) ) ;
#40569 = ADVANCED_FACE ( 'NONE', ( #51134 ), #67326, .T. ) ;
#40570 = CARTESIAN_POINT ( 'NONE',  ( -25.48237668717799309, 8.689083390666786144, -65.07822405608331451 ) ) ;
#40571 = EDGE_CURVE ( 'NONE', #62016, #49197, #58136, .T. ) ;
#40572 = CARTESIAN_POINT ( 'NONE',  ( 12.46277766093406569, 6.416700641561361884, 17.41053802626028357 ) ) ;
#40573 = ORIENTED_EDGE ( 'NONE', *, *, #30519, .F. ) ;
#40574 = DIRECTION ( 'NONE',  ( 0.000000000000000000, -1.000000000000000000, 0.000000000000000000 ) ) ;
#40575 = CARTESIAN_POINT ( 'NONE',  ( -62.54086041493280135, 17.86944394914986844, -69.06975546854211245 ) ) ;
#40576 = CARTESIAN_POINT ( 'NONE',  ( 199.3764470687683286, 100.9548044849099568, -65.37965796067832969 ) ) ;
#40577 = CARTESIAN_POINT ( 'NONE',  ( -180.3153482337535252, 95.51031295027644319, -40.07067488068217642 ) ) ;
#40578 = CARTESIAN_POINT ( 'NONE',  ( 108.3819860115547584, 28.02992728837241287, 2.986060834905694961 ) ) ;
#40579 = DIRECTION ( 'NONE',  ( 1.000000000000000000, 1.850550996349095901E-16, 1.228197773518735191E-20 ) ) ;
#40580 = CARTESIAN_POINT ( 'NONE',  ( -33.17493578845583357, -47.98885271304750688, 27.58472315868180402 ) ) ;
#40581 = CARTESIAN_POINT ( 'NONE',  ( -51.99406906667272921, 13.88268392809765750, 71.51408645859281421 ) ) ;
#40582 = ADVANCED_FACE ( 'NONE', ( #47222 ), #69017, .F. ) ;
#40583 = CARTESIAN_POINT ( 'NONE',  ( -98.82269223037674521, 31.05895700771357326, -89.54463258280026139 ) ) ;
#40584 = ORIENTED_EDGE ( 'NONE', *, *, #1786, .T. ) ;
#40585 = EDGE_CURVE ( 'NONE', #66914, #24361, #4930, .T. ) ;
#40586 = DIRECTION ( 'NONE',  ( 0.3513748240813435175, -0.9362348706397369824, 0.000000000000000000 ) ) ;
#40587 = AXIS2_PLACEMENT_3D ( 'NONE', #44663, #45347, #13011 ) ;
#40588 = CARTESIAN_POINT ( 'NONE',  ( -131.3154845336012500, 50.16828105866952825, -74.46309887825546525 ) ) ;
#40589 = CARTESIAN_POINT ( 'NONE',  ( -108.5248383251030475, 37.21456094989610364, -73.52032136529315665 ) ) ;
#40590 = CARTESIAN_POINT ( 'NONE',  ( -48.99162761293257518, 13.13973062091724131, -47.14059449902415366 ) ) ;
#40591 = CARTESIAN_POINT ( 'NONE',  ( 447.3372781065086201, 370.0000000000043769, 108.5502958579838264 ) ) ;
#40592 = DIRECTION ( 'NONE',  ( 0.000000000000000000, -1.000000000000000000, 0.000000000000000000 ) ) ;
#40593 = AXIS2_PLACEMENT_3D ( 'NONE', #68128, #30831, #14644 ) ;
#40594 = EDGE_LOOP ( 'NONE', ( #3695, #52630 ) ) ;
#40595 = DIRECTION ( 'NONE',  ( -0.000000000000000000, -0.000000000000000000, 1.000000000000000000 ) ) ;
#40596 = CARTESIAN_POINT ( 'NONE',  ( -8.000000000000000000, -4.618802153517024500, -0.7145311798163346273 ) ) ;
#40597 = ORIENTED_EDGE ( 'NONE', *, *, #19719, .F. ) ;
#40598 = VECTOR ( 'NONE', #60986, 1000.000000000000000 ) ;
#40599 = ORIENTED_EDGE ( 'NONE', *, *, #26208, .T. ) ;
#40600 = DIRECTION ( 'NONE',  ( 0.000000000000000000, 0.000000000000000000, 1.000000000000000000 ) ) ;
#40601 = CARTESIAN_POINT ( 'NONE',  ( 150.0278556977734468, 53.32860603304213498, 37.98783775011875719 ) ) ;
#40602 = CARTESIAN_POINT ( 'NONE',  ( 10.55634918610403084, 4.999999999999969802, 0.000000000000000000 ) ) ;
#40603 = ORIENTED_EDGE ( 'NONE', *, *, #28408, .F. ) ;
#40604 = DIRECTION ( 'NONE',  ( 5.551115123125781716E-16, 0.000000000000000000, 1.000000000000000000 ) ) ;
#40605 = CARTESIAN_POINT ( 'NONE',  ( -174.7800083645697100, 88.99302808536937448, 4.150939364941768517 ) ) ;
#40606 = DIRECTION ( 'NONE',  ( 0.000000000000000000, 0.7071067811865474617, 0.7071067811865474617 ) ) ;
#40607 = VECTOR ( 'NONE', #37780, 1000.000000000000000 ) ;
#40608 = CARTESIAN_POINT ( 'NONE',  ( 111.9975424824652634, 170.0000000000000284, 536.6193948016162949 ) ) ;
#40609 = CARTESIAN_POINT ( 'NONE',  ( -85.96384504792885650, 26.32782846176032621, 39.66807532746997822 ) ) ;
#40610 = CARTESIAN_POINT ( 'NONE',  ( 150.4558794230171657, 52.39657120201827922, 87.91895567814847823 ) ) ;
#40611 = CARTESIAN_POINT ( 'NONE',  ( 139.2921620648436942, 44.80435067172502528, 4.974970203711714944 ) ) ;
#40612 = ORIENTED_EDGE ( 'NONE', *, *, #6580, .T. ) ;
#40613 = LINE ( 'NONE', #39584, #60417 ) ;
#40614 = CARTESIAN_POINT ( 'NONE',  ( 9.823983574062873814, 6.382904402091122975, 59.78584119632682103 ) ) ;
#40615 = CARTESIAN_POINT ( 'NONE',  ( 45.34143264614440483, 9.256465810451187437, -47.70603915148674190 ) ) ;
#40616 = PLANE ( 'NONE',  #46618 ) ;
#40618 = EDGE_LOOP ( 'NONE', ( #29294, #56897, #29217, #48871 ) ) ;
#40617 = LINE ( 'NONE', #24800, #6239 ) ;
#40619 = CARTESIAN_POINT ( 'NONE',  ( 86.62931800182292363, 19.42108912189597092, -35.82156419891171595 ) ) ;
#40620 = VERTEX_POINT ( 'NONE', #63419 ) ;
#40621 = DIRECTION ( 'NONE',  ( 0.000000000000000000, -0.000000000000000000, -1.000000000000000000 ) ) ;
#40622 = CARTESIAN_POINT ( 'NONE',  ( 79.92842440418704086, 18.29578799637231512, 33.80686922133299532 ) ) ;
#40623 = DIRECTION ( 'NONE',  ( -0.000000000000000000, -0.000000000000000000, -1.000000000000000000 ) ) ;
#40624 = CARTESIAN_POINT ( 'NONE',  ( -65.00000000000000000, 0.000000000000000000, 40.00000000000003553 ) ) ;
#40625 = DIRECTION ( 'NONE',  ( -0.000000000000000000, 1.000000000000000000, -0.000000000000000000 ) ) ;
#40626 = CARTESIAN_POINT ( 'NONE',  ( -81.23268307104842734, 24.39742801172156561, -22.82221074267823724 ) ) ;
#40627 = CARTESIAN_POINT ( 'NONE',  ( -180.2243452982809515, 96.99029284948635166, -12.94268875518402240 ) ) ;
#40628 = CARTESIAN_POINT ( 'NONE',  ( -52.68206656346373506, 15.09776187114413659, 44.93691432116340678 ) ) ;
#40629 = ORIENTED_EDGE ( 'NONE', *, *, #4846, .T. ) ;
#40630 = ORIENTED_EDGE ( 'NONE', *, *, #43838, .T. ) ;
#40631 = CARTESIAN_POINT ( 'NONE',  ( 445.3372781065085633, 177.8591479523844612, -111.4497041420119388 ) ) ;
#40632 = AXIS2_PLACEMENT_3D ( 'NONE', #58400, #47845, #11250 ) ;
#40633 = CARTESIAN_POINT ( 'NONE',  ( 102.7571040248401175, 25.57023079238896557, 64.48323540187037395 ) ) ;
#40634 = DIRECTION ( 'NONE',  ( 0.000000000000000000, -1.000000000000000000, -0.000000000000000000 ) ) ;
#40635 = CARTESIAN_POINT ( 'NONE',  ( 0.000000000000000000, 0.000000000000000000, 170.0000000000000000 ) ) ;
#40636 = VECTOR ( 'NONE', #18900, 1000.000000000000227 ) ;
#40637 = CARTESIAN_POINT ( 'NONE',  ( 188.5837490358996149, 86.53279111916958755, -44.03581940269903328 ) ) ;
#40638 = CARTESIAN_POINT ( 'NONE',  ( 17.72992212664810552, 6.570588738776105053, 30.26623964099782427 ) ) ;
#40639 = CARTESIAN_POINT ( 'NONE',  ( -142.1933357692790878, 59.49560539235535117, 90.21512086776893113 ) ) ;
#40640 = ORIENTED_EDGE ( 'NONE', *, *, #65264, .T. ) ;
#40641 = PRODUCT_DEFINITION_SHAPE ( 'NONE', 'NONE',  #69589 ) ;
#40642 = ORIENTED_EDGE ( 'NONE', *, *, #37012, .F. ) ;
#40643 = ADVANCED_FACE ( 'NONE', ( #26124 ), #30368, .T. ) ;
#40644 = VERTEX_POINT ( 'NONE', #47558 ) ;
#40645 = AXIS2_PLACEMENT_3D ( 'NONE', #35276, #14167, #45476 ) ;
#40646 = VECTOR ( 'NONE', #64017, 1000.000000000000000 ) ;
#40647 = DIRECTION ( 'NONE',  ( -0.000000000000000000, 1.000000000000000000, -0.000000000000000000 ) ) ;
#40648 = EDGE_CURVE ( 'NONE', #58415, #2171, #53214, .T. ) ;
#40649 = CARTESIAN_POINT ( 'NONE',  ( -86.15441609607631790, 25.31657638323078530, 64.26769477816569065 ) ) ;
#40650 = CARTESIAN_POINT ( 'NONE',  ( 70.38121440378670002, 14.50253793787158862, -41.74354549825704908 ) ) ;
#40651 = PLANE ( 'NONE',  #713 ) ;
#40652 = VECTOR ( 'NONE', #9479, 1000.000000000000000 ) ;
#40653 = CARTESIAN_POINT ( 'NONE',  ( -62.14837099232447315, 17.75045801599141271, 40.25957659325134586 ) ) ;
#40654 = ADVANCED_FACE ( 'NONE', ( #68012 ), #24752, .T. ) ;
#40655 = CLOSED_SHELL ( 'NONE', ( #64072, #19069, #5302, #640, #66941, #34804, #41213, #18844, #17627, #41222, #30966, #24594, #60087, #46222, #58970, #24107, #12303, #48651, #45976, #6971 ) ) ;
#40656 = CARTESIAN_POINT ( 'NONE',  ( -38.88884187334147668, 11.95889603743728102, -70.65858916182976657 ) ) ;
#40657 = CARTESIAN_POINT ( 'NONE',  ( 33.44983424733139543, 7.709709042132401713, 68.84813754810760145 ) ) ;
#40658 = CARTESIAN_POINT ( 'NONE',  ( 43.46000298353792601, 8.971888098965388636, 84.78699099868985911 ) ) ;
#40659 = ORIENTED_EDGE ( 'NONE', *, *, #57725, .T. ) ;
#40660 = CARTESIAN_POINT ( 'NONE',  ( 65.78600691410852619, -10.66798400760944610, 34.48241823980617227 ) ) ;
#40661 = DIRECTION ( 'NONE',  ( 0.000000000000000000, 0.000000000000000000, 1.000000000000000000 ) ) ;
#40662 = LINE ( 'NONE', #35395, #10647 ) ;
#40663 = CARTESIAN_POINT ( 'NONE',  ( 66.73594759725088466, 13.56641407806658073, -63.54845448085986703 ) ) ;
#40664 = CARTESIAN_POINT ( 'NONE',  ( 129.4987365823222660, 38.85470922756779544, -22.78752412490684165 ) ) ;
#40665 = LINE ( 'NONE', #4083, #63585 ) ;
#40666 = CARTESIAN_POINT ( 'NONE',  ( -107.7893514267588557, 35.66840175773126020, -74.47184679149792430 ) ) ;
#40667 = EDGE_CURVE ( 'NONE', #4738, #67298, #19819, .T. ) ;
#40668 = ORIENTED_EDGE ( 'NONE', *, *, #32393, .T. ) ;
#40669 = DIRECTION ( 'NONE',  ( 9.508774330960553425E-15, -4.257857076819296916E-15, 0.9999999999999997780 ) ) ;
#40670 = CARTESIAN_POINT ( 'NONE',  ( 126.4757069339777189, 38.29528077539266206, -44.88019376975797314 ) ) ;
#40671 = DIRECTION ( 'NONE',  ( 0.000000000000000000, -1.000000000000000000, 0.000000000000000000 ) ) ;
#40672 = CARTESIAN_POINT ( 'NONE',  ( 444.9999999999999432, -35.00000000000000000, -2.000000000000000000 ) ) ;
#40673 = LINE ( 'NONE', #52608, #44502 ) ;
#40674 = VERTEX_POINT ( 'NONE', #62019 ) ;
#40675 = VERTEX_POINT ( 'NONE', #62730 ) ;
#40676 = CARTESIAN_POINT ( 'NONE',  ( 10.61438981621042643, -5.226566692248928447, -54.38561018378954515 ) ) ;
#40677 = LINE ( 'NONE', #36107, #12482 ) ;
#40678 = VERTEX_POINT ( 'NONE', #52166 ) ;
#40679 = CARTESIAN_POINT ( 'NONE',  ( 10.65073780419444738, -36.82468537061276237, 13.32819397642333215 ) ) ;
#40680 = ORIENTED_EDGE ( 'NONE', *, *, #7793, .T. ) ;
#40681 = CARTESIAN_POINT ( 'NONE',  ( 130.3281282802763315, 40.49854652972194202, -77.00284772816436885 ) ) ;
#40682 = CARTESIAN_POINT ( 'NONE',  ( -7.329206686002009974E-14, -41.66904755831212270, 0.000000000000000000 ) ) ;
#40683 = CARTESIAN_POINT ( 'NONE',  ( -153.6946616617039183, 69.16142959008686830, 31.98171298067408586 ) ) ;
#40684 = CARTESIAN_POINT ( 'NONE',  ( 0.000000000000000000, 0.000000000000000000, 0.000000000000000000 ) ) ;
#40685 = CARTESIAN_POINT ( 'NONE',  ( -27.00000000000000355, -27.00000000000000355, 12.00000000000000000 ) ) ;
#40686 = CIRCLE ( 'NONE', #45159, 5.000000000000004441 ) ;
#40688 = VERTEX_POINT ( 'NONE', #51820 ) ;
#40687 = LINE ( 'NONE', #47011, #19602 ) ;
#40689 = B_SPLINE_CURVE_WITH_KNOTS ( 'NONE', 3,
 ( #56985, #50657, #8096, #8803, #40451, #7761, #35531, #24637, #46412, #3510, #57327, #13045, #61568, #62250, #14420, #46071, #68235, #8451, #61217, #20043, #34844, #2477, #67542, #18659, #52048, #19339, #2823, #29210, #45733, #9140, #34505, #29545, #51014, #40795, #19687, #35872, #23932, #13383, #45382, #67212, #66861, #18999, #14065, #40111 ),
 .UNSPECIFIED., .F., .F.,
 ( 4, 2, 2, 2, 2, 2, 2, 2, 2, 2, 2, 2, 2, 2, 2, 2, 2, 2, 2, 2, 2, 4 ),
 ( 0.02416815208377490892, 0.02567033257376878305, 0.02642142281876571838, 0.02717251306376265718, 0.02867469355375653131, 0.02942578379875344929, 0.03017687404375036728, 0.03167905453374421365, 0.03318123502373805656, 0.03393232526873497801, 0.03468341551373190640, 0.03618559600372574930, 0.03693668624872267076, 0.03768777649371959221, 0.03918995698371342817, 0.04069213747370725720, 0.04219431796370109317, 0.04369649845369492913, 0.04444758869869186446, 0.04519867894368879979, 0.04670085943368265657, 0.04820303992367652723 ),
 .UNSPECIFIED. ) ;
#40690 = CARTESIAN_POINT ( 'NONE',  ( -4.529991408371923711, 7.705014754505700836, -89.81607011104952676 ) ) ;
#40691 = VERTEX_POINT ( 'NONE', #25454 ) ;
#40692 = VECTOR ( 'NONE', #4482, 1000.000000000000000 ) ;
#40693 = EDGE_LOOP ( 'NONE', ( #16332, #46241, #48461, #68589 ) ) ;
#40694 = CARTESIAN_POINT ( 'NONE',  ( 175.0634607207818760, 74.11351956991630630, 41.28835302766208315 ) ) ;
#40695 = CARTESIAN_POINT ( 'NONE',  ( 19.53470118933705635, 6.649487981843462236, -76.36537058919049059 ) ) ;
#40697 = ORIENTED_EDGE ( 'NONE', *, *, #25019, .F. ) ;
#40696 = CARTESIAN_POINT ( 'NONE',  ( -133.1566699306513044, 52.70203339370771545, 63.07426314407797463 ) ) ;
#40698 = CARTESIAN_POINT ( 'NONE',  ( -94.87248710667839191, 30.28499078005656742, 90.48868467975900387 ) ) ;
#40699 = MANIFOLD_SOLID_BREP ( 'Cut-Extrude2', #57536 ) ;
#40700 = AXIS2_PLACEMENT_3D ( 'NONE', #59364, #43530, #54784 ) ;
#40701 = FACE_BOUND ( 'NONE', #68225, .T. ) ;
#40702 = ORIENTED_EDGE ( 'NONE', *, *, #7779, .F. ) ;
#40703 = EDGE_CURVE ( 'NONE', #24540, #57182, #68592, .T. ) ;
#40704 = CARTESIAN_POINT ( 'NONE',  ( 208.5936709733498446, 113.6229123546138311, -77.09327358427836430 ) ) ;
#40705 = EDGE_CURVE ( 'NONE', #902, #20984, #43012, .T. ) ;
#40706 = PLANE ( 'NONE',  #37599 ) ;
#40707 = CARTESIAN_POINT ( 'NONE',  ( 112.5612011511790058, 31.08353758940340938, 29.96277884949118331 ) ) ;
#40708 = CARTESIAN_POINT ( 'NONE',  ( -128.1267916618075446, 49.19573276651589566, 18.45006178907944161 ) ) ;
#40709 = DIRECTION ( 'NONE',  ( 1.000000000000000000, 0.000000000000000000, -0.000000000000000000 ) ) ;
#40710 = ORIENTED_EDGE ( 'NONE', *, *, #7470, .T. ) ;
#40711 = ORIENTED_EDGE ( 'NONE', *, *, #2462, .F. ) ;
#40712 = B_SPLINE_CURVE_WITH_KNOTS ( 'NONE', 3,
 ( #25414, #10240, #14152, #3594, #51785, #4623, #36988, #3946, #57069, #52126, #47185, #46494, #8882, #25064, #68642, #42266, #31706, #63727, #30333, #15189, #63025, #62695, #67977, #47518, #53138, #14495, #41571, #26438, #20806, #15536, #63379, #19775, #14832, #58426, #26087, #36301, #46849, #68978, #41234, #9571, #68317, #20120, #31030, #35952 ),
 .UNSPECIFIED., .F., .F.,
 ( 4, 2, 2, 2, 2, 2, 2, 2, 2, 2, 2, 2, 2, 2, 2, 2, 2, 2, 2, 2, 2, 4 ),
 ( 0.000000000000000000, 0.001533942663855634905, 0.003067885327711269809, 0.004601827991566905147, 0.005368799323494720215, 0.006135770655422535282, 0.007669713319278181896, 0.008436684651206005636, 0.009203655983133829377, 0.01073759864698946125, 0.01150456997891726590, 0.01227154131084507056, 0.01303851264277287522, 0.01380548397470067988, 0.01533942663855628746, 0.01687336930241190025, 0.01840731196626750957, 0.01994125463012312235, 0.02070822596205092528, 0.02147519729397872820, 0.02300913995783436181, 0.02454308262168999541 ),
 .UNSPECIFIED. ) ;
#40713 = CARTESIAN_POINT ( 'NONE',  ( -142.8556048422594529, 60.01994222009838609, -11.99344991105233937 ) ) ;
#40714 = CARTESIAN_POINT ( 'NONE',  ( -124.9970785861867739, 47.10847819093958577, -49.86331799269337495 ) ) ;
#40715 = DIRECTION ( 'NONE',  ( -1.000000000000000000, 0.000000000000000000, 0.000000000000000000 ) ) ;
#40716 = CARTESIAN_POINT ( 'NONE',  ( -52.95121991886625068, 14.12782764494541432, -89.19314900505109733 ) ) ;
#40717 = CARTESIAN_POINT ( 'NONE',  ( -30.62628708973294422, -68.47330165179167238, 43.58025477438756212 ) ) ;
#40718 = CARTESIAN_POINT ( 'NONE',  ( -29.55217180659046861, 15.61897120291162011, 6.893343212288939981 ) ) ;
#40719 = CARTESIAN_POINT ( 'NONE',  ( 70.51583798635768119, 15.57951509147423508, -43.46259958853134719 ) ) ;
#40720 = ADVANCED_FACE ( 'NONE', ( #9608 ), #31071, .T. ) ;
#40721 = CARTESIAN_POINT ( 'NONE',  ( -142.0747101610765242, -170.0000000000000000, -95.00000000000133582 ) ) ;
#40722 = CARTESIAN_POINT ( 'NONE',  ( -165.9992860119574516, 79.53569239468048124, -71.42556836936645936 ) ) ;
#40723 = ADVANCED_BREP_SHAPE_REPRESENTATION ( '', ( #39790, #66832 ), #44451 ) ;
#40724 = ORIENTED_EDGE ( 'NONE', *, *, #59581, .T. ) ;
#40725 = CARTESIAN_POINT ( 'NONE',  ( -109.6657532478350419, 37.84376708859253569, 36.68825689172810200 ) ) ;
#40726 = EDGE_CURVE ( 'NONE', #21605, #16881, #22837, .T. ) ;
#40727 = ORIENTED_EDGE ( 'NONE', *, *, #13168, .T. ) ;
#40728 = CARTESIAN_POINT ( 'NONE',  ( -31.93184248720559637, 9.672312402099827011, 18.37190381572552056 ) ) ;
#40729 = DIRECTION ( 'NONE',  ( -1.000000000000000000, 0.000000000000000000, 0.000000000000000000 ) ) ;
#40730 = VERTEX_POINT ( 'NONE', #55534 ) ;
#40731 = DIRECTION ( 'NONE',  ( -1.000000000000000000, 0.000000000000000000, 0.000000000000000000 ) ) ;
#40732 = FACE_OUTER_BOUND ( 'NONE', #67618, .T. ) ;
#40733 = CYLINDRICAL_SURFACE ( 'NONE', #65859, 7.500000000000013323 ) ;
#40734 = DIRECTION ( 'NONE',  ( -0.000000000000000000, -6.405132834375902056E-16, 1.000000000000000000 ) ) ;
#40735 = DIRECTION ( 'NONE',  ( -0.000000000000000000, -0.000000000000000000, -1.000000000000000000 ) ) ;
#40736 = CARTESIAN_POINT ( 'NONE',  ( -55.05276343752910151, -170.0000000000000000, 64.66187836339484818 ) ) ;
#40737 = VECTOR ( 'NONE', #16372, 1000.000000000000000 ) ;
#40738 = EDGE_CURVE ( 'NONE', #42819, #2042, #33347, .T. ) ;
#40739 = DIRECTION ( 'NONE',  ( 1.000000000000000000, 1.850550996349095901E-16, 1.228197773518735191E-20 ) ) ;
#40740 = ORIENTED_EDGE ( 'NONE', *, *, #41333, .T. ) ;
#40741 = AXIS2_PLACEMENT_3D ( 'NONE', #52652, #25252, #14677 ) ;
#40742 = CARTESIAN_POINT ( 'NONE',  ( -15.55634918610400597, 20.55634918610405748, 2.000000000000001776 ) ) ;
#40743 = ORIENTED_EDGE ( 'NONE', *, *, #8530, .T. ) ;
#40744 = CARTESIAN_POINT ( 'NONE',  ( -59.57733000654212674, 15.94108165424592727, 31.81619162008844626 ) ) ;
#40745 = CARTESIAN_POINT ( 'NONE',  ( -61.10880364359508121, 17.43879918625642134, 60.23065452846851997 ) ) ;
#40746 = LINE ( 'NONE', #61847, #51042 ) ;
#40747 = VERTEX_POINT ( 'NONE', #58464 ) ;
#40748 = CARTESIAN_POINT ( 'NONE',  ( 73.51344971438143716, -14.61114034329455258, 41.38025477438755928 ) ) ;
#40749 = CARTESIAN_POINT ( 'NONE',  ( -15.32520546926283522, 7.495995523981878073, -69.26974520926577839 ) ) ;
#40750 = CARTESIAN_POINT ( 'NONE',  ( -37.92511097250854846, 10.74631978746601213, 41.49036279183128073 ) ) ;
#40751 = AXIS2_PLACEMENT_3D ( 'NONE', #17831, #60391, #22752 ) ;
#40752 = CARTESIAN_POINT ( 'NONE',  ( -27.48703802937315288, 8.975952825337621732, 70.94001361132677630 ) ) ;
#40753 = EDGE_CURVE ( 'NONE', #57123, #24108, #52638, .T. ) ;
#40754 = VERTEX_POINT ( 'NONE', #37026 ) ;
#40756 = AXIS2_PLACEMENT_3D ( 'NONE', #16662, #43390, #1902 ) ;
#40755 = CARTESIAN_POINT ( 'NONE',  ( 0.000000000000000000, 0.000000000000000000, 0.000000000000000000 ) ) ;
#40757 = DIRECTION ( 'NONE',  ( 0.000000000000000000, 0.000000000000000000, 1.000000000000000000 ) ) ;
#40758 = EDGE_CURVE ( 'NONE', #33355, #34907, #12637, .T. ) ;
#40759 = EDGE_CURVE ( 'NONE', #61817, #8726, #2094, .T. ) ;
#40760 = EDGE_CURVE ( 'NONE', #35601, #5954, #17559, .T. ) ;
#40761 = CARTESIAN_POINT ( 'NONE',  ( -118.8689810167776244, 42.03922634358561794, 35.47965570148047476 ) ) ;
#40762 = CARTESIAN_POINT ( 'NONE',  ( -56.72814287166056602, 15.13700122306437201, -35.40189249770946134 ) ) ;
#40763 = ORIENTED_EDGE ( 'NONE', *, *, #27397, .F. ) ;
#40764 = CARTESIAN_POINT ( 'NONE',  ( -179.8989115484066303, 96.59045402602906449, -65.83356435992200772 ) ) ;
#40765 = CARTESIAN_POINT ( 'NONE',  ( 91.67571176799444288, 21.20498955963028820, 58.50299178729044769 ) ) ;
#40766 = CARTESIAN_POINT ( 'NONE',  ( 111.8699272271189074, 29.64190505307781009, 29.78602444577448338 ) ) ;
#40767 = CARTESIAN_POINT ( 'NONE',  ( 133.8566784816069344, -170.0000000000000000, 44.51034083899536142 ) ) ;
#40768 = CARTESIAN_POINT ( 'NONE',  ( -118.6849742182705540, 41.92701402439730884, -67.17183305668943660 ) ) ;
#40769 = EDGE_LOOP ( 'NONE', ( #41211, #35958 ) ) ;
#40770 = CARTESIAN_POINT ( 'NONE',  ( 198.8687991397275709, 98.67887821384412916, 31.98142328829086622 ) ) ;
#40771 = CARTESIAN_POINT ( 'NONE',  ( 115.7746371641014775, 31.52600568297706829, -65.17888831513212722 ) ) ;
#40772 = DIRECTION ( 'NONE',  ( -1.000000000000000000, 0.000000000000000000, 0.000000000000000000 ) ) ;
#40773 = CARTESIAN_POINT ( 'NONE',  ( 141.2361973397653117, 47.26569015399787332, 11.53046231077025752 ) ) ;
#40774 = LINE ( 'NONE', #13701, #63346 ) ;
#40775 = EDGE_LOOP ( 'NONE', ( #59422, #36000, #18207, #35183, #21344, #42938, #47275, #18115, #57556 ) ) ;
#40776 = CARTESIAN_POINT ( 'NONE',  ( 164.8433205901839074, 64.93586312665797777, -15.37696764588941178 ) ) ;
#40777 = VERTEX_POINT ( 'NONE', #28820 ) ;
#40778 = CARTESIAN_POINT ( 'NONE',  ( -173.1211646369891355, 88.63826465341152527, -7.867406574286299303 ) ) ;
#40779 = DIRECTION ( 'NONE',  ( 0.000000000000000000, -1.000000000000000000, 0.000000000000000000 ) ) ;
#40780 = AXIS2_PLACEMENT_3D ( 'NONE', #57790, #3294, #62379 ) ;
#40781 = AXIS2_PLACEMENT_3D ( 'NONE', #32076, #20827, #26109 ) ;
#40783 = ORIENTED_EDGE ( 'NONE', *, *, #49285, .T. ) ;
#40782 = CARTESIAN_POINT ( 'NONE',  ( -2.282530889443167084E-17, -4.999999999999999112, 21.42428528562853529 ) ) ;
#40784 = CARTESIAN_POINT ( 'NONE',  ( 164.1338586910085553, 64.33646242148854810, -40.17183423574092416 ) ) ;
#40785 = PLANE ( 'NONE',  #57376 ) ;
#40786 = CARTESIAN_POINT ( 'NONE',  ( 162.6190874793280159, 61.76782592053310594, -49.08288557175567490 ) ) ;
#40787 = AXIS2_PLACEMENT_3D ( 'NONE', #18498, #33299, #13231 ) ;
#40788 = ORIENTED_EDGE ( 'NONE', *, *, #16743, .F. ) ;
#40789 = EDGE_CURVE ( 'NONE', #37097, #34803, #66126, .T. ) ;
#40790 = CARTESIAN_POINT ( 'NONE',  ( -97.49665543375860466, 31.53324358035374075, 16.97217977605912154 ) ) ;
#40791 = VECTOR ( 'NONE', #43854, 1000.000000000000000 ) ;
#40792 = CARTESIAN_POINT ( 'NONE',  ( -127.6861178856153458, 47.68458428355325651, 45.41653894850171724 ) ) ;
#40793 = EDGE_CURVE ( 'NONE', #40754, #48439, #31741, .T. ) ;
#40794 = CARTESIAN_POINT ( 'NONE',  ( 156.7505278390357262, 58.36400587947789376, -89.81328548006503354 ) ) ;
#40795 = CARTESIAN_POINT ( 'NONE',  ( 81.74250361646204510, 18.86685472882136239, -10.76652222608316301 ) ) ;
#40796 = CYLINDRICAL_SURFACE ( 'NONE', #2197, 65.00000000000000000 ) ;
#40797 = AXIS2_PLACEMENT_3D ( 'NONE', #39209, #12126, #7552 ) ;
#40798 = CARTESIAN_POINT ( 'NONE',  ( 150.0973882686024865, 52.13852366454154463, 65.15538058431675950 ) ) ;
#40799 = CARTESIAN_POINT ( 'NONE',  ( 90.91356992076215704, 21.99794663086830937, 43.37270543508057585 ) ) ;
#40800 = ORIENTED_EDGE ( 'NONE', *, *, #26128, .F. ) ;
#40801 = CARTESIAN_POINT ( 'NONE',  ( 6.000000000000000000, 19.07878402833891229, -20.00000000000000000 ) ) ;
#40802 = CARTESIAN_POINT ( 'NONE',  ( -12.40598104375064281, 8.242193636955557068, 70.41920131499857405 ) ) ;
#40803 = ORIENTED_EDGE ( 'NONE', *, *, #55726, .F. ) ;
#40804 = CIRCLE ( 'NONE', #12743, 25.12245591505646303 ) ;
#40805 = CARTESIAN_POINT ( 'NONE',  ( 10.00000000000000000, 0.000000000000000000, 5.000000000000000000 ) ) ;
#40806 = PLANE ( 'NONE',  #57858 ) ;
#40807 = CARTESIAN_POINT ( 'NONE',  ( 103.4725384926517080, 26.96797537091730135, 33.87479904705897837 ) ) ;
#40808 = CARTESIAN_POINT ( 'NONE',  ( 0.000000000000000000, 0.000000000000000000, 41.38025477438755928 ) ) ;
#40809 = CARTESIAN_POINT ( 'NONE',  ( 63.36339561252631114, 12.75346589351348392, 83.50301528697106335 ) ) ;
#40810 = CARTESIAN_POINT ( 'NONE',  ( -450.6627218934913230, 177.8591479523843475, -111.4497041420117966 ) ) ;
#40811 = EDGE_CURVE ( 'NONE', #53628, #61115, #38677, .T. ) ;
#40812 = CARTESIAN_POINT ( 'NONE',  ( -1.095583923122881442, 7.553030873957006897, -12.75389933006059806 ) ) ;
#40813 = CARTESIAN_POINT ( 'NONE',  ( 173.6012773665503914, 71.36035397668605640, 9.375753324076253392 ) ) ;
#40815 = ADVANCED_FACE ( 'NONE', ( #54834 ), #49907, .F. ) ;
#40814 = CARTESIAN_POINT ( 'NONE',  ( -59.36813706141742131, 15.88103696331963732, 17.11169410266594682 ) ) ;
#40816 = VERTEX_POINT ( 'NONE', #50269 ) ;
#40817 = CARTESIAN_POINT ( 'NONE',  ( 133.8566784816069344, 42.60093787723652525, 29.51034083899533300 ) ) ;
#40818 = ORIENTED_EDGE ( 'NONE', *, *, #32653, .T. ) ;
#40819 = CARTESIAN_POINT ( 'NONE',  ( 104.7147873368645037, 26.40702926859710686, -65.17463016867208125 ) ) ;
#40820 = EDGE_CURVE ( 'NONE', #7248, #13790, #11933, .T. ) ;
#40821 = DIRECTION ( 'NONE',  ( 0.8584487936018655452, 0.5128992774059070170, 0.000000000000000000 ) ) ;
#40822 = CARTESIAN_POINT ( 'NONE',  ( 43.14712943604300932, 8.926114770663669873, 70.76097164223719460 ) ) ;
#40823 = CARTESIAN_POINT ( 'NONE',  ( -32.29068479830811356, 9.732388393132145765, -89.04274443136878858 ) ) ;
#40824 = MANIFOLD_SOLID_BREP ( 'EndChamfer', #61987 ) ;
#40825 = DIRECTION ( 'NONE',  ( 0.000000000000000000, -1.000000000000000000, 0.000000000000000000 ) ) ;
#40826 = CARTESIAN_POINT ( 'NONE',  ( -108.9444157621018405, 37.44493815491210853, -12.19092097621495974 ) ) ;
#40827 = ORIENTED_EDGE ( 'NONE', *, *, #60282, .F. ) ;
#40828 = DIRECTION ( 'NONE',  ( 0.000000000000000000, -1.000000000000000000, 0.000000000000000000 ) ) ;
#40829 = CARTESIAN_POINT ( 'NONE',  ( -165.9986675144415926, 79.53506019208352029, 67.53357148677014266 ) ) ;
#40830 = VERTEX_POINT ( 'NONE', #39028 ) ;
#40831 = VERTEX_POINT ( 'NONE', #60472 ) ;
#40832 = CARTESIAN_POINT ( 'NONE',  ( -156.4841188516943191, 70.33041971808555104, 35.45435599281108807 ) ) ;
#40833 = CARTESIAN_POINT ( 'NONE',  ( 33.18066468065407548, -39.60239314731277460, 26.66469066592268433 ) ) ;
#40834 = CARTESIAN_POINT ( 'NONE',  ( 24.36509522348982060, 70.94296747916789059, 133.5802547743875550 ) ) ;
#40835 = CARTESIAN_POINT ( 'NONE',  ( 107.0447263249840830, 28.53200276018955961, 70.74387349886869458 ) ) ;
#40836 = COLOUR_RGB ( '',0.7921568627450980005, 0.8196078431372548767, 0.9333333333333333481 ) ;
#40837 = CARTESIAN_POINT ( 'NONE',  ( 68.07999999999999829, 0.000000000000000000, 0.000000000000000000 ) ) ;
#40838 = CARTESIAN_POINT ( 'NONE',  ( 59.30258796551119360, 12.87111270082601600, -22.91115838005825722 ) ) ;
#40839 = ORIENTED_EDGE ( 'NONE', *, *, #1755, .T. ) ;
#40840 = ADVANCED_FACE ( 'NONE', ( #40062 ), #49548, .T. ) ;
#40841 = EDGE_CURVE ( 'NONE', #27437, #62968, #24244, .T. ) ;
#40842 = CARTESIAN_POINT ( 'NONE',  ( -1.224646799147352468E-15, 2.449293598294706513E-15, -20.00000000000000000 ) ) ;
#40843 = ORIENTED_EDGE ( 'NONE', *, *, #66760, .F. ) ;
#40844 = CARTESIAN_POINT ( 'NONE',  ( 19.75315861330097533, 7.667327050329333815, -49.38992306506955998 ) ) ;
#40845 = CARTESIAN_POINT ( 'NONE',  ( -144.9412191745148561, 61.69548892475973645, 44.19022063994489713 ) ) ;
#40846 = VECTOR ( 'NONE', #17006, 1000.000000000000114 ) ;
#40847 = FACE_BOUND ( 'NONE', #15962, .T. ) ;
#40848 = EDGE_CURVE ( 'NONE', #28455, #16807, #8758, .T. ) ;
#40849 = CIRCLE ( 'NONE', #57674, 5.000000000000018652 ) ;
#40850 = VECTOR ( 'NONE', #42240, 1000.000000000000000 ) ;
#40851 = VECTOR ( 'NONE', #22862, 1000.000000000000114 ) ;
#40852 = ORIENTED_EDGE ( 'NONE', *, *, #39245, .F. ) ;
#40853 = VERTEX_POINT ( 'NONE', #24592 ) ;
#40854 = CARTESIAN_POINT ( 'NONE',  ( -452.6627218934914367, 399.9999999999998863, -111.4497041420118251 ) ) ;
#40855 = CARTESIAN_POINT ( 'NONE',  ( -133.3902399421379812, 52.86946745625289168, 91.39822547968469735 ) ) ;
#40856 = VECTOR ( 'NONE', #32354, 1000.000000000000000 ) ;
#40857 = CARTESIAN_POINT ( 'NONE',  ( 36.99999522780156980, 9.122638774496635961, -77.07355369017872704 ) ) ;
#40858 = CARTESIAN_POINT ( 'NONE',  ( 123.4242852856285566, 10.00000000000000000, -20.00000000000000000 ) ) ;
#40859 = CARTESIAN_POINT ( 'NONE',  ( 13.21458769038542336, 6.431875961233155081, 84.15148632264042305 ) ) ;
#40860 = CARTESIAN_POINT ( 'NONE',  ( 22.60595478824430415, 7.822665100698110940, 88.06109399808075011 ) ) ;
#40861 = ORIENTED_EDGE ( 'NONE', *, *, #54386, .F. ) ;
#40862 = LINE ( 'NONE', #8517, #11187 ) ;
#40863 = CARTESIAN_POINT ( 'NONE',  ( -46.66904755831212981, -15.55634918610397222, 85.00100000000000477 ) ) ;
#40864 = EDGE_LOOP ( 'NONE', ( #35298, #37422, #8292, #39486 ) ) ;
#40865 = CARTESIAN_POINT ( 'NONE',  ( -83.12901536265223967, 24.07178615860086879, 17.10644552692404119 ) ) ;
#40866 = ORIENTED_EDGE ( 'NONE', *, *, #50598, .T. ) ;
#40867 = CARTESIAN_POINT ( 'NONE',  ( -39.55079474733699385, 51.59997227570983824, 3.061616997868437868E-16 ) ) ;
#40868 = FACE_OUTER_BOUND ( 'NONE', #29698, .T. ) ;
#40869 = ORIENTED_EDGE ( 'NONE', *, *, #31510, .F. ) ;
#40870 = VERTEX_POINT ( 'NONE', #62202 ) ;
#40871 = CARTESIAN_POINT ( 'NONE',  ( -29.87147652227456263, -74.98256102853682137, 73.58025477438756923 ) ) ;
#40872 = DIRECTION ( 'NONE',  ( -1.000000000000000000, 0.000000000000000000, 0.000000000000000000 ) ) ;
#40873 = CARTESIAN_POINT ( 'NONE',  ( 102.7446498997619955, 26.65764321315727159, 9.730055971096106759 ) ) ;
#40874 = ORIENTED_EDGE ( 'NONE', *, *, #33892, .F. ) ;
#40875 = CARTESIAN_POINT ( 'NONE',  ( -30.81072340916226793, 9.488257828543728678, 83.90441008401572276 ) ) ;
#40876 = EDGE_CURVE ( 'NONE', #40902, #44954, #69326, .T. ) ;
#40877 = CARTESIAN_POINT ( 'NONE',  ( 174.2538192999569731, 73.34752463892029084, -73.67968158064373085 ) ) ;
#40878 = AXIS2_PLACEMENT_3D ( 'NONE', #2110, #23901, #49922 ) ;
#40879 = DIRECTION ( 'NONE',  ( 0.000000000000000000, 1.000000000000000000, -0.000000000000000000 ) ) ;
#40880 = FACE_OUTER_BOUND ( 'NONE', #23853, .T. ) ;
#40881 = CARTESIAN_POINT ( 'NONE',  ( 82.94816950786172072, 19.25538918181908343, -36.78261693489493211 ) ) ;
#40882 = LINE ( 'NONE', #13466, #24287 ) ;
#40883 = VERTEX_POINT ( 'NONE', #14373 ) ;
#40884 = AXIS2_PLACEMENT_3D ( 'NONE', #6565, #33658, #43830 ) ;
#40885 = VERTEX_POINT ( 'NONE', #51995 ) ;
#40886 = CIRCLE ( 'NONE', #56609, 74.95140232871122521 ) ;
#40887 = CARTESIAN_POINT ( 'NONE',  ( 44.34263167748004264, 9.103379693481585377, 4.905521142611629415 ) ) ;
#40888 = CARTESIAN_POINT ( 'NONE',  ( -180.6072146854561993, 97.46297145775103843, 91.41803955879689170 ) ) ;
#40889 = PLANE ( 'NONE',  #60424 ) ;
#40890 = DIRECTION ( 'NONE',  ( -0.000000000000000000, -0.000000000000000000, -1.000000000000000000 ) ) ;
#40891 = CARTESIAN_POINT ( 'NONE',  ( 128.4224537826253822, 38.23837035195744249, 15.35765953459713451 ) ) ;
#40892 = VECTOR ( 'NONE', #10869, 1000.000000000000114 ) ;
#40893 = CARTESIAN_POINT ( 'NONE',  ( 38.98661671391530348, 8.355545674958261060, -89.30891864635513855 ) ) ;
#40894 = EDGE_CURVE ( 'NONE', #17237, #44366, #44984, .T. ) ;
#40895 = CARTESIAN_POINT ( 'NONE',  ( 203.6529352990553150, 106.6193458023785183, 82.96504318203567152 ) ) ;
#40896 = CARTESIAN_POINT ( 'NONE',  ( 208.5884523568772693, 113.6152425727545534, 43.13355516528025646 ) ) ;
#40897 = CARTESIAN_POINT ( 'NONE',  ( -78.66644367742109978, 22.32174330031320508, -61.96000122218157458 ) ) ;
#40898 = CARTESIAN_POINT ( 'NONE',  ( -104.1342612728951593, 33.73231160250194449, 30.73689793636901157 ) ) ;
#40899 = ORIENTED_EDGE ( 'NONE', *, *, #42450, .T. ) ;
#40900 = AXIS2_PLACEMENT_3D ( 'NONE', #57907, #53648, #25907 ) ;
#40901 = LINE ( 'NONE', #45482, #36291 ) ;
#40902 = VERTEX_POINT ( 'NONE', #18608 ) ;
#40903 = ADVANCED_FACE ( 'NONE', ( #34457 ), #8403, .T. ) ;
#40904 = CARTESIAN_POINT ( 'NONE',  ( -149.5074843970971017, 65.50121172469319220, -76.65738112195568021 ) ) ;
#40905 = ORIENTED_EDGE ( 'NONE', *, *, #16012, .T. ) ;
#40906 = EDGE_CURVE ( 'NONE', #3054, #28358, #68521, .T. ) ;
#40907 = LINE ( 'NONE', #68001, #20844 ) ;
#40908 = CARTESIAN_POINT ( 'NONE',  ( 187.8965227056806953, 87.27289477191497724, -67.42077669584755029 ) ) ;
#40909 = VECTOR ( 'NONE', #32096, 1000.000000000000000 ) ;
#40910 = DIRECTION ( 'NONE',  ( -0.8160245890732938934, -0.5780171883497599028, 0.000000000000000000 ) ) ;
#40911 = CARTESIAN_POINT ( 'NONE',  ( 206.2980740120524388, 108.5619562183279925, -78.00887972345341836 ) ) ;
#40912 = B_SPLINE_CURVE_WITH_KNOTS ( 'NONE', 3,
 ( #14393, #18967, #36529, #3827, #14721, #30221, #30913, #51333, #40415, #57984, #56954, #20342, #67506, #13687, #9452, #35844, #19303, #30560, #51673, #35143, #15071, #57296, #25298, #41117, #9801, #52012, #46380, #19654, #56595, #8417, #40764, #62215, #3149, #25644, #46732, #24606, #20011, #52361, #35493, #4175, #67859, #14032, #41467, #62921 ),
 .UNSPECIFIED., .F., .F.,
 ( 4, 2, 2, 2, 2, 2, 2, 2, 2, 2, 2, 2, 2, 2, 2, 2, 2, 2, 2, 2, 2, 4 ),
 ( 0.02908143158676657763, 0.03095422299093864363, 0.03282701439511070962, 0.03469980579928277215, 0.03657259720345483467, 0.03844538860762689719, 0.04031818001179896666, 0.04125457571388498057, 0.04219097141597099448, 0.04312736711805700840, 0.04359556496910003964, 0.04406376282014306395, 0.04500015852222907786, 0.04593655422431509872, 0.04687294992640111263, 0.04780934562848712654, 0.04968213703265918907, 0.05155492843683125159, 0.05342771984100331412, 0.05530051124517537664, 0.05717330264934743222, 0.05904609405351949475 ),
 .UNSPECIFIED. ) ;
#40913 = CARTESIAN_POINT ( 'NONE',  ( 32.15641333221389431, 7.577415570152252755, -41.16723562843993989 ) ) ;
#40914 = LINE ( 'NONE', #45489, #20297 ) ;
#40915 = CARTESIAN_POINT ( 'NONE',  ( 444.9999999999999432, -35.00000000000000000, 380.0000000000000000 ) ) ;
#40916 = CARTESIAN_POINT ( 'NONE',  ( 126.6576865394846152, 37.24426596493990615, -41.40349033908344012 ) ) ;
#40917 = ORIENTED_EDGE ( 'NONE', *, *, #29845, .T. ) ;
#40918 = ORIENTED_EDGE ( 'NONE', *, *, #50583, .T. ) ;
#40919 = CARTESIAN_POINT ( 'NONE',  ( -4.613603609465520172, 74.86839895266042788, 170.0000000000000000 ) ) ;
#40920 = CARTESIAN_POINT ( 'NONE',  ( -24.18258876560172155, 8.512344710720679331, -71.62007224143587791 ) ) ;
#40921 =( REPRESENTATION_RELATIONSHIP ('NONE','NONE', #46031, #55473 ) REPRESENTATION_RELATIONSHIP_WITH_TRANSFORMATION ( #51590 )SHAPE_REPRESENTATION_RELATIONSHIP( ) );
#40922 = UNCERTAINTY_MEASURE_WITH_UNIT (LENGTH_MEASURE( 1.000000000000000082E-05 ), #46970, 'distance_accuracy_value', 'NONE');
#40923 = CARTESIAN_POINT ( 'NONE',  ( 9.057575839850581900, 6.378493414438676012, 13.98797822051807849 ) ) ;
#40924 = B_SPLINE_CURVE_WITH_KNOTS ( 'NONE', 3,
 ( #37156, #58603, #53671, #48374, #16397, #59300, #5831, #27287, #569, #59636, #1610, #2319, #55780, #29734, #23075, #45563, #61049, #40292, #60701, #12516, #39599, #7600, #23434, #67046, #49784, #39943, #66695, #18836, #34684, #55065, #44525, #33636, #61397, #12876, #28340, #6883, #44873, #7242, #18488, #66001, #33977, #17433, #13221 ),
 .UNSPECIFIED., .F., .F.,
 ( 4, 2, 2, 2, 2, 2, 2, 2, 2, 2, 2, 1, 2, 2, 2, 2, 2, 2, 2, 2, 2, 4 ),
 ( 0.02515559250233026858, 0.02674001423437959851, 0.02753222510040426521, 0.02832443596642893191, 0.02990885769847832429, 0.03149327943052772361, 0.03307770116257711251, 0.03386991202860181044, 0.03466212289462650142, 0.03624654462667584870, 0.03703875549270052581, 0.03783096635872520985, 0.03862317722474989390, 0.03941538809077457101, 0.04099980982282393216, 0.04258423155487330025, 0.04337644242089798430, 0.04416865328692266141, 0.04575307501897196705, 0.04733749675102127963, 0.04892191848307057833, 0.05050634021511988397 ),
 .UNSPECIFIED. ) ;
#40925 = DIRECTION ( 'NONE',  ( 0.000000000000000000, 0.000000000000000000, 1.000000000000000000 ) ) ;
#40926 = DIRECTION ( 'NONE',  ( -0.9959742939952397345, 0.08963930890342655666, 0.000000000000000000 ) ) ;
#40927 = CARTESIAN_POINT ( 'NONE',  ( 133.8566784816069344, 41.42467568809808398, 71.35489142945907304 ) ) ;
#40928 = CARTESIAN_POINT ( 'NONE',  ( -180.0179082103088035, 95.14811732286295864, -39.25080714274592708 ) ) ;
#40929 = CARTESIAN_POINT ( 'NONE',  ( 94.11746922806585758, 22.11341285603784002, -15.98499990942385907 ) ) ;
#40930 = CARTESIAN_POINT ( 'NONE',  ( -171.4814970982680222, 85.32124710276291069, 18.80751792912352727 ) ) ;
#40931 = CARTESIAN_POINT ( 'NONE',  ( -37.75148796553126829, -54.92203290797168336, 34.48241795236666007 ) ) ;
#40932 = EDGE_CURVE ( 'NONE', #65795, #27252, #20608, .T. ) ;
#40933 = CARTESIAN_POINT ( 'NONE',  ( -51.78153763344963778, 13.82841714689605439, 57.89563959941560967 ) ) ;
#40934 = CARTESIAN_POINT ( 'NONE',  ( -1.857619870843137733, 6.575690665396234813, 69.02910518084183877 ) ) ;
#40935 = ORIENTED_EDGE ( 'NONE', *, *, #6798, .T. ) ;
#40937 = CARTESIAN_POINT ( 'NONE',  ( -190.6985136298601731, 109.1272424661242582, 33.97142148329322708 ) ) ;
#40936 = STYLED_ITEM ( 'NONE', ( #20327 ), #40938 ) ;
#40938 = MANIFOLD_SOLID_BREP ( 'Boss-Extrude3', #41763 ) ;
#40939 = CARTESIAN_POINT ( 'NONE',  ( 153.4509883044095773, 55.84811350575043321, 57.41771316415564286 ) ) ;
#40940 = CARTESIAN_POINT ( 'NONE',  ( -104.1393288135077597, 34.86912007524089319, -62.07806153423428697 ) ) ;
#40941 = CARTESIAN_POINT ( 'NONE',  ( -54.09522495088364735, 14.42642983673692925, -50.17067796789629597 ) ) ;
#40942 = CARTESIAN_POINT ( 'NONE',  ( 50.03867889673373526, -42.05760816978109773, 43.58025477438756212 ) ) ;
#40943 = FACE_OUTER_BOUND ( 'NONE', #62529, .T. ) ;
#40944 = CIRCLE ( 'NONE', #19598, 5.000000000000000888 ) ;
#40945 = ORIENTED_EDGE ( 'NONE', *, *, #46393, .T. ) ;
#40946 = CARTESIAN_POINT ( 'NONE',  ( -9.744241279244798548, 37.07486149500672923, 13.32819299319724138 ) ) ;
#40947 = VECTOR ( 'NONE', #30488, 1000.000000000000000 ) ;
#40948 = CYLINDRICAL_SURFACE ( 'NONE', #65298, 85.31295361348101380 ) ;
#40949 = ORIENTED_EDGE ( 'NONE', *, *, #47466, .T. ) ;
#40950 = VERTEX_POINT ( 'NONE', #62903 ) ;
#40951 = VECTOR ( 'NONE', #44500, 1000.000000000000000 ) ;
#40952 = DIRECTION ( 'NONE',  ( 0.000000000000000000, 0.000000000000000000, 1.000000000000000000 ) ) ;
#40953 = CARTESIAN_POINT ( 'NONE',  ( 10.55634918610406281, 20.55634918610400064, 2.000000000000001776 ) ) ;
#40954 = DIRECTION ( 'NONE',  ( -0.8584487936018728726, 0.5128992774058949156, 0.000000000000000000 ) ) ;
#40955 = ORIENTED_EDGE ( 'NONE', *, *, #10925, .F. ) ;
#40956 = FACE_OUTER_BOUND ( 'NONE', #33703, .T. ) ;
#40957 = CARTESIAN_POINT ( 'NONE',  ( -55.05276343752909440, 14.68156374112637863, -62.06087458892354647 ) ) ;
#40958 = CARTESIAN_POINT ( 'NONE',  ( -417.6627218934914367, 399.9999999999998863, -146.4497041420118251 ) ) ;
#40959 = LINE ( 'NONE', #36028, #27559 ) ;
#40960 = CARTESIAN_POINT ( 'NONE',  ( -81.24432217070641116, 24.40203426192925207, 44.96528098049749644 ) ) ;
#40961 = CARTESIAN_POINT ( 'NONE',  ( -27.49195330402089255, 9.993776132065303131, -22.35462794406847920 ) ) ;
#40962 = CARTESIAN_POINT ( 'NONE',  ( 140.5781926063689298, 45.63383190293699698, 6.828449788819809463 ) ) ;
#40963 = EDGE_CURVE ( 'NONE', #36565, #51770, #9792, .T. ) ;
#40964 = ADVANCED_FACE ( 'NONE', ( #60392 ), #16436, .F. ) ;
#40965 = ORIENTED_EDGE ( 'NONE', *, *, #48455, .T. ) ;
#40966 = LINE ( 'NONE', #7587, #30102 ) ;
#40967 = EDGE_CURVE ( 'NONE', #58719, #41480, #16069, .T. ) ;
#40968 = DIRECTION ( 'NONE',  ( -1.000000000000000000, 0.000000000000000000, 0.000000000000000000 ) ) ;
#40969 = LINE ( 'NONE', #35703, #34937 ) ;
#40970 = CARTESIAN_POINT ( 'NONE',  ( -79.92415359841270117, 23.88316156050048988, 84.18770871290736579 ) ) ;
#40972 = VERTEX_POINT ( 'NONE', #64622 ) ;
#40971 = DIRECTION ( 'NONE',  ( -1.000000000000000000, 0.000000000000000000, 0.000000000000000000 ) ) ;
#40973 = LINE ( 'NONE', #8970, #13970 ) ;
#40974 = ORIENTED_EDGE ( 'NONE', *, *, #55129, .F. ) ;
#40975 = ORIENTED_EDGE ( 'NONE', *, *, #64567, .F. ) ;
#40976 = DIRECTION ( 'NONE',  ( 1.000000000000000000, 0.000000000000000000, 0.000000000000000000 ) ) ;
#40977 = DIRECTION ( 'NONE',  ( 0.000000000000000000, -1.000000000000000000, 0.000000000000000000 ) ) ;
#40978 = CARTESIAN_POINT ( 'NONE',  ( 422.4999999999999432, -18.06806526123148160, 0.000000000000000000 ) ) ;
#40979 = DIRECTION ( 'NONE',  ( 0.000000000000000000, 0.000000000000000000, 1.000000000000000000 ) ) ;
#40980 = CARTESIAN_POINT ( 'NONE',  ( -121.5677746760273692, 43.71038933438990881, 71.10937227840975083 ) ) ;
#40981 = FACE_BOUND ( 'NONE', #16112, .T. ) ;
#40982 = CARTESIAN_POINT ( 'NONE',  ( -180.6209674222602644, 97.47999311542515954, -15.53406542695830161 ) ) ;
#40983 = VECTOR ( 'NONE', #30092, 1000.000000000000000 ) ;
#40984 = CARTESIAN_POINT ( 'NONE',  ( -51.77779688167512973, 14.86590802019196822, 31.06571622856426274 ) ) ;
#40985 = ORIENTED_EDGE ( 'NONE', *, *, #52303, .T. ) ;
#40986 = EDGE_CURVE ( 'NONE', #66752, #2912, #32614, .T. ) ;
#40987 = ORIENTED_EDGE ( 'NONE', *, *, #9797, .F. ) ;
#40988 = EDGE_CURVE ( 'NONE', #11058, #39519, #34059, .T. ) ;
#40989 = DIRECTION ( 'NONE',  ( 1.000000000000000000, 0.000000000000000000, 0.000000000000000000 ) ) ;
#40990 = AXIS2_PLACEMENT_3D ( 'NONE', #5721, #64827, #10312 ) ;
#40991 = B_SPLINE_CURVE_WITH_KNOTS ( 'NONE', 3,
 ( #30999, #3915, #41546, #24688, #53114, #67947, #62664, #20775, #47491, #52447, #25034, #25727, #31342, #68288, #26064, #20093, #46467, #15160, #47156, #63001, #68620, #36621, #19742, #19392, #41205, #30306, #20425, #41889, #63349, #58071, #4598, #68952, #14472, #42237 ),
 .UNSPECIFIED., .F., .F.,
 ( 4, 2, 2, 2, 2, 2, 2, 2, 2, 2, 2, 2, 2, 2, 2, 2, 4 ),
 ( 0.007843851441979916850, 0.008823947846603241024, 0.009804044251226563464, 0.01078414065584988764, 0.01176423706047321008, 0.01274433346509653425, 0.01372442986971985843, 0.01470452627434318260, 0.01568462267896650331, 0.01666471908358983095, 0.01764481548821315166, 0.01862491189283647583, 0.01960500829745980000, 0.02058510470208312071, 0.02156520110670644835, 0.02254529751132976906, 0.02352539391595309323 ),
 .UNSPECIFIED. ) ;
#40992 = CARTESIAN_POINT ( 'NONE',  ( 103.5588133492864813, 25.91050225236391213, 60.51647513232768461 ) ) ;
#40993 = CARTESIAN_POINT ( 'NONE',  ( 164.8942204024298235, 63.66138186734711724, 64.85643587009047906 ) ) ;
#40994 = DIRECTION ( 'NONE',  ( -1.000000000000000000, 0.000000000000000000, 0.000000000000000000 ) ) ;
#40995 = AXIS2_PLACEMENT_3D ( 'NONE', #55066, #34685, #23435 ) ;
#40996 = TOROIDAL_SURFACE ( 'NONE', #67968, 20.30000000000000071, 0.3000000000000062061 ) ;
#40997 = PLANE ( 'NONE',  #38224 ) ;
#40998 = CARTESIAN_POINT ( 'NONE',  ( 16.27765348919936983, 6.516472002017811072, 30.01470767270521733 ) ) ;
#40999 = AXIS2_PLACEMENT_3D ( 'NONE', #14370, #30891, #67839 ) ;
#41000 = CARTESIAN_POINT ( 'NONE',  ( 11.05669727962759907, 0.000000000000000000, -27.88815958909220782 ) ) ;
#41001 = ORIENTED_EDGE ( 'NONE', *, *, #47179, .T. ) ;
#41002 = VERTEX_POINT ( 'NONE', #44562 ) ;
#41003 = VECTOR ( 'NONE', #49153, 1000.000000000000114 ) ;
#41004 = VERTEX_POINT ( 'NONE', #6576 ) ;
#41005 = CIRCLE ( 'NONE', #53323, 4.999999999999997335 ) ;
#41006 = CARTESIAN_POINT ( 'NONE',  ( -154.0716379918897303, 69.49957566103795159, -21.43849890716462170 ) ) ;
#41007 = CARTESIAN_POINT ( 'NONE',  ( 176.4195038744034605, 74.01628939311422073, -91.52755031942164976 ) ) ;
#41008 = CARTESIAN_POINT ( 'NONE',  ( 63.50528314073025626, 12.78634332146812547, -35.72069083216974406 ) ) ;
#41009 = CARTESIAN_POINT ( 'NONE',  ( 106.9483136162804584, -21.63883973695288887, 3.974316929722046865 ) ) ;
#41010 = DIRECTION ( 'NONE',  ( -0.8118923937861950435, -0.5838071093367415143, 0.000000000000000000 ) ) ;
#41011 = CARTESIAN_POINT ( 'NONE',  ( -38.68632430131781774, 11.91908191268692008, -67.71530391917285385 ) ) ;
#41012 = CARTESIAN_POINT ( 'NONE',  ( 32.67604596315972287, 7.629767358313825021, 60.93075647368799252 ) ) ;
#41013 = CARTESIAN_POINT ( 'NONE',  ( 46.51849888769739039, 9.442121512056541377, 93.49346967249300633 ) ) ;
#41014 = EDGE_LOOP ( 'NONE', ( #4933, #16317, #53691, #18377 ) ) ;
#41015 = CARTESIAN_POINT ( 'NONE',  ( -0.7174461528505763352, 6.532311451815526304, -40.51236224071276126 ) ) ;
#41016 = DIRECTION ( 'NONE',  ( -1.001917834450843231E-14, 1.000000000000000000, -7.216449660063517513E-16 ) ) ;
#41017 = CARTESIAN_POINT ( 'NONE',  ( -120.4586945679390766, 43.01762219615313398, 16.46653791979410641 ) ) ;
#41018 = CARTESIAN_POINT ( 'NONE',  ( 311.9975424824652350, 296.0000000000000000, 420.0000000000000000 ) ) ;
#41019 = DIRECTION ( 'NONE',  ( 1.000000000000000000, 0.000000000000000000, 0.000000000000000000 ) ) ;
#41020 = CARTESIAN_POINT ( 'NONE',  ( 16.28382582968307446, 7.523443033994206885, -8.674393508222102867 ) ) ;
#41021 = CARTESIAN_POINT ( 'NONE',  ( 11.21312910819263031, 7.403355431337016235, 4.706771331900731603 ) ) ;
#41022 = VERTEX_POINT ( 'NONE', #37892 ) ;
#41023 = SHAPE_DEFINITION_REPRESENTATION ( #55202, #38847 ) ;
#41024 = CARTESIAN_POINT ( 'NONE',  ( 131.3924949472283004, 41.12442122814099577, -50.61069983280304285 ) ) ;
#41025 = DIRECTION ( 'NONE',  ( -1.001915251000354105E-14, 1.000000000000000000, -5.551115123125782702E-17 ) ) ;
#41026 = CYLINDRICAL_SURFACE ( 'NONE', #20003, 7.500000000000013323 ) ;
#41027 = CONTEXT_DEPENDENT_SHAPE_REPRESENTATION ( #67430, #59597 ) ;
#41028 = CARTESIAN_POINT ( 'NONE',  ( 187.8965227056806953, 87.27289477191493461, -40.57622610538386709 ) ) ;
#41029 = ORIENTED_EDGE ( 'NONE', *, *, #33633, .T. ) ;
#41030 = VERTEX_POINT ( 'NONE', #59672 ) ;
#41031 = DIRECTION ( 'NONE',  ( 0.000000000000000000, 0.000000000000000000, -1.000000000000000000 ) ) ;
#41032 = CARTESIAN_POINT ( 'NONE',  ( 197.9868529032975744, 99.18611233336801547, 6.502487484275444096 ) ) ;
#41033 = EDGE_LOOP ( 'NONE', ( #18772, #50069, #55433, #54774 ) ) ;
#41034 = VECTOR ( 'NONE', #46514, 1000.000000000000000 ) ;
#41035 = CARTESIAN_POINT ( 'NONE',  ( 153.7637790416463872, 56.08283792975861815, 84.07092255572784723 ) ) ;
#41036 = ORIENTED_EDGE ( 'NONE', *, *, #14894, .F. ) ;
#41037 = CARTESIAN_POINT ( 'NONE',  ( -56.02289203441038268, 15.98631679403369965, 18.42565426861631650 ) ) ;
#41038 = CARTESIAN_POINT ( 'NONE',  ( 126.4324872316703363, 37.11876756822025669, 38.10631402826915348 ) ) ;
#41039 = VECTOR ( 'NONE', #52476, 1000.000000000000000 ) ;
#41040 = CARTESIAN_POINT ( 'NONE',  ( -154.0833774771448361, 69.51012195447349029, 44.18219951439326820 ) ) ;
#41042 = EDGE_CURVE ( 'NONE', #27439, #6794, #53262, .T. ) ;
#41041 = CARTESIAN_POINT ( 'NONE',  ( -98.69283175933883001, 30.99524616306737812, 31.41528330781012102 ) ) ;
#41043 = VECTOR ( 'NONE', #48402, 1000.000000000000000 ) ;
#41045 = DIRECTION ( 'NONE',  ( -1.000000000000000000, -4.565061778886334783E-18, -0.000000000000000000 ) ) ;
#41044 = AXIS2_PLACEMENT_3D ( 'NONE', #2282, #55026, #23037 ) ;
#41047 = EDGE_LOOP ( 'NONE', ( #40458, #24839, #66252, #48348 ) ) ;
#41046 = DIRECTION ( 'NONE',  ( -0.000000000000000000, 1.000000000000000000, -0.000000000000000000 ) ) ;
#41048 = CARTESIAN_POINT ( 'NONE',  ( 204.6977192012829789, -170.0000000000000000, -16.98138044215791354 ) ) ;
#41049 = AXIS2_PLACEMENT_3D ( 'NONE', #30498, #41407, #51951 ) ;
#41050 = ADVANCED_FACE ( 'NONE', ( #43152 ), #12552, .T. ) ;
#41051 = ORIENTED_EDGE ( 'NONE', *, *, #21428, .T. ) ;
#41052 = ORIENTED_EDGE ( 'NONE', *, *, #3924, .F. ) ;
#41053 = CARTESIAN_POINT ( 'NONE',  ( 173.8576514579035575, 72.97529922124006418, 38.83678981078923442 ) ) ;
#41054 = AXIS2_PLACEMENT_3D ( 'NONE', #12339, #22890, #44333 ) ;
#41055 = EDGE_CURVE ( 'NONE', #30681, #17378, #28374, .T. ) ;
#41056 = CARTESIAN_POINT ( 'NONE',  ( 19.54475376904848360, 6.649964688461121654, -63.36740267540860572 ) ) ;
#41058 = ORIENTED_EDGE ( 'NONE', *, *, #25273, .F. ) ;
#41057 = CARTESIAN_POINT ( 'NONE',  ( -133.0835080491125098, 52.64966140620840918, 62.81293648280888675 ) ) ;
#41059 = FACE_OUTER_BOUND ( 'NONE', #49235, .T. ) ;
#41061 = EDGE_CURVE ( 'NONE', #29607, #17632, #49113, .T. ) ;
#41060 = MANIFOLD_SOLID_BREP ( 'Boss-Extrude1', #21561 ) ;
#41062 = CARTESIAN_POINT ( 'NONE',  ( 41.66904755831208007, -15.55634918610412853, 85.00100000000000477 ) ) ;
#41063 = ORIENTED_EDGE ( 'NONE', *, *, #39166, .F. ) ;
#41064 = CARTESIAN_POINT ( 'NONE',  ( 0.000000000000000000, 0.000000000000000000, 0.000000000000000000 ) ) ;
#41065 = CARTESIAN_POINT ( 'NONE',  ( 141.0517870458594132, 47.14452711594498879, 39.14317607914329500 ) ) ;
#41066 = CARTESIAN_POINT ( 'NONE',  ( 115.0606351894211485, 32.29586232625066344, 31.34211210427034899 ) ) ;
#41067 = CARTESIAN_POINT ( 'NONE',  ( 109.9975424824652634, 171.8183490441642789, 533.9018882243741473 ) ) ;
#41068 = CARTESIAN_POINT ( 'NONE',  ( -101.3602137809054540, 32.31558061113913283, -76.81699020212612083 ) ) ;
#41069 = EDGE_CURVE ( 'NONE', #12143, #56454, #22055, .T. ) ;
#41070 = ORIENTED_EDGE ( 'NONE', *, *, #13596, .F. ) ;
#41071 = ORIENTED_EDGE ( 'NONE', *, *, #20805, .F. ) ;
#41072 = CARTESIAN_POINT ( 'NONE',  ( -147.3669217311067712, 63.69361261596466761, -22.65969703386014800 ) ) ;
#41073 = CARTESIAN_POINT ( 'NONE',  ( 15.55634918610396511, -41.66904755831214402, 85.00100000000000477 ) ) ;
#41074 = CARTESIAN_POINT ( 'NONE',  ( -23.73638277007033182, -7.847555861075553807, 0.000000000000000000 ) ) ;
#41075 = DIRECTION ( 'NONE',  ( 1.387778780781445922E-16, -1.000000000000000000, -3.469446951953615421E-17 ) ) ;
#41076 = CARTESIAN_POINT ( 'NONE',  ( -47.76881570271230970, 13.88249791001275391, -94.56390181705104681 ) ) ;
#41077 = LINE ( 'NONE', #3106, #15782 ) ;
#41078 = CARTESIAN_POINT ( 'NONE',  ( 0.000000000000000000, 6.928203230275505220, -4.000000000000007994 ) ) ;
#41079 = CARTESIAN_POINT ( 'NONE',  ( -120.5002574492098688, 44.22930148497319891, 43.33742215016130217 ) ) ;
#41080 = CARTESIAN_POINT ( 'NONE',  ( 208.5889601154908632, 111.8333159387241693, 57.12700094515400906 ) ) ;
#41081 = VERTEX_POINT ( 'NONE', #18872 ) ;
#41082 = CARTESIAN_POINT ( 'NONE',  ( -107.7886332494339854, 36.81249801143972178, 43.13215690507624345 ) ) ;
#41083 = ORIENTED_EDGE ( 'NONE', *, *, #22534, .T. ) ;
#41084 = CIRCLE ( 'NONE', #6264, 65.36598343705435354 ) ;
#41085 = CARTESIAN_POINT ( 'NONE',  ( 83.52009074181535198, 19.44074360878495966, -90.13814207189352601 ) ) ;
#41086 = CARTESIAN_POINT ( 'NONE',  ( -31.11269837220812207, -31.11269837220801193, 2.000000000000001776 ) ) ;
#41087 = ORIENTED_EDGE ( 'NONE', *, *, #5937, .T. ) ;
#41088 = CARTESIAN_POINT ( 'NONE',  ( 204.6977192012829789, 106.3443248447423599, 2.363170148305747009 ) ) ;
#41089 = FACE_OUTER_BOUND ( 'NONE', #46551, .T. ) ;
#41090 = CARTESIAN_POINT ( 'NONE',  ( 8.000000000000007105, 249.8719672152120381, -95.00000000000133582 ) ) ;
#41092 = SURFACE_STYLE_USAGE ( .BOTH. , #46352 ) ;
#41091 = VECTOR ( 'NONE', #40821, 1000.000000000000114 ) ;
#41093 = CARTESIAN_POINT ( 'NONE',  ( 33.03722315490662709, 7.666819786578629170, 14.54433801149057537 ) ) ;
#41094 = CARTESIAN_POINT ( 'NONE',  ( -11.79249160485393766, 8.191429102467035150, -36.54839574459859364 ) ) ;
#41095 = CARTESIAN_POINT ( 'NONE',  ( -2.116120943112233643, 74.98056102853672655, 170.0000000000000000 ) ) ;
#41096 = AXIS2_PLACEMENT_3D ( 'NONE', #43068, #64893, #64540 ) ;
#41097 = AXIS2_PLACEMENT_3D ( 'NONE', #11685, #32115, #37375 ) ;
#41098 = ORIENTED_EDGE ( 'NONE', *, *, #40811, .T. ) ;
#41099 = CARTESIAN_POINT ( 'NONE',  ( 0.000000000000000000, 0.000000000000000000, 170.0000000000000000 ) ) ;
#41100 = VERTEX_POINT ( 'NONE', #3384 ) ;
#41101 = CARTESIAN_POINT ( 'NONE',  ( -13.24252603915608617, 63.63674649211943546, 73.58025477438756923 ) ) ;
#41102 = CARTESIAN_POINT ( 'NONE',  ( -62.29496909743952671, 17.79481128341708285, 66.62724933386981263 ) ) ;
#41103 = CARTESIAN_POINT ( 'NONE',  ( -30.95355748062275936, 9.511738996772322707, 3.371903815725488140 ) ) ;
#41104 = VERTEX_POINT ( 'NONE', #66728 ) ;
#41105 = LINE ( 'NONE', #50966, #32246 ) ;
#41106 = CIRCLE ( 'NONE', #56876, 65.36598343705435354 ) ;
#41107 = DIRECTION ( 'NONE',  ( -1.000000000000000000, 0.000000000000000000, 0.000000000000000000 ) ) ;
#41108 = CARTESIAN_POINT ( 'NONE',  ( -38.92726670956012924, 10.94099576009806718, 37.22770458825116435 ) ) ;
#41109 =( BOUNDED_CURVE ( )  B_SPLINE_CURVE ( 3, ( #21182, #9246, #32079, #52153 ),
 .UNSPECIFIED., .F., .F. ) 
 B_SPLINE_CURVE_WITH_KNOTS ( ( 4, 4 ),
 ( 1.570796326794906772, 3.141592653589769135 ),
 .UNSPECIFIED. ) 
 CURVE ( )  GEOMETRIC_REPRESENTATION_ITEM ( )  RATIONAL_B_SPLINE_CURVE ( ( 1.000000000000000000, 0.8047378541243730421, 0.8047378541243730421, 1.000000000000000000 ) ) 
 REPRESENTATION_ITEM ( '' )  );
#41110 = VERTEX_POINT ( 'NONE', #34713 ) ;
#41111 = DIRECTION ( 'NONE',  ( 9.762711664770453435E-15, -2.336779715407619548E-15, 1.000000000000000000 ) ) ;
#41112 = DIRECTION ( 'NONE',  ( 0.000000000000000000, -5.102127870520020458E-18, -1.000000000000000000 ) ) ;
#41113 = CARTESIAN_POINT ( 'NONE',  ( 180.6713229637342693, 79.61878926895393249, -24.38050707541595941 ) ) ;
#41114 = DIRECTION ( 'NONE',  ( 1.000000000000000000, 2.263859959510412882E-16, -1.697894969632809662E-16 ) ) ;
#41115 = CARTESIAN_POINT ( 'NONE',  ( 0.000000000000000000, 0.000000000000000000, 85.00000000000000000 ) ) ;
#41116 = ORIENTED_EDGE ( 'NONE', *, *, #23269, .T. ) ;
#41117 = CARTESIAN_POINT ( 'NONE',  ( -180.6215424137752166, 97.48070480470860844, -68.75056467222114520 ) ) ;
#41118 = EDGE_CURVE ( 'NONE', #15890, #22095, #45943, .T. ) ;
#41119 = CARTESIAN_POINT ( 'NONE',  ( 134.5432377632815815, 43.01906612978911681, 83.22447129036004299 ) ) ;
#41120 = CARTESIAN_POINT ( 'NONE',  ( 117.0065308422768453, 32.13872219870568614, 33.86034543354286086 ) ) ;
#41121 = DIRECTION ( 'NONE',  ( 0.000000000000000000, 0.000000000000000000, 1.000000000000000000 ) ) ;
#41122 = VERTEX_POINT ( 'NONE', #2353 ) ;
#41123 = LINE ( 'NONE', #8783, #54712 ) ;
#41124 = CARTESIAN_POINT ( 'NONE',  ( -57.08057067389502492, 19.16407787157944398, 38.91942932610496797 ) ) ;
#41125 = CARTESIAN_POINT ( 'NONE',  ( 188.4365915667139006, 87.87248959723054043, 38.31765364999172618 ) ) ;
#41126 = CARTESIAN_POINT ( 'NONE',  ( 139.3041645503688528, 46.00819478311335331, 5.004763042418960417 ) ) ;
#41127 = DIRECTION ( 'NONE',  ( 0.000000000000000000, 0.000000000000000000, 1.000000000000000000 ) ) ;
#41128 = EDGE_LOOP ( 'NONE', ( #26468, #49960, #60513, #9688 ) ) ;
#41129 = CARTESIAN_POINT ( 'NONE',  ( 159.6614743841975042, 60.66237087206236822, -23.96642233299556324 ) ) ;
#41130 = ADVANCED_FACE ( 'NONE', ( #39630 ), #28479, .T. ) ;
#41131 = ORIENTED_EDGE ( 'NONE', *, *, #68661, .T. ) ;
#41132 = AXIS2_PLACEMENT_3D ( 'NONE', #40, #37328, #69348 ) ;
#41133 = DIRECTION ( 'NONE',  ( 0.000000000000000000, 1.000000000000000000, -0.000000000000000000 ) ) ;
#41134 = CARTESIAN_POINT ( 'NONE',  ( 140.6546466870198628, 45.68345804077596739, 87.51171208969724091 ) ) ;
#41135 = VECTOR ( 'NONE', #53003, 1000.000000000000114 ) ;
#41137 = VERTEX_POINT ( 'NONE', #61435 ) ;
#41136 = CARTESIAN_POINT ( 'NONE',  ( 155.2992895652388086, 57.24699634758579236, 2.872173225997780133 ) ) ;
#41138 = CARTESIAN_POINT ( 'NONE',  ( 161.7006237583813970, 62.31514460450499371, -49.83437428245752443 ) ) ;
#41139 = EDGE_CURVE ( 'NONE', #25048, #54323, #7968, .T. ) ;
#41140 = CARTESIAN_POINT ( 'NONE',  ( 26.99999999999999645, -27.00000000000000355, 12.00000000000000000 ) ) ;
#41141 = CARTESIAN_POINT ( 'NONE',  ( 162.7921669283191477, 61.91024532638673605, -48.91460448534603955 ) ) ;
#41142 = AXIS2_PLACEMENT_3D ( 'NONE', #1571, #23039, #39907 ) ;
#41143 = AXIS2_PLACEMENT_3D ( 'NONE', #38340, #59783, #11594 ) ;
#41144 = ORIENTED_EDGE ( 'NONE', *, *, #28417, .F. ) ;
#41145 = PRODUCT_DEFINITION_FORMATION_WITH_SPECIFIED_SOURCE ( 'ANY', '', #59083, .NOT_KNOWN. ) ;
#41146 = DIRECTION ( 'NONE',  ( -0.000000000000000000, -0.000000000000000000, 1.000000000000000000 ) ) ;
#41147 = VECTOR ( 'NONE', #19525, 1000.000000000000000 ) ;
#41148 = CARTESIAN_POINT ( 'NONE',  ( 31.11269837220800127, -31.11269837220812562, 0.000000000000000000 ) ) ;
#41149 = DIRECTION ( 'NONE',  ( 0.5508969814521065267, -0.8345732537212999791, 0.000000000000000000 ) ) ;
#41150 = VECTOR ( 'NONE', #39440, 1000.000000000000000 ) ;
#41151 = CARTESIAN_POINT ( 'NONE',  ( 0.000000000000000000, 0.000000000000000000, 43.58025477438756212 ) ) ;
#41152 = CARTESIAN_POINT ( 'NONE',  ( -9.964117946889912147, 64.24592483216710548, 41.38025477438755928 ) ) ;
#41153 = CARTESIAN_POINT ( 'NONE',  ( 149.9872551245001091, 52.05943539582077761, 64.32859008368343723 ) ) ;
#41154 = DIRECTION ( 'NONE',  ( 0.000000000000000000, 0.000000000000000000, 1.000000000000000000 ) ) ;
#41155 = EDGE_CURVE ( 'NONE', #7827, #53047, #21734, .T. ) ;
#41156 = ORIENTED_EDGE ( 'NONE', *, *, #69324, .F. ) ;
#41157 = CARTESIAN_POINT ( 'NONE',  ( -94.83794676023106263, 30.26879337035743944, 65.92642283735828812 ) ) ;
#41158 = CARTESIAN_POINT ( 'NONE',  ( -13.47517652744367034, 8.334971000693553123, 69.41689693878558387 ) ) ;
#41159 = ORIENTED_EDGE ( 'NONE', *, *, #54955, .T. ) ;
#41160 = EDGE_CURVE ( 'NONE', #41997, #64948, #12913, .T. ) ;
#41161 = EDGE_CURVE ( 'NONE', #52056, #30082, #45789, .T. ) ;
#41162 = DIRECTION ( 'NONE',  ( -1.000000000000000000, 0.000000000000000000, 0.000000000000000000 ) ) ;
#41163 = CARTESIAN_POINT ( 'NONE',  ( 204.6977192012829505, 108.0580384837234931, -24.48138044215792419 ) ) ;
#41164 = CARTESIAN_POINT ( 'NONE',  ( 103.5849290181278803, 27.01613348792541913, 33.64945997442609382 ) ) ;
#41165 = DIRECTION ( 'NONE',  ( -1.000000000000000000, 0.000000000000000000, 0.000000000000000000 ) ) ;
#41166 = CARTESIAN_POINT ( 'NONE',  ( -55.05276343752909440, 15.72344139423348430, -23.37177340799619785 ) ) ;
#41167 = CARTESIAN_POINT ( 'NONE',  ( 188.4920037102894241, 87.93425473911916868, 11.17357535198952867 ) ) ;
#41168 = CARTESIAN_POINT ( 'NONE',  ( 211.3917124729450734, 115.9987099435923597, -40.43198958513412578 ) ) ;
#41169 = CARTESIAN_POINT ( 'NONE',  ( 178.1999009735081358, 75.73911533785327777, 16.89086260446840981 ) ) ;
#41170 = CARTESIAN_POINT ( 'NONE',  ( -58.32860549785896609, 15.58423118879329472, 4.221608677645580343 ) ) ;
#41171 = VERTEX_POINT ( 'NONE', #35051 ) ;
#41172 = CYLINDRICAL_SURFACE ( 'NONE', #9418, 164.5210298272983778 ) ;
#41173 = ORIENTED_EDGE ( 'NONE', *, *, #16493, .F. ) ;
#41174 = CARTESIAN_POINT ( 'NONE',  ( 102.7425154123292828, 25.56407025871219219, -70.50869499390829276 ) ) ;
#41175 = CARTESIAN_POINT ( 'NONE',  ( 41.80372346091802882, 9.750024116765237281, -9.166004075864405465 ) ) ;
#41176 = CARTESIAN_POINT ( 'NONE',  ( 31.11269837220809364, 15.55634918610396866, 85.00100000000000477 ) ) ;
#41177 = CARTESIAN_POINT ( 'NONE',  ( 40.13282190615316836, 1.842283050316774879E-12, -5.000000000000000000 ) ) ;
#41178 = CARTESIAN_POINT ( 'NONE',  ( -0.7270333525066480229, 6.532611081232851724, 93.81168647148426487 ) ) ;
#41179 = CARTESIAN_POINT ( 'NONE',  ( -106.6711220790663077, 36.20923238211246797, -21.75507159268790147 ) ) ;
#41180 = VERTEX_POINT ( 'NONE', #40320 ) ;
#41181 = CARTESIAN_POINT ( 'NONE',  ( -72.76696720809546548, 20.16136115364205494, 69.42024918034346115 ) ) ;
#41182 = CARTESIAN_POINT ( 'NONE',  ( -166.2028657618940599, 79.74389853943287676, 68.07680179289491207 ) ) ;
#41183 = ORIENTED_EDGE ( 'NONE', *, *, #34739, .F. ) ;
#41184 = ORIENTED_EDGE ( 'NONE', *, *, #45812, .F. ) ;
#41185 = CARTESIAN_POINT ( 'NONE',  ( -152.5046761101291963, 66.76407727525177904, 45.09959997925059838 ) ) ;
#41186 = DIRECTION ( 'NONE',  ( -0.000000000000000000, -0.000000000000000000, -1.000000000000000000 ) ) ;
#41187 = CARTESIAN_POINT ( 'NONE',  ( 176.0745160362857860, 73.68684431790052258, -11.29378876841035684 ) ) ;
#41188 = VECTOR ( 'NONE', #68910, 1000.000000000000000 ) ;
#41189 = DIRECTION ( 'NONE',  ( -5.333935875449778863E-17, 1.000000000000000000, 6.106226635438359986E-16 ) ) ;
#41190 = VECTOR ( 'NONE', #33830, 1000.000000000000000 ) ;
#41191 = ORIENTED_EDGE ( 'NONE', *, *, #41837, .F. ) ;
#41192 = DIRECTION ( 'NONE',  ( -0.000000000000000000, -0.000000000000000000, -1.000000000000000000 ) ) ;
#41193 = VECTOR ( 'NONE', #22951, 1000.000000000000000 ) ;
#41194 = ORIENTED_EDGE ( 'NONE', *, *, #46995, .T. ) ;
#41195 = CARTESIAN_POINT ( 'NONE',  ( 207.8484262634767674, 110.7633525054914401, 3.044159929133792186 ) ) ;
#41196 = CARTESIAN_POINT ( 'NONE',  ( 8.336237313193162635, 7.382629160459399209, 65.33688261179428025 ) ) ;
#41197 = CARTESIAN_POINT ( 'NONE',  ( 211.5175447467296408, 116.1901475271413915, 39.84285645812254018 ) ) ;
#41198 = ADVANCED_FACE ( 'NONE', ( #50873 ), #29766, .F. ) ;
#41199 = FACE_BOUND ( 'NONE', #30457, .T. ) ;
#41200 = CARTESIAN_POINT ( 'NONE',  ( 68.11829950231073383, 13.91429225309574313, 85.49552249958776429 ) ) ;
#41201 = ADVANCED_FACE ( 'NONE', ( #13254, #61086 ), #28733, .F. ) ;
#41202 = CIRCLE ( 'NONE', #62547, 65.36598343705435354 ) ;
#41203 = ORIENTED_EDGE ( 'NONE', *, *, #23784, .T. ) ;
#41204 = VERTEX_POINT ( 'NONE', #56493 ) ;
#41205 = CARTESIAN_POINT ( 'NONE',  ( 113.7666631852362542, -21.75169080623576079, -3.304315882619072831 ) ) ;
#41206 = CARTESIAN_POINT ( 'NONE',  ( -119.4731043141009792, 43.59103079130043312, 87.91918064160569202 ) ) ;
#41207 = CARTESIAN_POINT ( 'NONE',  ( -165.6398193834832284, 79.16932278174802207, -15.97813448833655592 ) ) ;
#41208 = DIRECTION ( 'NONE',  ( -0.000000000000000000, 1.000000000000000000, -0.000000000000000000 ) ) ;
#41209 = CARTESIAN_POINT ( 'NONE',  ( 22.13124724433581392, 6.786568030646046523, 87.18837163059359341 ) ) ;
#41210 = CARTESIAN_POINT ( 'NONE',  ( 23.12438659259228046, 7.854523583799140063, 89.61051317704388453 ) ) ;
#41211 = ORIENTED_EDGE ( 'NONE', *, *, #52767, .F. ) ;
#41213 = ADVANCED_FACE ( 'NONE', ( #55815 ), #34012, .T. ) ;
#41212 = DIRECTION ( 'NONE',  ( 0.000000000000000000, 0.000000000000000000, 1.000000000000000000 ) ) ;
#41214 = CARTESIAN_POINT ( 'NONE',  ( 199.9103251464698303, 101.6434290204574893, -38.04802015360730394 ) ) ;
#41215 = ORIENTED_EDGE ( 'NONE', *, *, #7929, .T. ) ;
#41216 = ADVANCED_FACE ( 'NONE', ( #46280, #3047 ), #19201, .T. ) ;
#41217 = FACE_OUTER_BOUND ( 'NONE', #24542, .T. ) ;
#41218 = VERTEX_POINT ( 'NONE', #67757 ) ;
#41219 = CARTESIAN_POINT ( 'NONE',  ( -59.58556642339446796, 16.99097764963620705, -9.876509403717985691 ) ) ;
#41220 = B_SPLINE_CURVE_WITH_KNOTS ( 'NONE', 3,
 ( #31555, #68826, #4141, #20649, #63568, #56918, #36148, #8734, #20304, #68500, #67815, #25607, #36840, #15381, #35806, #41769, #52993, #4814, #46005, #67471, #19266, #40719, #30183, #19618, #62539, #57258, #9071, #30524, #3786, #25256, #63909, #10434, #26629, #43479, #47718, #11129, #15723, #31904, #48389, #65300, #64254, #27302, #37869, #53335 ),
 .UNSPECIFIED., .F., .F.,
 ( 4, 2, 2, 2, 2, 2, 2, 2, 2, 2, 2, 2, 2, 2, 2, 2, 2, 2, 2, 2, 2, 4 ),
 ( 0.000000000000000000, 0.001487235713946800280, 0.002230853570920181446, 0.002974471427893562395, 0.004461707141840288299, 0.005948942855787013768, 0.007436178569733738371, 0.008179796426707101539, 0.008923414283680465575, 0.01041064999762722661, 0.01189788571157398590, 0.01264150356854737769, 0.01338512142552076949, 0.01487235713946754440, 0.01561597499644093792, 0.01635959285341433492, 0.01784682856736112197, 0.01933406428130791249, 0.02007768213828130602, 0.02082129999525470301, 0.02230853570920150047, 0.02379577142314829794 ),
 .UNSPECIFIED. ) ;
#41221 = ORIENTED_EDGE ( 'NONE', *, *, #4654, .F. ) ;
#41222 = ADVANCED_FACE ( 'NONE', ( #13933 ), #29086, .T. ) ;
#41223 = VERTEX_POINT ( 'NONE', #62471 ) ;
#41224 = CARTESIAN_POINT ( 'NONE',  ( 8.480442907658520824, 6.376693431076494889, -41.31410600788661469 ) ) ;
#41225 = ADVANCED_FACE ( 'NONE', ( #50533 ), #30810, .F. ) ;
#41226 = CARTESIAN_POINT ( 'NONE',  ( -32.68347998332510684, -12.52158680757305298, 0.000000000000000000 ) ) ;
#41227 = CARTESIAN_POINT ( 'NONE',  ( 108.3753929817421238, 29.13179266688724312, 17.54579741615193100 ) ) ;
#41228 = EDGE_LOOP ( 'NONE', ( #6870, #57262, #54007, #1059 ) ) ;
#41229 = PRODUCT_DEFINITION_SHAPE ( 'NONE', 'NONE',  #69596 ) ;
#41230 = CARTESIAN_POINT ( 'NONE',  ( -24.01932733213275739, 8.490648912832073236, 92.54723777928531092 ) ) ;
#41231 = VECTOR ( 'NONE', #60463, 1000.000000000000000 ) ;
#41232 = CARTESIAN_POINT ( 'NONE',  ( 180.2565361171340896, 79.19912802278403774, -78.03579697056984799 ) ) ;
#41233 = LINE ( 'NONE', #62694, #65130 ) ;
#41234 = CARTESIAN_POINT ( 'NONE',  ( 107.2672065034543465, 27.52931006625853172, -50.31091384885557716 ) ) ;
#41235 = ADVANCED_FACE ( 'NONE', ( #15317 ), #52595, .T. ) ;
#41236 = LINE ( 'NONE', #35953, #68030 ) ;
#41237 = AXIS2_PLACEMENT_3D ( 'NONE', #58641, #31933, #6221 ) ;
#41238 = DIRECTION ( 'NONE',  ( -0.6910626489868685329, 0.7227948638273878901, 0.000000000000000000 ) ) ;
#41239 = EDGE_LOOP ( 'NONE', ( #38883, #50238 ) ) ;
#41240 = EDGE_CURVE ( 'NONE', #59777, #21604, #1511, .T. ) ;
#41241 = EDGE_CURVE ( 'NONE', #37573, #38237, #50902, .T. ) ;
#41242 = VECTOR ( 'NONE', #67020, 1000.000000000000114 ) ;
#41243 = EDGE_LOOP ( 'NONE', ( #10568, #60782, #52572, #11880 ) ) ;
#41244 = CARTESIAN_POINT ( 'NONE',  ( -85.89078989036967471, 26.29712602777652819, -71.49050017303922289 ) ) ;
#41245 = CARTESIAN_POINT ( 'NONE',  ( -2.460717450366728620, 6.600113625476148549, -91.29677748862752651 ) ) ;
#41246 = DIRECTION ( 'NONE',  ( 0.000000000000000000, 1.000000000000000000, -0.000000000000000000 ) ) ;
#41247 = CARTESIAN_POINT ( 'NONE',  ( 15.55634918610406103, 15.55634918610400241, 85.00100000000000477 ) ) ;
#41248 = AXIS2_PLACEMENT_3D ( 'NONE', #18946, #56574, #8749 ) ;
#41249 = CARTESIAN_POINT ( 'NONE',  ( 127.2202105166096402, 37.55913282978157497, 6.662491736991211333 ) ) ;
#41250 = CARTESIAN_POINT ( 'NONE',  ( 36.01249374622354082, 7.992843789158042611, -90.11533793215521371 ) ) ;
#41251 = LINE ( 'NONE', #68656, #14826 ) ;
#41252 = CARTESIAN_POINT ( 'NONE',  ( 204.6977192012829789, -170.0000000000000000, 56.05227132923312183 ) ) ;
#41253 = CARTESIAN_POINT ( 'NONE',  ( -15.55634918610400597, 15.55634918610405748, 85.00100000000000477 ) ) ;
#41254 = CARTESIAN_POINT ( 'NONE',  ( -105.8879439778144445, 34.65133284149107595, 31.42656481232496901 ) ) ;
#41255 = VERTEX_POINT ( 'NONE', #25880 ) ;
#41256 = VECTOR ( 'NONE', #22632, 1000.000000000000000 ) ;
#41257 = CARTESIAN_POINT ( 'NONE',  ( 8.288696687633807514, 7.382586467017839382, -16.67527755506199938 ) ) ;
#41258 = ORIENTED_EDGE ( 'NONE', *, *, #21752, .T. ) ;
#41259 = CARTESIAN_POINT ( 'NONE',  ( -3.325451350920383131E-15, 6.534749472788146107, 4.681481898397001906 ) ) ;
#41260 = ORIENTED_EDGE ( 'NONE', *, *, #29314, .T. ) ;
#41261 = CARTESIAN_POINT ( 'NONE',  ( -149.0764453401867229, 65.13297611514535390, 3.876270649435373805 ) ) ;
#41262 = CARTESIAN_POINT ( 'NONE',  ( 0.000000000000000000, 0.000000000000000000, 0.000000000000000000 ) ) ;
#41263 = DIRECTION ( 'NONE',  ( 0.000000000000000000, 0.000000000000000000, 1.000000000000000000 ) ) ;
#41264 = CARTESIAN_POINT ( 'NONE',  ( 5.799999999999999822, 4.618802153517004960, 7.999999999999998224 ) ) ;
#41265 = CARTESIAN_POINT ( 'NONE',  ( 33.44527180510249309, 7.709232309484704615, -47.70323226738239697 ) ) ;
#41266 = CARTESIAN_POINT ( 'NONE',  ( -439.4229916354183842, 400.0000000000021032, 101.0502958579930066 ) ) ;
#41267 = CARTESIAN_POINT ( 'NONE',  ( 8.540564391411910705, 7.383006541823031732, -44.96353512608188652 ) ) ;
#41268 = DIRECTION ( 'NONE',  ( 0.000000000000000000, 0.000000000000000000, 1.000000000000000000 ) ) ;
#41269 = ORIENTED_EDGE ( 'NONE', *, *, #24502, .F. ) ;
#41270 = ORIENTED_EDGE ( 'NONE', *, *, #42961, .F. ) ;
#41271 = DIRECTION ( 'NONE',  ( -0.000000000000000000, 1.000000000000000000, -0.000000000000000000 ) ) ;
#41272 = DIRECTION ( 'NONE',  ( 0.000000000000000000, 0.000000000000000000, 1.000000000000000000 ) ) ;
#41273 = CARTESIAN_POINT ( 'NONE',  ( -25.98312968277007684, 8.759224980175259745, -74.81367083702784271 ) ) ;
#41274 = CARTESIAN_POINT ( 'NONE',  ( 8.528421445032394743, 6.376778749352033593, 8.724639706960820362 ) ) ;
#41275 = CARTESIAN_POINT ( 'NONE',  ( 42.71247067544614140, 9.879726907348448606, -76.69866368401555690 ) ) ;
#41276 = DIRECTION ( 'NONE',  ( 0.000000000000000000, 0.000000000000000000, 1.000000000000000000 ) ) ;
#41277 = CARTESIAN_POINT ( 'NONE',  ( 176.0745160362857860, 73.68684431790050837, -64.98288994933773211 ) ) ;
#41278 =( LENGTH_UNIT ( ) NAMED_UNIT ( * ) SI_UNIT ( .MILLI., .METRE. ) );
#41279 = CONICAL_SURFACE ( 'NONE', #68250, 8.000000000000001776, 1.047197551196595855 ) ;
#41280 = CARTESIAN_POINT ( 'NONE',  ( -176.3896317155480062, 90.84057090619019448, -48.97646663013337331 ) ) ;
#41281 = CARTESIAN_POINT ( 'NONE',  ( 91.13361825170460406, 21.00701373666981198, -10.46045707455249563 ) ) ;
#41282 = CARTESIAN_POINT ( 'NONE',  ( -26.49928411671542605, 9.848831533840664676, 70.22566193647604393 ) ) ;
#41283 = CARTESIAN_POINT ( 'NONE',  ( 106.0273295991593301, 21.78875652052166956, 3.053836096979983594 ) ) ;
#41284 = CARTESIAN_POINT ( 'NONE',  ( -36.84489839129265931, -53.54860840895233309, 170.0000000000000000 ) ) ;
#41285 = AXIS2_PLACEMENT_3D ( 'NONE', #7092, #28552, #66213 ) ;
#41286 = EDGE_CURVE ( 'NONE', #7422, #52011, #58352, .T. ) ;
#41287 = ORIENTED_EDGE ( 'NONE', *, *, #4434, .T. ) ;
#41288 = VECTOR ( 'NONE', #65324, 1000.000000000000000 ) ;
#41289 = DIRECTION ( 'NONE',  ( -0.000000000000000000, -1.000000000000000000, -0.000000000000000000 ) ) ;
#41290 = MANIFOLD_SOLID_BREP ( 'Boss-Extrude1', #48503 ) ;
#41291 = CARTESIAN_POINT ( 'NONE',  ( -127.6992109187851980, 47.69334801994793338, -76.55208594102460040 ) ) ;
#41292 = CARTESIAN_POINT ( 'NONE',  ( -1.740765657700568569, -66.62262621221535142, 34.48241823979275722 ) ) ;
#41293 = CARTESIAN_POINT ( 'NONE',  ( -47.68742944762956881, 12.82957801017945343, -41.23781885043871398 ) ) ;
#41294 = CARTESIAN_POINT ( 'NONE',  ( 0.000000000000000000, 0.000000000000000000, 41.38025477438755928 ) ) ;
#41295 = DIRECTION ( 'NONE',  ( 0.000000000000000000, -0.000000000000000000, -1.000000000000000000 ) ) ;
#41296 = AXIS2_PLACEMENT_3D ( 'NONE', #43974, #38720, #60166 ) ;
#41297 = ORIENTED_EDGE ( 'NONE', *, *, #65529, .F. ) ;
#41299 = ADVANCED_FACE ( 'NONE', ( #515 ), #46979, .F. ) ;
#41298 = PRESENTATION_STYLE_ASSIGNMENT (( #19840 ) ) ;
#41300 = DIRECTION ( 'NONE',  ( -0.000000000000000000, 1.000000000000000000, -0.000000000000000000 ) ) ;
#41301 = ORIENTED_EDGE ( 'NONE', *, *, #28692, .T. ) ;
#41302 = VECTOR ( 'NONE', #16913, 1000.000000000000000 ) ;
#41303 = VERTEX_POINT ( 'NONE', #48672 ) ;
#41304 = DIRECTION ( 'NONE',  ( 1.000000000000000000, 0.000000000000000000, -0.000000000000000000 ) ) ;
#41305 = CARTESIAN_POINT ( 'NONE',  ( -180.5230320745700965, 95.76406004447554210, -70.30535114727260293 ) ) ;
#41306 = CARTESIAN_POINT ( 'NONE',  ( 136.2687650510572155, 44.08481419469791263, -90.10835114847000682 ) ) ;
#41307 = EDGE_LOOP ( 'NONE', ( #13669, #2024, #24210, #54844 ) ) ;
#41308 = LINE ( 'NONE', #62415, #27805 ) ;
#41309 = EDGE_CURVE ( 'NONE', #69425, #43897, #1215, .T. ) ;
#41310 = CARTESIAN_POINT ( 'NONE',  ( 394.5137675702981710, 500.0000000000000000, -53.65523180892861177 ) ) ;
#41311 = DIRECTION ( 'NONE',  ( -0.000000000000000000, 1.000000000000000000, -0.000000000000000000 ) ) ;
#41312 = LINE ( 'NONE', #30070, #33152 ) ;
#41313 = CARTESIAN_POINT ( 'NONE',  ( -55.05276343752910151, -170.0000000000000000, 57.16187836339483397 ) ) ;
#41314 = CARTESIAN_POINT ( 'NONE',  ( -25.79929641484368830, 9.749255553662438345, -20.94138654446484438 ) ) ;
#41315 = LINE ( 'NONE', #62770, #26431 ) ;
#41316 = ORIENTED_EDGE ( 'NONE', *, *, #68737, .T. ) ;
#41317 = CARTESIAN_POINT ( 'NONE',  ( 107.0555969502564437, 28.53646637607230829, -23.38328407531912490 ) ) ;
#41318 = CARTESIAN_POINT ( 'NONE',  ( 11.21387192505587294, 6.397095920409659797, 58.39573670284872975 ) ) ;
#41319 = B_SPLINE_CURVE_WITH_KNOTS ( 'NONE', 3,
 ( #33422, #28837, #17212, #1397, #34115, #6673, #38686, #12302, #61189, #34473, #55203, #46734, #8778, #68205, #20013, #19307, #57986, #68541 ),
 .UNSPECIFIED., .F., .F.,
 ( 4, 2, 2, 2, 2, 2, 2, 2, 4 ),
 ( 0.000000000000000000, 0.001652083204940604571, 0.002478124807410915422, 0.003304166409881226056, 0.004956249614821870743, 0.006608332819762517164, 0.009912499229643743220, 0.01156458243458435668, 0.01321666563952497188 ),
 .UNSPECIFIED. ) ;
#41320 = CARTESIAN_POINT ( 'NONE',  ( -24.32471770265757982, 9.546495606312143778, 35.29174336063405804 ) ) ;
#41321 = CARTESIAN_POINT ( 'NONE',  ( 204.6977192012829505, 108.0580384837234931, 29.20772073876942088 ) ) ;
#41322 = DIRECTION ( 'NONE',  ( 1.001917982681609001E-14, -1.000000000000000000, -5.551115123125782702E-17 ) ) ;
#41324 = VERTEX_POINT ( 'NONE', #33587 ) ;
#41323 = CARTESIAN_POINT ( 'NONE',  ( 209.3223706822284100, 172.0000000000000284, 31.44247402469554942 ) ) ;
#41325 = DIRECTION ( 'NONE',  ( -0.000000000000000000, -6.405132834375902056E-16, 1.000000000000000000 ) ) ;
#41326 = VERTEX_POINT ( 'NONE', #17025 ) ;
#41327 = EDGE_CURVE ( 'NONE', #16476, #20392, #35216, .T. ) ;
#41328 = ORIENTED_EDGE ( 'NONE', *, *, #44105, .F. ) ;
#41329 = CARTESIAN_POINT ( 'NONE',  ( 110.7167338301703694, 30.21148223254618159, -62.76698815611733551 ) ) ;
#41330 = AXIS2_PLACEMENT_3D ( 'NONE', #7217, #66331, #23051 ) ;
#41331 = CARTESIAN_POINT ( 'NONE',  ( -452.6627218934913799, 0.000000000000000000, -146.4497041420118251 ) ) ;
#41332 = CARTESIAN_POINT ( 'NONE',  ( 197.8436586345020487, 97.39326576892288756, -73.76851244691899012 ) ) ;
#41333 = EDGE_CURVE ( 'NONE', #56977, #50492, #6835, .T. ) ;
#41334 = FACE_OUTER_BOUND ( 'NONE', #23219, .T. ) ;
#41335 = CARTESIAN_POINT ( 'NONE',  ( -118.4063383664799858, 41.75753822095644097, 65.47488579310427781 ) ) ;
#41336 = CARTESIAN_POINT ( 'NONE',  ( 75.00000000000000000, -1.250000000000021982, 43.58025477438756212 ) ) ;
#41337 = DIRECTION ( 'NONE',  ( -0.7071067811865475727, 0.000000000000000000, 0.7071067811865475727 ) ) ;
#41338 = CARTESIAN_POINT ( 'NONE',  ( -49.12372073857199695, 14.20664392157176437, 33.19790897520485373 ) ) ;
#41339 = ORIENTED_EDGE ( 'NONE', *, *, #5567, .F. ) ;
#41340 =( REPRESENTATION_RELATIONSHIP ('NONE','NONE', #40274, #34334 ) REPRESENTATION_RELATIONSHIP_WITH_TRANSFORMATION ( #9240 )SHAPE_REPRESENTATION_RELATIONSHIP( ) );
#41341 = ORIENTED_EDGE ( 'NONE', *, *, #51126, .F. ) ;
#41342 = CIRCLE ( 'NONE', #32345, 5.000000000000000888 ) ;
#41343 = PLANE ( 'NONE',  #27512 ) ;
#41344 = CARTESIAN_POINT ( 'NONE',  ( 103.5839822277950049, 25.92130892112108853, 67.41571189329286540 ) ) ;
#41345 = CARTESIAN_POINT ( 'NONE',  ( 113.3994433585436923, 30.36970469616434087, 83.98924600679271180 ) ) ;
#41346 = DIRECTION ( 'NONE',  ( -0.000000000000000000, 1.000000000000000000, -0.000000000000000000 ) ) ;
#41347 = VECTOR ( 'NONE', #51701, 1000.000000000000000 ) ;
#41348 = CARTESIAN_POINT ( 'NONE',  ( 182.7720841008444097, 80.32850885226592652, -51.03576020520832657 ) ) ;
#41349 = FACE_OUTER_BOUND ( 'NONE', #16769, .T. ) ;
#41350 = CARTESIAN_POINT ( 'NONE',  ( -146.1773277338104720, 62.70721456556563567, 85.18395948454488575 ) ) ;
#41351 = ORIENTED_EDGE ( 'NONE', *, *, #33020, .F. ) ;
#41352 = ORIENTED_EDGE ( 'NONE', *, *, #17153, .T. ) ;
#41353 = ORIENTED_EDGE ( 'NONE', *, *, #69410, .F. ) ;
#41354 = AXIS2_PLACEMENT_3D ( 'NONE', #12361, #66200, #23618 ) ;
#41355 = LINE ( 'NONE', #63841, #52130 ) ;
#41356 = CARTESIAN_POINT ( 'NONE',  ( -85.35127931077731489, 24.98147633333000428, 61.35301968501214276 ) ) ;
#41357 = CARTESIAN_POINT ( 'NONE',  ( -4.000000000000000000, 192.0000000000000000, 0.000000000000000000 ) ) ;
#41358 = FACE_OUTER_BOUND ( 'NONE', #52412, .T. ) ;
#41359 = CARTESIAN_POINT ( 'NONE',  ( -58.75378739419586793, 16.75118858561005553, 31.27567419135673177 ) ) ;
#41360 = CARTESIAN_POINT ( 'NONE',  ( -33.85171821065139852, 11.02091558840052521, -62.54379208760393993 ) ) ;
#41361 = CARTESIAN_POINT ( 'NONE',  ( -156.4960819023051215, 70.34114605623871341, -12.69378895035390009 ) ) ;
#41362 = PRODUCT_RELATED_PRODUCT_CATEGORY ( 'part', '', ( #11948 ) ) ;
#41363 = CARTESIAN_POINT ( 'NONE',  ( 181.9411407973026087, 80.91291802046383452, 71.15314469597515767 ) ) ;
#41364 = CARTESIAN_POINT ( 'NONE',  ( 8.683531412707427677, 6.377173148747124820, -13.75927345114389233 ) ) ;
#41365 = ORIENTED_EDGE ( 'NONE', *, *, #12054, .T. ) ;
#41366 = CARTESIAN_POINT ( 'NONE',  ( -4.513903087372270306, 6.697902023160578366, -49.65186798646897870 ) ) ;
#41367 = CARTESIAN_POINT ( 'NONE',  ( 181.9295719569814480, 79.46350097013163349, 56.18870136843697338 ) ) ;
#41368 = CARTESIAN_POINT ( 'NONE',  ( -121.2008155373973466, 43.48033530165982796, 5.404909548456530821 ) ) ;
#41369 = DIRECTION ( 'NONE',  ( 1.387778780781446169E-16, -1.000000000000000000, -3.469446951953615421E-17 ) ) ;
#41370 = CARTESIAN_POINT ( 'NONE',  ( 126.5880720616305553, 37.20544379858408490, -14.81166450811346458 ) ) ;
#41372 = ADVANCED_FACE ( 'NONE', ( #49731 ), #53621, .T. ) ;
#41371 = CARTESIAN_POINT ( 'NONE',  ( 22.72762739171800206, 7.830015800126074232, -13.29790432193229321 ) ) ;
#41373 = CARTESIAN_POINT ( 'NONE',  ( 12.47451846520756646, 7.423604437114562415, 3.937467224307672264 ) ) ;
#41374 = EDGE_CURVE ( 'NONE', #32365, #49097, #34962, .T. ) ;
#41375 = EDGE_LOOP ( 'NONE', ( #40711, #56738, #25010, #25480 ) ) ;
#41376 = CARTESIAN_POINT ( 'NONE',  ( 186.6054783416232397, 84.37128553200979297, 4.863526534070675034 ) ) ;
#41377 = SHAPE_DEFINITION_REPRESENTATION ( #15268, #52783 ) ;
#41378 = CARTESIAN_POINT ( 'NONE',  ( 126.4318266066171930, 38.27072266789464550, -44.61505896352816336 ) ) ;
#41379 = CARTESIAN_POINT ( 'NONE',  ( -128.7650348665116837, 48.41336321950710442, -35.48127487991890661 ) ) ;
#41380 = DIRECTION ( 'NONE',  ( 0.000000000000000000, 1.232595164407830672E-32, 1.000000000000000000 ) ) ;
#41381 = CARTESIAN_POINT ( 'NONE',  ( 187.0788993276711665, 86.37277723143233743, -48.23884571524198606 ) ) ;
#41382 = EDGE_LOOP ( 'NONE', ( #58703, #48312, #64394, #401 ) ) ;
#41383 = EDGE_LOOP ( 'NONE', ( #63028, #48361, #44936, #43376 ) ) ;
#41385 = EDGE_CURVE ( 'NONE', #37671, #53408, #34637, .T. ) ;
#41384 = DIRECTION ( 'NONE',  ( -0.000000000000000000, -0.000000000000000000, -1.000000000000000000 ) ) ;
#41386 = CARTESIAN_POINT ( 'NONE',  ( -48.00000000000000711, -20.00000000000000355, 0.000000000000000000 ) ) ;
#41387 = VERTEX_POINT ( 'NONE', #12465 ) ;
#41388 = VECTOR ( 'NONE', #14886, 1000.000000000000000 ) ;
#41389 = ADVANCED_FACE ( 'NONE', ( #56074 ), #33930, .F. ) ;
#41390 = CARTESIAN_POINT ( 'NONE',  ( 156.3795552199950976, 58.07715209813575541, 83.15336215789184848 ) ) ;
#41391 = EDGE_LOOP ( 'NONE', ( #50909, #16874, #59195, #13882, #25131 ) ) ;
#41392 = CARTESIAN_POINT ( 'NONE',  ( 127.4992165631961285, 38.87141012667721895, -74.37822084336917783 ) ) ;
#41393 = DIRECTION ( 'NONE',  ( 0.000000000000000000, 0.000000000000000000, 1.000000000000000000 ) ) ;
#41394 = VECTOR ( 'NONE', #2113, 1000.000000000000000 ) ;
#41395 = EDGE_CURVE ( 'NONE', #6688, #3562, #7189, .T. ) ;
#41396 = DIRECTION ( 'NONE',  ( 1.000000000000000000, 0.000000000000000000, -0.000000000000000000 ) ) ;
#41397 = FACE_OUTER_BOUND ( 'NONE', #56560, .T. ) ;
#41398 = COLOUR_RGB ( '',0.7921568627450980005, 0.8196078431372548767, 0.9333333333333333481 ) ;
#41399 = DIRECTION ( 'NONE',  ( -0.000000000000000000, -0.000000000000000000, -1.000000000000000000 ) ) ;
#41401 = ORIENTED_EDGE ( 'NONE', *, *, #58585, .T. ) ;
#41400 = CARTESIAN_POINT ( 'NONE',  ( 0.000000000000000000, 0.000000000000000000, 0.000000000000000000 ) ) ;
#41402 = CARTESIAN_POINT ( 'NONE',  ( 429.8372781065087338, 395.0000000000001137, -128.9497041420121093 ) ) ;
#41403 = VERTEX_POINT ( 'NONE', #44474 ) ;
#41404 = VERTEX_POINT ( 'NONE', #8588 ) ;
#41405 = FACE_OUTER_BOUND ( 'NONE', #24024, .T. ) ;
#41406 = CARTESIAN_POINT ( 'NONE',  ( -178.0658882571760557, 92.80593104957422668, -21.01134249067511917 ) ) ;
#41408 = VERTEX_POINT ( 'NONE', #29009 ) ;
#41407 = DIRECTION ( 'NONE',  ( -0.000000000000000000, 1.000000000000000000, -0.000000000000000000 ) ) ;
#41409 = CARTESIAN_POINT ( 'NONE',  ( 0.000000000000000000, 0.000000000000000000, -50.00000000000000000 ) ) ;
#41410 = MANIFOLD_SOLID_BREP ( 'Mirror1', #27184 ) ;
#41411 = PLANE ( 'NONE',  #20500 ) ;
#41412 = ORIENTED_EDGE ( 'NONE', *, *, #68531, .T. ) ;
#41413 = CARTESIAN_POINT ( 'NONE',  ( -61.52143283897134296, 16.51181063611435462, -19.67550361010446380 ) ) ;
#41414 = ADVANCED_FACE ( 'NONE', ( #8235 ), #13171, .F. ) ;
#41415 = CARTESIAN_POINT ( 'NONE',  ( -133.3923804760465543, 52.87100816290223548, -69.82553800854516624 ) ) ;
#41416 = CARTESIAN_POINT ( 'NONE',  ( 116.9197133427646804, 33.22079464767577406, 33.65725764894440886 ) ) ;
#41417 = CARTESIAN_POINT ( 'NONE',  ( 5.799999999999999822, 6.928203230275504332, -4.000000000000007994 ) ) ;
#41418 = CARTESIAN_POINT ( 'NONE',  ( 70.45451534980406905, 15.56315969138428201, -71.05294828632224835 ) ) ;
#41419 = ORIENTED_EDGE ( 'NONE', *, *, #39691, .F. ) ;
#41420 = EDGE_LOOP ( 'NONE', ( #46697, #12378, #8077, #51788 ) ) ;
#41421 = CARTESIAN_POINT ( 'NONE',  ( -149.0764453401866945, 65.13297611514533969, -22.96827994102829251 ) ) ;
#41422 = LINE ( 'NONE', #47365, #39101 ) ;
#41423 = CARTESIAN_POINT ( 'NONE',  ( 0.000000000000000000, 0.000000000000000000, 5.000000000000000000 ) ) ;
#41424 = DIRECTION ( 'NONE',  ( -0.000000000000000000, 1.000000000000000000, -0.000000000000000000 ) ) ;
#41425 = CARTESIAN_POINT ( 'NONE',  ( -54.20542732064039626, 15.49651042269896806, -88.94138983813944321 ) ) ;
#41426 = DIRECTION ( 'NONE',  ( 0.000000000000000000, 0.000000000000000000, -1.000000000000000000 ) ) ;
#41427 = CARTESIAN_POINT ( 'NONE',  ( -143.8566410313463564, 59.53044870492033169, 43.17841504270860753 ) ) ;
#41428 = DIRECTION ( 'NONE',  ( -0.000000000000000000, -0.000000000000000000, -1.000000000000000000 ) ) ;
#41429 = CARTESIAN_POINT ( 'NONE',  ( -165.6398193834832284, 79.16932278174806470, -69.66723566926393119 ) ) ;
#41430 = VERTEX_POINT ( 'NONE', #51146 ) ;
#41431 = CARTESIAN_POINT ( 'NONE',  ( -108.1180879163843116, 36.99199941971028238, 42.75380726691431477 ) ) ;
#41432 = EDGE_LOOP ( 'NONE', ( #5218, #36686, #37073, #8853 ) ) ;
#41433 = CARTESIAN_POINT ( 'NONE',  ( 209.3223706822284100, 190.0000000000000000, 31.44247402469554942 ) ) ;
#41434 = CARTESIAN_POINT ( 'NONE',  ( 79.39764314491567632, 18.13166883367086868, 62.05256806867162567 ) ) ;
#41435 = LINE ( 'NONE', #30194, #26234 ) ;
#41436 = CARTESIAN_POINT ( 'NONE',  ( 55.65793654284683356, -50.28674377798225237, 170.0000000000000000 ) ) ;
#41437 = PLANE ( 'NONE',  #42239 ) ;
#41438 = CIRCLE ( 'NONE', #27918, 65.36598343705435354 ) ;
#41439 = CARTESIAN_POINT ( 'NONE',  ( 218.0000000000000000, 126.6235316737731296, -95.00000000000133582 ) ) ;
#41440 = CARTESIAN_POINT ( 'NONE',  ( 31.90184941268615759, 7.552181687745348704, 10.32724003673442148 ) ) ;
#41441 = CARTESIAN_POINT ( 'NONE',  ( 112.3013380801407237, 395.0000000000010800, 96.05029585798746439 ) ) ;
#41442 = CARTESIAN_POINT ( 'NONE',  ( -38.88884187334145537, 11.95889603743730056, -16.96948798090240373 ) ) ;
#41443 = EDGE_CURVE ( 'NONE', #67530, #53526, #50019, .T. ) ;
#41444 = VECTOR ( 'NONE', #58733, 1000.000000000000000 ) ;
#41445 = ORIENTED_EDGE ( 'NONE', *, *, #68368, .F. ) ;
#41446 = B_SPLINE_CURVE_WITH_KNOTS ( 'NONE', 3,
 ( #49434, #21669, #48726, #1265, #11451, #48375, #6547, #65283, #17435, #65642, #28342, #53673, #32579, #33289, #55067, #17078, #39259, #49082, #32239, #60703, #38911, #17802, #6185, #60355, #32921, #12176, #11812, #59990, #59637, #209, #43810, #33638, #16737, #64590, #38196, #570, #6885, #16398, #22022, #49786, #921, #37853, #1612, #23077, #66004, #5495 ),
 .UNSPECIFIED., .F., .F.,
 ( 4, 2, 2, 2, 2, 2, 2, 2, 2, 2, 2, 2, 2, 2, 2, 2, 2, 2, 2, 2, 2, 2, 4 ),
 ( 0.02404638330965504917, 0.02555608299537562300, 0.02631093283823590992, 0.02706578268109620031, 0.02857548236681679496, 0.02933033220967708882, 0.03008518205253738614, 0.03159488173825795304, 0.03310458142397851300, 0.03385943126683879645, 0.03461428110969907990, 0.03612398079541960516, 0.03687883063827988861, 0.03763368048114017206, 0.03838853032400045551, 0.03914338016686073896, 0.04065307985258127810, 0.04216277953830183112, 0.04367247922402237026, 0.04518217890974292328, 0.04593702875260319285, 0.04669187859546346242, 0.04820157828118400850 ),
 .UNSPECIFIED. ) ;
#41447 = DIRECTION ( 'NONE',  ( 0.000000000000000000, 0.000000000000000000, -1.000000000000000000 ) ) ;
#41448 = VERTEX_POINT ( 'NONE', #67336 ) ;
#41449 = CARTESIAN_POINT ( 'NONE',  ( -60.66241560458684035, 16.25736033771450550, 32.81469839604517347 ) ) ;
#41450 = DIRECTION ( 'NONE',  ( 0.000000000000000000, 0.000000000000000000, 1.000000000000000000 ) ) ;
#41451 = CARTESIAN_POINT ( 'NONE',  ( -189.4223925288096098, 107.3427006758676612, 13.29886559940774049 ) ) ;
#41452 = PLANE ( 'NONE',  #67070 ) ;
#41454 = EDGE_CURVE ( 'NONE', #11967, #40747, #12825, .T. ) ;
#41453 = CARTESIAN_POINT ( 'NONE',  ( -14.92903005859420951, 7.458185427130747946, -67.34419620779377169 ) ) ;
#41455 = CARTESIAN_POINT ( 'NONE',  ( -96.76159256735195413, 30.06445763698410190, -10.56742495184200159 ) ) ;
#41456 =( NAMED_UNIT ( * ) PLANE_ANGLE_UNIT ( ) SI_UNIT ( $, .RADIAN. ) );
#41457 = EDGE_CURVE ( 'NONE', #43408, #7667, #20503, .T. ) ;
#41458 = B_SPLINE_CURVE_WITH_KNOTS ( 'NONE', 3,
 ( #36204, #58673, #15092, #9821, #5220, #31279, #64308, #10838, #16115, #36550, #59022, #47426, #32309, #53737, #27015, #43185, #68880, #21733, #63629, #15443, #33705, #44228, #39322, #23497, #22438, #66074, #11521, #38618, #65009, #5896, #28407, #28058, #60765, #2045, #12590, #49855, #37923, #639, #54788, #16468, #64660, #990, #16802, #28771 ),
 .UNSPECIFIED., .F., .F.,
 ( 4, 2, 2, 2, 2, 2, 2, 2, 2, 2, 2, 2, 2, 2, 2, 2, 2, 2, 2, 2, 2, 4 ),
 ( 0.02432640572110343624, 0.02583721026359370523, 0.02659261253483881718, 0.02734801480608393259, 0.02885881934857419465, 0.02961422161981931006, 0.03036962389106442894, 0.03188042843355462508, 0.03339123297604482121, 0.03414663524728990540, 0.03490203751853499653, 0.03641284206102517185, 0.03716824433227024910, 0.03792364660351533329, 0.03943445114600548779, 0.04094525568849564923, 0.04245606023098580373, 0.04396686477347595823, 0.04472226704472104242, 0.04547766931596611967, 0.04698847385845632274, 0.04849927840094651887 ),
 .UNSPECIFIED. ) ;
#41459 = EDGE_LOOP ( 'NONE', ( #4612, #56200, #55871, #21163, #47325, #55785, #36369, #55057, #54023 ) ) ;
#41460 = ADVANCED_FACE ( 'NONE', ( #36347 ), #24762, .T. ) ;
#41461 = DIRECTION ( 'NONE',  ( 9.989315170677463157E-15, -1.000000000000000000, -4.052314039881817428E-15 ) ) ;
#41462 = CARTESIAN_POINT ( 'NONE',  ( 3.306546357697853733E-15, 35.00000000000000000, 27.00000000000000000 ) ) ;
#41463 = CARTESIAN_POINT ( 'NONE',  ( 174.6307688320643194, 73.70327352127000609, -20.71130733032186200 ) ) ;
#41464 = CARTESIAN_POINT ( 'NONE',  ( -188.6739852773920632, 108.2139733222100375, 63.56149477935467473 ) ) ;
#41465 = PLANE ( 'NONE',  #9717 ) ;
#41466 = EDGE_LOOP ( 'NONE', ( #22509, #65412, #47155, #60647 ) ) ;
#41467 = CARTESIAN_POINT ( 'NONE',  ( -173.5422248620772621, 89.11126078969415687, -61.55650775521368701 ) ) ;
#41468 = CARTESIAN_POINT ( 'NONE',  ( -0.7215816834507519095, 6.532459459468095808, -18.49149345562722146 ) ) ;
#41469 = CARTESIAN_POINT ( 'NONE',  ( -7.329206686002009974E-14, -46.66904755831211560, 0.000000000000000000 ) ) ;
#41470 = LINE ( 'NONE', #30566, #52879 ) ;
#41471 = EDGE_CURVE ( 'NONE', #32990, #8876, #20852, .T. ) ;
#41472 = CARTESIAN_POINT ( 'NONE',  ( -120.1259246007803654, 42.81147313035992141, -64.43732786190635409 ) ) ;
#41473 = EDGE_LOOP ( 'NONE', ( #37938, #15208, #44991, #66325 ) ) ;
#41474 = CARTESIAN_POINT ( 'NONE',  ( 197.3059626281005592, 96.72682679064186573, 38.01856143111450592 ) ) ;
#41475 = DIRECTION ( 'NONE',  ( 0.000000000000000000, 0.000000000000000000, -1.000000000000000000 ) ) ;
#41476 = EDGE_CURVE ( 'NONE', #22455, #50199, #49123, .T. ) ;
#41477 = CARTESIAN_POINT ( 'NONE',  ( 185.1710994180822354, 84.30654632312743502, 43.11307207121964780 ) ) ;
#41478 = CARTESIAN_POINT ( 'NONE',  ( 141.3556389957210229, 47.34429831367555863, 10.46169434721303482 ) ) ;
#41479 = CYLINDRICAL_SURFACE ( 'NONE', #55501, 4.999999999999997335 ) ;
#41480 = VERTEX_POINT ( 'NONE', #19828 ) ;
#41481 = CARTESIAN_POINT ( 'NONE',  ( 173.5836858989432301, 72.71885240881780987, 63.93992091031944369 ) ) ;
#41482 = ORIENTED_EDGE ( 'NONE', *, *, #38183, .F. ) ;
#41483 = CARTESIAN_POINT ( 'NONE',  ( 67.93154431625913503, 14.90489441944787430, 58.47168318147574695 ) ) ;
#41484 = CARTESIAN_POINT ( 'NONE',  ( 141.2060940825452064, 46.04283574924851052, 89.19312868080487533 ) ) ;
#41485 = AXIS2_PLACEMENT_3D ( 'NONE', #40263, #67699, #29031 ) ;
#41487 = ORIENTED_EDGE ( 'NONE', *, *, #25901, .T. ) ;
#41486 = CARTESIAN_POINT ( 'NONE',  ( 154.0515132159916902, 56.29926936869306076, 3.373288628613766882 ) ) ;
#41488 = CARTESIAN_POINT ( 'NONE',  ( -178.2427210808090479, 93.01567669683340966, 32.83739906211183524 ) ) ;
#41489 = DIRECTION ( 'NONE',  ( 0.000000000000000000, 0.000000000000000000, -1.000000000000000000 ) ) ;
#41490 = VECTOR ( 'NONE', #20515, 1000.000000000000114 ) ;
#41491 = CARTESIAN_POINT ( 'NONE',  ( 116.6681538161788438, 33.09439081574000596, -47.32309755658299366 ) ) ;
#41492 = ORIENTED_EDGE ( 'NONE', *, *, #58079, .F. ) ;
#41493 = FACE_OUTER_BOUND ( 'NONE', #37161, .T. ) ;
#41494 = CARTESIAN_POINT ( 'NONE',  ( 38.90907126433567242, 9.359889524363186553, 44.91383430596329163 ) ) ;
#41495 = VERTEX_POINT ( 'NONE', #36004 ) ;
#41496 = CARTESIAN_POINT ( 'NONE',  ( 136.1081004736419402, 42.80058051492066085, 56.69709667588018931 ) ) ;
#41497 = CARTESIAN_POINT ( 'NONE',  ( -165.7699288023689803, 79.30174988963855753, 36.80611496506521263 ) ) ;
#41498 = FACE_OUTER_BOUND ( 'NONE', #43174, .T. ) ;
#41499 = CARTESIAN_POINT ( 'NONE',  ( 133.6288034103009750, 41.28708886999546479, -77.86786152285937135 ) ) ;
#41500 = VERTEX_POINT ( 'NONE', #46900 ) ;
#41501 = DIRECTION ( 'NONE',  ( -0.000000000000000000, 1.000000000000000000, -0.000000000000000000 ) ) ;
#41502 = EDGE_LOOP ( 'NONE', ( #51708, #32009, #48824, #18857 ) ) ;
#41503 = CIRCLE ( 'NONE', #57224, 298.0000000000000000 ) ;
#41504 = CARTESIAN_POINT ( 'NONE',  ( 154.0281735872261493, 56.28213428456459866, -10.11222482322573413 ) ) ;
#41505 = CARTESIAN_POINT ( 'NONE',  ( -50.37626225203914032, 13.47725392609373429, 85.63415519923331942 ) ) ;
#41506 = CARTESIAN_POINT ( 'NONE',  ( 106.6181401479172308, 28.34160787025143691, 43.68143237657537981 ) ) ;
#41507 = CARTESIAN_POINT ( 'NONE',  ( -150.3898662070192529, 64.92828409760431896, -61.65738112195564469 ) ) ;
#41508 = CARTESIAN_POINT ( 'NONE',  ( 58.16156486118065772, 11.59853826451868564, 85.24551411657452604 ) ) ;
#41509 = CARTESIAN_POINT ( 'NONE',  ( 181.0840389613909736, 80.03940679743416808, 2.464043515047717570 ) ) ;
#41510 = CARTESIAN_POINT ( 'NONE',  ( 209.9944361927104239, 113.8994774711241291, -49.14096817356703895 ) ) ;
#41511 = CARTESIAN_POINT ( 'NONE',  ( 174.1364721914477229, 71.85829564941442982, 7.124632976745406410 ) ) ;
#41513 = ORIENTED_EDGE ( 'NONE', *, *, #35015, .T. ) ;
#41512 =( BOUNDED_CURVE ( )  B_SPLINE_CURVE ( 3, ( #50444, #2263, #23711, #18431 ),
 .UNSPECIFIED., .F., .F. ) 
 B_SPLINE_CURVE_WITH_KNOTS ( ( 4, 4 ),
 ( 2.506209174768084580, 3.776976132411494103 ),
 .UNSPECIFIED. ) 
 CURVE ( )  GEOMETRIC_REPRESENTATION_ITEM ( )  RATIONAL_B_SPLINE_CURVE ( ( 1.000000000000000000, 0.8698961108463049152, 0.8698961108463049152, 1.000000000000000000 ) ) 
 REPRESENTATION_ITEM ( '' )  );
#41514 = DIRECTION ( 'NONE',  ( -0.6234898018587431423, 0.7818314824680220321, 0.000000000000000000 ) ) ;
#41515 = EDGE_LOOP ( 'NONE', ( #61591, #43401, #11844, #9046, #35124 ) ) ;
#41516 =( NAMED_UNIT ( * ) SI_UNIT ( $, .STERADIAN. ) SOLID_ANGLE_UNIT ( ) );
#41517 = CARTESIAN_POINT ( 'NONE',  ( 55.57657751403269231, 11.06944050856661832, -71.05142857302701032 ) ) ;
#41518 = CARTESIAN_POINT ( 'NONE',  ( -74.40004226286974642, 20.74218500375952701, 4.900570124997223331 ) ) ;
#41519 = CARTESIAN_POINT ( 'NONE',  ( 99.71998884745383407, 188.0000000000000000, 7.478223336038896996 ) ) ;
#41520 = CARTESIAN_POINT ( 'NONE',  ( -0.3230440667461953463, 6.518512734653291396, 91.57163373586021748 ) ) ;
#41521 = AXIS2_PLACEMENT_3D ( 'NONE', #11542, #28082, #26709 ) ;
#41522 = CARTESIAN_POINT ( 'NONE',  ( -109.3386876948163433, 37.66246927061206407, -18.25541805540258622 ) ) ;
#41523 = VERTEX_POINT ( 'NONE', #20165 ) ;
#41524 = B_SPLINE_CURVE_WITH_KNOTS ( 'NONE', 3,
 ( #55947, #66862, #65455, #17963, #23591, #22886, #18304, #34506, #39412, #49957, #7762, #38361, #6356, #60860, #66512, #44329, #39076, #27811, #39762, #45383, #17249, #55231, #49598, #29211, #59806, #12683, #34150, #54530, #49249, #28870, #45029, #50658, #61219, #2478, #23933, #65816, #11620, #33094, #17610, #22535, #1082, #43973, #38719, #60518, #55585, #33792 ),
 .UNSPECIFIED., .F., .F.,
 ( 4, 2, 2, 2, 2, 2, 2, 2, 2, 2, 2, 2, 2, 2, 2, 2, 2, 2, 2, 2, 2, 2, 4 ),
 ( 0.000000000000000000, 0.001615199098318994761, 0.003230398196637989522, 0.004037997745797492107, 0.004845597294956995559, 0.006460796393276001595, 0.007268395942435538007, 0.008075995491595072684, 0.009691194589914093466, 0.01049879413907361947, 0.01130639368823314374, 0.01211399323739267148, 0.01292159278655219921, 0.01453679188487125643, 0.01615199098319031190, 0.01695959053234982056, 0.01776719008150933268, 0.01938238917982830489, 0.02099758827814728057, 0.02180518782730674412, 0.02261278737646620421, 0.02422798647478506540, 0.02584318557310392658 ),
 .UNSPECIFIED. ) ;
#41525 = LINE ( 'NONE', #30977, #65658 ) ;
#41526 = CARTESIAN_POINT ( 'NONE',  ( 203.3978200800095237, 104.5785882372513242, -90.12130148826626908 ) ) ;
#41527 = VERTEX_POINT ( 'NONE', #63076 ) ;
#41528 = ORIENTED_EDGE ( 'NONE', *, *, #29092, .F. ) ;
#41530 = EDGE_CURVE ( 'NONE', #38858, #62756, #27158, .T. ) ;
#41529 = CARTESIAN_POINT ( 'NONE',  ( -156.9910258076866114, 70.79617246506499839, 37.64717199668289282 ) ) ;
#41531 = CARTESIAN_POINT ( 'NONE',  ( 59.08638499266955790, 11.79550614876701431, -49.61367700836938610 ) ) ;
#41532 = DIRECTION ( 'NONE',  ( -1.000000000000000000, -0.000000000000000000, -0.000000000000000000 ) ) ;
#41533 = LINE ( 'NONE', #40154, #68944 ) ;
#41534 = VECTOR ( 'NONE', #35614, 1000.000000000000000 ) ;
#41535 = EDGE_CURVE ( 'NONE', #16864, #6290, #38065, .T. ) ;
#41536 = EDGE_LOOP ( 'NONE', ( #24296, #23041 ) ) ;
#41537 = LINE ( 'NONE', #57715, #13179 ) ;
#41538 = VERTEX_POINT ( 'NONE', #53539 ) ;
#41539 = CARTESIAN_POINT ( 'NONE',  ( 211.3917124729449881, 115.9987099435922886, 13.25711159579326548 ) ) ;
#41540 = CARTESIAN_POINT ( 'NONE',  ( 13.36262230781616012, 7.441298897118794997, 71.47295967330329347 ) ) ;
#41541 = SURFACE_SIDE_STYLE ('',( #47151 ) ) ;
#41542 = CARTESIAN_POINT ( 'NONE',  ( 14.12575540446280264, 6.452943588436218292, -89.38275910569522864 ) ) ;
#41543 = ADVANCED_FACE ( 'NONE', ( #33504 ), #44025, .T. ) ;
#41544 = EDGE_LOOP ( 'NONE', ( #18995, #36483 ) ) ;
#41545 = ORIENTED_EDGE ( 'NONE', *, *, #12069, .T. ) ;
#41546 = CARTESIAN_POINT ( 'NONE',  ( 110.6598192889778574, -21.43204465433285932, 4.967071677942377583 ) ) ;
#41547 = CARTESIAN_POINT ( 'NONE',  ( -130.2612055759786074, 50.66074200725057608, 85.70470224599091580 ) ) ;
#41548 = B_SPLINE_CURVE_WITH_KNOTS ( 'NONE', 3,
 ( #12411, #33868, #50396, #60941, #55310, #59882, #7129, #44770, #28590, #12760, #50043, #66246, #18038, #2211, #23662, #46837, #7833, #24710, #56021, #40523, #18378, #2903, #14144, #61972, #8873, #13792, #29622, #24008, #24363, #9211, #13116, #2554, #50731, #3583, #35943, #45808, #34583, #51088, #46144, #45454, #29282, #67287, #67614, #14488 ),
 .UNSPECIFIED., .F., .F.,
 ( 4, 2, 2, 2, 2, 2, 2, 2, 2, 2, 2, 2, 2, 2, 2, 2, 2, 2, 2, 2, 2, 4 ),
 ( 0.000000000000000000, 0.001472974678681641860, 0.002209462018022466910, 0.002945949357363291526, 0.004418924036044906932, 0.005891898714726521470, 0.007364873393408136008, 0.008101360732748960625, 0.008837848072089786108, 0.01031082275077139544, 0.01178379742945300651, 0.01252028476879383373, 0.01325677210813466095, 0.01472974678681628936, 0.01546623412615710617, 0.01620272146549792125, 0.01767569614417955487, 0.01914867082286118502, 0.01988515816220200877, 0.02062164550154282558, 0.02209462018022446961, 0.02356759485890611364 ),
 .UNSPECIFIED. ) ;
#41549 = CARTESIAN_POINT ( 'NONE',  ( -168.7150276173048269, 82.35404041280330034, -9.279753688084731778 ) ) ;
#41550 = DIRECTION ( 'NONE',  ( 1.000000000000000000, 0.000000000000000000, 0.000000000000000000 ) ) ;
#41551 = CARTESIAN_POINT ( 'NONE',  ( 18.97610100625297491, 6.623071417957627993, 84.38338133953382680 ) ) ;
#41552 = AXIS2_PLACEMENT_3D ( 'NONE', #28883, #33806, #1446 ) ;
#41553 = CARTESIAN_POINT ( 'NONE',  ( 79.82127737190242556, 17.20935440217363066, -73.32255258993723146 ) ) ;
#41554 = ORIENTED_EDGE ( 'NONE', *, *, #26351, .T. ) ;
#41555 = DIRECTION ( 'NONE',  ( -0.2225209339563184452, 0.9749279121818226201, 0.000000000000000000 ) ) ;
#41556 = CARTESIAN_POINT ( 'NONE',  ( -94.77925136849377452, 29.13093715379787696, 65.09547375720568141 ) ) ;
#41557 = ORIENTED_EDGE ( 'NONE', *, *, #30790, .F. ) ;
#41558 = CARTESIAN_POINT ( 'NONE',  ( -85.09761763353358788, 24.87634954265997322, 14.94058973873350382 ) ) ;
#41559 = VERTEX_POINT ( 'NONE', #32449 ) ;
#41560 = CARTESIAN_POINT ( 'NONE',  ( -57.43883374585514900, 16.37892664338859916, -8.757341026728871825 ) ) ;
#41561 = ORIENTED_EDGE ( 'NONE', *, *, #9399, .T. ) ;
#41562 = ORIENTED_EDGE ( 'NONE', *, *, #36471, .T. ) ;
#41563 = CARTESIAN_POINT ( 'NONE',  ( -121.2119672714299412, 44.67540322905998806, 17.15459649910451745 ) ) ;
#41564 = AXIS2_PLACEMENT_3D ( 'NONE', #5081, #58205, #26547 ) ;
#41565 = CARTESIAN_POINT ( 'NONE',  ( 188.9999999999999432, -57.00000000000007816, 72.99999999999998579 ) ) ;
#41566 = DIRECTION ( 'NONE',  ( 0.000000000000000000, 0.000000000000000000, 1.000000000000000000 ) ) ;
#41567 = ORIENTED_EDGE ( 'NONE', *, *, #24952, .F. ) ;
#41568 = CARTESIAN_POINT ( 'NONE',  ( -24.56126296900623274, 8.563129532889934836, 94.41426630670055431 ) ) ;
#41569 = CARTESIAN_POINT ( 'NONE',  ( 179.4227152810057930, 78.36166152262363482, -77.89550332129535093 ) ) ;
#41570 = CARTESIAN_POINT ( 'NONE',  ( -126.3495878770406762, 48.00153794568859666, -8.069153307770246641 ) ) ;
#41571 = CARTESIAN_POINT ( 'NONE',  ( 102.8458551240039611, 25.60773946375957166, -44.68694561986643521 ) ) ;
#41572 = CARTESIAN_POINT ( 'NONE',  ( 84.27937148876358719, 19.69225537006224513, -50.44796742885471730 ) ) ;
#41573 = CARTESIAN_POINT ( 'NONE',  ( 111.9975424824652634, 296.0000000000000000, 420.0000000000000568 ) ) ;
#41574 = ORIENTED_EDGE ( 'NONE', *, *, #50505, .F. ) ;
#41575 = VECTOR ( 'NONE', #30154, 1000.000000000000000 ) ;
#41576 = DIRECTION ( 'NONE',  ( 0.6910626489868580968, 0.7227948638273978821, 0.000000000000000000 ) ) ;
#41577 = CARTESIAN_POINT ( 'NONE',  ( -85.73740570227380431, 26.23277384689415115, -71.97308702196428953 ) ) ;
#41578 = CARTESIAN_POINT ( 'NONE',  ( 174.2538192999570015, 73.34752463892027663, 6.853970190747312508 ) ) ;
#41579 = PLANE ( 'NONE',  #17700 ) ;
#41580 = EDGE_CURVE ( 'NONE', #20568, #6663, #59222, .T. ) ;
#41581 = DIRECTION ( 'NONE',  ( 0.000000000000000000, -1.000000000000000000, 0.000000000000000000 ) ) ;
#41582 = CARTESIAN_POINT ( 'NONE',  ( 131.6189313563687620, 40.08924984825279125, 17.33914888436516222 ) ) ;
#41583 = CARTESIAN_POINT ( 'NONE',  ( -156.4960819023051499, 70.34114605623869920, 14.15076164010977600 ) ) ;
#41584 = CARTESIAN_POINT ( 'NONE',  ( 0.000000000000000000, 0.000000000000000000, 41.38025477438755928 ) ) ;
#41585 = CARTESIAN_POINT ( 'NONE',  ( 55.46196446482079523, 34.59309596431375411, 41.38025477438755928 ) ) ;
#41586 = CARTESIAN_POINT ( 'NONE',  ( -81.00768240531211006, 24.30850321514432366, 57.63353788888659324 ) ) ;
#41587 = DIRECTION ( 'NONE',  ( 0.000000000000000000, 1.000000000000000000, 0.000000000000000000 ) ) ;
#41589 = ORIENTED_EDGE ( 'NONE', *, *, #30254, .T. ) ;
#41588 = ADVANCED_FACE ( 'NONE', ( #47918 ), #17302, .F. ) ;
#41590 = CARTESIAN_POINT ( 'NONE',  ( -47.61678346849998178, 13.84663486211544026, 92.53719257853346392 ) ) ;
#41591 = EDGE_LOOP ( 'NONE', ( #41351, #52244 ) ) ;
#41592 = DIRECTION ( 'NONE',  ( 1.000000000000000000, 0.000000000000000000, 0.000000000000000000 ) ) ;
#41593 = VERTEX_POINT ( 'NONE', #82 ) ;
#41594 = CARTESIAN_POINT ( 'NONE',  ( 23.09590709048885060, 7.852755081912508928, -68.15776028566385492 ) ) ;
#41595 = DIRECTION ( 'NONE',  ( -0.000000000000000000, 1.000000000000000000, -0.000000000000000000 ) ) ;
#41596 = DIRECTION ( 'NONE',  ( -0.000000000000000000, -0.000000000000000000, -1.000000000000000000 ) ) ;
#41597 = DIRECTION ( 'NONE',  ( 1.000000000000000000, -0.000000000000000000, -0.000000000000000000 ) ) ;
#41598 = AXIS2_PLACEMENT_3D ( 'NONE', #24489, #50853, #13234 ) ;
#41599 = CARTESIAN_POINT ( 'NONE',  ( 134.7720294983483313, 43.15885542353190374, -36.06555109292058603 ) ) ;
#41600 = CARTESIAN_POINT ( 'NONE',  ( 31.99894129856762603, 7.561773404408281607, -44.34697420425325021 ) ) ;
#41601 = CARTESIAN_POINT ( 'NONE',  ( 11.81843724556920883, 7.412394300769733491, -36.65097937619014346 ) ) ;
#41602 = DIRECTION ( 'NONE',  ( 0.000000000000000000, -1.000000000000000000, 0.000000000000000000 ) ) ;
#41603 = CARTESIAN_POINT ( 'NONE',  ( -120.0051930351106648, 43.92079660368833771, -10.91750049354815388 ) ) ;
#41604 = ORIENTED_EDGE ( 'NONE', *, *, #57580, .F. ) ;
#41605 = EDGE_CURVE ( 'NONE', #36801, #55179, #29592, .T. ) ;
#41607 = EDGE_LOOP ( 'NONE', ( #30969, #62151 ) ) ;
#41606 = ADVANCED_BREP_SHAPE_REPRESENTATION ( '', ( #41410, #66832 ), #6181 ) ;
#41608 = EDGE_CURVE ( 'NONE', #46033, #9808, #26222, .T. ) ;
#41609 = CARTESIAN_POINT ( 'NONE',  ( 63.72039997003709288, 12.83396383267841223, 40.00000000000003553 ) ) ;
#41610 = CARTESIAN_POINT ( 'NONE',  ( -47.07758031033817048, 21.28397246211312321, 26.66469066592268788 ) ) ;
#41611 = CARTESIAN_POINT ( 'NONE',  ( -26.88245755577922935, 8.887394979218514734, -75.63929455523587819 ) ) ;
#41612 = UNCERTAINTY_MEASURE_WITH_UNIT (LENGTH_MEASURE( 1.000000000000000082E-05 ), #41278, 'distance_accuracy_value', 'NONE');
#41613 = EDGE_CURVE ( 'NONE', #55532, #67200, #34199, .T. ) ;
#41614 = AXIS2_PLACEMENT_3D ( 'NONE', #35823, #57277, #44183 ) ;
#41615 = CARTESIAN_POINT ( 'NONE',  ( 9.416603677636263825, 6.380307115728825806, 6.706382208024352920 ) ) ;
#41616 = DIRECTION ( 'NONE',  ( 0.000000000000000000, 1.000000000000000000, -0.000000000000000000 ) ) ;
#41617 = DIRECTION ( 'NONE',  ( -0.000000000000000000, -0.000000000000000000, -1.000000000000000000 ) ) ;
#41618 = CARTESIAN_POINT ( 'NONE',  ( 206.3053863259449372, 110.3084416756849464, 17.23374409832117138 ) ) ;
#41619 =( NAMED_UNIT ( * ) PLANE_ANGLE_UNIT ( ) SI_UNIT ( $, .RADIAN. ) );
#41620 = CARTESIAN_POINT ( 'NONE',  ( 0.000000000000000000, 0.000000000000000000, 170.0000000000000000 ) ) ;
#41621 = CARTESIAN_POINT ( 'NONE',  ( 92.51858280840788495, 21.51505926344913533, -21.14771471057316177 ) ) ;
#41622 = LINE ( 'NONE', #20504, #65708 ) ;
#41623 = CARTESIAN_POINT ( 'NONE',  ( -31.11269837220806878, 5.594483210025202879E-14, 85.00100000000000477 ) ) ;
#41624 = CARTESIAN_POINT ( 'NONE',  ( 0.000000000000000000, 0.000000000000000000, 40.00000000000003553 ) ) ;
#41625 = ADVANCED_FACE ( 'NONE', ( #18010 ), #44380, .F. ) ;
#41626 = VERTEX_POINT ( 'NONE', #2525 ) ;
#41627 = CARTESIAN_POINT ( 'NONE',  ( -12.71191156098292652, -50.07707454696033977, 26.66469104408690782 ) ) ;
#41628 = CARTESIAN_POINT ( 'NONE',  ( 111.9975424824652634, 172.0000000000000284, 420.0000000000000568 ) ) ;
#41629 = DIRECTION ( 'NONE',  ( 0.5409654940743039431, -0.000000000000000000, 0.8410447872859948548 ) ) ;
#41630 = DIRECTION ( 'NONE',  ( -0.000000000000000000, 1.000000000000000000, -0.000000000000000000 ) ) ;
#41631 = CARTESIAN_POINT ( 'NONE',  ( -47.56463531432803649, 12.80077789972090230, -42.22615997514142805 ) ) ;
#41632 = EDGE_CURVE ( 'NONE', #50425, #56268, #31842, .T. ) ;
#41633 = FACE_OUTER_BOUND ( 'NONE', #40084, .T. ) ;
#41634 = EDGE_CURVE ( 'NONE', #43258, #44455, #30747, .T. ) ;
#41635 = CARTESIAN_POINT ( 'NONE',  ( -0.4850857408069293442, 7.530899315854036935, 92.87821500056037394 ) ) ;
#41636 = ADVANCED_FACE ( 'NONE', ( #23299 ), #50371, .F. ) ;
#41637 = ORIENTED_EDGE ( 'NONE', *, *, #58353, .T. ) ;
#41638 = DIRECTION ( 'NONE',  ( 3.356887510711447811E-18, -3.842266915190389043E-18, -1.000000000000000000 ) ) ;
#41639 = CARTESIAN_POINT ( 'NONE',  ( -61.51762070241279190, 16.51067482779403761, 68.47209165092128558 ) ) ;
#41640 = VERTEX_POINT ( 'NONE', #51061 ) ;
#41641 = ORIENTED_EDGE ( 'NONE', *, *, #55766, .F. ) ;
#41642 = CARTESIAN_POINT ( 'NONE',  ( 46.89562634055204882, 10.52219511967644650, 91.55471069079136726 ) ) ;
#41643 = CARTESIAN_POINT ( 'NONE',  ( -179.0654441437004039, 93.99779465816536117, -73.63664225586808243 ) ) ;
#41644 = CARTESIAN_POINT ( 'NONE',  ( 134.6156496652957628, 43.06323651754149040, -89.74142866289044207 ) ) ;
#41645 = ORIENTED_EDGE ( 'NONE', *, *, #4786, .F. ) ;
#41646 = CARTESIAN_POINT ( 'NONE',  ( -47.68562151781910785, 13.86286849776707797, -95.00000000000133582 ) ) ;
#41647 = CARTESIAN_POINT ( 'NONE',  ( -27.00000000000000355, 26.99999999999999645, 15.00000000000000000 ) ) ;
#41648 = VECTOR ( 'NONE', #5862, 1000.000000000000000 ) ;
#41649 = CARTESIAN_POINT ( 'NONE',  ( 55.91133443650746671, 12.16263767238153726, -45.67481826356996777 ) ) ;
#41650 = CARTESIAN_POINT ( 'NONE',  ( -82.32006615997345023, 24.83050031643764655, 31.35040515247533577 ) ) ;
#41651 = CARTESIAN_POINT ( 'NONE',  ( -0.6543471694412734685, -8.859816792613656844, -0.4964154566688013248 ) ) ;
#41652 = CARTESIAN_POINT ( 'NONE',  ( 91.67571176799445709, 21.20498955963030596, 31.65844119682673963 ) ) ;
#41653 = VECTOR ( 'NONE', #36536, 1000.000000000000000 ) ;
#41654 = VERTEX_POINT ( 'NONE', #7466 ) ;
#41655 = AXIS2_PLACEMENT_3D ( 'NONE', #34047, #43877, #49498 ) ;
#41656 = CARTESIAN_POINT ( 'NONE',  ( 106.0228389049370321, 28.07756796303168301, -22.78257232089758944 ) ) ;
#41657 = CARTESIAN_POINT ( 'NONE',  ( 8.480442907658519047, 6.376693431076494889, 66.06409635396809676 ) ) ;
#41658 = CARTESIAN_POINT ( 'NONE',  ( -24.71645982722742119, 9.599558729461499240, 41.05070016659301047 ) ) ;
#41659 = CARTESIAN_POINT ( 'NONE',  ( 201.9822477997853412, 104.3642793804899895, 29.70478973244642873 ) ) ;
#41660 = CARTESIAN_POINT ( 'NONE',  ( -72.03776141304246039, 20.97207231437463548, 88.08361387805356912 ) ) ;
#41662 = VERTEX_POINT ( 'NONE', #45783 ) ;
#41661 = DIRECTION ( 'NONE',  ( -1.000000000000000000, 0.000000000000000000, 0.000000000000000000 ) ) ;
#41663 = CARTESIAN_POINT ( 'NONE',  ( 70.51522979775974420, 15.57935281015687323, 37.81516837416805998 ) ) ;
#41664 = ORIENTED_EDGE ( 'NONE', *, *, #34077, .F. ) ;
#41665 = VECTOR ( 'NONE', #40539, 1000.000000000000227 ) ;
#41666 = EDGE_LOOP ( 'NONE', ( #47859, #64047 ) ) ;
#41667 = CARTESIAN_POINT ( 'NONE',  ( 117.3246714514015707, 33.42485879931865611, -72.78854422093228038 ) ) ;
#41668 = CARTESIAN_POINT ( 'NONE',  ( 427.4999999999999432, 207.5000000000000284, 1.999999999999998224 ) ) ;
#41669 = CARTESIAN_POINT ( 'NONE',  ( 203.1420903260746229, 104.2307086582027864, -63.28900608065381306 ) ) ;
#41670 = CARTESIAN_POINT ( 'NONE',  ( -37.37206033059241861, 11.66494618096612967, 59.96638633092528892 ) ) ;
#41671 = CARTESIAN_POINT ( 'NONE',  ( -120.4586945679390482, 43.01762219615316241, 70.15563910072147280 ) ) ;
#41672 = CARTESIAN_POINT ( 'NONE',  ( -83.69370847062539553, 25.38703975185374517, -21.34185604462549790 ) ) ;
#41673 = DIRECTION ( 'NONE',  ( 1.000000000000000000, 0.000000000000000000, 0.000000000000000000 ) ) ;
#41674 = EDGE_CURVE ( 'NONE', #14714, #8542, #40160, .T. ) ;
#41675 = CARTESIAN_POINT ( 'NONE',  ( -157.0069704378501854, 70.81086990254192415, -41.73065021801657082 ) ) ;
#41676 = ORIENTED_EDGE ( 'NONE', *, *, #51845, .F. ) ;
#41677 = ORIENTED_EDGE ( 'NONE', *, *, #15797, .F. ) ;
#41678 = VECTOR ( 'NONE', #44268, 1000.000000000000000 ) ;
#41679 = DIRECTION ( 'NONE',  ( 0.000000000000000000, 0.000000000000000000, -1.000000000000000000 ) ) ;
#41680 = CARTESIAN_POINT ( 'NONE',  ( -78.66644367742111399, 23.39876645725287219, -50.11545063171791270 ) ) ;
#41681 = CARTESIAN_POINT ( 'NONE',  ( 102.9219037530332486, 25.63991434460579200, 92.46589979971660966 ) ) ;
#41682 = CARTESIAN_POINT ( 'NONE',  ( 10.06749493632500503, -74.32123213259498584, 0.000000000000000000 ) ) ;
#41683 = LINE ( 'NONE', #64167, #20257 ) ;
#41684 = FACE_OUTER_BOUND ( 'NONE', #52781, .T. ) ;
#41685 = CARTESIAN_POINT ( 'NONE',  ( 412.3372781065085633, 219.4906275429376308, -144.4497041420117682 ) ) ;
#41686 = ORIENTED_EDGE ( 'NONE', *, *, #1260, .T. ) ;
#41687 = ADVANCED_FACE ( 'NONE', ( #60566 ), #13766, .F. ) ;
#41688 = VERTEX_POINT ( 'NONE', #61612 ) ;
#41689 = EDGE_CURVE ( 'NONE', #48097, #36977, #44744, .T. ) ;
#41690 = EDGE_LOOP ( 'NONE', ( #3315, #1023, #40500, #65521, #62901, #5058, #31975, #55182, #30559, #4992, #37250, #57444 ) ) ;
#41691 = EDGE_CURVE ( 'NONE', #32243, #37937, #1477, .T. ) ;
#41692 = CARTESIAN_POINT ( 'NONE',  ( -15.55634918610396866, 31.11269837220809009, 2.000000000000001776 ) ) ;
#41693 = CARTESIAN_POINT ( 'NONE',  ( -84.97622048504844372, 24.82614411847755420, 60.70097479970424104 ) ) ;
#41694 = CARTESIAN_POINT ( 'NONE',  ( 105.0322429538348672, -21.99260513325770816, -0.6553719608279887643 ) ) ;
#41695 = EDGE_CURVE ( 'NONE', #63634, #58410, #13428, .T. ) ;
#41696 = VECTOR ( 'NONE', #55548, 1000.000000000000000 ) ;
#41697 = CARTESIAN_POINT ( 'NONE',  ( -32.40928421737412890, 10.77259363352673915, -77.11483472157956953 ) ) ;
#41698 = DIRECTION ( 'NONE',  ( 0.000000000000000000, 0.000000000000000000, 1.000000000000000000 ) ) ;
#41699 = CARTESIAN_POINT ( 'NONE',  ( 32.46582168790594380, 7.608418697099895489, 67.14276555145990244 ) ) ;
#41700 = CARTESIAN_POINT ( 'NONE',  ( 9.827939172326077610, 6.382931149346554811, -11.59534592424589228 ) ) ;
#41701 = AXIS2_PLACEMENT_3D ( 'NONE', #8691, #9032, #46297 ) ;
#41702 = ORIENTED_EDGE ( 'NONE', *, *, #10735, .F. ) ;
#41703 = CARTESIAN_POINT ( 'NONE',  ( 21.75198946226450047, 7.772524967554915953, 6.095983826864362243 ) ) ;
#41704 = CARTESIAN_POINT ( 'NONE',  ( 184.0013086981203401, 81.60415045669145684, 70.57588972765756807 ) ) ;
#41705 = DIRECTION ( 'NONE',  ( 0.000000000000000000, -1.000000000000000000, 0.000000000000000000 ) ) ;
#41706 = CYLINDRICAL_SURFACE ( 'NONE', #12948, 25.00000000000395772 ) ;
#41707 = CARTESIAN_POINT ( 'NONE',  ( -65.00000000000000000, 7.960204194457797252E-15, -0.002000000000002000178 ) ) ;
#41708 = CARTESIAN_POINT ( 'NONE',  ( 16.77480716385436921, 7.540753720029936602, -23.62535031654175199 ) ) ;
#41709 = CARTESIAN_POINT ( 'NONE',  ( 203.9276061909314990, 105.2889220654479061, 56.05227132923313604 ) ) ;
#41710 = VECTOR ( 'NONE', #46416, 1000.000000000000000 ) ;
#41711 = CIRCLE ( 'NONE', #49570, 243.4957430088094839 ) ;
#41712 = ORIENTED_EDGE ( 'NONE', *, *, #15088, .T. ) ;
#41713 = DIRECTION ( 'NONE',  ( -0.000000000000000000, 1.000000000000000000, -0.000000000000000000 ) ) ;
#41714 = APPLICATION_PROTOCOL_DEFINITION ( 'draft international standard', 'automotive_design', 1998, #13005 ) ;
#41715 = PRESENTATION_LAYER_ASSIGNMENT (  '', '', ( #2405 ) ) ;
#41716 = CARTESIAN_POINT ( 'NONE',  ( 176.6214367443247397, 74.20967084876662057, 42.85525822452583355 ) ) ;
#41717 = CARTESIAN_POINT ( 'NONE',  ( -31.08850300935970878, -49.36609570479362930, 27.58472369403420643 ) ) ;
#41718 = ADVANCED_FACE ( 'NONE', ( #12383 ), #24018, .F. ) ;
#41719 = CARTESIAN_POINT ( 'NONE',  ( -109.7686203588201295, 37.90089348911612888, -42.02286914772454907 ) ) ;
#41720 = ADVANCED_FACE ( 'NONE', ( #55993 ), #39460, .T. ) ;
#41721 = DIRECTION ( 'NONE',  ( -1.000000000000000000, 0.000000000000000000, 0.000000000000000000 ) ) ;
#41722 = ORIENTED_EDGE ( 'NONE', *, *, #13678, .T. ) ;
#41723 = ORIENTED_EDGE ( 'NONE', *, *, #49743, .T. ) ;
#41724 = ADVANCED_FACE ( 'NONE', ( #39128 ), #7808, .F. ) ;
#41725 = FACE_BOUND ( 'NONE', #57086, .T. ) ;
#41726 = CARTESIAN_POINT ( 'NONE',  ( 197.3700262219431067, 98.41176242030789467, 11.49295832791582050 ) ) ;
#41727 = EDGE_LOOP ( 'NONE', ( #8446, #67443, #1704, #47014 ) ) ;
#41728 = CARTESIAN_POINT ( 'NONE',  ( 151.3976820382521851, 54.32583990172415156, 94.99999999999866418 ) ) ;
#41729 = ORIENTED_EDGE ( 'NONE', *, *, #35646, .T. ) ;
#41730 = CARTESIAN_POINT ( 'NONE',  ( 128.0882145863933772, 39.20607399008167704, -75.18710712909908978 ) ) ;
#41731 = CARTESIAN_POINT ( 'NONE',  ( 130.7531879853686405, 39.58149302537893988, 43.85379998291934101 ) ) ;
#41732 = DIRECTION ( 'NONE',  ( 3.035766082959412908E-16, -1.033681467326434969E-16, -1.000000000000000000 ) ) ;
#41733 = CARTESIAN_POINT ( 'NONE',  ( -97.88309373898361798, 30.60238467438961862, 31.92441710568320801 ) ) ;
#41734 = CARTESIAN_POINT ( 'NONE',  ( 42.02161712141799654, -16.09918303830818687, 30.00000000000000000 ) ) ;
#41736 = ORIENTED_EDGE ( 'NONE', *, *, #8036, .T. ) ;
#41735 = DIRECTION ( 'NONE',  ( 0.000000000000000000, 1.000000000000000000, -0.000000000000000000 ) ) ;
#41737 = CARTESIAN_POINT ( 'NONE',  ( -17.50000000000000000, 207.5000000000000284, 0.000000000000000000 ) ) ;
#41738 = VERTEX_POINT ( 'NONE', #7103 ) ;
#41739 = ORIENTED_EDGE ( 'NONE', *, *, #62280, .T. ) ;
#41740 = CARTESIAN_POINT ( 'NONE',  ( -166.2053056899075045, 81.18967388993343093, 8.560883375255476935 ) ) ;
#41741 = DIRECTION ( 'NONE',  ( -0.04796746679614544845, 0.000000000000000000, -0.9988488985473031878 ) ) ;
#41742 = APPLICATION_CONTEXT ( 'automotive_design' ) ;
#41743 = CARTESIAN_POINT ( 'NONE',  ( -175.9852529046322616, 90.37283472601129120, -8.422923135414874807 ) ) ;
#41745 = ORIENTED_EDGE ( 'NONE', *, *, #54960, .T. ) ;
#41744 = CARTESIAN_POINT ( 'NONE',  ( -128.9863978264385480, 49.78205252558957739, 71.80115395911820997 ) ) ;
#41746 = CARTESIAN_POINT ( 'NONE',  ( -106.7873000096882947, 36.27154431140346702, 85.70575407879229601 ) ) ;
#41747 = MANIFOLD_SOLID_BREP ( 'Boss-Extrude2', #10318 ) ;
#41748 = AXIS2_PLACEMENT_3D ( 'NONE', #34204, #29601, #24347 ) ;
#41749 = CARTESIAN_POINT ( 'NONE',  ( 0.000000000000000000, 0.000000000000000000, 43.58025477438756212 ) ) ;
#41750 = ORIENTED_EDGE ( 'NONE', *, *, #9966, .F. ) ;
#41751 = AXIS2_PLACEMENT_3D ( 'NONE', #45973, #62851, #67441 ) ;
#41752 = CARTESIAN_POINT ( 'NONE',  ( -62.15324028806259093, 16.70091357159900980, -13.40636474727677552 ) ) ;
#41753 = VECTOR ( 'NONE', #49251, 1000.000000000000000 ) ;
#41754 = AXIS2_PLACEMENT_3D ( 'NONE', #36255, #57711, #31663 ) ;
#41755 = CARTESIAN_POINT ( 'NONE',  ( -128.7724923851857000, 49.63576597317770478, -62.32888474247882016 ) ) ;
#41756 = EDGE_CURVE ( 'NONE', #30714, #60665, #39733, .T. ) ;
#41757 = CARTESIAN_POINT ( 'NONE',  ( 57.83361077722076971, 11.53004742544596795, -91.47238847476954504 ) ) ;
#41758 = CARTESIAN_POINT ( 'NONE',  ( 5.799999999999999822, 0.000000000000000000, 0.000000000000000000 ) ) ;
#41759 = CARTESIAN_POINT ( 'NONE',  ( 69.48877314113909165, 15.30784187978995448, -66.26917009106811918 ) ) ;
#41760 = VERTEX_POINT ( 'NONE', #56680 ) ;
#41761 = ORIENTED_EDGE ( 'NONE', *, *, #8511, .T. ) ;
#41762 = CARTESIAN_POINT ( 'NONE',  ( 182.7720841008444381, 80.32850885226592652, -77.88031079567201687 ) ) ;
#41763 = CLOSED_SHELL ( 'NONE', ( #10210, #21219, #30138, #7741, #47931, #53192 ) ) ;
#41764 = LINE ( 'NONE', #37166, #69405 ) ;
#41765 = FACE_BOUND ( 'NONE', #54432, .T. ) ;
#41766 = CARTESIAN_POINT ( 'NONE',  ( 311.9975424824652350, 296.0000000000000000, 420.0000000000000000 ) ) ;
#41767 = CARTESIAN_POINT ( 'NONE',  ( -74.39861643904070831, 21.81123504700007487, 44.09021573614353429 ) ) ;
#41768 = CARTESIAN_POINT ( 'NONE',  ( 81.04675113612958626, 17.59091904316107247, 42.24460685193674436 ) ) ;
#41769 = CARTESIAN_POINT ( 'NONE',  ( 69.72564955710444679, 15.37006465677308853, -39.86102107153551088 ) ) ;
#41770 = CARTESIAN_POINT ( 'NONE',  ( -122.1940143064357187, 45.29738883755587153, 44.64808725341385554 ) ) ;
#41771 = CARTESIAN_POINT ( 'NONE',  ( -165.7699288023690087, 79.30174988963861438, -70.57208739678948461 ) ) ;
#41772 = EDGE_CURVE ( 'NONE', #3113, #30998, #43118, .T. ) ;
#41773 = ORIENTED_EDGE ( 'NONE', *, *, #67158, .F. ) ;
#41774 = CARTESIAN_POINT ( 'NONE',  ( -102.2801239173131194, 32.78103895658057354, -8.170026674512225640 ) ) ;
#41775 = ORIENTED_EDGE ( 'NONE', *, *, #42622, .F. ) ;
#41776 = CARTESIAN_POINT ( 'NONE',  ( -38.16002576456688899, 10.79155573432543314, 7.534217346251379510 ) ) ;
#41777 = DIRECTION ( 'NONE',  ( -0.7530714660036195163, 0.6579387259397027066, 0.000000000000000000 ) ) ;
#41778 = EDGE_CURVE ( 'NONE', #5626, #56227, #27331, .T. ) ;
#41779 = DIRECTION ( 'NONE',  ( -1.000000000000000000, 0.000000000000000000, 0.000000000000000000 ) ) ;
#41780 = CARTESIAN_POINT ( 'NONE',  ( -189.9554299271397895, 108.0836897899587825, -65.72664125847879291 ) ) ;
#41781 = FACE_OUTER_BOUND ( 'NONE', #68057, .T. ) ;
#41782 = EDGE_CURVE ( 'NONE', #30336, #22171, #21456, .T. ) ;
#41783 = LINE ( 'NONE', #41439, #669 ) ;
#41784 = CARTESIAN_POINT ( 'NONE',  ( 34.45500533947588906, 7.817363290423890554, 16.22768104404066491 ) ) ;
#41785 = CARTESIAN_POINT ( 'NONE',  ( -38.27142476814294980, 2.189438101076349508, 13.32819299319723783 ) ) ;
#41786 = CARTESIAN_POINT ( 'NONE',  ( -46.66904755831210139, 5.000000000000066613, 2.000000000000001776 ) ) ;
#41787 = EDGE_CURVE ( 'NONE', #55692, #22488, #37425, .T. ) ;
#41788 = VERTEX_POINT ( 'NONE', #53794 ) ;
#41789 = CARTESIAN_POINT ( 'NONE',  ( -124.4645780562616153, 46.76022866786750143, -88.73732779037004548 ) ) ;
#41790 = ORIENTED_EDGE ( 'NONE', *, *, #2182, .F. ) ;
#41791 = DIRECTION ( 'NONE',  ( -1.387778780781445676E-16, 1.000000000000000000, 4.294171409582122931E-32 ) ) ;
#41792 = CARTESIAN_POINT ( 'NONE',  ( 8.478575283864735468, 7.382882227715641399, -68.16705165657022292 ) ) ;
#41793 = CARTESIAN_POINT ( 'NONE',  ( 72.99999999999998579, 8.939921633775675282E-15, 85.00000000000000000 ) ) ;
#41794 = CARTESIAN_POINT ( 'NONE',  ( 444.9999999999999432, 225.0000000000000000, 2.000000000000000000 ) ) ;
#41795 = LINE ( 'NONE', #68852, #23124 ) ;
#41796 = CARTESIAN_POINT ( 'NONE',  ( -94.88380767928869375, 29.17964217339916999, -14.40065432143456370 ) ) ;
#41797 = CARTESIAN_POINT ( 'NONE',  ( 155.2992895652387801, 57.24699634758579947, -50.81692795492956805 ) ) ;
#41798 = ORIENTED_EDGE ( 'NONE', *, *, #1915, .F. ) ;
#41799 = AXIS2_PLACEMENT_3D ( 'NONE', #28484, #50630, #56255 ) ;
#41800 = DIRECTION ( 'NONE',  ( 1.015474350197485724E-14, -1.000000000000000000, -4.104355744161124797E-15 ) ) ;
#41801 = CARTESIAN_POINT ( 'NONE',  ( -150.5993571094983849, 66.43939758484181368, 57.64208039007107232 ) ) ;
#41802 = CARTESIAN_POINT ( 'NONE',  ( -36.11269837220804391, 15.55634918610408945, 2.000000000000000000 ) ) ;
#41803 = CARTESIAN_POINT ( 'NONE',  ( -106.6711220790662935, 36.20923238211247508, 58.77858017870315877 ) ) ;
#41804 = CARTESIAN_POINT ( 'NONE',  ( 0.000000000000000000, 70.00000000000000000, 0.000000000000000000 ) ) ;
#41805 = VERTEX_POINT ( 'NONE', #27074 ) ;
#41806 = CARTESIAN_POINT ( 'NONE',  ( -15.55634918610396866, 31.11269837220809009, 85.00100000000000477 ) ) ;
#41807 = VECTOR ( 'NONE', #4542, 1000.000000000000000 ) ;
#41808 = CARTESIAN_POINT ( 'NONE',  ( 87.59061758233883666, 19.75077892934020340, 71.51036996035465165 ) ) ;
#41809 = EDGE_CURVE ( 'NONE', #52011, #59523, #21795, .T. ) ;
#41810 = CARTESIAN_POINT ( 'NONE',  ( 116.6734749296699079, 31.97209464358272157, 41.00315203584806056 ) ) ;
#41811 = VECTOR ( 'NONE', #59396, 1000.000000000000000 ) ;
#41813 = VECTOR ( 'NONE', #52017, 1000.000000000000000 ) ;
#41812 = CARTESIAN_POINT ( 'NONE',  ( -35.00000000000002842, 225.0000000000000000, 378.0000000000000000 ) ) ;
#41814 = CARTESIAN_POINT ( 'NONE',  ( 134.7770330630253284, 41.98246829846536343, 44.46794315559043298 ) ) ;
#41815 = AXIS2_PLACEMENT_3D ( 'NONE', #10497, #42173, #15449 ) ;
#41816 = ORIENTED_EDGE ( 'NONE', *, *, #43792, .F. ) ;
#41817 = CARTESIAN_POINT ( 'NONE',  ( 204.6977192012829789, 106.3443248447423599, 29.20772073876942088 ) ) ;
#41818 = CARTESIAN_POINT ( 'NONE',  ( 117.0065308422768595, 32.13872219870569324, -73.51785692831180086 ) ) ;
#41819 = CARTESIAN_POINT ( 'NONE',  ( 188.5842358232186484, 88.03712271786936583, 36.50917097965209024 ) ) ;
#41820 = CARTESIAN_POINT ( 'NONE',  ( 157.2533363798599737, 58.75760182111574892, 29.40946747225335756 ) ) ;
#41821 = CARTESIAN_POINT ( 'NONE',  ( 140.0012045870120687, 45.26048451937214878, 94.99999999999866418 ) ) ;
#41822 = CLOSED_SHELL ( 'NONE', ( #57806, #60125, #38610, #51690, #61403, #43338, #38076, #43924, #23960, #69470, #41372, #18451, #2799, #42960, #25517, #14748, #40286, #43419, #25190, #18903, #37822, #52898, #37242, #57648, #64457, #41130, #4152, #28025 ) ) ;
#41823 = EDGE_LOOP ( 'NONE', ( #5542, #14801, #45822, #59812 ) ) ;
#41824 = CARTESIAN_POINT ( 'NONE',  ( -430.1627218934916073, 400.0000000000064801, 91.05029585798840230 ) ) ;
#41825 = ORIENTED_EDGE ( 'NONE', *, *, #43355, .T. ) ;
#41826 = CARTESIAN_POINT ( 'NONE',  ( -104.1342612728951593, 33.73231160250194449, -49.79675383502204511 ) ) ;
#41827 = CARTESIAN_POINT ( 'NONE',  ( 139.5488375718656755, 44.96856655640365830, 85.77057805547978830 ) ) ;
#41828 = CARTESIAN_POINT ( 'NONE',  ( -62.56514071794335052, 16.82532503654671885, 37.82479515852823937 ) ) ;
#41830 = ORIENTED_EDGE ( 'NONE', *, *, #24253, .F. ) ;
#41829 = CARTESIAN_POINT ( 'NONE',  ( 150.9128604434957310, 53.97103482421775311, 6.386753527089024551 ) ) ;
#41831 = PLANE ( 'NONE',  #42034 ) ;
#41832 = DIRECTION ( 'NONE',  ( -0.7071067811865543451, -7.105427357601001070E-15, -0.7071067811865408004 ) ) ;
#41833 = CARTESIAN_POINT ( 'NONE',  ( 114.6797682035589219, 32.10876583290006892, -49.48826977818937678 ) ) ;
#41834 = ORIENTED_EDGE ( 'NONE', *, *, #26459, .T. ) ;
#41835 = DIRECTION ( 'NONE',  ( 0.000000000000000000, 0.000000000000000000, 1.000000000000000000 ) ) ;
#41836 = EDGE_CURVE ( 'NONE', #32499, #9081, #13919, .T. ) ;
#41837 = EDGE_CURVE ( 'NONE', #15244, #46033, #60484, .T. ) ;
#41838 = CARTESIAN_POINT ( 'NONE',  ( 188.9999999999999432, -35.00000000000000000, -2.000000000000000000 ) ) ;
#41839 = ORIENTED_EDGE ( 'NONE', *, *, #31315, .T. ) ;
#41840 = CARTESIAN_POINT ( 'NONE',  ( 133.8566784816069060, 41.42467568809810530, 56.35489142945903751 ) ) ;
#41841 = ADVANCED_FACE ( 'NONE', ( #66139 ), #61185, .T. ) ;
#41842 = CARTESIAN_POINT ( 'NONE',  ( -173.1211646369891071, 87.12891641440859303, 45.82169460664104577 ) ) ;
#41843 = CARTESIAN_POINT ( 'NONE',  ( 150.7926588734435427, 52.63999027731880886, 67.17871942891498804 ) ) ;
#41844 = CARTESIAN_POINT ( 'NONE',  ( 91.11019107624156277, 22.06959540317787827, 43.23133666582459966 ) ) ;
#41845 = ORIENTED_EDGE ( 'NONE', *, *, #44211, .F. ) ;
#41846 = CARTESIAN_POINT ( 'NONE',  ( 46.12582897016703498, 10.39833982076227592, 13.90098705123808109 ) ) ;
#41847 = VERTEX_POINT ( 'NONE', #38683 ) ;
#41848 = CARTESIAN_POINT ( 'NONE',  ( 149.9683128897950155, 53.28564708287390062, -16.24937733141493368 ) ) ;
#41849 = CARTESIAN_POINT ( 'NONE',  ( -61.59945957978030151, 16.53503624374673109, 87.83294754670791349 ) ) ;
#41850 = CARTESIAN_POINT ( 'NONE',  ( 107.9213359589208920, 28.92595015506874390, 44.25850654564636244 ) ) ;
#41851 = VECTOR ( 'NONE', #47352, 1000.000000000000000 ) ;
#41852 = CARTESIAN_POINT ( 'NONE',  ( -156.1462053606562677, 70.02140399657012892, -65.65745857927204554 ) ) ;
#41853 = CARTESIAN_POINT ( 'NONE',  ( 55.52619835477052135, 11.05941016560235823, 91.52244839951424638 ) ) ;
#41854 = B_SPLINE_CURVE_WITH_KNOTS ( 'NONE', 3,
 ( #6577, #5192, #27322, #65323 ),
 .UNSPECIFIED., .F., .F.,
 ( 4, 4 ),
 ( 0.1259919275528364746, 0.1829744153748763535 ),
 .UNSPECIFIED. ) ;
#41855 = CARTESIAN_POINT ( 'NONE',  ( 184.9757174666827382, 84.09845285279331506, 3.548900157282363299 ) ) ;
#41856 = LINE ( 'NONE', #57344, #3589 ) ;
#41858 = FACE_OUTER_BOUND ( 'NONE', #44786, .T. ) ;
#41857 = VECTOR ( 'NONE', #15564, 1000.000000000000000 ) ;
#41859 = ORIENTED_EDGE ( 'NONE', *, *, #51773, .T. ) ;
#41860 = DIRECTION ( 'NONE',  ( 0.000000000000000000, -0.000000000000000000, 1.000000000000000000 ) ) ;
#41861 = ORIENTED_EDGE ( 'NONE', *, *, #23699, .T. ) ;
#41862 = EDGE_CURVE ( 'NONE', #5291, #61739, #47586, .T. ) ;
#41863 = CARTESIAN_POINT ( 'NONE',  ( 39.88975917505627677, 9.487965272711658571, -23.77526687496410673 ) ) ;
#41864 = EDGE_CURVE ( 'NONE', #46944, #24801, #28833, .T. ) ;
#41865 = DIRECTION ( 'NONE',  ( 1.000000000000000000, 0.000000000000000000, 0.000000000000000000 ) ) ;
#41866 = DIRECTION ( 'NONE',  ( 1.000000000000000000, 0.000000000000000000, 0.000000000000000000 ) ) ;
#41867 = MANIFOLD_SOLID_BREP ( 'Cut-Revolve1', #66543 ) ;
#41868 = CARTESIAN_POINT ( 'NONE',  ( -0.6810348268179097220, 6.531004596334747170, 88.99908247484378876 ) ) ;
#41869 = CARTESIAN_POINT ( 'NONE',  ( -109.3585523124447576, 37.67345343047318806, -13.13767328143380375 ) ) ;
#41870 = ORIENTED_EDGE ( 'NONE', *, *, #24458, .F. ) ;
#41871 = CARTESIAN_POINT ( 'NONE',  ( 21.96921518829188358, 71.65937688154191676, 41.38025477438755928 ) ) ;
#41872 = DIRECTION ( 'NONE',  ( -0.7071067811865476838, 6.441404958702661839E-16, -0.7071067811865474617 ) ) ;
#41873 = ORIENTED_EDGE ( 'NONE', *, *, #8877, .F. ) ;
#41874 = VERTEX_POINT ( 'NONE', #45348 ) ;
#41875 = CARTESIAN_POINT ( 'NONE',  ( -153.1121305730336815, 67.29834700374526335, 44.80172431058477400 ) ) ;
#41876 = CARTESIAN_POINT ( 'NONE',  ( 55.61382797299286551, 11.07686102552912111, -44.45554761801439270 ) ) ;
#41877 = CARTESIAN_POINT ( 'NONE',  ( 444.4083459183744935, 365.0000000000066507, -143.5207719538776132 ) ) ;
#41878 = CARTESIAN_POINT ( 'NONE',  ( 6.526941389886392386, -24.13294503563501436, 0.000000000000000000 ) ) ;
#41879 = CARTESIAN_POINT ( 'NONE',  ( -142.9728934044261734, 58.82891228489262403, 7.656646529977067850 ) ) ;
#41880 = VERTEX_POINT ( 'NONE', #50288 ) ;
#41881 = CARTESIAN_POINT ( 'NONE',  ( -133.3316503378477478, 52.82738260200862612, 37.01664400818041400 ) ) ;
#41882 = ORIENTED_EDGE ( 'NONE', *, *, #29262, .F. ) ;
#41883 = CARTESIAN_POINT ( 'NONE',  ( 212.0850679406003678, 117.0583048437722056, 11.20260716300226633 ) ) ;
#41884 = CARTESIAN_POINT ( 'NONE',  ( -142.0729208125266609, 59.40063722436772053, 39.35843688284292341 ) ) ;
#41885 = CARTESIAN_POINT ( 'NONE',  ( 211.0967808702091020, 115.5516932918876734, 32.78604062416883380 ) ) ;
#41886 = CARTESIAN_POINT ( 'NONE',  ( -63.33140416796853600, 16.18162651919394435, 3.125053320693577513E-16 ) ) ;
#41887 = VERTEX_POINT ( 'NONE', #23213 ) ;
#41888 = ORIENTED_EDGE ( 'NONE', *, *, #50896, .F. ) ;
#41889 = CARTESIAN_POINT ( 'NONE',  ( 112.5087422071486856, -21.56900326173646931, -4.337278505387113015 ) ) ;
#41890 = CARTESIAN_POINT ( 'NONE',  ( -120.0222670449324767, 43.93136592529501172, 87.13176881600898582 ) ) ;
#41891 = CIRCLE ( 'NONE', #11536, 65.00000000000000000 ) ;
#41892 = CARTESIAN_POINT ( 'NONE',  ( -172.3057147739576749, 86.22480007276992353, -22.83448960614214585 ) ) ;
#41893 = CARTESIAN_POINT ( 'NONE',  ( 0.000000000000000000, 0.000000000000000000, -30.00000000000000000 ) ) ;
#41894 = CARTESIAN_POINT ( 'NONE',  ( 23.28688665153870474, 6.856560375048495359, 91.56380556558386274 ) ) ;
#41895 = CARTESIAN_POINT ( 'NONE',  ( 10.03051694092593316, 7.390832984323265187, 86.38638643135473671 ) ) ;
#41896 = AXIS2_PLACEMENT_3D ( 'NONE', #35099, #13994, #63222 ) ;
#41897 = EDGE_LOOP ( 'NONE', ( #57060, #41215, #48208, #48039 ) ) ;
#41898 = DIRECTION ( 'NONE',  ( 1.000000000000000000, -3.344045254895050726E-17, -0.000000000000000000 ) ) ;
#41899 = CARTESIAN_POINT ( 'NONE',  ( -98.69283175933881580, 30.99524616306737101, 58.25983389827380421 ) ) ;
#41900 = ORIENTED_EDGE ( 'NONE', *, *, #68025, .F. ) ;
#41901 = VECTOR ( 'NONE', #52174, 1000.000000000000000 ) ;
#41902 = CARTESIAN_POINT ( 'NONE',  ( -82.53770812813169755, 23.83403279300011590, 4.645480920856400076 ) ) ;
#41903 = ORIENTED_EDGE ( 'NONE', *, *, #62489, .F. ) ;
#41904 = LINE ( 'NONE', #29973, #66974 ) ;
#41905 = ORIENTED_EDGE ( 'NONE', *, *, #14337, .T. ) ;
#41906 = ORIENTED_EDGE ( 'NONE', *, *, #27290, .T. ) ;
#41907 = CARTESIAN_POINT ( 'NONE',  ( 11.82322073186612954, 6.406156243758795554, -49.38981688001822334 ) ) ;
#41908 = CARTESIAN_POINT ( 'NONE',  ( -174.7800083645697100, 88.99302808536937448, 57.84004054586915800 ) ) ;
#41909 = CARTESIAN_POINT ( 'NONE',  ( 133.8566784816069060, 41.42467568809810530, 56.35489142945903751 ) ) ;
#41910 = B_SPLINE_CURVE_WITH_KNOTS ( 'NONE', 3,
 ( #7706, #34091, #66807, #28812, #44975, #66458, #50602, #2422, #23877, #18598, #14699, #62555, #46709, #63239, #24921, #3124, #8397, #57620, #15051, #24584, #51651, #35117, #67485, #56933, #56575, #29491, #30538, #67834, #29843, #30888, #18947, #3459, #2767, #47056, #36161, #30200, #41094, #45681, #35822, #51987, #13664, #46018, #46354, #40393, #19281 ),
 .UNSPECIFIED., .F., .F.,
 ( 4, 2, 2, 1, 2, 2, 2, 2, 2, 2, 2, 2, 2, 2, 2, 2, 2, 2, 2, 2, 2, 2, 4 ),
 ( 0.02346464386237015476, 0.02493212228186622928, 0.02566586149161426827, 0.02639960070136230380, 0.02713333991111034280, 0.02786707912085838179, 0.02933455754035447019, 0.03006829675010251959, 0.03080203595985056900, 0.03226951437934669209, 0.03300325358909474843, 0.03373699279884281171, 0.03520447121833893134, 0.03667194963783505096, 0.03740568884758310730, 0.03813942805733116365, 0.03960690647682728327, 0.04107438489632340983, 0.04254186331581952946, 0.04327560252556759968, 0.04400934173531566990, 0.04547682015481181034, 0.04694429857430795078 ),
 .UNSPECIFIED. ) ;
#41911 = ORIENTED_EDGE ( 'NONE', *, *, #13989, .F. ) ;
#41912 = EDGE_CURVE ( 'NONE', #36296, #8726, #25619, .T. ) ;
#41913 = CARTESIAN_POINT ( 'NONE',  ( 110.2429982417149574, -170.0000000000000000, -24.07788697519002596 ) ) ;
#41914 = DIRECTION ( 'NONE',  ( 0.5409654940743039431, 0.000000000000000000, 0.8410447872859947438 ) ) ;
#41915 = EDGE_CURVE ( 'NONE', #6663, #20568, #38169, .T. ) ;
#41916 = DIRECTION ( 'NONE',  ( -0.000000000000000000, -0.000000000000000000, -1.000000000000000000 ) ) ;
#41917 = LINE ( 'NONE', #35615, #38330 ) ;
#41918 = CARTESIAN_POINT ( 'NONE',  ( -26.87327614295025313, 8.886070347947290671, 43.68680226973125258 ) ) ;
#41919 = DIRECTION ( 'NONE',  ( -0.000000000000000000, 0.000000000000000000, -1.000000000000000000 ) ) ;
#41920 = ORIENTED_EDGE ( 'NONE', *, *, #35980, .F. ) ;
#41921 = EDGE_CURVE ( 'NONE', #26782, #24447, #22608, .T. ) ;
#41922 = DIRECTION ( 'NONE',  ( -0.000000000000000000, -0.000000000000000000, 1.000000000000000000 ) ) ;
#41923 = CARTESIAN_POINT ( 'NONE',  ( -86.16710354151693707, 26.41338104675949694, -69.22550752038515043 ) ) ;
#41924 = CARTESIAN_POINT ( 'NONE',  ( 173.7263186949344060, 72.85225335320951956, 8.481618603203305184 ) ) ;
#41925 = CARTESIAN_POINT ( 'NONE',  ( 0.000000000000000000, 0.000000000000000000, -10.00000000000000000 ) ) ;
#41926 = CARTESIAN_POINT ( 'NONE',  ( 0.000000000000000000, 0.000000000000000000, 170.0000000000000000 ) ) ;
#41927 = CARTESIAN_POINT ( 'NONE',  ( 131.6005058089755266, 40.07838125795770878, 2.997865343112388725 ) ) ;
#41928 = CARTESIAN_POINT ( 'NONE',  ( 33.00361537314734051, 7.663360536940698964, -92.89042083272292416 ) ) ;
#41929 = CARTESIAN_POINT ( 'NONE',  ( 197.9644510826045689, 99.15771744523051723, 93.72331163113166497 ) ) ;
#41930 = CARTESIAN_POINT ( 'NONE',  ( 410.0000000000000000, 190.0000000000000000, 380.0000000000000000 ) ) ;
#41931 = CARTESIAN_POINT ( 'NONE',  ( -440.1146514826278349, 400.0000000000064801, 101.0022254471246441 ) ) ;
#41932 = CARTESIAN_POINT ( 'NONE',  ( -109.5025362253418564, 36.60371748273998094, 40.10572810313013292 ) ) ;
#41933 = ORIENTED_EDGE ( 'NONE', *, *, #40988, .F. ) ;
#41934 = AXIS2_PLACEMENT_3D ( 'NONE', #26560, #63504, #36780 ) ;
#41935 = CARTESIAN_POINT ( 'NONE',  ( -47.66938934256014448, 13.85902735690713250, 92.86349970662286069 ) ) ;
#41936 = ORIENTED_EDGE ( 'NONE', *, *, #61693, .T. ) ;
#41937 = CYLINDRICAL_SURFACE ( 'NONE', #20540, 5.000000000000000888 ) ;
#41938 = ORIENTED_EDGE ( 'NONE', *, *, #31734, .T. ) ;
#41939 = EDGE_CURVE ( 'NONE', #9754, #27253, #60594, .T. ) ;
#41940 = CARTESIAN_POINT ( 'NONE',  ( 204.6977192012829789, -170.0000000000000000, -97.51503221354896311 ) ) ;
#41941 = AXIS2_PLACEMENT_3D ( 'NONE', #32342, #53769, #37953 ) ;
#41942 = CARTESIAN_POINT ( 'NONE',  ( -4.999999999999971578, 20.55634918610402906, 0.000000000000000000 ) ) ;
#41943 = B_SPLINE_CURVE_WITH_KNOTS ( 'NONE', 3,
 ( #43095, #64563, #53982, #5808, #27262, #48700, #543, #21994, #23317, #60586, #19406, #34212, #3243, #67607 ),
 .UNSPECIFIED., .F., .F.,
 ( 4, 2, 2, 2, 2, 2, 4 ),
 ( 0.000000000000000000, 0.001269157135653070081, 0.002538314271306140162, 0.003807471406959210027, 0.005076628542612280325, 0.007614942813918446941, 0.01015325708522461443 ),
 .UNSPECIFIED. ) ;
#41944 = CARTESIAN_POINT ( 'NONE',  ( -169.1122507277983118, 84.24359299875010265, 31.96755716570773131 ) ) ;
#41945 = LINE ( 'NONE', #9942, #6379 ) ;
#41946 = CARTESIAN_POINT ( 'NONE',  ( 140.4769819293527178, 46.76840769395176522, -47.05706312325354901 ) ) ;
#41947 = CARTESIAN_POINT ( 'NONE',  ( 32.90953848114694580, 7.653665824624195757, -46.88272753811734361 ) ) ;
#41948 = VECTOR ( 'NONE', #27567, 1000.000000000000000 ) ;
#41949 = CARTESIAN_POINT ( 'NONE',  ( 155.7262569076171417, 56.30477153194511430, -36.27408474916799008 ) ) ;
#41950 = DIRECTION ( 'NONE',  ( -0.9195277725514489076, -0.3930250316539278810, 2.500042656554810340E-16 ) ) ;
#41951 = CARTESIAN_POINT ( 'NONE',  ( -124.1095621208148430, 46.52671329146387791, -8.226765375838317240 ) ) ;
#41952 = ORIENTED_EDGE ( 'NONE', *, *, #29937, .T. ) ;
#41953 = VECTOR ( 'NONE', #62271, 1000.000000000000000 ) ;
#41954 = ORIENTED_EDGE ( 'NONE', *, *, #28347, .F. ) ;
#41955 = AXIS2_PLACEMENT_3D ( 'NONE', #6045, #54582, #5700 ) ;
#41956 = CARTESIAN_POINT ( 'NONE',  ( 182.6575447192646209, 81.65756500564891951, 83.15904816998347826 ) ) ;
#41957 = DIRECTION ( 'NONE',  ( 0.000000000000000000, 0.000000000000000000, -1.000000000000000000 ) ) ;
#41958 = VECTOR ( 'NONE', #54503, 1000.000000000000000 ) ;
#41959 = CARTESIAN_POINT ( 'NONE',  ( -168.1839487819771080, 83.25723186408069409, -9.716778674227802171 ) ) ;
#41960 = AXIS2_PLACEMENT_3D ( 'NONE', #21340, #58281, #5510 ) ;
#41961 = DIRECTION ( 'NONE',  ( -0.7071067811865475727, 4.529112861587823989E-16, -0.7071067811865475727 ) ) ;
#41962 = CARTESIAN_POINT ( 'NONE',  ( 86.62931800182293784, 20.48449268398423584, 17.86753698201564688 ) ) ;
#41963 = DIRECTION ( 'NONE',  ( 0.000000000000000000, 0.6427876096865404731, -0.7660444431189771253 ) ) ;
#41964 = CARTESIAN_POINT ( 'NONE',  ( 180.6710448012267989, 78.18844465372403363, -78.06960825634332934 ) ) ;
#41965 = CARTESIAN_POINT ( 'NONE',  ( 7.762887554996211747E-14, 46.66904755831208718, 85.00100000000000477 ) ) ;
#41966 = CARTESIAN_POINT ( 'NONE',  ( 94.06703982324145841, 22.09435144471463630, -15.47962683577384446 ) ) ;
#41967 = LINE ( 'NONE', #57456, #5029 ) ;
#41968 = DIRECTION ( 'NONE',  ( -0.000000000000000000, -0.000000000000000000, -1.000000000000000000 ) ) ;
#41969 = PLANE ( 'NONE',  #20952 ) ;
#41970 = ORIENTED_EDGE ( 'NONE', *, *, #67294, .T. ) ;
#41971 = CARTESIAN_POINT ( 'NONE',  ( 129.5225439633633755, 40.02995148249138424, 4.026654605326871028 ) ) ;
#41972 = DIRECTION ( 'NONE',  ( 1.000000000000000000, 0.000000000000000000, 0.000000000000000000 ) ) ;
#41973 = CARTESIAN_POINT ( 'NONE',  ( -53.14657859411973106, 15.21831473227210552, 71.91964493646879930 ) ) ;
#41974 = CARTESIAN_POINT ( 'NONE',  ( -106.7004823116342749, 36.22460663120047997, -63.28115470610104154 ) ) ;
#41975 = LINE ( 'NONE', #14891, #3796 ) ;
#41976 = FACE_OUTER_BOUND ( 'NONE', #18761, .T. ) ;
#41977 = EDGE_CURVE ( 'NONE', #64727, #25266, #8306, .T. ) ;
#41978 = ORIENTED_EDGE ( 'NONE', *, *, #63766, .F. ) ;
#41979 = DIRECTION ( 'NONE',  ( -0.000000000000000000, -0.000000000000000000, -1.000000000000000000 ) ) ;
#41980 = CARTESIAN_POINT ( 'NONE',  ( -62.30100056228380367, 16.74548393487070896, 66.65337513678986170 ) ) ;
#41981 = ORIENTED_EDGE ( 'NONE', *, *, #49368, .T. ) ;
#41982 = ORIENTED_EDGE ( 'NONE', *, *, #6157, .F. ) ;
#41983 = VECTOR ( 'NONE', #66588, 1000.000000000000000 ) ;
#41984 = CARTESIAN_POINT ( 'NONE',  ( 45.60406750853972824, 10.31565594232976402, 86.83412138438860950 ) ) ;
#41985 = CARTESIAN_POINT ( 'NONE',  ( -180.6009936245623351, 95.85948119829086522, -68.42513485405468998 ) ) ;
#41986 = DIRECTION ( 'NONE',  ( 0.000000000000000000, 0.000000000000000000, -1.000000000000000000 ) ) ;
#41987 = ORIENTED_EDGE ( 'NONE', *, *, #46368, .F. ) ;
#41988 = DIRECTION ( 'NONE',  ( 0.000000000000000000, 0.000000000000000000, -1.000000000000000000 ) ) ;
#41989 = CARTESIAN_POINT ( 'NONE',  ( -7.330690860789849772, 6.858814156830896458, 18.27103044898354867 ) ) ;
#41990 = VECTOR ( 'NONE', #26637, 1000.000000000000000 ) ;
#41991 = CARTESIAN_POINT ( 'NONE',  ( -1.454841858088668394, 7.566772088227304849, 6.805462143089243909 ) ) ;
#41992 = CARTESIAN_POINT ( 'NONE',  ( 180.6713229637342408, 79.61878926895391828, -51.22505766587962484 ) ) ;
#41993 = CARTESIAN_POINT ( 'NONE',  ( 164.6594616662011106, 63.46377020933756086, 92.76704941086832434 ) ) ;
#41994 = VECTOR ( 'NONE', #29584, 1000.000000000000000 ) ;
#41995 = CARTESIAN_POINT ( 'NONE',  ( 94.07616572255075482, 22.09777530676769430, 36.18770730423079129 ) ) ;
#41996 = VECTOR ( 'NONE', #11209, 1000.000000000000000 ) ;
#41997 = VERTEX_POINT ( 'NONE', #65534 ) ;
#41998 = AXIS2_PLACEMENT_3D ( 'NONE', #1405, #10908, #48868 ) ;
#41999 = EDGE_CURVE ( 'NONE', #56923, #1149, #17327, .T. ) ;
#42000 = CARTESIAN_POINT ( 'NONE',  ( 105.8229724512851249, 27.98935528750253354, -22.64196685832511591 ) ) ;
#42001 = CIRCLE ( 'NONE', #11665, 65.00000000000000000 ) ;
#42002 = CARTESIAN_POINT ( 'NONE',  ( 13.84937401517046318, 6.446378549072247388, 71.60848226474631417 ) ) ;
#42003 = CARTESIAN_POINT ( 'NONE',  ( -28.81071653159243695, 10.19258396314335258, 44.74508666141489499 ) ) ;
#42004 = CARTESIAN_POINT ( 'NONE',  ( 201.5876148766342908, 103.8397408698165378, 43.54586497944792711 ) ) ;
#42005 = CARTESIAN_POINT ( 'NONE',  ( -75.42286590136558289, 22.18381414075804869, 84.83773244433049854 ) ) ;
#42007 = EDGE_LOOP ( 'NONE', ( #53593, #6328, #16676, #2944 ) ) ;
#42006 = DIRECTION ( 'NONE',  ( 1.000000000000000000, 0.000000000000000000, 0.000000000000000000 ) ) ;
#42008 = EDGE_LOOP ( 'NONE', ( #50517, #54479 ) ) ;
#42009 = AXIS2_PLACEMENT_3D ( 'NONE', #22134, #28102, #43921 ) ;
#42010 = ADVANCED_FACE ( 'NONE', ( #22266 ), #38087, .F. ) ;
#42011 = VERTEX_POINT ( 'NONE', #39487 ) ;
#42012 = LINE ( 'NONE', #14927, #14294 ) ;
#42013 = CARTESIAN_POINT ( 'NONE',  ( 203.9276061909314421, 105.2889220654478777, -78.17048162308530834 ) ) ;
#42014 = LINE ( 'NONE', #20214, #27175 ) ;
#42015 = LINE ( 'NONE', #15289, #35432 ) ;
#42016 = CARTESIAN_POINT ( 'NONE',  ( 157.4703587214989113, 57.65129005721576050, -62.96873488960130771 ) ) ;
#42017 = CARTESIAN_POINT ( 'NONE',  ( 22.34696839782165867, 7.807102111783818188, -93.04585276060377907 ) ) ;
#42018 = CARTESIAN_POINT ( 'NONE',  ( -149.9449619562961686, 64.55090813009799433, -49.81283053149199702 ) ) ;
#42019 = VERTEX_POINT ( 'NONE', #44412 ) ;
#42020 = ORIENTED_EDGE ( 'NONE', *, *, #53796, .T. ) ;
#42021 = EDGE_CURVE ( 'NONE', #1085, #60210, #49856, .T. ) ;
#42022 = CARTESIAN_POINT ( 'NONE',  ( 67.93317348534930034, 14.90531593353392026, -10.69219403348423292 ) ) ;
#42023 = CARTESIAN_POINT ( 'NONE',  ( -85.89078989036968892, 26.29712602777651043, -44.64594958257553969 ) ) ;
#42024 = CARTESIAN_POINT ( 'NONE',  ( 106.8765028100539496, 27.35519873236687260, 84.09029707093864658 ) ) ;
#42026 = EDGE_CURVE ( 'NONE', #68287, #42704, #59532, .T. ) ;
#42025 = CARTESIAN_POINT ( 'NONE',  ( -155.1204242627070471, 70.44799358128194910, 6.395789732132856287 ) ) ;
#42027 = EDGE_CURVE ( 'NONE', #29458, #61321, #18384, .T. ) ;
#42028 = LINE ( 'NONE', #26198, #7916 ) ;
#42029 = CARTESIAN_POINT ( 'NONE',  ( 450.2085304802404835, 188.0000000000000000, -219.9999999999999147 ) ) ;
#42030 = CARTESIAN_POINT ( 'NONE',  ( -189.9051212200399448, 108.7693414241253720, -92.42498137349568310 ) ) ;
#42031 = ORIENTED_EDGE ( 'NONE', *, *, #31141, .T. ) ;
#42032 = EDGE_LOOP ( 'NONE', ( #23725, #68131, #23094, #29199 ) ) ;
#42033 = VERTEX_POINT ( 'NONE', #54608 ) ;
#42034 = AXIS2_PLACEMENT_3D ( 'NONE', #20035, #15100, #25666 ) ;
#42035 = DIRECTION ( 'NONE',  ( 0.000000000000000000, 0.000000000000000000, -1.000000000000000000 ) ) ;
#42036 = CARTESIAN_POINT ( 'NONE',  ( 89.35694261521391013, 21.43730924572641072, -90.01283748679323082 ) ) ;
#42037 = CARTESIAN_POINT ( 'NONE',  ( 105.5080822241900762, -21.88977794987918557, -2.220096651196666659 ) ) ;
#42038 = PLANE ( 'NONE',  #50603 ) ;
#42039 = CARTESIAN_POINT ( 'NONE',  ( 200.4590013143046860, 102.3556155835303088, 57.34765393025211466 ) ) ;
#42040 = VECTOR ( 'NONE', #40063, 1000.000000000000000 ) ;
#42041 = CARTESIAN_POINT ( 'NONE',  ( 31.95008798096002423, 7.556925044648909129, 65.24089643825568885 ) ) ;
#42042 = CARTESIAN_POINT ( 'NONE',  ( 13.37366753069833258, 6.435102282077983737, -23.29209217290729939 ) ) ;
#42043 = CARTESIAN_POINT ( 'NONE',  ( 18.20314211955701822, 7.596739727129570241, 3.552554644654912330 ) ) ;
#42044 = CARTESIAN_POINT ( 'NONE',  ( 188.4359598230020651, 86.36951380984524462, 62.14128191421917791 ) ) ;
#42045 = CARTESIAN_POINT ( 'NONE',  ( -123.4531143159639015, 44.90777521523904880, 4.179957208476558606 ) ) ;
#42046 = CARTESIAN_POINT ( 'NONE',  ( 66.94779593213115731, 13.61918177102164762, -63.67398222617447345 ) ) ;
#42047 = AXIS2_PLACEMENT_3D ( 'NONE', #66895, #12716, #61598 ) ;
#42048 = DIRECTION ( 'NONE',  ( 0.7071067811865474617, 0.000000000000000000, 0.7071067811865474617 ) ) ;
#42049 = CARTESIAN_POINT ( 'NONE',  ( -18.89790202299212396, 62.20684691518604836, 170.0000000000000000 ) ) ;
#42050 = CARTESIAN_POINT ( 'NONE',  ( 201.5903370237274146, 102.1785392640257726, 56.71277855772954979 ) ) ;
#42051 = B_SPLINE_CURVE_WITH_KNOTS ( 'NONE', 3,
 ( #65070, #27076, #22158, #342, #37987, #48860, #59430, #11243, #5963, #27423, #703, #43601, #16869, #38329, #17930, #2112, #39731, #7024, #22850, #45351, #28122, #28477 ),
 .UNSPECIFIED., .F., .F.,
 ( 4, 2, 2, 2, 2, 2, 2, 2, 2, 2, 4 ),
 ( 0.01030631445004988149, 0.01159271714570041245, 0.01223591849352568227, 0.01287911984135095382, 0.01416552253700148478, 0.01480872388482676327, 0.01545192523265203829, 0.01673832792830262650, 0.01738152927612790846, 0.01802473062395318695, 0.02059753601525430092 ),
 .UNSPECIFIED. ) ;
#42052 = ORIENTED_EDGE ( 'NONE', *, *, #51706, .T. ) ;
#42053 = CARTESIAN_POINT ( 'NONE',  ( 185.1802655733641245, 82.84606286178495793, 16.26266218441142541 ) ) ;
#42054 = SHAPE_DEFINITION_REPRESENTATION ( #32711, #64925 ) ;
#42055 = LINE ( 'NONE', #69119, #28440 ) ;
#42056 = DIRECTION ( 'NONE',  ( 1.000000000000000000, 0.000000000000000000, 0.000000000000000000 ) ) ;
#42057 = CARTESIAN_POINT ( 'NONE',  ( -107.7677210873465867, 36.80113675102408166, -47.64980430669002232 ) ) ;
#42058 = CARTESIAN_POINT ( 'NONE',  ( 188.5653887627527752, 88.01608521313127653, -44.33439866442006405 ) ) ;
#42059 = VERTEX_POINT ( 'NONE', #38802 ) ;
#42060 = EDGE_CURVE ( 'NONE', #57348, #21955, #12062, .T. ) ;
#42061 = ORIENTED_EDGE ( 'NONE', *, *, #23667, .T. ) ;
#42062 = FACE_OUTER_BOUND ( 'NONE', #61016, .T. ) ;
#42063 = CARTESIAN_POINT ( 'NONE',  ( 173.6802822489493963, 71.43367662455597156, 91.71180641136416511 ) ) ;
#42064 = VERTEX_POINT ( 'NONE', #28946 ) ;
#42065 = EDGE_CURVE ( 'NONE', #2060, #64129, #27355, .T. ) ;
#42066 = CARTESIAN_POINT ( 'NONE',  ( 116.5096233816162083, 31.89062767870469983, 59.82761199116307438 ) ) ;
#42067 = ORIENTED_EDGE ( 'NONE', *, *, #18828, .T. ) ;
#42068 = CARTESIAN_POINT ( 'NONE',  ( 126.7877523219523255, 38.47018873135925077, -67.80797154038901908 ) ) ;
#42069 = LINE ( 'NONE', #5470, #49706 ) ;
#42070 = LINE ( 'NONE', #58580, #37576 ) ;
#42071 = CARTESIAN_POINT ( 'NONE',  ( 164.2909821920446234, 63.15460073159351140, -94.16473412953207855 ) ) ;
#42072 = CARTESIAN_POINT ( 'NONE',  ( 88.52345267551655184, 20.07594890262053866, -50.58241302559184049 ) ) ;
#42074 = EDGE_LOOP ( 'NONE', ( #49111, #41052, #25451, #61879, #1401, #12509, #25031, #14689, #44001 ) ) ;
#42073 = CARTESIAN_POINT ( 'NONE',  ( 0.000000000000000000, 0.000000000000000000, 41.38025477438755928 ) ) ;
#42075 = EDGE_CURVE ( 'NONE', #48718, #45468, #67863, .T. ) ;
#42076 = DIRECTION ( 'NONE',  ( -0.000000000000000000, 1.000000000000000000, -0.000000000000000000 ) ) ;
#42077 = VERTEX_POINT ( 'NONE', #22966 ) ;
#42079 = ORIENTED_EDGE ( 'NONE', *, *, #54238, .T. ) ;
#42078 = EDGE_CURVE ( 'NONE', #8034, #29948, #41548, .T. ) ;
#42080 = CARTESIAN_POINT ( 'NONE',  ( -170.2856292770789821, 85.50720222068223109, 4.520652531662902263 ) ) ;
#42081 = VECTOR ( 'NONE', #46767, 1000.000000000000000 ) ;
#42082 = DIRECTION ( 'NONE',  ( -0.9959742939952397345, 0.08963930890342655666, 0.000000000000000000 ) ) ;
#42083 = CARTESIAN_POINT ( 'NONE',  ( -173.9656771507955000, 88.06879734510550861, -7.867406574286302856 ) ) ;
#42084 = EDGE_CURVE ( 'NONE', #68160, #43082, #19414, .T. ) ;
#42086 = ORIENTED_EDGE ( 'NONE', *, *, #2953, .F. ) ;
#42085 = CARTESIAN_POINT ( 'NONE',  ( 41.66904755831212981, 15.55634918610394379, 85.00100000000000477 ) ) ;
#42087 = FACE_OUTER_BOUND ( 'NONE', #33027, .T. ) ;
#42088 = EDGE_CURVE ( 'NONE', #53754, #50282, #25183, .T. ) ;
#42089 = CARTESIAN_POINT ( 'NONE',  ( -1.666933348991701536, -64.97862212458817055, 170.0000000000000000 ) ) ;
#42090 = VECTOR ( 'NONE', #28563, 1000.000000000000000 ) ;
#42091 = ORIENTED_EDGE ( 'NONE', *, *, #52263, .F. ) ;
#42092 = FACE_OUTER_BOUND ( 'NONE', #27097, .T. ) ;
#42093 = VECTOR ( 'NONE', #61799, 1000.000000000000000 ) ;
#42094 = CARTESIAN_POINT ( 'NONE',  ( 134.3135005523732559, 42.87884033955815966, 29.52074435543002906 ) ) ;
#42095 = B_SPLINE_CURVE_WITH_KNOTS ( 'NONE', 3,
 ( #39770, #44703, #2489, #23943, #19009, #46081, #29559, #39420 ),
 .UNSPECIFIED., .F., .F.,
 ( 4, 2, 2, 4 ),
 ( 0.004673709593152140102, 0.005837709341827639065, 0.007001709090503138895, 0.009329708587854137689 ),
 .UNSPECIFIED. ) ;
#42096 = CARTESIAN_POINT ( 'NONE',  ( 56.55557087522677762, 11.26645937438482115, -93.07732634674349015 ) ) ;
#42097 = AXIS2_PLACEMENT_3D ( 'NONE', #51187, #9656, #29723 ) ;
#42098 = CARTESIAN_POINT ( 'NONE',  ( -39.87466933223296905, 12.30143995236625365, 13.79046340968177553 ) ) ;
#42099 = CARTESIAN_POINT ( 'NONE',  ( -102.2801239173131052, 32.78103895658057354, -61.85912785543958847 ) ) ;
#42100 = ORIENTED_EDGE ( 'NONE', *, *, #7432, .T. ) ;
#42101 = VERTEX_POINT ( 'NONE', #61639 ) ;
#42102 = CARTESIAN_POINT ( 'NONE',  ( 183.1910712700538681, 80.76073941711163684, -63.35883323969136427 ) ) ;
#42103 = CARTESIAN_POINT ( 'NONE',  ( -165.9992860119575084, 79.53569239468049545, -44.58101777890279038 ) ) ;
#42105 = EDGE_CURVE ( 'NONE', #7559, #295, #46486, .T. ) ;
#42104 = CARTESIAN_POINT ( 'NONE',  ( 0.000000000000000000, 0.000000000000000000, 0.000000000000000000 ) ) ;
#42106 = EDGE_CURVE ( 'NONE', #30275, #64382, #34915, .T. ) ;
#42107 = CARTESIAN_POINT ( 'NONE',  ( 103.8325688302027459, 27.12251147381402561, -74.16827293220038086 ) ) ;
#42108 = CARTESIAN_POINT ( 'NONE',  ( -75.00452312211128003, 22.03104735285380755, 31.36846399027299626 ) ) ;
#42109 = CARTESIAN_POINT ( 'NONE',  ( 86.62931800182292363, 19.42108912189597092, 44.71208757247933363 ) ) ;
#42110 = EDGE_CURVE ( 'NONE', #45314, #19626, #34833, .T. ) ;
#42111 = CARTESIAN_POINT ( 'NONE',  ( -142.9730935922299295, 58.82921737386681116, 41.91139747252092462 ) ) ;
#42112 = CARTESIAN_POINT ( 'NONE',  ( -28.32746765835429414, -69.45586423092650818, 43.58025477438756923 ) ) ;
#42113 = CARTESIAN_POINT ( 'NONE',  ( 212.1707951106656651, 117.1901534358505899, 64.21020998533151669 ) ) ;
#42114 = VERTEX_POINT ( 'NONE', #10575 ) ;
#42115 = CARTESIAN_POINT ( 'NONE',  ( -105.4589068214114462, 34.42476264325677704, -22.47934715272176476 ) ) ;
#42116 = ORIENTED_EDGE ( 'NONE', *, *, #52093, .F. ) ;
#42117 = CARTESIAN_POINT ( 'NONE',  ( -38.15923928782689245, 10.79140400702259228, 14.21113170898300915 ) ) ;
#42118 = CARTESIAN_POINT ( 'NONE',  ( 79.33384730094456927, 18.11203072455034047, 62.29897845281649182 ) ) ;
#42119 = DIRECTION ( 'NONE',  ( 1.000000000000000000, 0.000000000000000000, 0.000000000000000000 ) ) ;
#42120 = CARTESIAN_POINT ( 'NONE',  ( 86.62931800182293784, 19.42108912189599934, 17.86753698201564688 ) ) ;
#42121 = PLANE ( 'NONE',  #35515 ) ;
#42122 = FILL_AREA_STYLE ('',( #56931 ) ) ;
#42123 = CARTESIAN_POINT ( 'NONE',  ( 39.40195752203892710, 8.409560354027393103, -62.46436805589144114 ) ) ;
#42124 = DIRECTION ( 'NONE',  ( -0.000000000000000000, -0.000000000000000000, 1.000000000000000000 ) ) ;
#42125 = CARTESIAN_POINT ( 'NONE',  ( -38.93847286785603501, 11.96870349976818027, -16.47936910502927077 ) ) ;
#42126 = ORIENTED_EDGE ( 'NONE', *, *, #53887, .T. ) ;
#42127 = CARTESIAN_POINT ( 'NONE',  ( -65.36598343705435354, 0.000000000000000000, 41.38025477438755928 ) ) ;
#42128 = ORIENTED_EDGE ( 'NONE', *, *, #6664, .F. ) ;
#42129 = CARTESIAN_POINT ( 'NONE',  ( 0.000000000000000000, 0.000000000000000000, 41.38025477438755928 ) ) ;
#42130 = CARTESIAN_POINT ( 'NONE',  ( 9.275903038161093406, 7.385619229189523516, -66.11132412825449478 ) ) ;
#42131 = CARTESIAN_POINT ( 'NONE',  ( -24.19091603582231542, 8.513464105188681685, 12.81483973167518187 ) ) ;
#42132 = LINE ( 'NONE', #31248, #28895 ) ;
#42133 = CARTESIAN_POINT ( 'NONE',  ( -13.47230132170245653, 7.324574289401438065, -64.80259611343139170 ) ) ;
#42134 = FACE_BOUND ( 'NONE', #45311, .T. ) ;
#42135 = CARTESIAN_POINT ( 'NONE',  ( 154.4617654203035784, 56.60942201271841867, -50.50876627099340510 ) ) ;
#42136 = AXIS2_PLACEMENT_3D ( 'NONE', #44076, #33560, #15971 ) ;
#42137 = ORIENTED_EDGE ( 'NONE', *, *, #57402, .T. ) ;
#42138 = AXIS2_PLACEMENT_3D ( 'NONE', #68984, #36992, #36653 ) ;
#42139 = CARTESIAN_POINT ( 'NONE',  ( 403.0071894358296731, 992.0915846175136039, 794.0068267248735765 ) ) ;
#42140 = CARTESIAN_POINT ( 'NONE',  ( -150.3850953947693085, 66.25368649589884740, 72.52681933769164857 ) ) ;
#42141 = DIRECTION ( 'NONE',  ( -0.000000000000000000, -0.000000000000000000, 1.000000000000000000 ) ) ;
#42142 = CARTESIAN_POINT ( 'NONE',  ( -109.7156874346698174, 37.87149323084330632, 65.87937654599812731 ) ) ;
#42143 = CARTESIAN_POINT ( 'NONE',  ( -20.00000000000002842, -6.319444444444441089, 4.000000000000000000 ) ) ;
#42144 = ORIENTED_EDGE ( 'NONE', *, *, #47643, .T. ) ;
#42146 = DIRECTION ( 'NONE',  ( -0.000000000000000000, -0.000000000000000000, 1.000000000000000000 ) ) ;
#42145 = CIRCLE ( 'NONE', #34325, 25.12245591505646303 ) ;
#42147 = CIRCLE ( 'NONE', #11801, 5.000000000000004441 ) ;
#42148 = CARTESIAN_POINT ( 'NONE',  ( -4.513903087372272083, 6.697902023160598795, -22.80731739600529906 ) ) ;
#42149 = CARTESIAN_POINT ( 'NONE',  ( 197.3064269725218765, 98.33232022113057269, -15.66748082040111534 ) ) ;
#42150 = AXIS2_PLACEMENT_3D ( 'NONE', #33872, #60945, #11354 ) ;
#42151 = CARTESIAN_POINT ( 'NONE',  ( -143.2562389366337925, 59.05327470469417506, 87.75316541060529119 ) ) ;
#42152 = EDGE_CURVE ( 'NONE', #24493, #35316, #63370, .T. ) ;
#42153 = CONICAL_SURFACE ( 'NONE', #43277, 65.00000000000000000, 0.7853981633974497223 ) ;
#42154 = CARTESIAN_POINT ( 'NONE',  ( 141.2366329129480675, 46.06278879703613427, 35.64775270001474183 ) ) ;
#42155 = VERTEX_POINT ( 'NONE', #59107 ) ;
#42156 = CARTESIAN_POINT ( 'NONE',  ( 198.7084915431530021, 98.47675983942193056, 32.18548563730031020 ) ) ;
#42157 = CARTESIAN_POINT ( 'NONE',  ( 83.38619203015946368, 19.39783821526631513, 3.588035180901903765 ) ) ;
#42158 = CARTESIAN_POINT ( 'NONE',  ( 183.1873354889582117, 82.20882912211247628, 29.59664944175426271 ) ) ;
#42159 = CARTESIAN_POINT ( 'NONE',  ( 163.7379901688713062, 64.00402364591248272, 14.19210081108414201 ) ) ;
#42160 = DIRECTION ( 'NONE',  ( 2.312964634635743450E-16, -0.000000000000000000, 1.000000000000000000 ) ) ;
#42161 = ORIENTED_EDGE ( 'NONE', *, *, #58762, .F. ) ;
#42162 = EDGE_CURVE ( 'NONE', #50858, #2381, #28980, .T. ) ;
#42163 = CARTESIAN_POINT ( 'NONE',  ( 174.1422537179814469, 73.24254491731254291, 60.79958808295376116 ) ) ;
#42164 = VERTEX_POINT ( 'NONE', #44684 ) ;
#42165 = CARTESIAN_POINT ( 'NONE',  ( -102.7456062648101778, 33.01749955571778372, -50.01457726497594791 ) ) ;
#42166 = CARTESIAN_POINT ( 'NONE',  ( -7.329206686002009974E-14, -46.66904755831211560, 2.000000000000001776 ) ) ;
#42167 = EDGE_CURVE ( 'NONE', #27278, #4891, #55576, .T. ) ;
#42168 = CARTESIAN_POINT ( 'NONE',  ( -61.52143283897135717, 16.51181063611435818, 34.01359757082287416 ) ) ;
#42169 = ADVANCED_FACE ( 'NONE', ( #33444 ), #17601, .T. ) ;
#42171 = ORIENTED_EDGE ( 'NONE', *, *, #12155, .F. ) ;
#42170 = CARTESIAN_POINT ( 'NONE',  ( 154.4617654203035499, 56.60942201271836893, 3.180334909933947074 ) ) ;
#42172 = CARTESIAN_POINT ( 'NONE',  ( 157.9121974517528315, 59.27335488206246339, -51.12418429913765294 ) ) ;
#42173 = DIRECTION ( 'NONE',  ( -0.000000000000000000, -0.000000000000000000, 1.000000000000000000 ) ) ;
#42174 = CARTESIAN_POINT ( 'NONE',  ( 41.72486082342823011, -50.31647622756197080, 41.38025477438755928 ) ) ;
#42175 = ORIENTED_EDGE ( 'NONE', *, *, #54938, .T. ) ;
#42176 = DIRECTION ( 'NONE',  ( 0.000000000000000000, 0.000000000000000000, -1.000000000000000000 ) ) ;
#42177 = CARTESIAN_POINT ( 'NONE',  ( -439.4229916354182706, 388.0000000000064233, 91.05029585798840230 ) ) ;
#42178 = AXIS2_PLACEMENT_3D ( 'NONE', #27284, #38906, #22365 ) ;
#42179 = CARTESIAN_POINT ( 'NONE',  ( 135.6842057900327347, 42.53841116629839547, 71.14344607389850239 ) ) ;
#42180 = CARTESIAN_POINT ( 'NONE',  ( -172.3018509397888067, 86.22053936367352378, 45.78839510999039675 ) ) ;
#42181 = CARTESIAN_POINT ( 'NONE',  ( 152.1190604254710195, 53.60705199010334354, 58.49325996993837151 ) ) ;
#42182 = DIRECTION ( 'NONE',  ( -0.000000000000000000, 1.000000000000000000, -0.000000000000000000 ) ) ;
#42183 = VERTEX_POINT ( 'NONE', #43620 ) ;
#42184 = CARTESIAN_POINT ( 'NONE',  ( 46.65974587859241041, 10.48396258569370509, 8.615397572259070103 ) ) ;
#42185 = ORIENTED_EDGE ( 'NONE', *, *, #9396, .T. ) ;
#42186 = CIRCLE ( 'NONE', #18595, 5.000000000000000888 ) ;
#42188 = EDGE_CURVE ( 'NONE', #68800, #40688, #23241, .T. ) ;
#42187 = CARTESIAN_POINT ( 'NONE',  ( 150.5744176759382924, 53.72473166688033785, -19.74036240759600958 ) ) ;
#42189 = CARTESIAN_POINT ( 'NONE',  ( -53.82256742816888817, 14.35433967245538511, 84.08070474350741108 ) ) ;
#42190 = VECTOR ( 'NONE', #48240, 1000.000000000000000 ) ;
#42191 = CIRCLE ( 'NONE', #17485, 65.00000000000000000 ) ;
#42192 = CARTESIAN_POINT ( 'NONE',  ( 31.11269837220812562, 31.11269837220800483, 0.000000000000000000 ) ) ;
#42193 = CARTESIAN_POINT ( 'NONE',  ( -153.5002794404625490, 67.64160439471093866, -75.51027764244948060 ) ) ;
#42194 = LINE ( 'NONE', #4559, #9 ) ;
#42195 = AXIS2_PLACEMENT_3D ( 'NONE', #25289, #68532, #53023 ) ;
#42196 = EDGE_CURVE ( 'NONE', #56134, #5466, #367, .T. ) ;
#42197 = CARTESIAN_POINT ( 'NONE',  ( 188.5842358232186200, 88.03712271786933741, 9.664620389188403493 ) ) ;
#42198 = DIRECTION ( 'NONE',  ( -3.081487911019579554E-32, -1.000000000000000000, -3.469446951953612956E-17 ) ) ;
#42199 = VECTOR ( 'NONE', #44146, 1000.000000000000000 ) ;
#42200 = LINE ( 'NONE', #54099, #39996 ) ;
#42201 = ORIENTED_EDGE ( 'NONE', *, *, #65296, .F. ) ;
#42203 = VECTOR ( 'NONE', #47888, 1000.000000000000000 ) ;
#42202 = CARTESIAN_POINT ( 'NONE',  ( 447.3372781065085633, 399.9999999999998863, 113.5502958579881891 ) ) ;
#42204 = ORIENTED_EDGE ( 'NONE', *, *, #47643, .F. ) ;
#42205 = CARTESIAN_POINT ( 'NONE',  ( -71.22896441287284119, 20.69091426169410397, 63.76365484910760983 ) ) ;
#42206 = CARTESIAN_POINT ( 'NONE',  ( -95.19652294162978023, 29.32558722310179178, -39.99725502653443954 ) ) ;
#42207 = CARTESIAN_POINT ( 'NONE',  ( 59.95259601283822093, 11.98300577492410923, -76.91558238451790430 ) ) ;
#42208 = SURFACE_STYLE_FILL_AREA ( #47128 ) ;
#42209 = CARTESIAN_POINT ( 'NONE',  ( 31.11269837220812562, 31.11269837220800483, 85.00100000000000477 ) ) ;
#42210 = DIRECTION ( 'NONE',  ( -0.8160245890732938934, -0.5780171883497599028, 0.000000000000000000 ) ) ;
#42211 = LINE ( 'NONE', #37610, #32161 ) ;
#42212 = EDGE_LOOP ( 'NONE', ( #26423, #52537, #65049, #60147 ) ) ;
#42213 = DIRECTION ( 'NONE',  ( 0.000000000000000000, 1.000000000000000000, 0.000000000000000000 ) ) ;
#42214 = PLANE ( 'NONE',  #17236 ) ;
#42215 = EDGE_LOOP ( 'NONE', ( #63762, #63590, #7942, #50678 ) ) ;
#42216 = ORIENTED_EDGE ( 'NONE', *, *, #62641, .F. ) ;
#42217 = CARTESIAN_POINT ( 'NONE',  ( -156.0171627975467743, 69.90368824761763733, 41.95465397809884678 ) ) ;
#42218 = CARTESIAN_POINT ( 'NONE',  ( 56.53776994993147298, 11.26292242501182805, -39.43272109873624487 ) ) ;
#42219 = CARTESIAN_POINT ( 'NONE',  ( -783.0172411895269988, -622.0000000000060254, 0.000000000000000000 ) ) ;
#42220 = DIRECTION ( 'NONE',  ( 0.000000000000000000, 1.000000000000000000, 0.000000000000000000 ) ) ;
#42221 = CARTESIAN_POINT ( 'NONE',  ( -65.00200000000002376, -1.250000000000021094, 170.0000000000000000 ) ) ;
#42222 = ORIENTED_EDGE ( 'NONE', *, *, #18655, .T. ) ;
#42223 = CARTESIAN_POINT ( 'NONE',  ( -132.0870433264402948, 51.94057326482882786, 42.35753507293710385 ) ) ;
#42224 = PRODUCT_RELATED_PRODUCT_CATEGORY ( 'part', '', ( #19738 ) ) ;
#42225 = ORIENTED_EDGE ( 'NONE', *, *, #18406, .F. ) ;
#42226 = DIRECTION ( 'NONE',  ( 1.000000000000000000, 0.000000000000000000, 0.000000000000000000 ) ) ;
#42227 = CARTESIAN_POINT ( 'NONE',  ( -142.5042386072304623, 59.74110826975219624, 35.48376318634494453 ) ) ;
#42228 = CARTESIAN_POINT ( 'NONE',  ( 209.5118425285948831, 113.1852661712287471, 42.46319131594169960 ) ) ;
#42229 = DIRECTION ( 'NONE',  ( -0.000000000000000000, 1.000000000000000000, -0.000000000000000000 ) ) ;
#42230 = PRODUCT_DEFINITION_SHAPE ( 'NONE', 'NONE',  #58568 ) ;
#42231 = EDGE_CURVE ( 'NONE', #28106, #4215, #28141, .T. ) ;
#42232 = FACE_OUTER_BOUND ( 'NONE', #33204, .T. ) ;
#42233 = CONICAL_SURFACE ( 'NONE', #65854, 74.95140232871122521, 0.8777644062502172329 ) ;
#42234 = EDGE_CURVE ( 'NONE', #58547, #18138, #54872, .T. ) ;
#42235 = ORIENTED_EDGE ( 'NONE', *, *, #38908, .F. ) ;
#42236 = VERTEX_POINT ( 'NONE', #33084 ) ;
#42237 = CARTESIAN_POINT ( 'NONE',  ( 110.0000000000000284, -21.42428528562853174, -5.000000000000004441 ) ) ;
#42238 = CARTESIAN_POINT ( 'NONE',  ( -120.8834178727915400, 44.46913122494650139, 86.21984674650981617 ) ) ;
#42239 = AXIS2_PLACEMENT_3D ( 'NONE', #42463, #57617, #9430 ) ;
#42240 = DIRECTION ( 'NONE',  ( -0.000000000000000000, 1.000000000000000000, -0.000000000000000000 ) ) ;
#42241 = DIRECTION ( 'NONE',  ( 0.7818314824680311359, -0.6234898018587319291, 0.000000000000000000 ) ) ;
#42242 = DIRECTION ( 'NONE',  ( -0.7071067811865487940, 0.000000000000000000, 0.7071067811865462405 ) ) ;
#42243 = CARTESIAN_POINT ( 'NONE',  ( 11.75170693505526032, 7.411272167608774275, 84.87420514505134861 ) ) ;
#42244 = AXIS2_PLACEMENT_3D ( 'NONE', #28294, #49387, #2277 ) ;
#42245 = AXIS2_PLACEMENT_3D ( 'NONE', #17686, #34576, #19065 ) ;
#42246 = ORIENTED_EDGE ( 'NONE', *, *, #53101, .T. ) ;
#42247 = AXIS2_PLACEMENT_3D ( 'NONE', #43852, #17117, #45952 ) ;
#42248 = DIRECTION ( 'NONE',  ( -0.04486483035051862939, 0.9989930665413143673, 0.000000000000000000 ) ) ;
#42249 = ADVANCED_FACE ( 'NONE', ( #17238 ), #65090, .F. ) ;
#42250 = AXIS2_PLACEMENT_3D ( 'NONE', #52474, #4299, #31032 ) ;
#42251 = CARTESIAN_POINT ( 'NONE',  ( -94.84390436305041305, 29.16104988397309938, 65.87395087744090461 ) ) ;
#42252 = ORIENTED_EDGE ( 'NONE', *, *, #128, .F. ) ;
#42253 = CARTESIAN_POINT ( 'NONE',  ( -85.10774223992955001, 24.88053943842881921, 7.223589135002512762 ) ) ;
#42254 = ORIENTED_EDGE ( 'NONE', *, *, #56996, .T. ) ;
#42255 = CIRCLE ( 'NONE', #11915, 65.00000000000000000 ) ;
#42256 = EDGE_CURVE ( 'NONE', #57574, #1313, #7167, .T. ) ;
#42257 = ORIENTED_EDGE ( 'NONE', *, *, #49791, .F. ) ;
#42258 = EDGE_CURVE ( 'NONE', #24352, #34130, #64210, .T. ) ;
#42259 = ORIENTED_EDGE ( 'NONE', *, *, #38377, .T. ) ;
#42260 = CARTESIAN_POINT ( 'NONE',  ( 10.83418588031599583, 6.392467435475928994, -48.67156742485343557 ) ) ;
#42261 = CARTESIAN_POINT ( 'NONE',  ( -55.05276343752910151, -170.0000000000000000, 72.16187836339486239 ) ) ;
#42262 = CARTESIAN_POINT ( 'NONE',  ( 8.000000000000007105, 249.8719672152120381, 94.99999999999866418 ) ) ;
#42263 = ORIENTED_EDGE ( 'NONE', *, *, #2529, .F. ) ;
#42264 = CARTESIAN_POINT ( 'NONE',  ( 8.390996311772823901, 10.00000000000000000, 0.000000000000000000 ) ) ;
#42265 = CARTESIAN_POINT ( 'NONE',  ( 154.0401952541422474, 55.03227529428313147, 43.58305379128945134 ) ) ;
#42266 = CARTESIAN_POINT ( 'NONE',  ( 103.5839822277949764, 25.92130892112108498, -39.96249046856183895 ) ) ;
#42267 = CARTESIAN_POINT ( 'NONE',  ( 139.2794027252093940, 45.99190465195506050, -65.16434641514403836 ) ) ;
#42268 = DIRECTION ( 'NONE',  ( 0.000000000000000000, 0.000000000000000000, -1.000000000000000000 ) ) ;
#42269 = ORIENTED_EDGE ( 'NONE', *, *, #15732, .T. ) ;
#42270 = LINE ( 'NONE', #3951, #37605 ) ;
#42271 = CARTESIAN_POINT ( 'NONE',  ( -85.12122836439579032, 25.97531040437156946, -65.60879660851998096 ) ) ;
#42272 = CARTESIAN_POINT ( 'NONE',  ( -5.000000000000073719, -41.66904755831212270, 2.000000000000001776 ) ) ;
#42273 = CARTESIAN_POINT ( 'NONE',  ( -121.5928001448268958, 44.91559452735374691, -36.25159717105308488 ) ) ;
#42274 = CARTESIAN_POINT ( 'NONE',  ( -79.14638003838379632, 23.58242782405879012, 18.57365054920947856 ) ) ;
#42275 = PLANE ( 'NONE',  #14586 ) ;
#42276 = CARTESIAN_POINT ( 'NONE',  ( -155.5978531700837095, 69.52241200678679434, 15.76037129834827510 ) ) ;
#42277 = DIRECTION ( 'NONE',  ( 1.000000000000000000, 0.000000000000000000, -0.000000000000000000 ) ) ;
#42278 = CARTESIAN_POINT ( 'NONE',  ( 70.11438327604405174, 14.43198353181102256, 12.90143265241210280 ) ) ;
#42279 = CARTESIAN_POINT ( 'NONE',  ( 164.8886903222557407, 63.65672212134880681, 8.925453984754252446 ) ) ;
#42280 = CARTESIAN_POINT ( 'NONE',  ( 209.3223706822284100, 0.000000000000000000, 31.44247402469554942 ) ) ;
#42281 = VERTEX_POINT ( 'NONE', #24970 ) ;
#42282 = VECTOR ( 'NONE', #52653, 1000.000000000000000 ) ;
#42283 = ITEM_DEFINED_TRANSFORMATION ( 'NONE', 'NONE', #36581,  #66832 ) ;
#42284 = DIRECTION ( 'NONE',  ( -0.8160245890732938934, -0.5780171883497599028, 0.000000000000000000 ) ) ;
#42285 = ORIENTED_EDGE ( 'NONE', *, *, #1603, .T. ) ;
#42286 = PLANE ( 'NONE',  #40781 ) ;
#42287 = ORIENTED_EDGE ( 'NONE', *, *, #69237, .T. ) ;
#42288 = CARTESIAN_POINT ( 'NONE',  ( 23.28809538736928886, 7.864824219997537114, -69.37130277028362002 ) ) ;
#42289 = VECTOR ( 'NONE', #32695, 1000.000000000000000 ) ;
#42290 = DIRECTION ( 'NONE',  ( -0.000000000000000000, -0.000000000000000000, -1.000000000000000000 ) ) ;
#42291 = DIRECTION ( 'NONE',  ( -0.000000000000000000, -0.000000000000000000, 1.000000000000000000 ) ) ;
#42292 = PLANE ( 'NONE',  #52430 ) ;
#42293 = CARTESIAN_POINT ( 'NONE',  ( 137.5911612413395630, 44.91497189902067078, -37.01495899583318305 ) ) ;
#42294 = AXIS2_PLACEMENT_3D ( 'NONE', #45958, #36794, #19217 ) ;
#42295 = CARTESIAN_POINT ( 'NONE',  ( -31.11269837220804035, 20.55634918610408945, 2.000000000000001776 ) ) ;
#42296 = CARTESIAN_POINT ( 'NONE',  ( 152.1327777395850376, 53.61712543276775733, -38.34954180087900966 ) ) ;
#42297 = LINE ( 'NONE', #58696, #28839 ) ;
#42298 = DIRECTION ( 'NONE',  ( -1.850371928290090422E-16, 1.000000000000000000, 1.110223024625156171E-16 ) ) ;
#42299 = DIRECTION ( 'NONE',  ( 0.000000000000000000, 0.000000000000000000, 1.000000000000000000 ) ) ;
#42300 = ORIENTED_EDGE ( 'NONE', *, *, #46855, .F. ) ;
#42301 = ORIENTED_EDGE ( 'NONE', *, *, #19951, .F. ) ;
#42302 = CARTESIAN_POINT ( 'NONE',  ( 37.47470330837911945, 8.071072105428767074, 13.32819299319724138 ) ) ;
#42303 = AXIS2_PLACEMENT_3D ( 'NONE', #56310, #50689, #34180 ) ;
#42304 = DIRECTION ( 'NONE',  ( -0.2225209339563042066, -0.9749279121818259508, 0.000000000000000000 ) ) ;
#42305 = LINE ( 'NONE', #9953, #46501 ) ;
#42306 = DIRECTION ( 'NONE',  ( -0.7071067811865474617, 0.000000000000000000, 0.7071067811865474617 ) ) ;
#42307 = EDGE_CURVE ( 'NONE', #37010, #25774, #55775, .T. ) ;
#42308 = CARTESIAN_POINT ( 'NONE',  ( 87.58754341703159696, 20.81465688423119786, 17.82130253370978323 ) ) ;
#42309 = CARTESIAN_POINT ( 'NONE',  ( 0.000000000000000000, 0.000000000000000000, 0.000000000000000000 ) ) ;
#42310 = CARTESIAN_POINT ( 'NONE',  ( 173.9413349464226997, 71.67637800842362594, -72.87454113658040455 ) ) ;
#42311 = CARTESIAN_POINT ( 'NONE',  ( -20.55634918610411077, -46.66904755831208718, 0.000000000000000000 ) ) ;
#42312 = CARTESIAN_POINT ( 'NONE',  ( 53.32245423372562243, 37.19594572654712294, 41.38025477438755928 ) ) ;
#42313 = LINE ( 'NONE', #31753, #69036 ) ;
#42314 = CARTESIAN_POINT ( 'NONE',  ( 106.6972452105824800, 21.67615690170939757, -3.768214559138922226 ) ) ;
#42315 = CARTESIAN_POINT ( 'NONE',  ( 26.12852347772543737, 100.0000000000000000, 77.58025477438755502 ) ) ;
#42316 = ADVANCED_FACE ( 'NONE', ( #4878 ), #47099, .F. ) ;
#42317 = ADVANCED_FACE ( 'NONE', ( #26689, #48118, #14743 ), #41831, .T. ) ;
#42318 = VERTEX_POINT ( 'NONE', #37580 ) ;
#42319 = DIRECTION ( 'NONE',  ( 0.000000000000000000, -0.000000000000000000, -1.000000000000000000 ) ) ;
#42320 = CARTESIAN_POINT ( 'NONE',  ( 110.2429982417149432, 28.88204397445231564, -9.077886975189997543 ) ) ;
#42321 = EDGE_CURVE ( 'NONE', #28307, #61600, #50788, .T. ) ;
#42322 = CARTESIAN_POINT ( 'NONE',  ( 151.7783534118502189, 54.60545177578661225, 68.64412217554496465 ) ) ;
#42323 = CARTESIAN_POINT ( 'NONE',  ( 290.0000000000000568, -5.000000000000000888, 19.36491673103706290 ) ) ;
#42324 = LINE ( 'NONE', #59174, #4888 ) ;
#42325 = CARTESIAN_POINT ( 'NONE',  ( -2.773325569976919702, 7.621740129702524236, 85.75189649308317996 ) ) ;
#42326 = ORIENTED_EDGE ( 'NONE', *, *, #37236, .F. ) ;
#42327 = PLANE ( 'NONE',  #9718 ) ;
#42328 = CARTESIAN_POINT ( 'NONE',  ( 0.1306530452038101031, 7.903938623646867612, 2.309976723937613663 ) ) ;
#42329 = ORIENTED_EDGE ( 'NONE', *, *, #66197, .F. ) ;
#42330 = VECTOR ( 'NONE', #62638, 1000.000000000000000 ) ;
#42331 = ORIENTED_EDGE ( 'NONE', *, *, #3444, .T. ) ;
#42332 = CARTESIAN_POINT ( 'NONE',  ( 43.75276484590834514, 10.03191092760626724, 84.95856299007903090 ) ) ;
#42333 = CARTESIAN_POINT ( 'NONE',  ( 46.66904755831212981, 20.55634918610394379, 2.000000000000001776 ) ) ;
#42334 = CARTESIAN_POINT ( 'NONE',  ( 139.3536337508564031, 46.03986978183306888, -92.09433734929739046 ) ) ;
#42335 = EDGE_CURVE ( 'NONE', #49747, #61334, #66759, .T. ) ;
#42336 = ORIENTED_EDGE ( 'NONE', *, *, #42152, .T. ) ;
#42337 = VECTOR ( 'NONE', #55103, 1000.000000000000227 ) ;
#42338 = DIRECTION ( 'NONE',  ( -1.000000000000000000, 0.000000000000000000, 0.000000000000000000 ) ) ;
#42339 = DIRECTION ( 'NONE',  ( -0.000000000000000000, -0.000000000000000000, 1.000000000000000000 ) ) ;
#42340 = CARTESIAN_POINT ( 'NONE',  ( -0.3252226420479325530, 7.525368746738511305, 10.28429167359196583 ) ) ;
#42341 = CARTESIAN_POINT ( 'NONE',  ( 176.6238742729555327, 75.60943990211370647, -49.77349832926806528 ) ) ;
#42342 = VECTOR ( 'NONE', #23731, 1000.000000000000000 ) ;
#42343 = DIRECTION ( 'NONE',  ( 0.000000000000000000, 1.000000000000000000, 0.000000000000000000 ) ) ;
#42344 = FACE_OUTER_BOUND ( 'NONE', #62139, .T. ) ;
#42345 = AXIS2_PLACEMENT_3D ( 'NONE', #20066, #9510, #29928 ) ;
#42346 = ORIENTED_EDGE ( 'NONE', *, *, #36691, .T. ) ;
#42347 = CARTESIAN_POINT ( 'NONE',  ( 103.4725384926516938, 26.96797537091726582, -19.81430213386833472 ) ) ;
#42348 = CYLINDRICAL_SURFACE ( 'NONE', #29185, 7.500000000000013323 ) ;
#42349 = CARTESIAN_POINT ( 'NONE',  ( 13.36262230781615301, 7.441298897118795885, 44.62840908283959607 ) ) ;
#42350 = CARTESIAN_POINT ( 'NONE',  ( 199.9103251464698872, 101.6434290204574751, 42.48563161778374564 ) ) ;
#42351 = CARTESIAN_POINT ( 'NONE',  ( -84.79548387674154242, 25.84023516422310252, 87.27273205877571627 ) ) ;
#42353 = ORIENTED_EDGE ( 'NONE', *, *, #40421, .T. ) ;
#42352 = CARTESIAN_POINT ( 'NONE',  ( 19.21260300789856501, 55.08522701181888692, 27.58472315868180402 ) ) ;
#42354 = ORIENTED_EDGE ( 'NONE', *, *, #26141, .T. ) ;
#42355 = ORIENTED_EDGE ( 'NONE', *, *, #29712, .T. ) ;
#42356 = CARTESIAN_POINT ( 'NONE',  ( 113.4418023215250457, 31.50656691678299026, -77.06712383350409823 ) ) ;
#42357 = CARTESIAN_POINT ( 'NONE',  ( -439.4229916354182706, 400.0000000000065370, -123.9497041420119530 ) ) ;
#42358 = CARTESIAN_POINT ( 'NONE',  ( 198.7029050523552769, 98.46895521196213963, -66.13463292241958413 ) ) ;
#42359 = DIRECTION ( 'NONE',  ( -1.000000000000000000, 0.000000000000000000, 0.000000000000000000 ) ) ;
#42360 = CARTESIAN_POINT ( 'NONE',  ( -12.39770133248888939, 8.241491894828989473, -22.03905660758730889 ) ) ;
#42361 = CARTESIAN_POINT ( 'NONE',  ( 152.8558173410470147, 54.14978343559394602, -64.53641076882379934 ) ) ;
#42362 = DIRECTION ( 'NONE',  ( 0.000000000000000000, 0.000000000000000000, 1.000000000000000000 ) ) ;
#42363 = DIRECTION ( 'NONE',  ( 0.000000000000000000, 0.000000000000000000, 1.000000000000000000 ) ) ;
#42364 = ORIENTED_EDGE ( 'NONE', *, *, #876, .T. ) ;
#42365 = VERTEX_POINT ( 'NONE', #1691 ) ;
#42366 = CARTESIAN_POINT ( 'NONE',  ( 70.50376765786472788, 15.57629333413343353, -16.86642105671132086 ) ) ;
#42367 = CARTESIAN_POINT ( 'NONE',  ( -81.89510452344295288, 24.66033552777455995, -49.40161435469455853 ) ) ;
#42368 = CARTESIAN_POINT ( 'NONE',  ( 108.0836640549675991, 27.89549093408031766, 83.61057402085626222 ) ) ;
#42369 = CARTESIAN_POINT ( 'NONE',  ( -155.7455325080991031, 71.01834415181987481, 15.54818467395414316 ) ) ;
#42370 = EDGE_CURVE ( 'NONE', #32880, #36565, #21739, .T. ) ;
#42372 = CARTESIAN_POINT ( 'NONE',  ( 17.98081503251148661, 17.36923402935782690, 0.000000000000000000 ) ) ;
#42371 = AXIS2_PLACEMENT_3D ( 'NONE', #7812, #61271, #2531 ) ;
#42373 = CARTESIAN_POINT ( 'NONE',  ( 18.89356949897824123, 62.19351277735709260, 170.0000000000000000 ) ) ;
#42374 = CARTESIAN_POINT ( 'NONE',  ( -156.5979701648280695, 71.80257276515639830, 94.37845108976992492 ) ) ;
#42375 = ORIENTED_EDGE ( 'NONE', *, *, #68898, .F. ) ;
#42376 = EDGE_LOOP ( 'NONE', ( #53104, #11377, #24587, #13368 ) ) ;
#42377 = ORIENTED_EDGE ( 'NONE', *, *, #49625, .F. ) ;
#42378 = AXIS2_PLACEMENT_3D ( 'NONE', #1641, #20761, #63679 ) ;
#42379 = CARTESIAN_POINT ( 'NONE',  ( -149.5074843970971017, 65.50121172469319220, -22.96827994102830317 ) ) ;
#42380 = CARTESIAN_POINT ( 'NONE',  ( 63.01563776193091826, 12.67277567978498176, 56.65751152968497451 ) ) ;
#42381 = CARTESIAN_POINT ( 'NONE',  ( 104.3787150408505653, 26.26206731247476256, -92.41814093530493324 ) ) ;
#42382 = VECTOR ( 'NONE', #53789, 999.9999999999998863 ) ;
#42383 = LINE ( 'NONE', #32180, #59565 ) ;
#42384 = CARTESIAN_POINT ( 'NONE',  ( 200.8383807319520997, 102.8517715783673339, 57.10714352580840369 ) ) ;
#42385 = VERTEX_POINT ( 'NONE', #54081 ) ;
#42386 = CIRCLE ( 'NONE', #21058, 65.36598343705435354 ) ;
#42387 = CARTESIAN_POINT ( 'NONE',  ( 181.0840389613909736, 80.03940679743415387, 71.15314469597512925 ) ) ;
#42388 = CARTESIAN_POINT ( 'NONE',  ( 46.89128214611609735, 9.502158095527986958, 91.88262892997218501 ) ) ;
#42389 = VECTOR ( 'NONE', #6705, 1000.000000000000000 ) ;
#42390 = DIRECTION ( 'NONE',  ( -0.000000000000000000, 0.000000000000000000, -1.000000000000000000 ) ) ;
#42391 = CARTESIAN_POINT ( 'NONE',  ( 188.2988323915788271, 86.21831227955483712, 65.72281026858398434 ) ) ;
#42392 = DIRECTION ( 'NONE',  ( -1.000000000000000000, 0.000000000000000000, 0.000000000000000000 ) ) ;
#42393 = CARTESIAN_POINT ( 'NONE',  ( -85.90441187606238316, 25.21188850826090899, -40.58563879895491766 ) ) ;
#42394 = CARTESIAN_POINT ( 'NONE',  ( 21.42484406671928099, 6.746536496442160136, 59.40547109256082337 ) ) ;
#42395 = FACE_OUTER_BOUND ( 'NONE', #37462, .T. ) ;
#42396 = CARTESIAN_POINT ( 'NONE',  ( 8.683910719548894264, 7.383368463746304400, 8.253806082366962116 ) ) ;
#42397 = EDGE_CURVE ( 'NONE', #51247, #18030, #22957, .T. ) ;
#42398 = CIRCLE ( 'NONE', #68221, 20.00000000000001066 ) ;
#42399 = ORIENTED_EDGE ( 'NONE', *, *, #46938, .T. ) ;
#42400 = CARTESIAN_POINT ( 'NONE',  ( 186.2651679807462415, 84.00458780104318635, 4.520801913443380116 ) ) ;
#42401 = PRODUCT_CONTEXT ( 'NONE', #63726, 'mechanical' ) ;
#42402 = EDGE_CURVE ( 'NONE', #9126, #38828, #994, .T. ) ;
#42403 = DIRECTION ( 'NONE',  ( -1.000000000000000000, 0.000000000000000000, 0.000000000000000000 ) ) ;
#42404 = CARTESIAN_POINT ( 'NONE',  ( -156.9402586331177361, 72.11962769956262775, -95.00000000000133582 ) ) ;
#42405 = CARTESIAN_POINT ( 'NONE',  ( 2.694222958124177204E-15, 35.00000000000000000, 22.00000000000000355 ) ) ;
#42406 = CARTESIAN_POINT ( 'NONE',  ( 181.0840389613909736, 80.03940679743416808, -51.22505766587963905 ) ) ;
#42407 = ORIENTED_EDGE ( 'NONE', *, *, #3318, .T. ) ;
#42408 = VERTEX_POINT ( 'NONE', #65365 ) ;
#42409 = DIRECTION ( 'NONE',  ( 0.000000000000000000, 0.000000000000000000, 1.000000000000000000 ) ) ;
#42410 = CARTESIAN_POINT ( 'NONE',  ( 203.9203998321607116, 106.9845510704142413, 17.33319198133153805 ) ) ;
#42411 = ORIENTED_EDGE ( 'NONE', *, *, #4432, .F. ) ;
#42412 = DIRECTION ( 'NONE',  ( -0.000000000000000000, 1.000000000000000000, -0.000000000000000000 ) ) ;
#42413 = EDGE_CURVE ( 'NONE', #47971, #30365, #11885, .T. ) ;
#42414 = EDGE_LOOP ( 'NONE', ( #20277, #14562, #52682, #46406 ) ) ;
#42415 = CARTESIAN_POINT ( 'NONE',  ( -422.6627218934906978, 394.9999999999998295, 83.55029585798750702 ) ) ;
#42416 = DIRECTION ( 'NONE',  ( -0.8118923937861950435, -0.5838071093367415143, 0.000000000000000000 ) ) ;
#42417 = CARTESIAN_POINT ( 'NONE',  ( -440.1146514826276075, 394.9999999999998295, -133.9016337311479958 ) ) ;
#42418 = EDGE_CURVE ( 'NONE', #39568, #68560, #45401, .T. ) ;
#42419 = CARTESIAN_POINT ( 'NONE',  ( -96.76159256735192571, 30.06445763698411255, 43.12167622908535236 ) ) ;
#42420 = CARTESIAN_POINT ( 'NONE',  ( 93.85846834761630930, 22.01563781856521018, -45.33479466209353603 ) ) ;
#42422 = EDGE_LOOP ( 'NONE', ( #12249, #58786, #21896, #14851 ) ) ;
#42421 = CARTESIAN_POINT ( 'NONE',  ( -28.32746765835526048, 69.45586423092609607, 170.0000000000000000 ) ) ;
#42423 = VECTOR ( 'NONE', #67103, 1000.000000000000000 ) ;
#42424 = ORIENTED_EDGE ( 'NONE', *, *, #6338, .F. ) ;
#42425 = VERTEX_POINT ( 'NONE', #18219 ) ;
#42426 = CARTESIAN_POINT ( 'NONE',  ( -167.6524579626395166, 82.69702609844094354, 6.338703478976664307 ) ) ;
#42427 = DIRECTION ( 'NONE',  ( 1.282270072030906146E-16, -2.146158602472679632E-16, 1.000000000000000000 ) ) ;
#42428 = CARTESIAN_POINT ( 'NONE',  ( -179.0654441437004323, 93.99779465816534696, -19.94754107494070183 ) ) ;
#42429 = VECTOR ( 'NONE', #6590, 1000.000000000000000 ) ;
#42430 = CARTESIAN_POINT ( 'NONE',  ( 442.3372781065085633, 399.9999999999998863, 103.5502958579881891 ) ) ;
#42432 = ORIENTED_EDGE ( 'NONE', *, *, #30751, .F. ) ;
#42431 = CARTESIAN_POINT ( 'NONE',  ( -142.3178993725748853, 58.31327888234797285, -40.10431696157230874 ) ) ;
#42433 = CARTESIAN_POINT ( 'NONE',  ( -109.5517607553961739, 37.78054172120042153, 89.84167037464601435 ) ) ;
#42434 = AXIS2_PLACEMENT_3D ( 'NONE', #26167, #21235, #42682 ) ;
#42435 = ORIENTED_EDGE ( 'NONE', *, *, #47943, .F. ) ;
#42436 = CARTESIAN_POINT ( 'NONE',  ( -133.0808647576834005, 51.41195281028756625, 40.28004429727871383 ) ) ;
#42437 = CARTESIAN_POINT ( 'NONE',  ( 154.4165763529819628, -26.99999999999998224, 108.9999999999999858 ) ) ;
#42438 = DIRECTION ( 'NONE',  ( -0.000000000000000000, 0.000000000000000000, 1.000000000000000000 ) ) ;
#42439 = CARTESIAN_POINT ( 'NONE',  ( 64.52696037203355672, 10.43950074664854633, 43.58025477438756212 ) ) ;
#42440 = CARTESIAN_POINT ( 'NONE',  ( 0.000000000000000000, 0.000000000000000000, 41.38025477438755928 ) ) ;
#42441 = CARTESIAN_POINT ( 'NONE',  ( -101.8145602049406051, 32.54453702486151201, 18.67452391595144334 ) ) ;
#42442 = CARTESIAN_POINT ( 'NONE',  ( -94.89192151156326815, 29.18342430963125977, -70.67526850584850706 ) ) ;
#42443 = ORIENTED_EDGE ( 'NONE', *, *, #68814, .F. ) ;
#42444 = ORIENTED_EDGE ( 'NONE', *, *, #20573, .T. ) ;
#42445 = CARTESIAN_POINT ( 'NONE',  ( 185.5415406465189676, 83.23025870924408309, -76.61970377424405854 ) ) ;
#42446 = CARTESIAN_POINT ( 'NONE',  ( -169.8791831685529985, 83.59058982490282119, -35.43423335292201415 ) ) ;
#42447 = PLANE ( 'NONE',  #14925 ) ;
#42448 = CARTESIAN_POINT ( 'NONE',  ( 105.4376736768159191, 27.81988511842611800, -76.03054162972082963 ) ) ;
#42449 = CARTESIAN_POINT ( 'NONE',  ( -72.21889834709583056, 21.03534256744171316, 41.78139917607329323 ) ) ;
#42450 = EDGE_CURVE ( 'NONE', #56697, #6738, #50226, .T. ) ;
#42451 = CARTESIAN_POINT ( 'NONE',  ( 82.94943325692331371, 18.19803534719805782, 30.67239719205550941 ) ) ;
#42452 = DIRECTION ( 'NONE',  ( 1.387778780781445429E-16, -1.000000000000000000, -3.081487911019577365E-33 ) ) ;
#42453 = CARTESIAN_POINT ( 'NONE',  ( 41.09759788073308329, 9.651672055033845510, -35.80995810388947120 ) ) ;
#42454 = CARTESIAN_POINT ( 'NONE',  ( 207.4867844023104624, 110.2451255333963331, 70.52645239145388700 ) ) ;
#42455 = ORIENTED_EDGE ( 'NONE', *, *, #936, .T. ) ;
#42456 = DIRECTION ( 'NONE',  ( -1.000000000000000000, 0.000000000000000000, 0.000000000000000000 ) ) ;
#42457 = ORIENTED_EDGE ( 'NONE', *, *, #47179, .F. ) ;
#42458 = EDGE_CURVE ( 'NONE', #12369, #58185, #55491, .T. ) ;
#42459 = CARTESIAN_POINT ( 'NONE',  ( -37.07602570886410831, 10.58457435034603478, 5.899994561324445108 ) ) ;
#42460 = CARTESIAN_POINT ( 'NONE',  ( -48.12872802574267439, 43.70867239603707333, 170.0000000000000000 ) ) ;
#42461 = CARTESIAN_POINT ( 'NONE',  ( 89.65730223173024172, 21.54473673261223254, 57.19084295439972720 ) ) ;
#42462 = CARTESIAN_POINT ( 'NONE',  ( 133.8566784816069344, 42.60093787723652525, 29.51034083899533300 ) ) ;
#42463 = CARTESIAN_POINT ( 'NONE',  ( 412.3372781065085633, 219.4906275429376308, 111.5502958579881749 ) ) ;
#42464 = CARTESIAN_POINT ( 'NONE',  ( 33.75639351246965703, 7.742023566824297376, -74.92653034813449153 ) ) ;
#42465 = DIRECTION ( 'NONE',  ( -0.000000000000000000, -0.000000000000000000, 1.000000000000000000 ) ) ;
#42466 = CARTESIAN_POINT ( 'NONE',  ( -35.17296606710972640, 11.25626711331309515, -22.49574526638046024 ) ) ;
#42467 = ORIENTED_EDGE ( 'NONE', *, *, #62022, .F. ) ;
#42468 = FACE_OUTER_BOUND ( 'NONE', #14762, .T. ) ;
#42469 = VERTEX_POINT ( 'NONE', #50569 ) ;
#42470 = CARTESIAN_POINT ( 'NONE',  ( -7.825402957745087207, -170.0000000000000000, -42.91807073194382838 ) ) ;
#42471 = CARTESIAN_POINT ( 'NONE',  ( 12.04188192036245653, 7.416006018508749520, -76.36538918330802517 ) ) ;
#42472 = CARTESIAN_POINT ( 'NONE',  ( -190.6985136298601731, 109.1272424661242582, 7.126870892829554549 ) ) ;
#42473 = ADVANCED_FACE ( 'NONE', ( #35438 ), #67797, .F. ) ;
#42474 = CARTESIAN_POINT ( 'NONE',  ( 8.000000000000007105, 249.8719672152120381, -95.00000000000133582 ) ) ;
#42475 = CARTESIAN_POINT ( 'NONE',  ( -2.866724795119724778, 6.618578306599219196, 43.26370662482394636 ) ) ;
#42476 = CARTESIAN_POINT ( 'NONE',  ( -95.05546640093037070, 29.25972325950975517, -17.74977852771992204 ) ) ;
#42477 = EDGE_CURVE ( 'NONE', #42318, #32375, #24075, .T. ) ;
#42478 = VECTOR ( 'NONE', #44290, 1000.000000000000000 ) ;
#42479 = CARTESIAN_POINT ( 'NONE',  ( 157.0357419681844249, 58.58786672900117765, -51.11478325206026341 ) ) ;
#42480 = ADVANCED_FACE ( 'NONE', ( #28776 ), #23849, .T. ) ;
#42481 = AXIS2_PLACEMENT_3D ( 'NONE', #35500, #68208, #14041 ) ;
#42482 = ORIENTED_EDGE ( 'NONE', *, *, #58661, .T. ) ;
#42483 = DIRECTION ( 'NONE',  ( 4.052314039881818217E-15, -4.052314039881777196E-15, 1.000000000000000000 ) ) ;
#42484 = ADVANCED_FACE ( 'NONE', ( #67122 ), #2388, .F. ) ;
#42485 = CARTESIAN_POINT ( 'NONE',  ( 307.2575771313985342, 18.00000000000002842, 256.6193948016162381 ) ) ;
#42486 = CARTESIAN_POINT ( 'NONE',  ( 177.0027897064244939, 75.97676392242547649, -10.57201763481611856 ) ) ;
#42487 = EDGE_CURVE ( 'NONE', #60730, #20522, #24550, .T. ) ;
#42488 = CARTESIAN_POINT ( 'NONE',  ( -109.4995148930278361, 37.75156937139181679, 62.76486868760267157 ) ) ;
#42489 = VECTOR ( 'NONE', #2135, 1000.000000000000000 ) ;
#42490 = DIRECTION ( 'NONE',  ( -0.2225209339563184452, 0.9749279121818226201, 0.000000000000000000 ) ) ;
#42491 = ORIENTED_EDGE ( 'NONE', *, *, #63382, .F. ) ;
#42492 = CARTESIAN_POINT ( 'NONE',  ( -15.76129977463530274, 63.43731725181437042, 3.125053320693565680E-16 ) ) ;
#42493 = CARTESIAN_POINT ( 'NONE',  ( -4.955782654901483397, 6.720825733572408645, -23.01568829693101392 ) ) ;
#42494 = CARTESIAN_POINT ( 'NONE',  ( 197.3700262219431067, 98.41176242030789467, -15.35159226254784315 ) ) ;
#42495 = CARTESIAN_POINT ( 'NONE',  ( -142.3798905661107028, 58.36196886944601658, 89.55050332779295275 ) ) ;
#42496 = AXIS2_PLACEMENT_3D ( 'NONE', #29238, #33485, #44723 ) ;
#42497 = DIRECTION ( 'NONE',  ( 0.000000000000000000, 0.000000000000000000, -1.000000000000000000 ) ) ;
#42498 = EDGE_CURVE ( 'NONE', #20901, #60423, #58888, .T. ) ;
#42499 = ORIENTED_EDGE ( 'NONE', *, *, #31873, .T. ) ;
#42500 = CARTESIAN_POINT ( 'NONE',  ( 0.4969600502617513293, -4.995646404165285936, 7.347286611336975248 ) ) ;
#42501 = CARTESIAN_POINT ( 'NONE',  ( 79.39764314491569053, 18.13166883367087223, 8.363466887744241518 ) ) ;
#42502 = CARTESIAN_POINT ( 'NONE',  ( 163.7403496014744633, 64.00600007368875310, 5.941244934767215824 ) ) ;
#42503 = CARTESIAN_POINT ( 'NONE',  ( -98.68609963468200874, 32.11186931716880366, 44.61905611811087624 ) ) ;
#42504 = ADVANCED_FACE ( 'NONE', ( #40014 ), #61477, .F. ) ;
#42505 = EDGE_CURVE ( 'NONE', #5910, #66136, #30609, .T. ) ;
#42506 = EDGE_CURVE ( 'NONE', #45932, #49158, #4119, .T. ) ;
#42507 = VERTEX_POINT ( 'NONE', #35788 ) ;
#42508 =( GEOMETRIC_REPRESENTATION_CONTEXT ( 3 ) GLOBAL_UNCERTAINTY_ASSIGNED_CONTEXT ( ( #51489 ) ) GLOBAL_UNIT_ASSIGNED_CONTEXT ( ( #8038, #3122, #56221 ) ) REPRESENTATION_CONTEXT ( 'NONE', 'WORKASPACE' ) );
#42509 = CARTESIAN_POINT ( 'NONE',  ( -66.50000000000000000, 8.541911424052787628E-15, 17.57656211871651308 ) ) ;
#42510 = ORIENTED_EDGE ( 'NONE', *, *, #36279, .F. ) ;
#42511 = DIRECTION ( 'NONE',  ( 0.000000000000000000, 0.000000000000000000, 1.000000000000000000 ) ) ;
#42512 = CARTESIAN_POINT ( 'NONE',  ( 70.11766033381769603, 14.43277633974327046, -72.52602136616579287 ) ) ;
#42513 = DIRECTION ( 'NONE',  ( 2.220446049250313081E-16, 0.000000000000000000, 1.000000000000000000 ) ) ;
#42515 = ORIENTED_EDGE ( 'NONE', *, *, #22416, .T. ) ;
#42514 = CARTESIAN_POINT ( 'NONE',  ( 152.8373718734504791, 55.38925997611394081, 15.98291334453402079 ) ) ;
#42516 = CARTESIAN_POINT ( 'NONE',  ( -179.5082312244189495, 94.53075638132058600, 34.38164526738366789 ) ) ;
#42517 = CARTESIAN_POINT ( 'NONE',  ( 6.400000000000000355, 4.618802153517004960, 8.000000000000000000 ) ) ;
#42518 = CARTESIAN_POINT ( 'NONE',  ( -71.28077210551055032, -170.0000000000000000, -95.00000000000133582 ) ) ;
#42519 = ORIENTED_EDGE ( 'NONE', *, *, #39014, .T. ) ;
#42520 = DIRECTION ( 'NONE',  ( 0.7660444431189771253, 0.6427876096865404731, 1.661094098900087138E-16 ) ) ;
#42521 = CARTESIAN_POINT ( 'NONE',  ( 141.3445468829084746, 46.13338528906590597, 64.35867967590782257 ) ) ;
#42522 = CARTESIAN_POINT ( 'NONE',  ( -90.13282190615392153, -1.844136286507718230E-12, -5.000000000000000000 ) ) ;
#42523 = CARTESIAN_POINT ( 'NONE',  ( -32.41982179707238032, 9.753975577087194537, -77.11329407010529735 ) ) ;
#42524 = CARTESIAN_POINT ( 'NONE',  ( 93.87650740736113164, 23.09802612281734113, 35.21570653740766943 ) ) ;
#42525 = ORIENTED_EDGE ( 'NONE', *, *, #39384, .T. ) ;
#42526 = CIRCLE ( 'NONE', #17837, 65.00000000000000000 ) ;
#42527 = CARTESIAN_POINT ( 'NONE',  ( 45.04506994399700659, 10.22854084020123722, 5.604377804579494082 ) ) ;
#42528 = VERTEX_POINT ( 'NONE', #14664 ) ;
#42529 = ORIENTED_EDGE ( 'NONE', *, *, #9097, .T. ) ;
#42530 = CARTESIAN_POINT ( 'NONE',  ( -17.54261607806453327, -37.86253161628560093, 13.79046340968177908 ) ) ;
#42531 = AXIS2_PLACEMENT_3D ( 'NONE', #54449, #6278, #61494 ) ;
#42532 = CARTESIAN_POINT ( 'NONE',  ( 211.3710169359753763, 117.8057917113659556, -20.41562570395084109 ) ) ;
#42533 = DIRECTION ( 'NONE',  ( -1.000000000000000000, 1.232595164407830946E-32, 7.703719777548943412E-34 ) ) ;
#42534 = CARTESIAN_POINT ( 'NONE',  ( -156.0300823189602113, 69.91528270335479078, -72.89804073699036735 ) ) ;
#42535 = CARTESIAN_POINT ( 'NONE',  ( -109.1218018794893538, 36.39436146239677328, 88.61840892032539330 ) ) ;
#42536 = CARTESIAN_POINT ( 'NONE',  ( 186.2575601542430377, 85.47765906955507376, 15.39943919417170370 ) ) ;
#42537 = DIRECTION ( 'NONE',  ( 2.477416674922665047E-16, -3.355888904727913208E-17, 1.000000000000000000 ) ) ;
#42538 = FACE_BOUND ( 'NONE', #28623, .T. ) ;
#42539 = EDGE_LOOP ( 'NONE', ( #23839, #45837, #60138, #58764 ) ) ;
#42540 = EDGE_CURVE ( 'NONE', #4404, #68395, #48040, .T. ) ;
#42541 = CYLINDRICAL_SURFACE ( 'NONE', #44242, 65.00000000000000000 ) ;
#42542 = EDGE_LOOP ( 'NONE', ( #11884, #55325, #2550, #59002 ) ) ;
#42543 = CARTESIAN_POINT ( 'NONE',  ( -78.66644367742111399, 23.39876645725286863, 72.26275173013684139 ) ) ;
#42544 = CARTESIAN_POINT ( 'NONE',  ( 205.5105258529712557, 107.4632495673648265, -63.20359001240491637 ) ) ;
#42545 = CARTESIAN_POINT ( 'NONE',  ( 62.04664474957771603, 12.44961624115901877, -62.61246026202184112 ) ) ;
#42546 = DIRECTION ( 'NONE',  ( 0.000000000000000000, 0.000000000000000000, 1.000000000000000000 ) ) ;
#42547 = CARTESIAN_POINT ( 'NONE',  ( -36.80780718687457664, 10.53430034069837440, -91.25189668311308822 ) ) ;
#42548 = CARTESIAN_POINT ( 'NONE',  ( 22.72762730455395896, 7.830015919864530716, 40.39119682621441854 ) ) ;
#42549 = CARTESIAN_POINT ( 'NONE',  ( 197.8107221832102312, 97.35272301387820448, 87.39809707970657371 ) ) ;
#42550 = CARTESIAN_POINT ( 'NONE',  ( 157.4703587214989113, 58.92748579479259519, -62.96873488960130771 ) ) ;
#42551 = ORIENTED_EDGE ( 'NONE', *, *, #30192, .T. ) ;
#42552 = CARTESIAN_POINT ( 'NONE',  ( -71.56718866013697777, 19.74312628447963647, 67.23400750481188481 ) ) ;
#42553 = CARTESIAN_POINT ( 'NONE',  ( -15.55634918610403439, 5.000000000000028422, 85.00100000000000477 ) ) ;
#42554 = VERTEX_POINT ( 'NONE', #57237 ) ;
#42555 = ORIENTED_EDGE ( 'NONE', *, *, #6969, .F. ) ;
#42556 = ADVANCED_FACE ( 'NONE', ( #41059 ), #9052, .T. ) ;
#42557 = ADVANCED_FACE ( 'NONE', ( #42087 ), #10413, .F. ) ;
#42558 = CARTESIAN_POINT ( 'NONE',  ( -61.41100614348687969, 43.07262267896646790, 170.0000000000000000 ) ) ;
#42559 = DIRECTION ( 'NONE',  ( 0.000000000000000000, 0.000000000000000000, 1.000000000000000000 ) ) ;
#42560 = DIRECTION ( 'NONE',  ( 0.000000000000000000, 0.000000000000000000, 1.000000000000000000 ) ) ;
#42561 = EDGE_CURVE ( 'NONE', #5030, #15461, #15011, .T. ) ;
#42562 = CARTESIAN_POINT ( 'NONE',  ( -39.55079474733702227, 51.59997227570980982, 170.0000000000000000 ) ) ;
#42563 = LINE ( 'NONE', #31331, #58896 ) ;
#42564 = B_SPLINE_CURVE_WITH_KNOTS ( 'NONE', 3,
 ( #59223, #48653, #11380, #845, #22297, #44805 ),
 .UNSPECIFIED., .F., .F.,
 ( 4, 2, 4 ),
 ( 2.380731629583756093E-07, 0.002336973833157569413, 0.004673709593152181735 ),
 .UNSPECIFIED. ) ;
#42565 = EDGE_CURVE ( 'NONE', #56347, #22683, #68480, .T. ) ;
#42566 = ORIENTED_EDGE ( 'NONE', *, *, #12140, .F. ) ;
#42567 = ORIENTED_EDGE ( 'NONE', *, *, #44221, .F. ) ;
#42568 = CARTESIAN_POINT ( 'NONE',  ( -128.3448054685827913, 49.34430406923179646, 31.02807967144357804 ) ) ;
#42569 = EDGE_LOOP ( 'NONE', ( #52218, #47774 ) ) ;
#42570 = CARTESIAN_POINT ( 'NONE',  ( 111.9975424824652634, 296.0000000000000000, 529.9060149868646477 ) ) ;
#42571 = DIRECTION ( 'NONE',  ( 1.000000000000000000, 0.000000000000000000, 0.000000000000000000 ) ) ;
#42572 = CARTESIAN_POINT ( 'NONE',  ( 57.39674746172462960, 11.43903079040059190, 69.14934571406377017 ) ) ;
#42573 = LINE ( 'NONE', #31673, #56514 ) ;
#42574 = DIRECTION ( 'NONE',  ( -0.000000000000000000, -0.000000000000000000, -1.000000000000000000 ) ) ;
#42575 = PRESENTATION_STYLE_ASSIGNMENT (( #59773 ) ) ;
#42576 = ORIENTED_EDGE ( 'NONE', *, *, #1786, .F. ) ;
#42577 = AXIS2_PLACEMENT_3D ( 'NONE', #63203, #36465, #40442 ) ;
#42578 = ORIENTED_EDGE ( 'NONE', *, *, #3058, .F. ) ;
#42579 = DIRECTION ( 'NONE',  ( -0.9959742939952382912, -0.08963930890344087854, 0.000000000000000000 ) ) ;
#42580 = FACE_OUTER_BOUND ( 'NONE', #5571, .T. ) ;
#42581 = CARTESIAN_POINT ( 'NONE',  ( -165.6393662153604396, 79.16886183052815795, -14.76170845779348539 ) ) ;
#42582 = CARTESIAN_POINT ( 'NONE',  ( 136.1081004736419402, 42.80058051492065374, -77.52565627643819823 ) ) ;
#42583 = CARTESIAN_POINT ( 'NONE',  ( 66.72974708835177182, 13.56459745268607087, 30.77864159763544549 ) ) ;
#42584 = EDGE_CURVE ( 'NONE', #34225, #63173, #54116, .T. ) ;
#42585 = CARTESIAN_POINT ( 'NONE',  ( -189.5329886872043517, 107.4958891766011106, -71.08704754913541990 ) ) ;
#42586 = EDGE_CURVE ( 'NONE', #10801, #29739, #26942, .T. ) ;
#42587 = VECTOR ( 'NONE', #4940, 1000.000000000000000 ) ;
#42588 = EDGE_CURVE ( 'NONE', #65715, #48270, #11798, .T. ) ;
#42589 = ORIENTED_EDGE ( 'NONE', *, *, #42778, .T. ) ;
#42590 = EDGE_CURVE ( 'NONE', #48880, #39196, #33280, .T. ) ;
#42591 = CARTESIAN_POINT ( 'NONE',  ( 202.7506655727289058, 105.3943386412348673, -36.57149851176358624 ) ) ;
#42592 = ORIENTED_EDGE ( 'NONE', *, *, #9480, .F. ) ;
#42593 = CARTESIAN_POINT ( 'NONE',  ( -5.000000000000026645, -15.55634918610403616, 2.000000000000001776 ) ) ;
#42594 = ORIENTED_EDGE ( 'NONE', *, *, #55396, .F. ) ;
#42595 = ORIENTED_EDGE ( 'NONE', *, *, #1164, .T. ) ;
#42596 = CARTESIAN_POINT ( 'NONE',  ( -119.9771613955297198, 43.90337778233482879, 6.659436444873731098 ) ) ;
#42597 = CARTESIAN_POINT ( 'NONE',  ( -180.0175713311536470, 95.14770835574077523, 62.20439195989532521 ) ) ;
#42598 = CARTESIAN_POINT ( 'NONE',  ( 126.8015497489690091, 37.32461426945040728, 61.29668405129906716 ) ) ;
#42599 = VERTEX_POINT ( 'NONE', #48369 ) ;
#42600 = LINE ( 'NONE', #54879, #23384 ) ;
#42601 = CARTESIAN_POINT ( 'NONE',  ( 150.0501577908836168, 52.10460126680126791, 38.03534073332230747 ) ) ;
#42602 = CARTESIAN_POINT ( 'NONE',  ( 31.11269837220803325, -15.55634918610409656, 0.000000000000000000 ) ) ;
#42603 = LINE ( 'NONE', #53829, #15439 ) ;
#42604 = CARTESIAN_POINT ( 'NONE',  ( -51.66904755831210139, 6.635317295611287136E-14, 85.00100000000000477 ) ) ;
#42605 = CARTESIAN_POINT ( 'NONE',  ( -24.18258876560172865, 8.512344710720677554, 35.75813012041879091 ) ) ;
#42606 = FACE_OUTER_BOUND ( 'NONE', #18389, .T. ) ;
#42607 = EDGE_LOOP ( 'NONE', ( #46202, #9602, #20787, #40642 ) ) ;
#42608 = VECTOR ( 'NONE', #31214, 1000.000000000000000 ) ;
#42609 = FACE_BOUND ( 'NONE', #61488, .T. ) ;
#42610 = CARTESIAN_POINT ( 'NONE',  ( 31.89651141207536256, 56.63578868294628421, 170.0000000000000000 ) ) ;
#42611 = CARTESIAN_POINT ( 'NONE',  ( 429.8372781065087906, 400.0000000000067075, -128.9497041420121093 ) ) ;
#42612 = CARTESIAN_POINT ( 'NONE',  ( 0.4988340113715887814, 3.871605243926956152, 8.000000000000001776 ) ) ;
#42613 = CARTESIAN_POINT ( 'NONE',  ( -119.6801029354224823, 43.71909921132880328, -46.62127720739779591 ) ) ;
#42614 = CARTESIAN_POINT ( 'NONE',  ( -86.11230725916327344, 26.39026888680166749, 10.03994749107184070 ) ) ;
#42615 = CARTESIAN_POINT ( 'NONE',  ( -452.6627218934914936, 364.9999999999953957, 113.5502958579925945 ) ) ;
#42616 = DIRECTION ( 'NONE',  ( -0.000000000000000000, -0.000000000000000000, -1.000000000000000000 ) ) ;
#42617 = CARTESIAN_POINT ( 'NONE',  ( 197.7943621856794891, 98.94371996881450571, 93.35786775789816261 ) ) ;
#42618 = CARTESIAN_POINT ( 'NONE',  ( 65.41496713438827726, 13.24164235279043922, 17.59071151666574195 ) ) ;
#42619 = DIRECTION ( 'NONE',  ( -1.000000000000000000, 0.000000000000000000, 0.000000000000000000 ) ) ;
#42620 = CARTESIAN_POINT ( 'NONE',  ( 87.10672734544985474, 20.64813880796637235, -23.97701360844805762 ) ) ;
#42621 = ORIENTED_EDGE ( 'NONE', *, *, #4817, .T. ) ;
#42622 = EDGE_CURVE ( 'NONE', #5387, #59334, #33049, .T. ) ;
#42623 = ORIENTED_EDGE ( 'NONE', *, *, #69086, .T. ) ;
#42624 = DIRECTION ( 'NONE',  ( -1.000000000000000000, 0.000000000000000000, 0.000000000000000000 ) ) ;
#42625 = ORIENTED_EDGE ( 'NONE', *, *, #2236, .T. ) ;
#42626 = CIRCLE ( 'NONE', #15668, 65.00000000000000000 ) ;
#42627 = CARTESIAN_POINT ( 'NONE',  ( 22.28556289340100349, 7.803548444155008035, -73.61795775605594372 ) ) ;
#42628 = CARTESIAN_POINT ( 'NONE',  ( 412.0000000000000000, -2.000000000000000000, 378.0000000000000000 ) ) ;
#42629 = CARTESIAN_POINT ( 'NONE',  ( -143.8634661037140745, 60.82480701605700091, 60.09994342671955536 ) ) ;
#42630 = CARTESIAN_POINT ( 'NONE',  ( 69.50572373348801136, 14.27208627753790537, -12.58521233645258874 ) ) ;
#42632 = CARTESIAN_POINT ( 'NONE',  ( 139.6150621148398727, 46.20856238844175579, -38.69201805759518464 ) ) ;
#42631 = AXIS2_PLACEMENT_3D ( 'NONE', #57559, #19574, #41031 ) ;
#42633 = CARTESIAN_POINT ( 'NONE',  ( 211.3689821960821291, 117.8027529136708296, -94.07932131241392426 ) ) ;
#42634 = LINE ( 'NONE', #47551, #65609 ) ;
#42635 = CARTESIAN_POINT ( 'NONE',  ( -121.2119672714299838, 44.67540322905997385, -9.689954091359160415 ) ) ;
#42636 = ORIENTED_EDGE ( 'NONE', *, *, #56859, .F. ) ;
#42637 = ORIENTED_EDGE ( 'NONE', *, *, #4822, .T. ) ;
#42638 = EDGE_CURVE ( 'NONE', #61969, #45785, #44148, .T. ) ;
#42639 = CARTESIAN_POINT ( 'NONE',  ( 69.73342236697681074, 14.33173522011653134, -46.59197138149946937 ) ) ;
#42640 = DIRECTION ( 'NONE',  ( 0.000000000000000000, 0.000000000000000000, 1.000000000000000000 ) ) ;
#42641 = CARTESIAN_POINT ( 'NONE',  ( 13.24564585880038159, 63.65041531508843065, 0.000000000000000000 ) ) ;
#42642 = CARTESIAN_POINT ( 'NONE',  ( -9.291678301352703784, 76.94361032721405991, 73.58025477438756923 ) ) ;
#42643 = EDGE_CURVE ( 'NONE', #47508, #55364, #58944, .T. ) ;
#42644 = ADVANCED_FACE ( 'NONE', ( #43112 ), #64581, .T. ) ;
#42645 = AXIS2_PLACEMENT_3D ( 'NONE', #22188, #16900, #21483 ) ;
#42646 = CARTESIAN_POINT ( 'NONE',  ( 65.60421405224433045, 14.32371900106614149, -89.86771203546919651 ) ) ;
#42647 = ADVANCED_FACE ( 'NONE', ( #11107 ), #32570, .F. ) ;
#42648 = CARTESIAN_POINT ( 'NONE',  ( 284.7436796776308938, 21.94282408638629889, 1.613761426918498776 ) ) ;
#42649 = CARTESIAN_POINT ( 'NONE',  ( 188.2950976467626560, 87.71503060978557187, -14.79773892726507611 ) ) ;
#42650 = CARTESIAN_POINT ( 'NONE',  ( 208.5936709733499015, 113.6229123546138453, 3.440378187112652419 ) ) ;
#42651 = CARTESIAN_POINT ( 'NONE',  ( -85.53181628782058965, 26.14670395349505583, -93.27685199465567223 ) ) ;
#42652 = CARTESIAN_POINT ( 'NONE',  ( 44.35071890818840501, 9.104600422692255890, -10.61849397789796967 ) ) ;
#42653 = CARTESIAN_POINT ( 'NONE',  ( -31.43908319763709969, 10.61114334766715928, 57.06100499665286208 ) ) ;
#42654 = CARTESIAN_POINT ( 'NONE',  ( 105.1286806118793749, 21.97108935923501960, 1.139020068845009614 ) ) ;
#42655 = CARTESIAN_POINT ( 'NONE',  ( 161.1112535418156426, 61.83422628788728304, 70.31501105061632018 ) ) ;
#42656 =( REPRESENTATION_RELATIONSHIP ('NONE','NONE', #40274, #46431 ) REPRESENTATION_RELATIONSHIP_WITH_TRANSFORMATION ( #22070 )SHAPE_REPRESENTATION_RELATIONSHIP( ) );
#42657 = ORIENTED_EDGE ( 'NONE', *, *, #14558, .F. ) ;
#42658 = LINE ( 'NONE', #34729, #41388 ) ;
#42659 = CARTESIAN_POINT ( 'NONE',  ( 94.11733320392094981, 23.18939451097131865, -43.81524227077105138 ) ) ;
#42660 = CARTESIAN_POINT ( 'NONE',  ( -185.0000000000000000, 2.265596578422603396E-14, -2.500000000000002220 ) ) ;
#42661 = CARTESIAN_POINT ( 'NONE',  ( 230.9999999999999432, 0.000000000000000000, 0.000000000000000000 ) ) ;
#42662 = CARTESIAN_POINT ( 'NONE',  ( 150.5550643769628323, 52.46819381604269239, 7.149426911769203308 ) ) ;
#42663 = VECTOR ( 'NONE', #17532, 1000.000000000000000 ) ;
#42664 = CARTESIAN_POINT ( 'NONE',  ( -14.92342969503865469, 8.468308978091254602, 93.81261129068334981 ) ) ;
#42665 = ORIENTED_EDGE ( 'NONE', *, *, #41286, .F. ) ;
#42666 = EDGE_CURVE ( 'NONE', #43978, #7110, #64934, .T. ) ;
#42667 = LINE ( 'NONE', #47582, #12363 ) ;
#42668 = CARTESIAN_POINT ( 'NONE',  ( -62.53989795537026453, 16.81768094534200131, 65.16712804106848012 ) ) ;
#42669 = ORIENTED_EDGE ( 'NONE', *, *, #31073, .T. ) ;
#42670 = VERTEX_POINT ( 'NONE', #56112 ) ;
#42671 = CARTESIAN_POINT ( 'NONE',  ( 35.07875163271969399, 8.898953321987049137, 84.96543998221538629 ) ) ;
#42672 = CARTESIAN_POINT ( 'NONE',  ( 173.0237957311180708, 69.97204739562489806, -91.14091141288837150 ) ) ;
#42673 = CARTESIAN_POINT ( 'NONE',  ( 8.000000000000007105, 249.8719672152120381, -95.00000000000133582 ) ) ;
#42674 = ORIENTED_EDGE ( 'NONE', *, *, #14132, .T. ) ;
#42675 = DIRECTION ( 'NONE',  ( 1.000000000000000000, 0.000000000000000000, 0.000000000000000000 ) ) ;
#42676 = CARTESIAN_POINT ( 'NONE',  ( -0.7211439451572434489, 7.539282923622933730, 13.18759299316698552 ) ) ;
#42677 = CARTESIAN_POINT ( 'NONE',  ( 177.7886308167536242, 76.74396398590877766, -36.97273068449148781 ) ) ;
#42678 = VECTOR ( 'NONE', #66926, 1000.000000000000000 ) ;
#42679 = CARTESIAN_POINT ( 'NONE',  ( 10.55634918610409656, 31.11269837220803325, 0.000000000000000000 ) ) ;
#42680 = CARTESIAN_POINT ( 'NONE',  ( 89.21005684773504640, 20.31770592753387206, 30.16603058232306367 ) ) ;
#42681 = ORIENTED_EDGE ( 'NONE', *, *, #12, .T. ) ;
#42682 = DIRECTION ( 'NONE',  ( -1.000000000000000000, 0.000000000000000000, 0.000000000000000000 ) ) ;
#42683 = CARTESIAN_POINT ( 'NONE',  ( 46.66904755831207297, -15.55634918610412853, 0.000000000000000000 ) ) ;
#42684 = CARTESIAN_POINT ( 'NONE',  ( 10.31616749326173732, 7.393414706728907326, 32.37994498868797422 ) ) ;
#42685 = CARTESIAN_POINT ( 'NONE',  ( 199.7291770695760533, 101.4092159658447372, 42.33109527906247394 ) ) ;
#42686 = CARTESIAN_POINT ( 'NONE',  ( -86.17314828412035865, 26.41592763503389207, 91.53058199398142847 ) ) ;
#42688 = ORIENTED_EDGE ( 'NONE', *, *, #14696, .F. ) ;
#42687 = DIRECTION ( 'NONE',  ( 0.000000000000000000, 0.000000000000000000, 1.000000000000000000 ) ) ;
#42689 = VERTEX_POINT ( 'NONE', #13213 ) ;
#42690 = AXIS2_PLACEMENT_3D ( 'NONE', #62264, #36232, #35190 ) ;
#42692 = ORIENTED_EDGE ( 'NONE', *, *, #47258, .F. ) ;
#42691 = ADVANCED_FACE ( 'NONE', ( #18827 ), #34677, .T. ) ;
#42693 = CARTESIAN_POINT ( 'NONE',  ( 117.4806398654733783, 33.50379325299403632, -72.30120517819882764 ) ) ;
#42694 = PLANE ( 'NONE',  #55864 ) ;
#42695 = DIRECTION ( 'NONE',  ( 1.000000000000000000, 0.000000000000000000, 0.000000000000000000 ) ) ;
#42696 = CARTESIAN_POINT ( 'NONE',  ( -37.05762690088739930, 11.60527003175540806, 59.58680104041130221 ) ) ;
#42697 = EDGE_CURVE ( 'NONE', #47148, #22089, #47410, .T. ) ;
#42698 = CARTESIAN_POINT ( 'NONE',  ( -15.27594996066617661, 8.502079791899639361, -17.06292143071024725 ) ) ;
#42699 = DIRECTION ( 'NONE',  ( 0.000000000000000000, 1.000000000000000000, 0.000000000000000000 ) ) ;
#42700 = DIRECTION ( 'NONE',  ( 0.000000000000000000, 0.000000000000000000, 1.000000000000000000 ) ) ;
#42701 = EDGE_CURVE ( 'NONE', #35154, #38444, #56643, .T. ) ;
#42702 = LINE ( 'NONE', #64158, #11558 ) ;
#42703 = ORIENTED_EDGE ( 'NONE', *, *, #19360, .F. ) ;
#42704 = VERTEX_POINT ( 'NONE', #8280 ) ;
#42705 = CARTESIAN_POINT ( 'NONE',  ( 69.72789637502502558, 15.37065610545704075, -19.73133222002547171 ) ) ;
#42706 = EDGE_CURVE ( 'NONE', #14371, #35720, #48727, .T. ) ;
#42707 = LINE ( 'NONE', #20222, #1242 ) ;
#42708 = CARTESIAN_POINT ( 'NONE',  ( -24.54245881417235609, 9.575750052011494873, 94.42483238541157675 ) ) ;
#42709 = CARTESIAN_POINT ( 'NONE',  ( -150.3831389294225573, 66.25266777263976792, 3.924350373141658466 ) ) ;
#42710 = LINE ( 'NONE', #36758, #59548 ) ;
#42711 = LINE ( 'NONE', #16672, #68533 ) ;
#42712 = CARTESIAN_POINT ( 'NONE',  ( -439.4229916354183842, 394.9999999999998295, -128.9497041420121093 ) ) ;
#42713 = ORIENTED_EDGE ( 'NONE', *, *, #3964, .T. ) ;
#42714 = ORIENTED_EDGE ( 'NONE', *, *, #48872, .F. ) ;
#42715 = ORIENTED_EDGE ( 'NONE', *, *, #42477, .F. ) ;
#42716 = DIRECTION ( 'NONE',  ( 0.000000000000000000, -0.8660254037844380415, 0.5000000000000009992 ) ) ;
#42717 = CARTESIAN_POINT ( 'NONE',  ( 34.45158752686798209, 8.829194381142000836, -37.46439019260278513 ) ) ;
#42718 = EDGE_CURVE ( 'NONE', #27634, #59026, #65643, .T. ) ;
#42719 = ADVANCED_FACE ( 'NONE', ( #35707 ), #30418, .F. ) ;
#42720 = CARTESIAN_POINT ( 'NONE',  ( -38.87848244732138880, 10.93141945332449794, 63.57758875895522266 ) ) ;
#42721 = CARTESIAN_POINT ( 'NONE',  ( 199.7286177451875915, 101.4075663537892211, 57.91560235614644370 ) ) ;
#42722 = VECTOR ( 'NONE', #25909, 1000.000000000000000 ) ;
#42723 = VERTEX_POINT ( 'NONE', #57158 ) ;
#42724 = B_SPLINE_CURVE_WITH_KNOTS ( 'NONE', 3,
 ( #38071, #69394, #59866, #26832, #16270, #5709, #48260, #47924, #65160, #16614, #88, #49308, #21541, #21888, #21214, #65514, #33155, #43341, #59513, #42988, #54231, #64813, #11683, #42659, #16953, #64460, #54592, #6416, #53886, #27869, #1140, #22591, #44031, #17311, #38781, #19052, #18359, #44390, #61952, #29265, #60574, #56004, #60919, #28568, #61272 ),
 .UNSPECIFIED., .F., .F.,
 ( 4, 2, 2, 2, 2, 2, 2, 2, 2, 2, 2, 1, 2, 2, 2, 2, 2, 2, 2, 2, 2, 2, 4 ),
 ( 0.000000000000000000, 0.001510509505236005533, 0.002265764257853987700, 0.003021019010471969433, 0.004531528515707886930, 0.005286783268325868229, 0.006042038020943850396, 0.007552547526179788709, 0.009063057031415727022, 0.01057356653665166533, 0.01132882128926963536, 0.01208407604188760538, 0.01283933079450557367, 0.01359458554712354196, 0.01510509505235946466, 0.01586034980497742428, 0.01661560455759538563, 0.01812611406283129445, 0.01963662356806720327, 0.02039187832068514034, 0.02114713307330307393, 0.02265764257853898622, 0.02416815208377489851 ),
 .UNSPECIFIED. ) ;
#42725 = CARTESIAN_POINT ( 'NONE',  ( 175.0857681883884140, 72.74906374897946648, 94.99999999999866418 ) ) ;
#42726 = CARTESIAN_POINT ( 'NONE',  ( -156.9406434201983984, 70.74968524571474404, 66.21526506586671701 ) ) ;
#42727 = CARTESIAN_POINT ( 'NONE',  ( 19.11382977197791888, 7.636807742668408672, 17.41050504540015353 ) ) ;
#42728 = CARTESIAN_POINT ( 'NONE',  ( 182.7789203043890041, 80.33475476315294372, 70.97149666712105898 ) ) ;
#42729 = DIRECTION ( 'NONE',  ( -0.9195277725514489076, -0.3930250316539278810, 0.000000000000000000 ) ) ;
#42730 = CARTESIAN_POINT ( 'NONE',  ( -86.06489347855098515, 25.27905598459107139, -43.87173148075923734 ) ) ;
#42731 = CARTESIAN_POINT ( 'NONE',  ( 19.10216788411013411, 6.629360741291161929, 57.62663534263347032 ) ) ;
#42732 = DIRECTION ( 'NONE',  ( 0.000000000000000000, 0.000000000000000000, -1.000000000000000000 ) ) ;
#42733 = CARTESIAN_POINT ( 'NONE',  ( 8.540853903193189822, 6.376814430361480213, -67.91796824995262227 ) ) ;
#42734 = VERTEX_POINT ( 'NONE', #16211 ) ;
#42735 = CARTESIAN_POINT ( 'NONE',  ( 187.8959968237854241, 85.77553094678179946, 6.814269787780084187 ) ) ;
#42736 = CIRCLE ( 'NONE', #12429, 298.0000000000000000 ) ;
#42737 = CARTESIAN_POINT ( 'NONE',  ( 177.0075766083211875, 74.58167636505950782, 30.50888549528974281 ) ) ;
#42738 = CARTESIAN_POINT ( 'NONE',  ( -149.5074843970971301, -170.0000000000000000, 45.72082123989907387 ) ) ;
#42739 = CARTESIAN_POINT ( 'NONE',  ( 41.33692564073606235, 8.668977654195476390, -77.21459316755360192 ) ) ;
#42740 = LINE ( 'NONE', #27601, #7461 ) ;
#42741 = ORIENTED_EDGE ( 'NONE', *, *, #463, .T. ) ;
#42742 = ORIENTED_EDGE ( 'NONE', *, *, #60981, .T. ) ;
#42743 = CARTESIAN_POINT ( 'NONE',  ( -25.50312845906833914, 8.692070753302656883, -20.56343087316415819 ) ) ;
#42744 = CARTESIAN_POINT ( 'NONE',  ( 204.6977192012829789, 108.0580384837234931, 17.36317014830577321 ) ) ;
#42745 = EDGE_LOOP ( 'NONE', ( #20106, #15973 ) ) ;
#42746 = B_SPLINE_CURVE_WITH_KNOTS ( 'NONE', 3,
 ( #13237, #7951, #49096, #39613, #60007, #17092, #935, #22383, #1628, #33304, #22738, #38926, #23093, #44540, #66022, #12532, #55432, #7263, #50165, #61064, #13572, #36068, #13915, #14605, #61749, #14948, #30793, #24136, #3369, #46262, #36411, #67739, #29749, #56838, #57867, #29404, #4062, #57179, #51212, #68425, #63146, #3024, #57525, #62099 ),
 .UNSPECIFIED., .F., .F.,
 ( 4, 2, 2, 2, 2, 2, 2, 2, 2, 2, 2, 2, 2, 2, 2, 2, 2, 2, 2, 2, 2, 4 ),
 ( 0.02638217555535140105, 0.02805347641364870290, 0.02972477727194600128, 0.03139607813024330313, 0.03306737898854060498, 0.03390302941768924549, 0.03473867984683789295, 0.03640998070513518092, 0.03724563113428379368, 0.03808128156343241338, 0.03891693199258103308, 0.03975258242172964585, 0.04058823285087826555, 0.04142388328002688525, 0.04225953370917549801, 0.04309518413832411771, 0.04476648499662130853, 0.04643778585491847855, 0.04810908671321565550, 0.04978038757151283245, 0.05145168842981000246, 0.05312298928810717941 ),
 .UNSPECIFIED. ) ;
#42747 = ORIENTED_EDGE ( 'NONE', *, *, #28236, .T. ) ;
#42748 = CARTESIAN_POINT ( 'NONE',  ( 114.4640969196986191, 30.88424258798506372, 57.75175038263319038 ) ) ;
#42749 = VERTEX_POINT ( 'NONE', #46585 ) ;
#42750 = CARTESIAN_POINT ( 'NONE',  ( -11.75099048680784364, -77.43714764088365143, 133.5802547743875550 ) ) ;
#42751 = CARTESIAN_POINT ( 'NONE',  ( 140.5958192060901126, 46.84598876498520781, 60.55316104302657720 ) ) ;
#42752 = CARTESIAN_POINT ( 'NONE',  ( 15.55634918610411610, 51.66904755831205875, 0.000000000000000000 ) ) ;
#42753 = VECTOR ( 'NONE', #21354, 1000.000000000000000 ) ;
#42754 = CARTESIAN_POINT ( 'NONE',  ( 83.90793350743913948, 18.51008205890721214, -90.01042505155271556 ) ) ;
#42755 = DIRECTION ( 'NONE',  ( 0.000000000000000000, 0.000000000000000000, 1.000000000000000000 ) ) ;
#42756 = LINE ( 'NONE', #16029, #48845 ) ;
#42757 = VERTEX_POINT ( 'NONE', #36391 ) ;
#42758 = ORIENTED_EDGE ( 'NONE', *, *, #51653, .F. ) ;
#42759 = CARTESIAN_POINT ( 'NONE',  ( -169.1122507277983402, 84.24359299875008844, 5.123006575244060556 ) ) ;
#42760 = FACE_BOUND ( 'NONE', #42376, .T. ) ;
#42761 = CARTESIAN_POINT ( 'NONE',  ( -178.5790738944853331, 93.41591512785083751, -10.21774767167227616 ) ) ;
#42762 = CARTESIAN_POINT ( 'NONE',  ( -59.42430146430388049, -27.22983999535795618, 6.377659838150141321E-18 ) ) ;
#42764 = ORIENTED_EDGE ( 'NONE', *, *, #57099, .T. ) ;
#42763 = CARTESIAN_POINT ( 'NONE',  ( -142.3393481102175429, 58.33014244976926932, -44.53616841364604539 ) ) ;
#42765 = DIRECTION ( 'NONE',  ( -0.000000000000000000, 1.000000000000000000, -0.000000000000000000 ) ) ;
#42766 = EDGE_LOOP ( 'NONE', ( #16089, #30844, #38997, #12061 ) ) ;
#42767 = CARTESIAN_POINT ( 'NONE',  ( -31.11269837220809364, -15.55634918610397754, 0.000000000000000000 ) ) ;
#42768 = PLANE ( 'NONE',  #56973 ) ;
#42769 = EDGE_CURVE ( 'NONE', #52737, #26538, #14248, .T. ) ;
#42770 = CARTESIAN_POINT ( 'NONE',  ( 82.13067365723603075, 17.93447087949265395, -22.49758088646247600 ) ) ;
#42771 = CARTESIAN_POINT ( 'NONE',  ( 134.7708899521910837, 43.15864772107690328, 29.56272650432242699 ) ) ;
#42772 = CARTESIAN_POINT ( 'NONE',  ( 56.35108009888376301, 11.22498869437516866, -93.44476644971953760 ) ) ;
#42773 = EDGE_CURVE ( 'NONE', #45699, #68395, #40973, .T. ) ;
#42774 = CARTESIAN_POINT ( 'NONE',  ( -94.89192151156323973, 29.18342430963126688, 9.858383265542547846 ) ) ;
#42775 = CARTESIAN_POINT ( 'NONE',  ( -94.85061234775062644, 29.16417548023187578, -70.41713452772432902 ) ) ;
#42776 = ORIENTED_EDGE ( 'NONE', *, *, #27605, .T. ) ;
#42777 = VERTEX_POINT ( 'NONE', #26776 ) ;
#42778 = EDGE_CURVE ( 'NONE', #9035, #63750, #24802, .T. ) ;
#42779 = CYLINDRICAL_SURFACE ( 'NONE', #67532, 7.500000000000020428 ) ;
#42780 = CARTESIAN_POINT ( 'NONE',  ( 4.000000000000012434, 6.928203230275504332, 0.000000000000000000 ) ) ;
#42781 = CARTESIAN_POINT ( 'NONE',  ( -166.7068579965637127, 80.26142964949322334, -46.10773525000625739 ) ) ;
#42782 = CARTESIAN_POINT ( 'NONE',  ( 427.4999999999999432, 207.5000000000000284, 0.000000000000000000 ) ) ;
#42783 = CARTESIAN_POINT ( 'NONE',  ( -71.42007367207962432, 20.75704712149297748, 35.91863450065896046 ) ) ;
#42784 = CARTESIAN_POINT ( 'NONE',  ( 79.82127737190243977, 17.20935440217364487, 34.05564977191748000 ) ) ;
#42785 = CARTESIAN_POINT ( 'NONE',  ( 230.9999999999999432, 192.0000000000000000, 72.99999999999998579 ) ) ;
#42786 = CARTESIAN_POINT ( 'NONE',  ( -121.5680658099884113, 44.89994870382101055, 31.97482362736482031 ) ) ;
#42787 = CARTESIAN_POINT ( 'NONE',  ( 209.6877167158271220, 113.4449353909247691, 69.15631450432505289 ) ) ;
#42788 = ORIENTED_EDGE ( 'NONE', *, *, #36037, .F. ) ;
#42789 = CARTESIAN_POINT ( 'NONE',  ( -105.4556185321791588, 34.42302275449794990, -8.858947522874947467 ) ) ;
#42790 = ORIENTED_EDGE ( 'NONE', *, *, #50252, .F. ) ;
#42791 = VECTOR ( 'NONE', #60258, 1000.000000000000000 ) ;
#42792 = DIRECTION ( 'NONE',  ( -0.000000000000000000, 0.000000000000000000, -1.000000000000000000 ) ) ;
#42793 = CARTESIAN_POINT ( 'NONE',  ( -86.10037789697233279, 25.29391845275002737, 90.56095318331921362 ) ) ;
#42794 = CARTESIAN_POINT ( 'NONE',  ( 86.62931800182293784, 20.48449268398423229, 56.55663816294300261 ) ) ;
#42795 = ADVANCED_FACE ( 'NONE', ( #64398 ), #9307, .T. ) ;
#42796 = CARTESIAN_POINT ( 'NONE',  ( 156.5909039492009640, 56.96742803863246252, -9.279633708673955539 ) ) ;
#42797 = CARTESIAN_POINT ( 'NONE',  ( 32.15613847490628530, 8.588587416860168133, 8.617515965834311231 ) ) ;
#42798 = CARTESIAN_POINT ( 'NONE',  ( 32.67604596315971577, 7.629767358313821468, -73.29199647863042344 ) ) ;
#42799 = CARTESIAN_POINT ( 'NONE',  ( -97.88021438939452423, 31.71889184683102059, -63.26670929094522933 ) ) ;
#42800 = AXIS2_PLACEMENT_3D ( 'NONE', #16310, #49693, #54631 ) ;
#42801 = LINE ( 'NONE', #26975, #74 ) ;
#42802 = ORIENTED_EDGE ( 'NONE', *, *, #7801, .F. ) ;
#42803 = CARTESIAN_POINT ( 'NONE',  ( -39.55079474733624068, -51.59997227571039957, 41.38025477438755928 ) ) ;
#42804 = ORIENTED_EDGE ( 'NONE', *, *, #25098, .F. ) ;
#42805 = DIRECTION ( 'NONE',  ( 0.000000000000000000, 0.000000000000000000, 1.000000000000000000 ) ) ;
#42806 = CARTESIAN_POINT ( 'NONE',  ( 8.480977594057447888, 7.382886909400594888, -71.57027735648773614 ) ) ;
#42807 = CARTESIAN_POINT ( 'NONE',  ( 172.9865732929135902, 70.06394889612622023, 0.000000000000000000 ) ) ;
#42808 = CYLINDRICAL_SURFACE ( 'NONE', #24374, 7.500000000000013323 ) ;
#42809 = CARTESIAN_POINT ( 'NONE',  ( -4.513903087372268530, 6.697902023160576590, 30.88178378492203890 ) ) ;
#42810 = CARTESIAN_POINT ( 'NONE',  ( -95.52163045714287648, 29.47808868198296040, -18.93148129228250554 ) ) ;
#42811 = CARTESIAN_POINT ( 'NONE',  ( 79.17772719511384594, 18.06403411472781428, 91.81807103218608290 ) ) ;
#42812 = B_SPLINE_CURVE_WITH_KNOTS ( 'NONE', 3,
 ( #12530, #55430, #51890, #62801, #3368, #57178 ),
 .UNSPECIFIED., .F., .F.,
 ( 4, 2, 4 ),
 ( 2.380731629581200700E-07, 0.002336973833157563775, 0.004673709593152168724 ),
 .UNSPECIFIED. ) ;
#42813 = ORIENTED_EDGE ( 'NONE', *, *, #28421, .F. ) ;
#42814 = DIRECTION ( 'NONE',  ( -9.950807539071958118E-15, 1.000000000000000000, 4.024558464266191670E-15 ) ) ;
#42815 = CARTESIAN_POINT ( 'NONE',  ( 311.9975424824652350, 20.00000000000003197, 255.6641978984094408 ) ) ;
#42816 = CARTESIAN_POINT ( 'NONE',  ( -133.0808647576833721, 51.41195281028755915, 13.43549370681501109 ) ) ;
#42817 = CARTESIAN_POINT ( 'NONE',  ( -108.9145525555662317, 37.42858360505775295, 61.35666273033913143 ) ) ;
#42818 = DIRECTION ( 'NONE',  ( -1.000000000000000000, 0.000000000000000000, 0.000000000000000000 ) ) ;
#42819 = VERTEX_POINT ( 'NONE', #21828 ) ;
#42820 = DIRECTION ( 'NONE',  ( 0.000000000000000000, 1.000000000000000000, 0.000000000000000000 ) ) ;
#42821 = CARTESIAN_POINT ( 'NONE',  ( 91.13361825170463248, 21.00701373666981553, 70.07319469683858415 ) ) ;
#42822 = CARTESIAN_POINT ( 'NONE',  ( 197.9843579228224542, 99.18296459057400227, -13.62550849792877727 ) ) ;
#42823 = CARTESIAN_POINT ( 'NONE',  ( -156.6452887561481191, 70.47820714639399853, 89.58194124164906214 ) ) ;
#42824 = LINE ( 'NONE', #69560, #44751 ) ;
#42825 = VERTEX_POINT ( 'NONE', #62780 ) ;
#42826 = CARTESIAN_POINT ( 'NONE',  ( 0.7145311798161619876, -4.618802153517266085, -8.000000000000000000 ) ) ;
#42827 = CARTESIAN_POINT ( 'NONE',  ( 79.13041963748372609, 18.04952109592810316, 9.847327292909767493 ) ) ;
#42828 = CARTESIAN_POINT ( 'NONE',  ( 164.9547823171480161, 65.03046442419433504, 9.505235400904521015 ) ) ;
#42829 = DIRECTION ( 'NONE',  ( -1.000000000000000000, 0.000000000000000000, 0.000000000000000000 ) ) ;
#42830 = VECTOR ( 'NONE', #38868, 1000.000000000000000 ) ;
#42831 = AXIS2_PLACEMENT_3D ( 'NONE', #28678, #33265, #17411 ) ;
#42832 = ORIENTED_EDGE ( 'NONE', *, *, #42586, .F. ) ;
#42833 = EDGE_CURVE ( 'NONE', #57391, #54100, #29688, .T. ) ;
#42834 = CARTESIAN_POINT ( 'NONE',  ( 0.000000000000000000, 0.000000000000000000, 41.38025477438755928 ) ) ;
#42835 = AXIS2_PLACEMENT_3D ( 'NONE', #65818, #13722, #50660 ) ;
#42836 = VERTEX_POINT ( 'NONE', #48202 ) ;
#42837 = CARTESIAN_POINT ( 'NONE',  ( -107.0751323097254755, 35.28386110859232616, -48.30244191324285197 ) ) ;
#42838 = CARTESIAN_POINT ( 'NONE',  ( 68.61679388097590504, 14.04192738700837673, -75.05900237351899307 ) ) ;
#42839 = CARTESIAN_POINT ( 'NONE',  ( 16.78635691501517613, 0.000000000000000000, -36.68900338898716740 ) ) ;
#42841 = ORIENTED_EDGE ( 'NONE', *, *, #57039, .F. ) ;
#42840 = CARTESIAN_POINT ( 'NONE',  ( 149.9883446984744637, 53.30011109831375649, 9.477168676321245044 ) ) ;
#42842 = CARTESIAN_POINT ( 'NONE',  ( -175.1920326508032986, 89.46239303019291356, 31.10066421722925867 ) ) ;
#42843 = VECTOR ( 'NONE', #29316, 1000.000000000000000 ) ;
#42844 = DIRECTION ( 'NONE',  ( 1.000000000000000000, 0.000000000000000000, 0.000000000000000000 ) ) ;
#42845 = CARTESIAN_POINT ( 'NONE',  ( 117.3246714514015849, 33.42485879931865611, -45.94399363046861140 ) ) ;
#42846 = ORIENTED_EDGE ( 'NONE', *, *, #67027, .T. ) ;
#42847 = CARTESIAN_POINT ( 'NONE',  ( 41.72486082342823721, -50.31647622756196370, 3.125053320693569132E-16 ) ) ;
#42848 = EDGE_CURVE ( 'NONE', #66081, #12944, #52404, .T. ) ;
#42849 = EDGE_CURVE ( 'NONE', #9033, #3775, #27451, .T. ) ;
#42850 = DIRECTION ( 'NONE',  ( 0.000000000000000000, 0.000000000000000000, -1.000000000000000000 ) ) ;
#42851 = CARTESIAN_POINT ( 'NONE',  ( -15.55634918610396866, 31.11269837220809009, 0.000000000000000000 ) ) ;
#42852 = CARTESIAN_POINT ( 'NONE',  ( 126.3732561463888118, 38.23795180971326602, 63.29033028859080900 ) ) ;
#42853 = EDGE_LOOP ( 'NONE', ( #57738, #43648, #56935, #23898, #64358, #12355, #3672, #43603, #48748 ) ) ;
#42854 = EDGE_LOOP ( 'NONE', ( #45965, #65055 ) ) ;
#42855 = ORIENTED_EDGE ( 'NONE', *, *, #59929, .F. ) ;
#42856 = EDGE_CURVE ( 'NONE', #23240, #14014, #7052, .T. ) ;
#42857 = CARTESIAN_POINT ( 'NONE',  ( 204.6977192012829789, -170.0000000000000000, 71.05227132923315025 ) ) ;
#42858 = LINE ( 'NONE', #39001, #54463 ) ;
#42859 = LINE ( 'NONE', #48464, #48135 ) ;
#42860 = FACE_OUTER_BOUND ( 'NONE', #33827, .T. ) ;
#42861 = CARTESIAN_POINT ( 'NONE',  ( 67.87214640187850989, 13.85168242453936216, 85.27733058027321533 ) ) ;
#42862 = DIRECTION ( 'NONE',  ( 0.000000000000000000, 0.000000000000000000, -1.000000000000000000 ) ) ;
#42863 = CARTESIAN_POINT ( 'NONE',  ( -132.4819073909166320, 50.98736898418875541, 68.58703093612896851 ) ) ;
#42864 = DIRECTION ( 'NONE',  ( 0.000000000000000000, 0.000000000000000000, 1.000000000000000000 ) ) ;
#42865 = VERTEX_POINT ( 'NONE', #54529 ) ;
#42866 = CARTESIAN_POINT ( 'NONE',  ( -96.89873354725229149, 31.24547541778401794, -90.96072102636905754 ) ) ;
#42867 = ORIENTED_EDGE ( 'NONE', *, *, #38012, .F. ) ;
#42868 = CARTESIAN_POINT ( 'NONE',  ( -71.17846906053300415, 20.67346400882179935, 64.26825347421748802 ) ) ;
#42869 = CARTESIAN_POINT ( 'NONE',  ( 212.0180052085438263, 116.9552462415715013, -69.00676071747216156 ) ) ;
#42870 = EDGE_CURVE ( 'NONE', #42507, #52659, #2089, .T. ) ;
#42871 = CYLINDRICAL_SURFACE ( 'NONE', #26474, 65.36598343705435354 ) ;
#42872 = LINE ( 'NONE', #59404, #27047 ) ;
#42873 = CARTESIAN_POINT ( 'NONE',  ( -34.73655621045444519, 10.15566554627628371, -89.75670392811869647 ) ) ;
#42874 = CARTESIAN_POINT ( 'NONE',  ( 46.66904755831207297, -10.55634918610412853, 0.000000000000000000 ) ) ;
#42875 = VECTOR ( 'NONE', #4350, 1000.000000000000114 ) ;
#42876 = CARTESIAN_POINT ( 'NONE',  ( 0.000000000000000000, 0.000000000000000000, 2.000000000000001776 ) ) ;
#42877 = ADVANCED_FACE ( 'NONE', ( #11619 ), #33093, .T. ) ;
#42878 = EDGE_CURVE ( 'NONE', #44611, #34598, #40689, .T. ) ;
#42879 = CARTESIAN_POINT ( 'NONE',  ( 164.4760519199595592, 64.62478832434436526, -67.73851987524837170 ) ) ;
#42880 = ORIENTED_EDGE ( 'NONE', *, *, #66000, .T. ) ;
#42881 = AXIS2_PLACEMENT_3D ( 'NONE', #16475, #33366, #37582 ) ;
#42882 = CARTESIAN_POINT ( 'NONE',  ( 49.76301652092165995, 41.81676920493114835, 170.0000000000000000 ) ) ;
#42883 = CARTESIAN_POINT ( 'NONE',  ( 8.000000000000007105, 249.8719672152120381, -95.00000000000133582 ) ) ;
#42884 = EDGE_LOOP ( 'NONE', ( #36085, #44147, #19149, #41790 ) ) ;
#42885 = VERTEX_POINT ( 'NONE', #30253 ) ;
#42886 = CARTESIAN_POINT ( 'NONE',  ( -28.13128612339710344, 10.08889185338653327, -62.91279178769815417 ) ) ;
#42887 = CARTESIAN_POINT ( 'NONE',  ( 56.66438910147189034, 11.28870326331392704, -47.21719651937512197 ) ) ;
#42888 = VECTOR ( 'NONE', #29055, 1000.000000000000000 ) ;
#42889 = CARTESIAN_POINT ( 'NONE',  ( 31.11269837220803325, -10.55634918610409656, 2.000000000000001776 ) ) ;
#42890 = CARTESIAN_POINT ( 'NONE',  ( 15.55634918610400241, -15.55634918610406103, 2.000000000000001776 ) ) ;
#42891 = VECTOR ( 'NONE', #20366, 1000.000000000000000 ) ;
#42892 = ORIENTED_EDGE ( 'NONE', *, *, #65928, .F. ) ;
#42893 = CLOSED_SHELL ( 'NONE', ( #21321, #26910, #50343, #65857, #27010, #8423, #12964, #28319, #61135, #21352, #53679, #9857, #10700, #21422, #24695, #13635, #32965, #3439, #45010, #10784, #31914, #20784, #12906 ) ) ;
#42894 = VERTEX_POINT ( 'NONE', #25330 ) ;
#42895 = CARTESIAN_POINT ( 'NONE',  ( -126.7944042662569046, 48.29830493043729689, 30.66038275586655359 ) ) ;
#42896 = ORIENTED_EDGE ( 'NONE', *, *, #14153, .T. ) ;
#42897 = DIRECTION ( 'NONE',  ( -0.000000000000000000, -0.000000000000000000, 1.000000000000000000 ) ) ;
#42898 = CARTESIAN_POINT ( 'NONE',  ( 187.1539087446606118, 86.45467532021284285, -92.98937004433818743 ) ) ;
#42899 = CARTESIAN_POINT ( 'NONE',  ( 59.29597493004737174, 11.84030339376940510, 70.68833123368655436 ) ) ;
#42900 = CARTESIAN_POINT ( 'NONE',  ( -33.15588700722115334, 4.239136313921378907, 6.893343212288942645 ) ) ;
#42901 = DIRECTION ( 'NONE',  ( -1.000000000000000000, 0.000000000000000000, 0.000000000000000000 ) ) ;
#42902 =( NAMED_UNIT ( * ) PLANE_ANGLE_UNIT ( ) SI_UNIT ( $, .RADIAN. ) );
#42903 = CYLINDRICAL_SURFACE ( 'NONE', #9904, 7.500000000000013323 ) ;
#42904 = ORIENTED_EDGE ( 'NONE', *, *, #7249, .F. ) ;
#42905 = ORIENTED_EDGE ( 'NONE', *, *, #64505, .T. ) ;
#42906 = CARTESIAN_POINT ( 'NONE',  ( -1.734723475976807094E-15, 9.237604307034022355, -0.7145311798163346273 ) ) ;
#42907 = CARTESIAN_POINT ( 'NONE',  ( 110.0000000000000284, -22.00000000000000000, 5.000000000000004441 ) ) ;
#42908 = CARTESIAN_POINT ( 'NONE',  ( 412.0000000000000000, -2.000000000000000000, 0.000000000000000000 ) ) ;
#42909 = CARTESIAN_POINT ( 'NONE',  ( 23.17627457812186620, -71.32923872213625316, 0.000000000000000000 ) ) ;
#42910 = CARTESIAN_POINT ( 'NONE',  ( 75.31295361348104223, 9.223176757708265897E-15, -2.499999999999970246 ) ) ;
#42911 = CARTESIAN_POINT ( 'NONE',  ( 19.83783859368179492, 7.671370827793382752, 84.88257075276666797 ) ) ;
#42912 = ORIENTED_EDGE ( 'NONE', *, *, #46537, .F. ) ;
#42913 = ADVANCED_FACE ( 'NONE', ( #24980 ), #56280, .T. ) ;
#42914 = FACE_OUTER_BOUND ( 'NONE', #7500, .T. ) ;
#42915 = ORIENTED_EDGE ( 'NONE', *, *, #27694, .F. ) ;
#42916 = CARTESIAN_POINT ( 'NONE',  ( -71.96390573417173186, 19.88067451234326199, 41.32151012117945754 ) ) ;
#42917 = ORIENTED_EDGE ( 'NONE', *, *, #63278, .F. ) ;
#42918 = EDGE_CURVE ( 'NONE', #47295, #38817, #56630, .T. ) ;
#42919 = VECTOR ( 'NONE', #16540, 1000.000000000000000 ) ;
#42920 = VERTEX_POINT ( 'NONE', #51363 ) ;
#42921 = CARTESIAN_POINT ( 'NONE',  ( 14.80205238535217127, 6.470775952815777998, -50.46994021608795578 ) ) ;
#42922 = CARTESIAN_POINT ( 'NONE',  ( -178.7483298110140311, 93.61800926271537548, 60.20166031997415956 ) ) ;
#42923 = CARTESIAN_POINT ( 'NONE',  ( 18.21423326326597802, 6.590134686181412960, 17.78374723810611258 ) ) ;
#42924 = VECTOR ( 'NONE', #57338, 1000.000000000000000 ) ;
#42925 = VERTEX_POINT ( 'NONE', #67892 ) ;
#42926 = EDGE_CURVE ( 'NONE', #69067, #10198, #31990, .T. ) ;
#42927 = AXIS2_PLACEMENT_3D ( 'NONE', #50962, #8047, #25278 ) ;
#42928 = EDGE_CURVE ( 'NONE', #68299, #39568, #30596, .T. ) ;
#42929 = DIRECTION ( 'NONE',  ( 1.000000000000000000, -0.000000000000000000, 0.000000000000000000 ) ) ;
#42930 = FACE_OUTER_BOUND ( 'NONE', #56166, .T. ) ;
#42931 = CARTESIAN_POINT ( 'NONE',  ( 70.26639875985991068, 15.51307715494295891, 39.29493570883701636 ) ) ;
#42932 = DIRECTION ( 'NONE',  ( -1.000000000000000000, 0.000000000000000000, 0.000000000000000000 ) ) ;
#42933 = CARTESIAN_POINT ( 'NONE',  ( 16.78635691501517613, 6.000000000000000000, -9.435653166495500344 ) ) ;
#42934 = DIRECTION ( 'NONE',  ( 0.4738686624730094610, -0.8805955318567321166, 0.000000000000000000 ) ) ;
#42935 = EDGE_CURVE ( 'NONE', #26400, #6906, #12930, .T. ) ;
#42936 = CARTESIAN_POINT ( 'NONE',  ( -27.70562707895080123, 9.007984652865420827, 31.19301926817212944 ) ) ;
#42937 = CARTESIAN_POINT ( 'NONE',  ( 141.9165763529819344, -52.00000000000000711, 129.0000000000000000 ) ) ;
#42938 = ORIENTED_EDGE ( 'NONE', *, *, #31321, .T. ) ;
#42939 = LINE ( 'NONE', #64408, #2736 ) ;
#42940 = CARTESIAN_POINT ( 'NONE',  ( -5.871577929436020860, 6.771181646175758573, -62.50473750044589849 ) ) ;
#42941 = CARTESIAN_POINT ( 'NONE',  ( -173.9526029538035914, 89.57590038685106038, 57.70062692409361205 ) ) ;
#42942 = CARTESIAN_POINT ( 'NONE',  ( 2.005731055991735623, 2.000000000000000000, 0.000000000000000000 ) ) ;
#42943 = CARTESIAN_POINT ( 'NONE',  ( -120.6739978760426482, 44.33795494230364653, -37.02276080820320203 ) ) ;
#42944 = CARTESIAN_POINT ( 'NONE',  ( -83.13046924527391468, 25.15778674529013870, 5.041952259388867041 ) ) ;
#42945 = DIRECTION ( 'NONE',  ( 4.573512162503259427E-19, 5.081588203714612465E-18, -1.000000000000000000 ) ) ;
#42946 = CARTESIAN_POINT ( 'NONE',  ( 111.3012118866375033, 21.46131765974229566, -4.839032743736826347 ) ) ;
#42947 = CARTESIAN_POINT ( 'NONE',  ( -124.7710763417278059, 46.96042092553522451, -76.67722191208665095 ) ) ;
#42948 = CARTESIAN_POINT ( 'NONE',  ( 68.93219921887765622, 14.12322281954859804, 5.852687346813395308 ) ) ;
#42949 = CARTESIAN_POINT ( 'NONE',  ( 41.66904755831210849, 0.000000000000000000, 2.000000000000000000 ) ) ;
#42950 = CARTESIAN_POINT ( 'NONE',  ( 91.49210130311621469, 22.20929244416438664, -10.76186516580451524 ) ) ;
#42951 = ORIENTED_EDGE ( 'NONE', *, *, #19934, .F. ) ;
#42952 = CARTESIAN_POINT ( 'NONE',  ( -37.93379515072632557, 11.77251734620211110, 7.088915133309215300 ) ) ;
#42953 = EDGE_LOOP ( 'NONE', ( #44769, #68209, #54473, #33996 ) ) ;
#42954 = DIRECTION ( 'NONE',  ( 1.000000000000000000, 0.000000000000000000, 0.000000000000000000 ) ) ;
#42955 = EDGE_LOOP ( 'NONE', ( #44979, #28304, #33028, #5577 ) ) ;
#42956 = DIRECTION ( 'NONE',  ( 1.000000000000000000, 0.000000000000000000, 0.000000000000000000 ) ) ;
#42957 = CARTESIAN_POINT ( 'NONE',  ( 103.0533600994152295, 26.78891014864192499, 88.63686854957322225 ) ) ;
#42958 = CARTESIAN_POINT ( 'NONE',  ( -147.7925265216585444, 64.04960911618972830, 57.76075631580095404 ) ) ;
#42959 = PLANE ( 'NONE',  #33309 ) ;
#42960 = ADVANCED_FACE ( 'NONE', ( #48456 ), #290, .T. ) ;
#42961 = EDGE_CURVE ( 'NONE', #58924, #6777, #20372, .T. ) ;
#42962 = CARTESIAN_POINT ( 'NONE',  ( 141.2801018238827169, 47.29457739955284978, -42.42097328515919941 ) ) ;
#42963 = CARTESIAN_POINT ( 'NONE',  ( -47.65155309726507937, 13.85482731128118239, -70.79954927902053896 ) ) ;
#42964 = LINE ( 'NONE', #43311, #22972 ) ;
#42965 = EDGE_CURVE ( 'NONE', #6792, #36547, #443, .T. ) ;
#42966 = DIRECTION ( 'NONE',  ( 0.000000000000000000, 0.000000000000000000, 1.000000000000000000 ) ) ;
#42967 = ORIENTED_EDGE ( 'NONE', *, *, #18590, .F. ) ;
#42968 = ORIENTED_EDGE ( 'NONE', *, *, #16733, .F. ) ;
#42969 = CARTESIAN_POINT ( 'NONE',  ( 32.38493285958205803, 8.611594965040680449, 61.59909279486555533 ) ) ;
#42970 = CARTESIAN_POINT ( 'NONE',  ( 185.0682806122092927, 84.19715153078853120, 84.13611250625842786 ) ) ;
#42971 = CARTESIAN_POINT ( 'NONE',  ( 26.12852347772543737, 100.0000000000000000, 129.5802547743875550 ) ) ;
#42972 = CIRCLE ( 'NONE', #68793, 63.00000000000000000 ) ;
#42973 = CARTESIAN_POINT ( 'NONE',  ( 447.3372781065086201, 177.8591479523844612, 78.55029585798806124 ) ) ;
#42974 = ORIENTED_EDGE ( 'NONE', *, *, #65680, .T. ) ;
#42975 = CARTESIAN_POINT ( 'NONE',  ( 93.08174259058942823, 22.79847752828721852, 14.22235957612315005 ) ) ;
#42976 = CARTESIAN_POINT ( 'NONE',  ( 181.5079096844945923, 80.47139261082469375, -24.38050707541594875 ) ) ;
#42977 = CARTESIAN_POINT ( 'NONE',  ( 208.9583973663597760, 114.1615900753670871, 3.674711021178045822 ) ) ;
#42978 = CIRCLE ( 'NONE', #41896, 246.3582898394606957 ) ;
#42979 = CYLINDRICAL_SURFACE ( 'NONE', #41955, 7.500000000000013323 ) ;
#42980 = CARTESIAN_POINT ( 'NONE',  ( 42.70988075781784232, 8.862408058333477001, -23.02393441155776088 ) ) ;
#42981 = CARTESIAN_POINT ( 'NONE',  ( -430.1627218934915504, 400.0000000000065370, -123.9497041420119530 ) ) ;
#42982 = DIRECTION ( 'NONE',  ( 0.7071067811865477948, -9.875400524329059797E-15, 0.7071067811865473507 ) ) ;
#42983 = CARTESIAN_POINT ( 'NONE',  ( 164.4761273435911164, 64.62485394454741083, 61.02434369218256904 ) ) ;
#42984 = VECTOR ( 'NONE', #49112, 1000.000000000000000 ) ;
#42985 = AXIS2_PLACEMENT_3D ( 'NONE', #27583, #26894, #11057 ) ;
#42986 = ORIENTED_EDGE ( 'NONE', *, *, #30873, .T. ) ;
#42987 = CARTESIAN_POINT ( 'NONE',  ( -149.5074843970971017, 64.17983161892348676, -22.96827994102829962 ) ) ;
#42988 = CARTESIAN_POINT ( 'NONE',  ( 94.02499804464933675, 23.15433260743127519, -42.04956284518182485 ) ) ;
#42989 = AXIS2_PLACEMENT_3D ( 'NONE', #39181, #17000, #12440 ) ;
#42990 = DIRECTION ( 'NONE',  ( -1.000000000000000000, 0.000000000000000000, 0.000000000000000000 ) ) ;
#42991 = DIRECTION ( 'NONE',  ( 0.000000000000000000, 1.000000000000000000, -0.000000000000000000 ) ) ;
#42992 = CARTESIAN_POINT ( 'NONE',  ( 150.0433793199863999, 52.09973307442957235, 8.984650821496048323 ) ) ;
#42993 = CARTESIAN_POINT ( 'NONE',  ( -15.30860234794697128, 8.505246639038775314, 91.90313363028508320 ) ) ;
#42994 = ORIENTED_EDGE ( 'NONE', *, *, #18905, .T. ) ;
#42995 = CARTESIAN_POINT ( 'NONE',  ( 36.85262215550149278, -53.56030941157680303, 170.0000000000000000 ) ) ;
#42996 = CARTESIAN_POINT ( 'NONE',  ( 110.2429982417149574, -170.0000000000000000, -35.92243756565368784 ) ) ;
#42997 = EDGE_LOOP ( 'NONE', ( #16580, #6243, #69449, #55082 ) ) ;
#42998 = ORIENTED_EDGE ( 'NONE', *, *, #38644, .T. ) ;
#42999 = ADVANCED_FACE ( 'NONE', ( #10503 ), #26694, .F. ) ;
#43000 = CARTESIAN_POINT ( 'NONE',  ( 39.74315982117121138, 9.468838313655563610, 83.60352190905523173 ) ) ;
#43001 = CARTESIAN_POINT ( 'NONE',  ( 209.3223706822284100, 190.0000000000000000, 276.7520087653757628 ) ) ;
#43002 = CARTESIAN_POINT ( 'NONE',  ( 91.49210130311617206, 22.20929244416436887, -64.45096634673186031 ) ) ;
#43003 = ORIENTED_EDGE ( 'NONE', *, *, #66795, .F. ) ;
#43004 = CARTESIAN_POINT ( 'NONE',  ( -61.38706483483510823, 16.47181058798476272, -65.53751323400399542 ) ) ;
#43005 = CARTESIAN_POINT ( 'NONE',  ( -1.328627985309863258, 7.561890325089884790, 7.015677182669254996 ) ) ;
#43006 = CARTESIAN_POINT ( 'NONE',  ( 178.1888264190354221, 77.13727704498026583, -36.79301795762072658 ) ) ;
#43007 = CARTESIAN_POINT ( 'NONE',  ( 161.5764509652428558, 60.91546192849696695, 84.31444485276320222 ) ) ;
#43008 = CARTESIAN_POINT ( 'NONE',  ( 94.12811352634518869, 22.11743943276050217, 36.68810650112212812 ) ) ;
#43009 = EDGE_CURVE ( 'NONE', #57368, #43248, #21406, .T. ) ;
#43010 = ORIENTED_EDGE ( 'NONE', *, *, #65275, .T. ) ;
#43011 = CARTESIAN_POINT ( 'NONE',  ( -47.94536219817736367, 13.92422159065987586, -45.16206988751260099 ) ) ;
#43012 = CIRCLE ( 'NONE', #40780, 4.250000000000000000 ) ;
#43013 = CARTESIAN_POINT ( 'NONE',  ( -173.1211646369891355, -170.0000000000000000, 38.32169460664103156 ) ) ;
#43014 = EDGE_CURVE ( 'NONE', #14760, #50465, #59032, .T. ) ;
#43015 = CARTESIAN_POINT ( 'NONE',  ( 8.679939806240504652, 7.383357464882123189, 39.91928050070973200 ) ) ;
#43016 = CARTESIAN_POINT ( 'NONE',  ( 123.4242852856285566, 10.00000000000000000, -20.00000000000000000 ) ) ;
#43017 = EDGE_CURVE ( 'NONE', #30419, #64201, #22450, .T. ) ;
#43018 = CARTESIAN_POINT ( 'NONE',  ( 79.17818378172918869, 17.01182329587643238, 91.82197126792017627 ) ) ;
#43020 = EDGE_LOOP ( 'NONE', ( #40827, #20767, #11775, #39542, #57360 ) ) ;
#43019 = CARTESIAN_POINT ( 'NONE',  ( 311.9975424824652350, 20.00000000000003197, 380.0000000000001137 ) ) ;
#43021 = ORIENTED_EDGE ( 'NONE', *, *, #41061, .F. ) ;
#43022 = VECTOR ( 'NONE', #22214, 1000.000000000000000 ) ;
#43023 = EDGE_CURVE ( 'NONE', #35894, #49086, #50234, .T. ) ;
#43024 = ORIENTED_EDGE ( 'NONE', *, *, #37141, .T. ) ;
#43025 = AXIS2_PLACEMENT_3D ( 'NONE', #67829, #15046, #19276 ) ;
#43026 = CARTESIAN_POINT ( 'NONE',  ( 0.000000000000000000, 35.00000000000000000, 0.000000000000000000 ) ) ;
#43027 = CARTESIAN_POINT ( 'NONE',  ( -166.2780847427887352, 81.26478456797779870, 88.92219257149233158 ) ) ;
#43028 = DIRECTION ( 'NONE',  ( -1.000000000000000000, 0.000000000000000000, 0.000000000000000000 ) ) ;
#43029 = DIRECTION ( 'NONE',  ( -0.000000000000000000, -0.000000000000000000, -1.000000000000000000 ) ) ;
#43030 = AXIS2_PLACEMENT_3D ( 'NONE', #7675, #55492, #62775 ) ;
#43031 = CARTESIAN_POINT ( 'NONE',  ( -38.68632430131781064, 11.91908191268693251, 66.50744903314554790 ) ) ;
#43032 = AXIS2_PLACEMENT_3D ( 'NONE', #44570, #39297, #27682 ) ;
#43033 = CARTESIAN_POINT ( 'NONE',  ( -12.78319349481551725, 8.274445259016797394, -10.42464620885755266 ) ) ;
#43034 = CARTESIAN_POINT ( 'NONE',  ( 153.8366942494330942, 54.87992279068316037, -63.90365245542865580 ) ) ;
#43035 = DIRECTION ( 'NONE',  ( 1.000000000000000000, 0.000000000000000000, 0.000000000000000000 ) ) ;
#43036 = ORIENTED_EDGE ( 'NONE', *, *, #56793, .T. ) ;
#43037 = AXIS2_PLACEMENT_3D ( 'NONE', #29011, #29340, #66643 ) ;
#43038 = CARTESIAN_POINT ( 'NONE',  ( -156.4841188516942907, 70.33041971808550841, -45.07929577857993308 ) ) ;
#43039 = VERTEX_POINT ( 'NONE', #60074 ) ;
#43040 = ORIENTED_EDGE ( 'NONE', *, *, #37560, .F. ) ;
#43041 = CARTESIAN_POINT ( 'NONE',  ( 9.319975126229035567, 7.386007236262731368, 94.99999999999866418 ) ) ;
#43042 = CARTESIAN_POINT ( 'NONE',  ( -81.90760111942957167, 24.66532273091449312, -35.83518030727707071 ) ) ;
#43043 = VECTOR ( 'NONE', #62802, 1000.000000000000000 ) ;
#43044 = CARTESIAN_POINT ( 'NONE',  ( -23.94713223918401823, 9.496086756559476427, 90.93069671979091595 ) ) ;
#43045 = CARTESIAN_POINT ( 'NONE',  ( -150.5993571094983281, 66.43939758484178526, 3.952979209143682837 ) ) ;
#43046 = EDGE_CURVE ( 'NONE', #57672, #30275, #55499, .T. ) ;
#43047 = LINE ( 'NONE', #23001, #68562 ) ;
#43048 = FACE_OUTER_BOUND ( 'NONE', #10384, .T. ) ;
#43049 = EDGE_CURVE ( 'NONE', #67765, #33172, #59721, .T. ) ;
#43050 = CARTESIAN_POINT ( 'NONE',  ( -146.9440914296272354, 63.34059920040223091, 84.83934254479170534 ) ) ;
#43051 = ORIENTED_EDGE ( 'NONE', *, *, #28779, .F. ) ;
#43052 = VERTEX_POINT ( 'NONE', #22103 ) ;
#43053 = ORIENTED_EDGE ( 'NONE', *, *, #41772, .F. ) ;
#43054 = CARTESIAN_POINT ( 'NONE',  ( -156.4797890011541313, 71.69341087347109465, -18.24543932660331080 ) ) ;
#43055 = CARTESIAN_POINT ( 'NONE',  ( 87.42982051347729566, 20.76007613954182318, -89.54297233556741276 ) ) ;
#43056 = APPLICATION_CONTEXT ( 'automotive_design' ) ;
#43057 = CARTESIAN_POINT ( 'NONE',  ( 24.39800339187844003, 60.26242556095705538, 0.000000000000000000 ) ) ;
#43058 = LINE ( 'NONE', #5093, #26249 ) ;
#43059 = ORIENTED_EDGE ( 'NONE', *, *, #2575, .T. ) ;
#43060 = DIRECTION ( 'NONE',  ( -0.000000000000000000, -0.000000000000000000, 1.000000000000000000 ) ) ;
#43061 = CARTESIAN_POINT ( 'NONE',  ( -149.9449619562961402, 64.55090813009800854, 57.56537183036274996 ) ) ;
#43062 =( NAMED_UNIT ( * ) PLANE_ANGLE_UNIT ( ) SI_UNIT ( $, .RADIAN. ) );
#43063 = CARTESIAN_POINT ( 'NONE',  ( 22.62427395637551086, 7.823784829753561709, 7.575073927682081987 ) ) ;
#43064 =( NAMED_UNIT ( * ) SI_UNIT ( $, .STERADIAN. ) SOLID_ANGLE_UNIT ( ) );
#43065 = LINE ( 'NONE', #59584, #60053 ) ;
#43066 = CARTESIAN_POINT ( 'NONE',  ( -84.97622048504842951, 24.82614411847759683, -46.67722756215049884 ) ) ;
#43067 = CARTESIAN_POINT ( 'NONE',  ( 19.75784582661439970, 6.660183274347837745, 70.72739093580082681 ) ) ;
#43068 = CARTESIAN_POINT ( 'NONE',  ( -12.99999999999999822, 10.00000000000000000, -17.00000000000000355 ) ) ;
#43069 = CARTESIAN_POINT ( 'NONE',  ( 8.528421445032392967, 6.376778749352034481, -71.80901206443022033 ) ) ;
#43070 = AXIS2_PLACEMENT_3D ( 'NONE', #35661, #52518, #62389 ) ;
#43071 = ORIENTED_EDGE ( 'NONE', *, *, #33742, .T. ) ;
#43073 = DIRECTION ( 'NONE',  ( 1.000000000000000000, 0.000000000000000000, 1.337618101958020291E-16 ) ) ;
#43072 = AXIS2_PLACEMENT_3D ( 'NONE', #46347, #35109, #61155 ) ;
#43074 = PRODUCT_CONTEXT ( 'NONE', #14326, 'mechanical' ) ;
#43075 = CYLINDRICAL_SURFACE ( 'NONE', #56562, 65.00000000000000000 ) ;
#43076 = DIRECTION ( 'NONE',  ( -0.000000000000000000, -0.000000000000000000, -1.000000000000000000 ) ) ;
#43077 = CARTESIAN_POINT ( 'NONE',  ( 46.41758729921146198, 9.425975226414248453, -72.62734698405610345 ) ) ;
#43078 = CARTESIAN_POINT ( 'NONE',  ( 55.56634333706183781, 12.09342294753929714, -71.06672960848410980 ) ) ;
#43079 = VERTEX_POINT ( 'NONE', #6265 ) ;
#43080 = PRODUCT_DEFINITION ( 'UNKNOWN', '', #10805, #5010 ) ;
#43081 = AXIS2_PLACEMENT_3D ( 'NONE', #2079, #23530, #45318 ) ;
#43082 = VERTEX_POINT ( 'NONE', #11530 ) ;
#43083 = CARTESIAN_POINT ( 'NONE',  ( -35.00000000000002842, -35.00000000000000000, 0.000000000000000000 ) ) ;
#43084 = EDGE_CURVE ( 'NONE', #8339, #6977, #28633, .T. ) ;
#43085 = B_SPLINE_CURVE_WITH_KNOTS ( 'NONE', 3,
 ( #46398, #56267, #3497, #24275, #4198, #51001, #63283, #18985, #8084, #68557, #29889, #51691, #30239, #35160, #25662, #14409, #61885, #67878, #24623, #20031, #62936, #56617, #14053, #46057, #8792, #29531, #52031, #56975, #51353, #45722, #35513, #8439, #20360, #47094, #13707, #3165, #19674, #41827, #67528, #36206, #41134, #15093, #57661, #30583, #41484, #62601, #35860, #9473, #40437, #3851, #57314, #9129, #46750, #14740, #2812, #68223, #19328, #30934 ),
 .UNSPECIFIED., .F., .F.,
 ( 4, 2, 2, 2, 2, 2, 2, 2, 2, 2, 2, 2, 2, 2, 2, 2, 2, 2, 2, 2, 2, 2, 2, 2, 2, 2, 2, 2, 4 ),
 ( 0.000000000000000000, 0.002174461951613288098, 0.003261692927419951663, 0.004348923903226615227, 0.005436154879033277924, 0.006523385854839942356, 0.007610616830646605054, 0.008697847806453268618, 0.009785078782259933050, 0.01087230975806659575, 0.01195954073387325844, 0.01304677170967992288, 0.01522123366129330725, 0.01630846463709996821, 0.01739569561290663091, 0.01957015756451988345, 0.02065738854032650451, 0.02174461951613312558, 0.02391908146774630525, 0.02609354341935948840, 0.02718077439516605742, 0.02826800537097262644, 0.02881162085887593177, 0.02935523634677923710, 0.03044246732258585816, 0.03152969829839247229, 0.03261692927419908988, 0.03370416025000570748, 0.03479139122581232507 ),
 .UNSPECIFIED. ) ;
#43086 = VECTOR ( 'NONE', #63176, 1000.000000000000000 ) ;
#43087 = CARTESIAN_POINT ( 'NONE',  ( 197.4121679705847896, 98.46451029407256783, 8.075550651409916014 ) ) ;
#43088 = ORIENTED_EDGE ( 'NONE', *, *, #24415, .F. ) ;
#43089 = ORIENTED_EDGE ( 'NONE', *, *, #33274, .F. ) ;
#43090 = EDGE_CURVE ( 'NONE', #40950, #16235, #14656, .T. ) ;
#43091 = VECTOR ( 'NONE', #48859, 1000.000000000000000 ) ;
#43092 = CARTESIAN_POINT ( 'NONE',  ( 117.3110050642448243, 32.29133253383017177, 61.39698313137674290 ) ) ;
#43093 = VERTEX_POINT ( 'NONE', #45293 ) ;
#43094 = CARTESIAN_POINT ( 'NONE',  ( 116.8917656767876565, 33.20682060519245482, 67.43530244170412402 ) ) ;
#43095 = CARTESIAN_POINT ( 'NONE',  ( 103.0463737467386665, 26.78595250599333255, -95.00000000000133582 ) ) ;
#43096 = CARTESIAN_POINT ( 'NONE',  ( 138.5684226926155418, 45.53585076428268508, 69.70997248683153202 ) ) ;
#43097 = DIRECTION ( 'NONE',  ( -0.000000000000000000, -0.000000000000000000, -1.000000000000000000 ) ) ;
#43098 = AXIS2_PLACEMENT_3D ( 'NONE', #37697, #42299, #5354 ) ;
#43099 = CARTESIAN_POINT ( 'NONE',  ( 0.000000000000000000, 0.000000000000000000, 41.38025477438755928 ) ) ;
#43100 = DIRECTION ( 'NONE',  ( 0.000000000000000000, 1.000000000000000000, -0.000000000000000000 ) ) ;
#43101 = LINE ( 'NONE', #190, #29805 ) ;
#43102 = EDGE_LOOP ( 'NONE', ( #10465, #13359, #5434, #37827 ) ) ;
#43103 = ORIENTED_EDGE ( 'NONE', *, *, #33142, .T. ) ;
#43104 = CARTESIAN_POINT ( 'NONE',  ( 8.000000000000000000, -3.867591403079183365, -0.4976753153245864758 ) ) ;
#43105 = FACE_BOUND ( 'NONE', #67926, .T. ) ;
#43106 = ADVANCED_FACE ( 'NONE', ( #12958 ), #34758, .F. ) ;
#43107 = CARTESIAN_POINT ( 'NONE',  ( -145.3246383987844297, 62.00818849034185121, -48.54254619255401337 ) ) ;
#43108 = EDGE_CURVE ( 'NONE', #4486, #54708, #7679, .T. ) ;
#43109 = DIRECTION ( 'NONE',  ( 0.000000000000000000, 0.9952373409613455291, -0.09748146057682102739 ) ) ;
#43111 = ORIENTED_EDGE ( 'NONE', *, *, #40705, .T. ) ;
#43110 = CARTESIAN_POINT ( 'NONE',  ( -144.9287131874382055, 60.39056348581544853, -36.35316711580674820 ) ) ;
#43112 = FACE_OUTER_BOUND ( 'NONE', #20355, .T. ) ;
#43113 = ORIENTED_EDGE ( 'NONE', *, *, #57336, .T. ) ;
#43114 = LINE ( 'NONE', #30594, #50330 ) ;
#43115 = DIRECTION ( 'NONE',  ( -0.3930250316539148359, -0.9195277725514544587, 0.000000000000000000 ) ) ;
#43116 = CARTESIAN_POINT ( 'NONE',  ( 79.14129363775931836, 17.00055658855363916, -16.97005576640699331 ) ) ;
#43117 = DIRECTION ( 'NONE',  ( -0.9639628606958550172, 0.2660368455666687892, 0.000000000000000000 ) ) ;
#43119 = LINE ( 'NONE', #36829, #49359 ) ;
#43118 = CIRCLE ( 'NONE', #31889, 5.000000000000170530 ) ;
#43120 = CARTESIAN_POINT ( 'NONE',  ( -2.645453300864630819E-14, -15.55634918610403616, 85.00100000000000477 ) ) ;
#43121 = CARTESIAN_POINT ( 'NONE',  ( -94.79534239005255358, 29.13842790650045700, -69.90232742285510881 ) ) ;
#43122 = ORIENTED_EDGE ( 'NONE', *, *, #20955, .T. ) ;
#43123 = ORIENTED_EDGE ( 'NONE', *, *, #2276, .T. ) ;
#43124 = CONICAL_SURFACE ( 'NONE', #29636, 65.00000000000000000, 0.7853981633974497223 ) ;
#43125 = DIRECTION ( 'NONE',  ( 1.000000000000000000, 0.000000000000000000, 0.000000000000000000 ) ) ;
#43126 = CARTESIAN_POINT ( 'NONE',  ( 45.39413431650373809, 0.000000000000000000, -5.000000000000000000 ) ) ;
#43127 = CARTESIAN_POINT ( 'NONE',  ( 39.40195752203892710, -170.0000000000000000, 56.75838489642694640 ) ) ;
#43128 = CARTESIAN_POINT ( 'NONE',  ( -51.66904755831212981, -10.55634918610397222, 2.000000000000001776 ) ) ;
#43129 = CARTESIAN_POINT ( 'NONE',  ( 107.9342863085848450, 28.93180871323605174, -77.41840800766151176 ) ) ;
#43130 = CARTESIAN_POINT ( 'NONE',  ( 80.30232379693109124, 17.35837133860831116, 33.17720279973744368 ) ) ;
#43131 = CARTESIAN_POINT ( 'NONE',  ( 10.18313837588858384, 65.86279856773080610, 34.48241795236666718 ) ) ;
#43132 = CIRCLE ( 'NONE', #33065, 5.000000000000004441 ) ;
#43133 = CARTESIAN_POINT ( 'NONE',  ( 46.84154678921878912, 10.51341196666389521, -44.10166628834166147 ) ) ;
#43134 = CARTESIAN_POINT ( 'NONE',  ( 204.6977192012829789, 106.3443248447423315, 71.05227132923315025 ) ) ;
#43135 = EDGE_LOOP ( 'NONE', ( #65035, #20996, #6961, #57541 ) ) ;
#43137 = CARTESIAN_POINT ( 'NONE',  ( -109.5142642360664667, 36.61018064014776741, -17.71775249749087067 ) ) ;
#43136 = AXIS2_PLACEMENT_3D ( 'NONE', #38339, #33432, #12313 ) ;
#43138 = ORIENTED_EDGE ( 'NONE', *, *, #65358, .F. ) ;
#43139 = CARTESIAN_POINT ( 'NONE',  ( -15.32520546926283345, 7.495995523981875408, -42.42519461880208809 ) ) ;
#43140 = VECTOR ( 'NONE', #45361, 1000.000000000000000 ) ;
#43141 = CARTESIAN_POINT ( 'NONE',  ( -81.10316978278179079, 23.26460499017369798, 84.50753759321933956 ) ) ;
#43142 = CARTESIAN_POINT ( 'NONE',  ( 93.08073375333748345, 22.79826000593200774, 60.22361380431165401 ) ) ;
#43143 = CARTESIAN_POINT ( 'NONE',  ( 150.2809931605061990, 52.27058242113236020, -18.93275037951032758 ) ) ;
#43144 = CARTESIAN_POINT ( 'NONE',  ( 32.89501968360929851, 8.663558833820818705, 14.33097644123245828 ) ) ;
#43145 = CARTESIAN_POINT ( 'NONE',  ( -95.20053778133916467, 30.43887292928076960, -71.88691849379360121 ) ) ;
#43146 = CARTESIAN_POINT ( 'NONE',  ( -15.55634918610405748, -15.55634918610400774, 2.000000000000001776 ) ) ;
#43147 = ORIENTED_EDGE ( 'NONE', *, *, #34391, .T. ) ;
#43148 = CARTESIAN_POINT ( 'NONE',  ( 212.1414097338564488, 117.1449328067268993, 89.45312194060214495 ) ) ;
#43149 = DIRECTION ( 'NONE',  ( -9.109522253334613014E-16, -1.000000000000000000, 3.889846672687432470E-31 ) ) ;
#43150 = VERTEX_POINT ( 'NONE', #18919 ) ;
#43151 = PLANE ( 'NONE',  #47456 ) ;
#43152 = FACE_OUTER_BOUND ( 'NONE', #46812, .T. ) ;
#43153 = CARTESIAN_POINT ( 'NONE',  ( -10.23531775138760658, 8.068923942586298637, 3.664519661588847121 ) ) ;
#43154 = CARTESIAN_POINT ( 'NONE',  ( 45.04020069093783007, 10.22779424730543063, -64.99450957612113200 ) ) ;
#43155 = CARTESIAN_POINT ( 'NONE',  ( -2.174378755909792460, 6.588636630831476992, 42.57095561852364085 ) ) ;
#43156 = CARTESIAN_POINT ( 'NONE',  ( 122.2516123306975402, 190.0000000000000000, -91.28179539054376335 ) ) ;
#43157 = CARTESIAN_POINT ( 'NONE',  ( 84.41121179164569810, 19.73587740566237159, 83.72931267887217643 ) ) ;
#43158 = EDGE_LOOP ( 'NONE', ( #56517, #21082, #14630 ) ) ;
#43159 = DIRECTION ( 'NONE',  ( -0.9108602745606092510, -0.4127148655274866518, 6.907644228904597601E-15 ) ) ;
#43160 = CARTESIAN_POINT ( 'NONE',  ( -149.5074843970971017, 65.50121172469319220, 72.56537183036277838 ) ) ;
#43161 = CARTESIAN_POINT ( 'NONE',  ( -131.3154845336013068, 50.16828105866954246, 6.070552893135558570 ) ) ;
#43162 = CARTESIAN_POINT ( 'NONE',  ( -166.7136514167008556, 81.71618216218797670, -46.11898781893540900 ) ) ;
#43163 = EDGE_CURVE ( 'NONE', #7668, #9033, #49955, .T. ) ;
#43164 = CONTEXT_DEPENDENT_SHAPE_REPRESENTATION ( #4053, #43941 ) ;
#43165 = CARTESIAN_POINT ( 'NONE',  ( -180.5628792467297501, 95.81282809867099104, 91.05901154845440715 ) ) ;
#43166 = ORIENTED_EDGE ( 'NONE', *, *, #31987, .T. ) ;
#43167 = CYLINDRICAL_SURFACE ( 'NONE', #16657, 60.00000000000000000 ) ;
#43168 = CARTESIAN_POINT ( 'NONE',  ( -66.47744216009887452, -4.728025614004670807, 34.48241795236666718 ) ) ;
#43169 = ADVANCED_FACE ( 'NONE', ( #45651 ), #40706, .F. ) ;
#43170 = CARTESIAN_POINT ( 'NONE',  ( -156.8688717293649972, 70.68369417233287777, 93.38775103858958460 ) ) ;
#43171 = EDGE_CURVE ( 'NONE', #37385, #63094, #50576, .T. ) ;
#43172 = B_SPLINE_CURVE_WITH_KNOTS ( 'NONE', 3,
 ( #16980, #10665, #65185, #38450, #53572, #113, #11709, #53911, #6079, #6784, #49681, #59539, #21916, #5402, #11357, #27539, #32134, #21568, #5734, #27190, #59887, #48622, #64839, #48979, #6445, #60251, #43011, #64489, #16301, #37749, #59196, #12070, #33539, #32478, #54967, #32825, #466, #54253, #7502, #45460, #66942, #60947, #17699, #8536 ),
 .UNSPECIFIED., .F., .F.,
 ( 4, 2, 2, 2, 2, 2, 2, 2, 2, 2, 2, 2, 2, 2, 2, 2, 2, 2, 2, 2, 2, 4 ),
 ( 0.000000000000000000, 0.001488594467279787332, 0.002232891700919671998, 0.002977188934559557316, 0.004465783401839307568, 0.005954377869119058253, 0.007442972336398808071, 0.008187269570038688618, 0.008931566803678568298, 0.01042016127095831204, 0.01190875573823805232, 0.01265305297187791292, 0.01339735020551777699, 0.01488594467279747389, 0.01563024190643732408, 0.01637453914007717254, 0.01786313360735686598, 0.01935172807463656636, 0.02009602530827640440, 0.02084032254191624939, 0.02232891700919594283, 0.02381751147647563974 ),
 .UNSPECIFIED. ) ;
#43173 = CARTESIAN_POINT ( 'NONE',  ( 134.3159642998340644, 41.70198410084979201, 29.51034083899532590 ) ) ;
#43174 = EDGE_LOOP ( 'NONE', ( #46966, #50218, #54926, #5803 ) ) ;
#43175 = CARTESIAN_POINT ( 'NONE',  ( 0.3173508448886570021, -5.375634714784626844, 6.689127551062011179 ) ) ;
#43176 = CARTESIAN_POINT ( 'NONE',  ( 79.91920957766411959, 18.29292522273509647, 13.75549202193108833 ) ) ;
#43177 = CARTESIAN_POINT ( 'NONE',  ( 164.8914542114683570, 64.97670918603526502, 8.943675762355397296 ) ) ;
#43178 = EDGE_CURVE ( 'NONE', #31575, #67718, #6161, .T. ) ;
#43179 = CYLINDRICAL_SURFACE ( 'NONE', #3852, 65.36598343705435354 ) ;
#43180 = ORIENTED_EDGE ( 'NONE', *, *, #47563, .F. ) ;
#43181 = VECTOR ( 'NONE', #32610, 1000.000000000000114 ) ;
#43182 = DIRECTION ( 'NONE',  ( -0.000000000000000000, -0.000000000000000000, -1.000000000000000000 ) ) ;
#43183 = AXIS2_PLACEMENT_3D ( 'NONE', #28940, #806, #60239 ) ;
#43184 = ORIENTED_EDGE ( 'NONE', *, *, #64969, .F. ) ;
#43185 = CARTESIAN_POINT ( 'NONE',  ( -72.21652659655759976, 19.96855882996550235, -19.63090997373414481 ) ) ;
#43186 = EDGE_CURVE ( 'NONE', #10198, #69476, #9402, .T. ) ;
#43187 = DIRECTION ( 'NONE',  ( 0.000000000000000000, 0.000000000000000000, -1.000000000000000000 ) ) ;
#43189 = ORIENTED_EDGE ( 'NONE', *, *, #44417, .T. ) ;
#43188 = CARTESIAN_POINT ( 'NONE',  ( 150.0516754638055943, 53.34587188591231666, 8.929522449978659182 ) ) ;
#43190 = CARTESIAN_POINT ( 'NONE',  ( 163.1495034066983862, 62.20479872133083177, 41.83434947820244787 ) ) ;
#43191 = CARTESIAN_POINT ( 'NONE',  ( 13.24564585880132839, -63.65041531508827433, 43.58025477438756923 ) ) ;
#43192 = CARTESIAN_POINT ( 'NONE',  ( 0.000000000000000000, 192.0000000000000000, 0.000000000000000000 ) ) ;
#43193 = ORIENTED_EDGE ( 'NONE', *, *, #54046, .F. ) ;
#43194 = CARTESIAN_POINT ( 'NONE',  ( -51.66904755831210139, 5.000000000000066613, 85.00100000000000477 ) ) ;
#43195 = CARTESIAN_POINT ( 'NONE',  ( -31.43908319763710679, 9.591432048623756756, -8.472646774738153752 ) ) ;
#43196 = CARTESIAN_POINT ( 'NONE',  ( -180.4614954900548298, 97.28277348252828460, 36.75295334209538112 ) ) ;
#43197 = CARTESIAN_POINT ( 'NONE',  ( 140.0012045870120687, 46.45892655944614091, 94.99999999999866418 ) ) ;
#43198 = EDGE_LOOP ( 'NONE', ( #5861, #65959, #67196, #65125 ) ) ;
#43199 = ORIENTED_EDGE ( 'NONE', *, *, #23843, .T. ) ;
#43200 = ORIENTED_EDGE ( 'NONE', *, *, #3335, .T. ) ;
#43201 =( NAMED_UNIT ( * ) PLANE_ANGLE_UNIT ( ) SI_UNIT ( $, .RADIAN. ) );
#43202 = CARTESIAN_POINT ( 'NONE',  ( 149.0250918491436778, 6.000000000000000000, -14.43565316649551811 ) ) ;
#43203 =( NAMED_UNIT ( * ) PLANE_ANGLE_UNIT ( ) SI_UNIT ( $, .RADIAN. ) );
#43204 = CARTESIAN_POINT ( 'NONE',  ( 141.9165763529819344, 242.0000000000000000, 129.0000000000000000 ) ) ;
#43205 = CARTESIAN_POINT ( 'NONE',  ( 70.50670201344738075, 14.53584474203976917, 90.50562999910829376 ) ) ;
#43206 = DIRECTION ( 'NONE',  ( 0.9362348706397369824, 0.3513748240813435175, 0.000000000000000000 ) ) ;
#43207 = CARTESIAN_POINT ( 'NONE',  ( -55.05276343752909440, 15.72344139423348430, -50.21632399845989170 ) ) ;
#43208 = DIRECTION ( 'NONE',  ( 0.000000000000000000, 0.000000000000000000, 1.000000000000000000 ) ) ;
#43209 = VERTEX_POINT ( 'NONE', #42439 ) ;
#43210 = AXIS2_PLACEMENT_3D ( 'NONE', #58871, #43387, #839 ) ;
#43211 = DIRECTION ( 'NONE',  ( -0.000000000000000000, -0.000000000000000000, -1.000000000000000000 ) ) ;
#43212 = ORIENTED_EDGE ( 'NONE', *, *, #25901, .F. ) ;
#43213 = DIRECTION ( 'NONE',  ( 1.000000000000000000, 0.000000000000000000, -1.697894969632810155E-16 ) ) ;
#43214 = CARTESIAN_POINT ( 'NONE',  ( 188.0081045302011944, 85.89855126821618114, 33.91234789090425039 ) ) ;
#43215 = CARTESIAN_POINT ( 'NONE',  ( -417.6627218934913230, 399.9999999999998295, 113.5502958579882602 ) ) ;
#43217 = CARTESIAN_POINT ( 'NONE',  ( -71.43874587651171737, 19.69883891272895227, 9.055200870754841702 ) ) ;
#43216 = VECTOR ( 'NONE', #17618, 1000.000000000000000 ) ;
#43218 = CARTESIAN_POINT ( 'NONE',  ( -123.0348077379026392, 45.83489305753317922, 71.90199806622466383 ) ) ;
#43219 = DIRECTION ( 'NONE',  ( 0.000000000000000000, 0.000000000000000000, 1.000000000000000000 ) ) ;
#43220 = CARTESIAN_POINT ( 'NONE',  ( 447.3372781065085064, 365.0000000000043769, 113.5502958579838122 ) ) ;
#43222 = CARTESIAN_POINT ( 'NONE',  ( -17.50000000000000000, -17.50000000000000000, 0.000000000000000000 ) ) ;
#43221 = VECTOR ( 'NONE', #13562, 1000.000000000000000 ) ;
#43223 = VECTOR ( 'NONE', #64110, 1000.000000000000000 ) ;
#43224 = EDGE_LOOP ( 'NONE', ( #31538, #18923, #62872, #44785 ) ) ;
#43225 = EDGE_CURVE ( 'NONE', #32511, #20457, #63213, .T. ) ;
#43226 = CYLINDRICAL_SURFACE ( 'NONE', #38735, 10.00000000000000000 ) ;
#43227 = CARTESIAN_POINT ( 'NONE',  ( 154.4165763529819628, -26.99999999999998224, 129.0000000000000000 ) ) ;
#43228 = ORIENTED_EDGE ( 'NONE', *, *, #58649, .T. ) ;
#43229 = ORIENTED_EDGE ( 'NONE', *, *, #15435, .T. ) ;
#43230 = CARTESIAN_POINT ( 'NONE',  ( -439.4229916354184979, 388.0000000000064801, -128.9497041420121093 ) ) ;
#43231 = CIRCLE ( 'NONE', #5033, 75.31295361348099959 ) ;
#43232 = CARTESIAN_POINT ( 'NONE',  ( 149.0250918491436778, 6.000000000000000000, -9.435653166495526989 ) ) ;
#43233 = CARTESIAN_POINT ( 'NONE',  ( 39.88975917505624835, 9.487965272711656795, 29.91383430596323834 ) ) ;
#43234 = CARTESIAN_POINT ( 'NONE',  ( 112.3013380801408658, 400.0000000000066507, -133.9497041420121377 ) ) ;
#43235 = VECTOR ( 'NONE', #36551, 1000.000000000000000 ) ;
#43236 = CARTESIAN_POINT ( 'NONE',  ( -145.9095871962850310, 61.18682730038537443, 17.96100122531099075 ) ) ;
#43237 = ORIENTED_EDGE ( 'NONE', *, *, #4786, .T. ) ;
#43238 = EDGE_LOOP ( 'NONE', ( #33428, #637 ) ) ;
#43239 = CARTESIAN_POINT ( 'NONE',  ( -132.5976199670998881, 52.30296609017644016, 34.74704912185334393 ) ) ;
#43240 = ORIENTED_EDGE ( 'NONE', *, *, #20232, .F. ) ;
#43241 = CARTESIAN_POINT ( 'NONE',  ( -166.2425995121691642, -170.0000000000000000, 94.99999999999866418 ) ) ;
#43242 = CARTESIAN_POINT ( 'NONE',  ( -439.4229916354184979, 400.0000000000065370, -133.9497041420121377 ) ) ;
#43243 = CARTESIAN_POINT ( 'NONE',  ( 61.10129719786242219, 12.23677173834304810, 71.41316413118165940 ) ) ;
#43244 = CARTESIAN_POINT ( 'NONE',  ( -7.330587818645181386, 7.867004275019543691, 71.96013162991091860 ) ) ;
#43245 = EDGE_CURVE ( 'NONE', #24506, #18617, #34730, .T. ) ;
#43246 = CARTESIAN_POINT ( 'NONE',  ( 437.3372781065085633, 394.9999999999999432, 103.5502958579882460 ) ) ;
#43247 = DIRECTION ( 'NONE',  ( 1.940875045995544638E-32, -1.110223024625156171E-16, 1.000000000000000000 ) ) ;
#43248 = VERTEX_POINT ( 'NONE', #47703 ) ;
#43249 = ORIENTED_EDGE ( 'NONE', *, *, #16205, .F. ) ;
#43250 = CARTESIAN_POINT ( 'NONE',  ( -3.319543390096042490, 7.321065037175422674, -0.01688885742776483068 ) ) ;
#43251 = CARTESIAN_POINT ( 'NONE',  ( -4.164416015345870470, 64.86646004871185767, 133.5802547743875550 ) ) ;
#43252 = PLANE ( 'NONE',  #26288 ) ;
#43253 = CARTESIAN_POINT ( 'NONE',  ( 135.4423125506058625, 42.39015362494583883, -77.70187412784397907 ) ) ;
#43254 = EDGE_CURVE ( 'NONE', #3570, #54048, #69164, .T. ) ;
#43255 = CARTESIAN_POINT ( 'NONE',  ( 69.73342236697678231, 14.33173522011652778, 33.94168038989159442 ) ) ;
#43256 = ORIENTED_EDGE ( 'NONE', *, *, #12616, .F. ) ;
#43257 = CARTESIAN_POINT ( 'NONE',  ( 79.11678589158262298, 16.99307320450158443, 10.37612617437139662 ) ) ;
#43258 = VERTEX_POINT ( 'NONE', #38547 ) ;
#43259 = CARTESIAN_POINT ( 'NONE',  ( -73.09185868250597196, 20.27574131633383558, 42.95950369064131280 ) ) ;
#43260 = VERTEX_POINT ( 'NONE', #44527 ) ;
#43261 = AXIS2_PLACEMENT_3D ( 'NONE', #67211, #2821, #52047 ) ;
#43262 = ADVANCED_FACE ( 'NONE', ( #54719 ), #27990, .F. ) ;
#43263 = CIRCLE ( 'NONE', #10745, 5.000000000000004441 ) ;
#43264 = ORIENTED_EDGE ( 'NONE', *, *, #40726, .F. ) ;
#43265 = CARTESIAN_POINT ( 'NONE',  ( 8.000000000000003553, -4.618802153517020948, -0.7145311798163346273 ) ) ;
#43266 = ADVANCED_FACE ( 'NONE', ( #26948 ), #64943, .T. ) ;
#43268 = EDGE_CURVE ( 'NONE', #63745, #52584, #41446, .T. ) ;
#43267 = CARTESIAN_POINT ( 'NONE',  ( 90.30166390191403991, 20.70652093100729019, 3.810012513778408216 ) ) ;
#43269 = PLANE ( 'NONE',  #54115 ) ;
#43270 = CIRCLE ( 'NONE', #56763, 22.00000000000000355 ) ;
#43271 = AXIS2_PLACEMENT_3D ( 'NONE', #61359, #45176, #23398 ) ;
#43272 = ORIENTED_EDGE ( 'NONE', *, *, #9138, .F. ) ;
#43273 = AXIS2_PLACEMENT_3D ( 'NONE', #39375, #61179, #18269 ) ;
#43274 = CARTESIAN_POINT ( 'NONE',  ( 290.0000000000000568, -5.000000000000000888, 18.50000000000000000 ) ) ;
#43275 = AXIS2_PLACEMENT_3D ( 'NONE', #27546, #48986, #60953 ) ;
#43276 = CARTESIAN_POINT ( 'NONE',  ( 151.7956716830626362, 53.36999433148312733, 41.81961525401386126 ) ) ;
#43277 = AXIS2_PLACEMENT_3D ( 'NONE', #47519, #48545, #9917 ) ;
#43278 = CARTESIAN_POINT ( 'NONE',  ( 67.93154431625913503, 14.90489441944787430, 31.62713259101203178 ) ) ;
#43279 = CYLINDRICAL_SURFACE ( 'NONE', #29154, 4.999999999999997335 ) ;
#43280 = CARTESIAN_POINT ( 'NONE',  ( 31.71171429570986788, 10.56647038281439954, 6.893343212288932875 ) ) ;
#43281 = DIRECTION ( 'NONE',  ( 0.000000000000000000, 0.000000000000000000, 1.000000000000000000 ) ) ;
#43282 = CARTESIAN_POINT ( 'NONE',  ( 134.3182571105338923, 42.88121222759018991, -62.86786152285935003 ) ) ;
#43283 = LINE ( 'NONE', #12340, #10753 ) ;
#43284 = ORIENTED_EDGE ( 'NONE', *, *, #60610, .T. ) ;
#43285 = FACE_BOUND ( 'NONE', #45208, .T. ) ;
#43286 = CARTESIAN_POINT ( 'NONE',  ( -0.8011128725815451768, 6.535315321814158196, -67.12254502563429526 ) ) ;
#43287 = CARTESIAN_POINT ( 'NONE',  ( -178.5848962563133568, 94.99295350784007042, 70.32832319493537909 ) ) ;
#43288 = CARTESIAN_POINT ( 'NONE',  ( 113.9884483999549047, 30.65255989963792160, -90.56438067049403173 ) ) ;
#43289 = CARTESIAN_POINT ( 'NONE',  ( -124.9915686518654780, 47.10215472274616388, -34.91370389823391918 ) ) ;
#43290 = CARTESIAN_POINT ( 'NONE',  ( -84.55783695959765112, 25.74181993349144548, 15.74135957251160001 ) ) ;
#43291 = CARTESIAN_POINT ( 'NONE',  ( 133.3990214534117058, 41.14886683286417224, 2.676281182479414156 ) ) ;
#43292 = CARTESIAN_POINT ( 'NONE',  ( 412.0000000000000000, 0.000000000000000000, -0.000000000000000000 ) ) ;
#43293 = CARTESIAN_POINT ( 'NONE',  ( -73.58753291667264307, 20.45143618612268455, -90.76877822284814101 ) ) ;
#43294 = CARTESIAN_POINT ( 'NONE',  ( 65.40032188136231639, 13.23841673691966925, 3.353476667165713465 ) ) ;
#43295 = LINE ( 'NONE', #37002, #9561 ) ;
#43296 = CARTESIAN_POINT ( 'NONE',  ( 93.43270425363543552, 22.93046121381056324, -19.64350642960366855 ) ) ;
#43297 = ORIENTED_EDGE ( 'NONE', *, *, #11514, .F. ) ;
#43298 = FACE_OUTER_BOUND ( 'NONE', #12239, .T. ) ;
#43299 = ORIENTED_EDGE ( 'NONE', *, *, #62319, .F. ) ;
#43300 = CARTESIAN_POINT ( 'NONE',  ( 108.3906473026529937, 28.03385344351494624, -62.98435907625002272 ) ) ;
#43301 = VERTEX_POINT ( 'NONE', #59302 ) ;
#43302 = B_SPLINE_CURVE_WITH_KNOTS ( 'NONE', 3,
 ( #65594, #65957, #59943, #29342, #17756, #39211, #12470, #33934, #50104, #1934, #66312, #18099, #12829, #34284, #55732, #7554, #29013, #35313 ),
 .UNSPECIFIED., .F., .F.,
 ( 4, 2, 2, 2, 2, 2, 2, 2, 4 ),
 ( 9.309503074677274191E-17, 0.002090076166982583316, 0.003135114250473834858, 0.003657633292219452607, 0.004180152333965070355, 0.005225190417456297177, 0.006270228500947524868, 0.007315266584438751690, 0.008360304667929979380 ),
 .UNSPECIFIED. ) ;
#43303 = CARTESIAN_POINT ( 'NONE',  ( 29.86848256228521237, 58.14280299503739258, 43.58025477438756212 ) ) ;
#43304 = CARTESIAN_POINT ( 'NONE',  ( 107.7683756309525336, 28.85711661752776180, 83.71285356453704196 ) ) ;
#43305 = CARTESIAN_POINT ( 'NONE',  ( -145.3246383987844581, 62.00818849034184410, 58.83565616930072650 ) ) ;
#43306 = CARTESIAN_POINT ( 'NONE',  ( 86.62931800182293784, -170.0000000000000000, -35.82156419891171595 ) ) ;
#43307 = CARTESIAN_POINT ( 'NONE',  ( -24.60892750534351237, 9.584951112520231575, -45.92522378588709842 ) ) ;
#43308 = PRODUCT_DEFINITION_SHAPE ( 'NONE', 'NONE',  #69612 ) ;
#43309 = CARTESIAN_POINT ( 'NONE',  ( -47.56466076048273095, 13.83435953640667826, -70.05170999023415845 ) ) ;
#43310 = EDGE_CURVE ( 'NONE', #48257, #55132, #43463, .T. ) ;
#43311 = CARTESIAN_POINT ( 'NONE',  ( 46.66904755831207297, -15.55634918610412853, 85.00100000000000477 ) ) ;
#43312 = CARTESIAN_POINT ( 'NONE',  ( -123.6618353044034535, 46.23845779494348562, -22.74412515443657767 ) ) ;
#43313 = ORIENTED_EDGE ( 'NONE', *, *, #17240, .T. ) ;
#43314 = ORIENTED_EDGE ( 'NONE', *, *, #37008, .T. ) ;
#43315 = CARTESIAN_POINT ( 'NONE',  ( 32.09610685027467269, 8.582590950734816815, 62.54528762178141221 ) ) ;
#43316 = EDGE_CURVE ( 'NONE', #11641, #49852, #5832, .T. ) ;
#43317 = AXIS2_PLACEMENT_3D ( 'NONE', #16312, #15967, #6094 ) ;
#43318 = CARTESIAN_POINT ( 'NONE',  ( -166.7050147108374460, 81.70694330787519277, 69.08965843878142721 ) ) ;
#43319 = CARTESIAN_POINT ( 'NONE',  ( 130.9157159354502369, 40.84309122054532537, -90.30233232517586828 ) ) ;
#43320 = VECTOR ( 'NONE', #58629, 1000.000000000000000 ) ;
#43321 = CARTESIAN_POINT ( 'NONE',  ( 427.4999999999999432, -18.06806526123148160, 380.0000000000000000 ) ) ;
#43322 = ORIENTED_EDGE ( 'NONE', *, *, #15075, .F. ) ;
#43323 = CARTESIAN_POINT ( 'NONE',  ( 283.9761838721219078, 21.78940454476515853, 3.049139182071509691 ) ) ;
#43324 = VECTOR ( 'NONE', #60030, 1000.000000000000000 ) ;
#43325 = AXIS2_PLACEMENT_3D ( 'NONE', #4680, #26146, #24770 ) ;
#43326 = CARTESIAN_POINT ( 'NONE',  ( 187.5246323291927126, 86.86207184872515086, -12.99861875644394971 ) ) ;
#43327 = DIRECTION ( 'NONE',  ( 0.000000000000000000, -1.000000000000000000, 0.000000000000000000 ) ) ;
#43328 = CARTESIAN_POINT ( 'NONE',  ( 99.99999999999997158, 0.000000000000000000, -25.00000000000000000 ) ) ;
#43329 = CARTESIAN_POINT ( 'NONE',  ( 39.88971011078924533, 8.472992116645418292, -23.77526687496409252 ) ) ;
#43330 = CYLINDRICAL_SURFACE ( 'NONE', #6123, 7.500000000000013323 ) ;
#43331 = CARTESIAN_POINT ( 'NONE',  ( -442.6627218934912662, 394.9999999999998295, 113.5502958579882034 ) ) ;
#43332 = PRODUCT_DEFINITION_FORMATION_WITH_SPECIFIED_SOURCE ( 'ANY', '', #56359, .NOT_KNOWN. ) ;
#43333 = EDGE_CURVE ( 'NONE', #25277, #60956, #9553, .T. ) ;
#43334 = CARTESIAN_POINT ( 'NONE',  ( 164.9540180502650912, 65.02981548735056094, 64.32247932210420061 ) ) ;
#43335 = AXIS2_PLACEMENT_3D ( 'NONE', #3516, #14072, #46419 ) ;
#43336 = EDGE_CURVE ( 'NONE', #3776, #62313, #62370, .T. ) ;
#43337 = CONICAL_SURFACE ( 'NONE', #15292, 65.00000000000000000, 0.7853981633974497223 ) ;
#43338 = ADVANCED_FACE ( 'NONE', ( #8641 ), #27450, .T. ) ;
#43339 = ORIENTED_EDGE ( 'NONE', *, *, #56385, .T. ) ;
#43340 = CARTESIAN_POINT ( 'NONE',  ( 26.11269837220800127, -31.11269837220812562, 2.000000000000001776 ) ) ;
#43341 = CARTESIAN_POINT ( 'NONE',  ( 93.72059824125564376, 23.03897520779758423, -40.82895870122177939 ) ) ;
#43342 = CARTESIAN_POINT ( 'NONE',  ( -54.57263979903870421, 15.59415114099630983, 57.16187836339484107 ) ) ;
#43343 = CARTESIAN_POINT ( 'NONE',  ( -440.1146514826278349, 400.0000000000021032, 101.0022254471289358 ) ) ;
#43344 = EDGE_CURVE ( 'NONE', #54626, #48794, #38063, .T. ) ;
#43345 = CARTESIAN_POINT ( 'NONE',  ( -7.825402957745087207, -170.0000000000000000, -16.07352014148014163 ) ) ;
#43346 = CARTESIAN_POINT ( 'NONE',  ( -12.63148932007802472, 8.261552044977213072, 85.53769020324797623 ) ) ;
#43347 = ORIENTED_EDGE ( 'NONE', *, *, #53818, .T. ) ;
#43348 = CARTESIAN_POINT ( 'NONE',  ( 56.19211641164837090, 11.19288081156168246, 7.345765177167212556 ) ) ;
#43349 = CARTESIAN_POINT ( 'NONE',  ( -51.66904755831210139, 5.000000000000066613, 0.000000000000000000 ) ) ;
#43350 = ORIENTED_EDGE ( 'NONE', *, *, #1876, .F. ) ;
#43351 = ORIENTED_EDGE ( 'NONE', *, *, #58508, .T. ) ;
#43352 = DIRECTION ( 'NONE',  ( -0.9362348706397369824, -0.3513748240813435175, 0.000000000000000000 ) ) ;
#43353 = DIRECTION ( 'NONE',  ( 0.000000000000000000, 1.000000000000000000, -0.000000000000000000 ) ) ;
#43354 = CARTESIAN_POINT ( 'NONE',  ( 103.9652201950894437, 26.08439499369982428, 41.22229790462832000 ) ) ;
#43356 = ORIENTED_EDGE ( 'NONE', *, *, #23118, .F. ) ;
#43355 = EDGE_CURVE ( 'NONE', #989, #58090, #20742, .T. ) ;
#43357 = CARTESIAN_POINT ( 'NONE',  ( -57.42615654242916889, 15.33060010148602892, -62.44219422609327808 ) ) ;
#43358 = CARTESIAN_POINT ( 'NONE',  ( -2.873329055852804625, 7.626065826870669362, 5.116632491166936525 ) ) ;
#43359 = EDGE_CURVE ( 'NONE', #41874, #26400, #68415, .T. ) ;
#43361 = EDGE_CURVE ( 'NONE', #51605, #34064, #60046, .T. ) ;
#43360 = CARTESIAN_POINT ( 'NONE',  ( 180.2494929075577943, 79.18888319146950039, -36.22505766587960352 ) ) ;
#43362 = CARTESIAN_POINT ( 'NONE',  ( 164.2665160441432874, 63.13418342263689453, 93.79059897813883140 ) ) ;
#43363 = FACE_OUTER_BOUND ( 'NONE', #25776, .T. ) ;
#43364 = CARTESIAN_POINT ( 'NONE',  ( -31.11269837220809364, -10.55634918610397932, 2.000000000000001776 ) ) ;
#43365 = PRODUCT ( 'bearing', 'bearing', '', ( #19921 ) ) ;
#43366 = ORIENTED_EDGE ( 'NONE', *, *, #58511, .F. ) ;
#43367 = CARTESIAN_POINT ( 'NONE',  ( 106.4072861358878299, 28.24787347451998798, -10.12839677197858812 ) ) ;
#43368 = VECTOR ( 'NONE', #35885, 1000.000000000000000 ) ;
#43369 = DIRECTION ( 'NONE',  ( -0.3930250316539278255, 0.9195277725514487965, 0.000000000000000000 ) ) ;
#43370 = CARTESIAN_POINT ( 'NONE',  ( -29.03891846981456126, 10.22741474064059020, 30.59402320536396402 ) ) ;
#43371 = CARTESIAN_POINT ( 'NONE',  ( 3.000000000000002665, 3.043247295881173007E-15, 24.69999999999999929 ) ) ;
#43372 = CARTESIAN_POINT ( 'NONE',  ( 79.68455349783286579, 17.16711484584623904, 93.81489682416450648 ) ) ;
#43373 = VECTOR ( 'NONE', #11663, 1000.000000000000000 ) ;
#43375 = ORIENTED_EDGE ( 'NONE', *, *, #35171, .T. ) ;
#43374 = CYLINDRICAL_SURFACE ( 'NONE', #19706, 7.500000000000013323 ) ;
#43376 = ORIENTED_EDGE ( 'NONE', *, *, #9993, .T. ) ;
#43377 = CONICAL_SURFACE ( 'NONE', #33318, 74.95140232871122521, 0.8777644062502172329 ) ;
#43378 = VERTEX_POINT ( 'NONE', #10014 ) ;
#43379 = DIRECTION ( 'NONE',  ( 0.000000000000000000, 1.000000000000000000, 0.000000000000000000 ) ) ;
#43380 = CARTESIAN_POINT ( 'NONE',  ( -53.13004807512038496, 14.17398740785106526, 45.08299798962536187 ) ) ;
#43381 = CARTESIAN_POINT ( 'NONE',  ( -55.05276343752909440, 14.68156374112638929, -23.37177340799619785 ) ) ;
#43382 = DIRECTION ( 'NONE',  ( 0.000000000000000000, 0.000000000000000000, 1.000000000000000000 ) ) ;
#43383 = CARTESIAN_POINT ( 'NONE',  ( 0.000000000000000000, 0.000000000000000000, 41.38025477438755928 ) ) ;
#43384 = CARTESIAN_POINT ( 'NONE',  ( -55.05276343752909440, 15.72344139423348430, -50.21632399845989170 ) ) ;
#43385 = CARTESIAN_POINT ( 'NONE',  ( -14.56631729561072675, 8.434645566888200108, -12.74894963134235049 ) ) ;
#43386 = PLANE ( 'NONE',  #27517 ) ;
#43387 = DIRECTION ( 'NONE',  ( 0.5773502691896258421, 0.5773502691896258421, 0.5773502691896258421 ) ) ;
#43388 = ORIENTED_EDGE ( 'NONE', *, *, #22305, .T. ) ;
#43389 = AXIS2_PLACEMENT_3D ( 'NONE', #47045, #5171, #26289 ) ;
#43390 = DIRECTION ( 'NONE',  ( 0.000000000000000000, -1.000000000000000000, 0.000000000000000000 ) ) ;
#43391 = ORIENTED_EDGE ( 'NONE', *, *, #25685, .F. ) ;
#43392 = VERTEX_POINT ( 'NONE', #26534 ) ;
#43393 = CARTESIAN_POINT ( 'NONE',  ( 63.01563776193090405, 13.70579113808098093, -8.876140241706053757 ) ) ;
#43394 = CARTESIAN_POINT ( 'NONE',  ( -57.96271610907653837, 16.52641986079314762, -89.48962646049473335 ) ) ;
#43395 = CARTESIAN_POINT ( 'NONE',  ( -62.41990535723909517, 17.83270318706536983, -95.00000000000133582 ) ) ;
#43396 = CARTESIAN_POINT ( 'NONE',  ( 110.7167338301703978, 30.21148223254618870, -9.077886975190001095 ) ) ;
#43397 = CARTESIAN_POINT ( 'NONE',  ( -108.0980548770428271, 35.83569586822709141, 15.93332971359382988 ) ) ;
#43398 = DIRECTION ( 'NONE',  ( 0.000000000000000000, 0.5000000000000013323, 0.8660254037844379305 ) ) ;
#43399 = DIRECTION ( 'NONE',  ( -0.000000000000000000, 1.000000000000000000, -0.000000000000000000 ) ) ;
#43400 = ORIENTED_EDGE ( 'NONE', *, *, #68025, .T. ) ;
#43401 = ORIENTED_EDGE ( 'NONE', *, *, #67988, .T. ) ;
#43402 = VERTEX_POINT ( 'NONE', #69074 ) ;
#43403 = ADVANCED_FACE ( 'NONE', ( #4723 ), #62790, .T. ) ;
#43404 = CARTESIAN_POINT ( 'NONE',  ( -155.7455325080990747, 71.01834415181986060, -11.29636591650952582 ) ) ;
#43405 = CARTESIAN_POINT ( 'NONE',  ( 89.73102809687581782, 21.57092797140214557, -90.17038539412145326 ) ) ;
#43406 = CARTESIAN_POINT ( 'NONE',  ( -34.74740905761647269, 10.15745573515589406, 71.30966891704866839 ) ) ;
#43407 = CARTESIAN_POINT ( 'NONE',  ( -153.6931187576189757, 67.81270084382354923, -21.69602582841185878 ) ) ;
#43408 = VERTEX_POINT ( 'NONE', #30781 ) ;
#43409 = CARTESIAN_POINT ( 'NONE',  ( 185.5412249395996582, 84.70425786166002524, 57.61695868165770662 ) ) ;
#43410 = CARTESIAN_POINT ( 'NONE',  ( -156.1462053606562961, 70.02140399657017156, 68.56529437304638464 ) ) ;
#43411 = CARTESIAN_POINT ( 'NONE',  ( 100.0000000000000284, 0.000000000000000000, 0.000000000000000000 ) ) ;
#43412 = PRESENTATION_STYLE_ASSIGNMENT (( #37802 ) ) ;
#43413 = CARTESIAN_POINT ( 'NONE',  ( 126.6904219525097659, 38.41566710102375737, -95.00000000000133582 ) ) ;
#43414 = DIRECTION ( 'NONE',  ( 1.000000000000000000, 0.000000000000000000, 0.000000000000000000 ) ) ;
#43415 = DIRECTION ( 'NONE',  ( 1.387778780781445922E-16, -1.000000000000000000, -1.232595164407830946E-32 ) ) ;
#43416 = ADVANCED_FACE ( 'NONE', ( #3691 ), #36056, .F. ) ;
#43417 = DIRECTION ( 'NONE',  ( -0.000000000000000000, -0.000000000000000000, -1.000000000000000000 ) ) ;
#43418 = CARTESIAN_POINT ( 'NONE',  ( 15.78827728214693416, 6.500811158483284835, -77.36349468914950478 ) ) ;
#43419 = ADVANCED_FACE ( 'NONE', ( #46952 ), #31466, .F. ) ;
#43420 = ORIENTED_EDGE ( 'NONE', *, *, #14616, .T. ) ;
#43421 = CARTESIAN_POINT ( 'NONE',  ( -8.000000000000000000, 4.618802153516996079, -0.7145311798163263006 ) ) ;
#43422 = CONTEXT_DEPENDENT_SHAPE_REPRESENTATION ( #11212, #28836 ) ;
#43423 = DIRECTION ( 'NONE',  ( 0.000000000000000000, 0.000000000000000000, 1.000000000000000000 ) ) ;
#43424 = CARTESIAN_POINT ( 'NONE',  ( -133.2698123908828620, 51.54642138335022850, -41.02960792264190104 ) ) ;
#43425 = CARTESIAN_POINT ( 'NONE',  ( 4.165045035620146940, 64.88046627338042072, 43.58025477438756923 ) ) ;
#43426 = CARTESIAN_POINT ( 'NONE',  ( 56.52205390515080552, 12.28646189164057745, -66.28031366309063799 ) ) ;
#43427 = EDGE_LOOP ( 'NONE', ( #38794, #66431, #21915, #29094 ) ) ;
#43428 = VECTOR ( 'NONE', #54596, 1000.000000000000000 ) ;
#43429 = DIRECTION ( 'NONE',  ( 0.000000000000000000, -0.000000000000000000, 1.000000000000000000 ) ) ;
#43430 = ORIENTED_EDGE ( 'NONE', *, *, #1666, .F. ) ;
#43431 = CARTESIAN_POINT ( 'NONE',  ( -24.32937228292060539, 8.531905774118438757, -18.41076230671387037 ) ) ;
#43432 = CARTESIAN_POINT ( 'NONE',  ( 185.0770371948367199, 82.73585087248531522, 84.12142509379798128 ) ) ;
#43433 = VERTEX_POINT ( 'NONE', #21251 ) ;
#43434 = VECTOR ( 'NONE', #49542, 1000.000000000000000 ) ;
#43435 = ORIENTED_EDGE ( 'NONE', *, *, #56326, .F. ) ;
#43436 = CARTESIAN_POINT ( 'NONE',  ( 186.5979919519638486, 85.84756789133375321, 41.89830629180269739 ) ) ;
#43437 = DIRECTION ( 'NONE',  ( 0.000000000000000000, 0.000000000000000000, -1.000000000000000000 ) ) ;
#43438 = VERTEX_POINT ( 'NONE', #15633 ) ;
#43439 = CARTESIAN_POINT ( 'NONE',  ( 116.5100763992442836, 33.01539745157281658, 68.08308399614098505 ) ) ;
#43440 = CARTESIAN_POINT ( 'NONE',  ( -56.28348399776044175, 22.91216519805206531, -30.77441063284156897 ) ) ;
#43441 = DIRECTION ( 'NONE',  ( 0.000000000000000000, 1.000000000000000000, 0.000000000000000000 ) ) ;
#43442 = EDGE_CURVE ( 'NONE', #60938, #67479, #52902, .T. ) ;
#43443 = CARTESIAN_POINT ( 'NONE',  ( 164.4645769411267793, 63.30014054308799842, -94.56787564473663110 ) ) ;
#43444 = CARTESIAN_POINT ( 'NONE',  ( 311.9732115134679020, 2.000000000000000000, -151.4173343409194672 ) ) ;
#43445 = CARTESIAN_POINT ( 'NONE',  ( -47.60266343315662851, 13.84328785304053078, -14.87255105764826446 ) ) ;
#43446 = EDGE_CURVE ( 'NONE', #25227, #37904, #10343, .T. ) ;
#43447 = ORIENTED_EDGE ( 'NONE', *, *, #67362, .T. ) ;
#43448 = ORIENTED_EDGE ( 'NONE', *, *, #61245, .F. ) ;
#43449 = DIRECTION ( 'NONE',  ( 0.000000000000000000, 0.000000000000000000, 1.000000000000000000 ) ) ;
#43450 = DIRECTION ( 'NONE',  ( -0.8118923937861950435, -0.5838071093367415143, 0.000000000000000000 ) ) ;
#43451 = FACE_OUTER_BOUND ( 'NONE', #54576, .T. ) ;
#43452 = CARTESIAN_POINT ( 'NONE',  ( -166.7050147108374460, 81.70694330787516435, -65.13309451353698876 ) ) ;
#43454 = EDGE_LOOP ( 'NONE', ( #31530, #54291, #39496, #55035 ) ) ;
#43453 = CARTESIAN_POINT ( 'NONE',  ( -146.7345109736526183, 61.86270848728295135, -35.34073819673365335 ) ) ;
#43455 = CARTESIAN_POINT ( 'NONE',  ( 55.14772863908626732, 34.40534879854737227, 170.0000000000000000 ) ) ;
#43456 = ORIENTED_EDGE ( 'NONE', *, *, #4841, .T. ) ;
#43457 = FACE_OUTER_BOUND ( 'NONE', #66786, .T. ) ;
#43458 = VECTOR ( 'NONE', #4515, 1000.000000000000000 ) ;
#43459 = CYLINDRICAL_SURFACE ( 'NONE', #44604, 7.500000000000013323 ) ;
#43460 = CARTESIAN_POINT ( 'NONE',  ( -49.77357484059130854, -41.82599373102874551, 3.061616997868437868E-16 ) ) ;
#43461 = CARTESIAN_POINT ( 'NONE',  ( 79.53408731553403754, 17.12082763744058411, -13.99589305005577877 ) ) ;
#43462 = AXIS2_PLACEMENT_3D ( 'NONE', #4494, #42465, #37528 ) ;
#43463 = LINE ( 'NONE', #11114, #24124 ) ;
#43464 = CYLINDRICAL_SURFACE ( 'NONE', #59500, 7.500000000000013323 ) ;
#43465 = PLANE ( 'NONE',  #34754 ) ;
#43466 = DIRECTION ( 'NONE',  ( 1.000000000000000000, 2.465190328815660250E-32, 0.000000000000000000 ) ) ;
#43467 = ORIENTED_EDGE ( 'NONE', *, *, #40030, .T. ) ;
#43468 = ORIENTED_EDGE ( 'NONE', *, *, #36922, .T. ) ;
#43469 = CIRCLE ( 'NONE', #13228, 74.95140232871122521 ) ;
#43470 = CARTESIAN_POINT ( 'NONE',  ( 46.64694836521739774, 9.462741877720624473, 35.45895907357519405 ) ) ;
#43471 = LINE ( 'NONE', #49089, #62073 ) ;
#43472 = CARTESIAN_POINT ( 'NONE',  ( 209.9518228411288874, 170.0000000000000284, 31.43423095485942298 ) ) ;
#43473 = CYLINDRICAL_SURFACE ( 'NONE', #36276, 2.999999999999999112 ) ;
#43474 = AXIS2_PLACEMENT_3D ( 'NONE', #59282, #27272, #26935 ) ;
#43475 = PRODUCT_DEFINITION ( 'UNKNOWN', '', #4140, #778 ) ;
#43476 = CARTESIAN_POINT ( 'NONE',  ( 212.1669304543881651, 119.0398299474538533, -44.52663591005489963 ) ) ;
#43477 = PLANE ( 'NONE',  #46110 ) ;
#43478 = CIRCLE ( 'NONE', #69304, 25.12245591505646303 ) ;
#43479 = CARTESIAN_POINT ( 'NONE',  ( 67.93154431625912082, 14.90489441944787075, -48.90651918037900003 ) ) ;
#43480 = CARTESIAN_POINT ( 'NONE',  ( -118.8392474096542202, 43.20060570451234838, 35.52071490940999610 ) ) ;
#43481 = DIRECTION ( 'NONE',  ( 0.000000000000000000, 0.000000000000000000, 1.000000000000000000 ) ) ;
#43483 = EDGE_LOOP ( 'NONE', ( #43583, #6062 ) ) ;
#43482 = EDGE_CURVE ( 'NONE', #13178, #64820, #14594, .T. ) ;
#43484 = CARTESIAN_POINT ( 'NONE',  ( -24.18270484670773257, 9.527492911955587118, 12.83203105897101892 ) ) ;
#43485 = ORIENTED_EDGE ( 'NONE', *, *, #25032, .F. ) ;
#43487 = VECTOR ( 'NONE', #28968, 1000.000000000000114 ) ;
#43486 = CARTESIAN_POINT ( 'NONE',  ( -11.14445507968271976, 7.129894202659276203, -49.64817737260776198 ) ) ;
#43488 = EDGE_CURVE ( 'NONE', #13467, #65661, #46597, .T. ) ;
#43489 = CARTESIAN_POINT ( 'NONE',  ( -21.95369412746257254, 11.95973721106814835, 0.000000000000000000 ) ) ;
#43490 = CARTESIAN_POINT ( 'NONE',  ( 93.72059824125561533, 23.03897520779757357, 66.54924366063296759 ) ) ;
#43491 = CARTESIAN_POINT ( 'NONE',  ( 151.3309484205705076, 53.03078371058071383, -12.46437990871518409 ) ) ;
#43492 = DIRECTION ( 'NONE',  ( 0.000000000000000000, 0.000000000000000000, 1.000000000000000000 ) ) ;
#43493 = CARTESIAN_POINT ( 'NONE',  ( -94.78138776532239262, 30.24234841992714706, -68.82308172911717747 ) ) ;
#43494 = CARTESIAN_POINT ( 'NONE',  ( 110.2429982417149574, 29.99119854320845846, -89.61153874658103291 ) ) ;
#43495 = LINE ( 'NONE', #64972, #11300 ) ;
#43496 = CARTESIAN_POINT ( 'NONE',  ( 429.8372781065087338, 400.0000000000067075, -128.9497041420121093 ) ) ;
#43497 = ORIENTED_EDGE ( 'NONE', *, *, #11730, .F. ) ;
#43498 = CARTESIAN_POINT ( 'NONE',  ( -450.6627218934913230, 177.8591479523843475, 78.55029585798814651 ) ) ;
#43499 = CARTESIAN_POINT ( 'NONE',  ( -31.43908319763709258, 9.591432048623765638, 18.37190381572551701 ) ) ;
#43500 = CARTESIAN_POINT ( 'NONE',  ( -125.8938041572051389, -170.0000000000000000, -34.91370389823391918 ) ) ;
#43501 = EDGE_CURVE ( 'NONE', #54597, #11779, #4391, .T. ) ;
#43502 = CARTESIAN_POINT ( 'NONE',  ( 282.2205320413087293, -21.53693364843037017, 4.491889980468770638 ) ) ;
#43503 = CARTESIAN_POINT ( 'NONE',  ( -0.2727178028659107967, 0.000000000000000000, 23.97499999999999787 ) ) ;
#43504 = CARTESIAN_POINT ( 'NONE',  ( 79.29204528441387367, 18.09916687801608504, 92.49219715506139039 ) ) ;
#43505 = EDGE_CURVE ( 'NONE', #67008, #22304, #12034, .T. ) ;
#43506 = ADVANCED_FACE ( 'NONE', ( #27209 ), #21935, .T. ) ;
#43507 = ORIENTED_EDGE ( 'NONE', *, *, #43807, .F. ) ;
#43508 = CARTESIAN_POINT ( 'NONE',  ( 681.0906130828562937, 908.9915846175126717, 803.5068267248677785 ) ) ;
#43509 = LINE ( 'NONE', #53716, #59904 ) ;
#43510 = CARTESIAN_POINT ( 'NONE',  ( 0.7145311798163274108, 9.237604307034018802, -2.124379920709345337E-16 ) ) ;
#43511 = CARTESIAN_POINT ( 'NONE',  ( -168.7314919967217861, 83.83749564070829763, -36.11248519031690307 ) ) ;
#43512 = CARTESIAN_POINT ( 'NONE',  ( -126.3495878770406193, 48.00153794568856114, -34.91370389823391918 ) ) ;
#43513 = EDGE_LOOP ( 'NONE', ( #54301, #28963, #14899, #33751 ) ) ;
#43514 = CARTESIAN_POINT ( 'NONE',  ( 16.78635691501517613, 6.000000000000000000, -9.435653166495500344 ) ) ;
#43515 = CARTESIAN_POINT ( 'NONE',  ( -5.871577929436022636, 6.771181646175757685, -8.815636319518523223 ) ) ;
#43516 = VECTOR ( 'NONE', #21383, 1000.000000000000000 ) ;
#43517 = CARTESIAN_POINT ( 'NONE',  ( 197.4121679705847612, 98.46451029407255362, -18.76899993905374586 ) ) ;
#43518 = CARTESIAN_POINT ( 'NONE',  ( -144.4736899159893824, 60.02381438289076243, 86.31825897600546682 ) ) ;
#43519 = AXIS2_PLACEMENT_3D ( 'NONE', #38939, #49106, #60385 ) ;
#43520 = CARTESIAN_POINT ( 'NONE',  ( 116.4569059613810680, -170.0000000000000000, 94.99999999999866418 ) ) ;
#43521 = VERTEX_POINT ( 'NONE', #11374 ) ;
#43522 = CARTESIAN_POINT ( 'NONE',  ( 46.66904755831207297, -10.55634918610412853, 85.00100000000000477 ) ) ;
#43523 = CARTESIAN_POINT ( 'NONE',  ( 84.27937148876361562, 19.69225537006225579, 3.241133752072656193 ) ) ;
#43524 = VECTOR ( 'NONE', #48166, 1000.000000000000000 ) ;
#43525 = CARTESIAN_POINT ( 'NONE',  ( -96.77705718164446580, 31.18700926299574050, 43.13870737491041041 ) ) ;
#43526 = CARTESIAN_POINT ( 'NONE',  ( -12.50000000000002842, 207.5000000000000284, 380.0000000000000000 ) ) ;
#43527 = CIRCLE ( 'NONE', #48043, 21.99999999999998579 ) ;
#43528 = ORIENTED_EDGE ( 'NONE', *, *, #36685, .F. ) ;
#43529 = EDGE_CURVE ( 'NONE', #2204, #21329, #52226, .T. ) ;
#43530 = DIRECTION ( 'NONE',  ( 0.000000000000000000, 0.000000000000000000, 1.000000000000000000 ) ) ;
#43531 = EDGE_LOOP ( 'NONE', ( #37859, #61008, #23311, #54867 ) ) ;
#43532 = ORIENTED_EDGE ( 'NONE', *, *, #26231, .F. ) ;
#43533 = VECTOR ( 'NONE', #35800, 1000.000000000000114 ) ;
#43534 = CARTESIAN_POINT ( 'NONE',  ( 178.1965488566140152, 77.14488558164482868, 29.87333967559920822 ) ) ;
#43535 = DIRECTION ( 'NONE',  ( 0.000000000000000000, 0.000000000000000000, 1.000000000000000000 ) ) ;
#43537 = ORIENTED_EDGE ( 'NONE', *, *, #67999, .F. ) ;
#43536 = DIRECTION ( 'NONE',  ( 0.7071067811865485719, 0.000000000000000000, 0.7071067811865465735 ) ) ;
#43538 = CARTESIAN_POINT ( 'NONE',  ( 162.8142581494935826, 61.92799983924230389, 42.19344870861107921 ) ) ;
#43539 = CARTESIAN_POINT ( 'NONE',  ( -15.67984581960975632, -63.08044415722883969, 170.0000000000000000 ) ) ;
#43540 = LINE ( 'NONE', #21742, #27169 ) ;
#43541 = ORIENTED_EDGE ( 'NONE', *, *, #31698, .F. ) ;
#43542 = CARTESIAN_POINT ( 'NONE',  ( -55.89173064941029878, -16.72186800183967748, 27.58472369374500843 ) ) ;
#43543 = DIRECTION ( 'NONE',  ( 0.9362348706397369824, 0.3513748240813435175, -0.000000000000000000 ) ) ;
#43544 = CARTESIAN_POINT ( 'NONE',  ( 152.6650207832379351, 54.00889961337554723, -91.54105675057486735 ) ) ;
#43545 = CARTESIAN_POINT ( 'NONE',  ( -38.26732153931118319, 10.81230693396213027, -72.77399863615724485 ) ) ;
#43546 = B_SPLINE_CURVE_WITH_KNOTS ( 'NONE', 3,
 ( #30341, #67983, #14841, #4303, #41245, #53144, #58104, #63388, #52135, #20461 ),
 .UNSPECIFIED., .F., .F.,
 ( 4, 2, 2, 2, 4 ),
 ( 0.000000000000000000, 0.002530181115235016244, 0.005060362230470032488, 0.007590543345705047865, 0.01012072446094006324 ),
 .UNSPECIFIED. ) ;
#43547 = ORIENTED_EDGE ( 'NONE', *, *, #42773, .F. ) ;
#43548 = ORIENTED_EDGE ( 'NONE', *, *, #3905, .T. ) ;
#43549 = ORIENTED_EDGE ( 'NONE', *, *, #9957, .T. ) ;
#43550 = PLANE ( 'NONE',  #3636 ) ;
#43551 = EDGE_CURVE ( 'NONE', #12492, #31642, #48825, .T. ) ;
#43552 = CARTESIAN_POINT ( 'NONE',  ( -47.90432812485480696, 12.88062469954617306, 93.79905434906177675 ) ) ;
#43553 = ADVANCED_FACE ( 'NONE', ( #11728 ), #43727, .T. ) ;
#43554 = SURFACE_SIDE_STYLE ('',( #69263 ) ) ;
#43555 = CARTESIAN_POINT ( 'NONE',  ( -149.9449619562961118, 64.55090813009796591, -76.65738112195566600 ) ) ;
#43556 = VECTOR ( 'NONE', #21053, 1000.000000000000000 ) ;
#43557 = CARTESIAN_POINT ( 'NONE',  ( 70.09861411860619285, 14.42781432017776666, 93.49106116398942845 ) ) ;
#43558 = LINE ( 'NONE', #53416, #26943 ) ;
#43559 = EDGE_CURVE ( 'NONE', #6090, #37545, #59854, .T. ) ;
#43560 = CARTESIAN_POINT ( 'NONE',  ( -125.8938041572051105, 46.49392987655495091, 72.46449846362081360 ) ) ;
#43561 = CARTESIAN_POINT ( 'NONE',  ( -47.78501581516121632, 13.88632236864699010, 89.62634416545391502 ) ) ;
#43562 = ADVANCED_FACE ( 'NONE', ( #22637 ), #18587, .T. ) ;
#43563 = CARTESIAN_POINT ( 'NONE',  ( 81.57482918025355900, 17.75786713398421313, 69.60303055166224340 ) ) ;
#43564 = ORIENTED_EDGE ( 'NONE', *, *, #53399, .F. ) ;
#43565 = AXIS2_PLACEMENT_3D ( 'NONE', #3992, #41963, #46896 ) ;
#43566 = LINE ( 'NONE', #33390, #62230 ) ;
#43568 = ORIENTED_EDGE ( 'NONE', *, *, #44854, .F. ) ;
#43567 = EDGE_CURVE ( 'NONE', #42077, #49905, #54985, .T. ) ;
#43569 = CARTESIAN_POINT ( 'NONE',  ( 212.1931396682532807, 117.2245435827728954, -70.35676384241855885 ) ) ;
#43570 = CARTESIAN_POINT ( 'NONE',  ( -3.364862276287834408, -74.92447999059862696, 43.58025477438756212 ) ) ;
#43571 = AXIS2_PLACEMENT_3D ( 'NONE', #53966, #27250, #48685 ) ;
#43572 = DIRECTION ( 'NONE',  ( -0.000000000000000000, 1.000000000000000000, -0.000000000000000000 ) ) ;
#43573 = DIRECTION ( 'NONE',  ( 0.6234898018587431423, -0.7818314824680220321, 0.000000000000000000 ) ) ;
#43574 = EDGE_CURVE ( 'NONE', #14487, #16778, #38778, .T. ) ;
#43575 = CARTESIAN_POINT ( 'NONE',  ( -442.6627218934912662, 394.9999999999998295, 113.5502958579881465 ) ) ;
#43576 = CARTESIAN_POINT ( 'NONE',  ( 197.1981527292630858, 96.59367172725642092, 90.15674701874463892 ) ) ;
#43577 = CARTESIAN_POINT ( 'NONE',  ( 156.5909039492010209, 56.96742803863244831, -36.12418429913764584 ) ) ;
#43578 = AXIS2_PLACEMENT_3D ( 'NONE', #62437, #8974, #14252 ) ;
#43579 = DIRECTION ( 'NONE',  ( 1.000000000000000000, 0.000000000000000000, 0.000000000000000000 ) ) ;
#43580 = ORIENTED_EDGE ( 'NONE', *, *, #34557, .F. ) ;
#43581 = CARTESIAN_POINT ( 'NONE',  ( 427.4999999999999432, 207.5000000000000284, 20.00000000000000000 ) ) ;
#43582 = CARTESIAN_POINT ( 'NONE',  ( -173.1211646369891355, -170.0000000000000000, -42.21195716474999671 ) ) ;
#43583 = ORIENTED_EDGE ( 'NONE', *, *, #51686, .F. ) ;
#43584 = ORIENTED_EDGE ( 'NONE', *, *, #5535, .T. ) ;
#43585 = CARTESIAN_POINT ( 'NONE',  ( -85.35127931077731489, 24.98147633333000783, 34.50846909454845246 ) ) ;
#43586 = CARTESIAN_POINT ( 'NONE',  ( -24.95010104166213694, 9.631487977190602123, -65.89293244537743988 ) ) ;
#43587 = CARTESIAN_POINT ( 'NONE',  ( 46.80475532923157544, 10.50744084852537341, 36.18526792674665415 ) ) ;
#43588 = CARTESIAN_POINT ( 'NONE',  ( -29.75049355503753290, 9.320234381800293733, 57.24947098832353731 ) ) ;
#43589 = VECTOR ( 'NONE', #22645, 1000.000000000000114 ) ;
#43590 = DIRECTION ( 'NONE',  ( 0.9749279121818226201, 0.2225209339563184452, -0.000000000000000000 ) ) ;
#43591 = EDGE_CURVE ( 'NONE', #53656, #66593, #18405, .T. ) ;
#43592 = ADVANCED_FACE ( 'NONE', ( #13480 ), #56737, .F. ) ;
#43593 = ORIENTED_EDGE ( 'NONE', *, *, #11182, .T. ) ;
#43594 = ORIENTED_EDGE ( 'NONE', *, *, #21884, .F. ) ;
#43595 = DIRECTION ( 'NONE',  ( 1.000000000000000000, 0.000000000000000000, 0.000000000000000000 ) ) ;
#43596 = ORIENTED_EDGE ( 'NONE', *, *, #43981, .F. ) ;
#43597 = CARTESIAN_POINT ( 'NONE',  ( 35.66087318222938052, 8.964867769223227256, -22.79433549599965048 ) ) ;
#43598 = CARTESIAN_POINT ( 'NONE',  ( 183.8582891103381201, 82.91081946035752992, -90.40977833027336885 ) ) ;
#43599 = CARTESIAN_POINT ( 'NONE',  ( 60.63507185982727776, 12.13307030573223244, 71.27383786105745855 ) ) ;
#43600 = CARTESIAN_POINT ( 'NONE',  ( 138.5824539808545239, 45.54502076838151226, 84.86660875767417167 ) ) ;
#43601 = CARTESIAN_POINT ( 'NONE',  ( -27.05154547620706040, 9.929048335933888580, -90.41981277176407161 ) ) ;
#43602 = CARTESIAN_POINT ( 'NONE',  ( 45.57199999999999562, 0.000000000000000000, 5.000000000000000000 ) ) ;
#43603 = ORIENTED_EDGE ( 'NONE', *, *, #49402, .F. ) ;
#43604 = CARTESIAN_POINT ( 'NONE',  ( 183.2136430849847955, 6.000000000000000000, -41.68900338898720292 ) ) ;
#43605 = VERTEX_POINT ( 'NONE', #66612 ) ;
#43606 = ORIENTED_EDGE ( 'NONE', *, *, #38822, .F. ) ;
#43607 = CARTESIAN_POINT ( 'NONE',  ( 157.9130201331580849, 57.99550255803045218, -24.27963370867398041 ) ) ;
#43608 = CARTESIAN_POINT ( 'NONE',  ( -36.11269837220812207, -31.11269837220801193, 0.000000000000000000 ) ) ;
#43609 = CARTESIAN_POINT ( 'NONE',  ( -430.1627218934916073, 400.0000000000065370, -123.9497041420119530 ) ) ;
#43610 = CARTESIAN_POINT ( 'NONE',  ( 134.7697261969508702, 41.97802808873666436, -77.82602812282750904 ) ) ;
#43611 = CARTESIAN_POINT ( 'NONE',  ( 0.000000000000000000, 0.000000000000000000, 0.000000000000000000 ) ) ;
#43612 = ORIENTED_EDGE ( 'NONE', *, *, #8844, .F. ) ;
#43613 = CARTESIAN_POINT ( 'NONE',  ( 79.19345177405118363, 17.01649702043280499, 11.37811128945321926 ) ) ;
#43614 = ORIENTED_EDGE ( 'NONE', *, *, #38124, .T. ) ;
#43615 = CARTESIAN_POINT ( 'NONE',  ( -71.16770070143907390, 19.60548673929830343, 37.39342123284746577 ) ) ;
#43616 = EDGE_LOOP ( 'NONE', ( #11455, #56382 ) ) ;
#43617 = CARTESIAN_POINT ( 'NONE',  ( 46.66904755831210139, -9.150666335777657423E-14, 85.00100000000000477 ) ) ;
#43618 = VECTOR ( 'NONE', #30569, 999.9999999999998863 ) ;
#43619 = ORIENTED_EDGE ( 'NONE', *, *, #46085, .F. ) ;
#43620 = CARTESIAN_POINT ( 'NONE',  ( -55.05276343752909440, 14.68156374112637330, -8.371773407996169425 ) ) ;
#43621 = DIRECTION ( 'NONE',  ( 0.000000000000000000, 0.000000000000000000, 1.000000000000000000 ) ) ;
#43622 = CIRCLE ( 'NONE', #47009, 65.36598343705435354 ) ;
#43623 = CARTESIAN_POINT ( 'NONE',  ( 44.01696072966020523, -47.84694004974148385, 43.58025477438756923 ) ) ;
#43624 = VERTEX_POINT ( 'NONE', #7159 ) ;
#43625 = LINE ( 'NONE', #43274, #23332 ) ;
#43626 = CARTESIAN_POINT ( 'NONE',  ( 157.0336341255056141, 57.31169401067821667, 29.40946747225336111 ) ) ;
#43627 = CARTESIAN_POINT ( 'NONE',  ( -173.9617926765113793, 89.58633395456783433, -34.74738087939574172 ) ) ;
#43628 = CARTESIAN_POINT ( 'NONE',  ( -44.99999999999998579, 22.99999999999998579, 4.000000000000000000 ) ) ;
#43629 = CARTESIAN_POINT ( 'NONE',  ( -7.825402957745081878, 7.899365992529270741, -77.26262132240753999 ) ) ;
#43630 = DIRECTION ( 'NONE',  ( 0.000000000000000000, 0.000000000000000000, 1.000000000000000000 ) ) ;
#43631 = VERTEX_POINT ( 'NONE', #56043 ) ;
#43632 = CARTESIAN_POINT ( 'NONE',  ( 139.3041645503688812, 46.00819478311336042, -75.52888872897204919 ) ) ;
#43633 = CARTESIAN_POINT ( 'NONE',  ( -143.3980294393559802, 60.45217072626400068, -73.51509446168660133 ) ) ;
#43634 = VERTEX_POINT ( 'NONE', #40213 ) ;
#43635 = FACE_BOUND ( 'NONE', #5021, .T. ) ;
#43636 = CARTESIAN_POINT ( 'NONE',  ( -1.088326810997879202, 6.545818265928948776, -73.09474285069318000 ) ) ;
#43637 = CARTESIAN_POINT ( 'NONE',  ( -177.5288247523079690, 93.72924674643515175, 71.25209080205243595 ) ) ;
#43638 = CARTESIAN_POINT ( 'NONE',  ( -144.9412191745148277, 61.69548892475974355, -9.498880540982458598 ) ) ;
#43639 = CARTESIAN_POINT ( 'NONE',  ( -119.5563837756079550, 43.64229894412654431, -38.37123407000066777 ) ) ;
#43640 = CARTESIAN_POINT ( 'NONE',  ( -79.14094329813313777, 23.58034730000058232, 3.573650549209439919 ) ) ;
#43641 = CARTESIAN_POINT ( 'NONE',  ( 86.62931800182293784, 20.48449268398423939, -77.66611478937542756 ) ) ;
#43642 = FACE_OUTER_BOUND ( 'NONE', #48874, .T. ) ;
#43643 = CARTESIAN_POINT ( 'NONE',  ( -121.1841775822197889, 44.65790002524553870, -75.11573309556970912 ) ) ;
#43644 = EDGE_CURVE ( 'NONE', #57348, #46836, #31348, .T. ) ;
#43645 = CARTESIAN_POINT ( 'NONE',  ( 63.01563776193090405, 12.67277567978497643, 17.96841034875761878 ) ) ;
#43646 = DIRECTION ( 'NONE',  ( 0.000000000000000000, 1.000000000000000000, 0.000000000000000000 ) ) ;
#43647 = CARTESIAN_POINT ( 'NONE',  ( 88.53025347111697840, 21.14438024052372711, -23.74787560486554838 ) ) ;
#43648 = ORIENTED_EDGE ( 'NONE', *, *, #30143, .F. ) ;
#43649 = DIRECTION ( 'NONE',  ( 0.000000000000000000, 0.000000000000000000, 1.000000000000000000 ) ) ;
#43650 = EDGE_LOOP ( 'NONE', ( #33201, #45741, #13115, #64369 ) ) ;
#43651 = DIRECTION ( 'NONE',  ( -1.020422603260505347E-14, 1.000000000000000000, 5.551115123125782702E-17 ) ) ;
#43652 = CARTESIAN_POINT ( 'NONE',  ( 79.91920957766414801, 18.29292522273511779, -66.77815974945997368 ) ) ;
#43653 = CARTESIAN_POINT ( 'NONE',  ( 117.4401308804713437, 33.48331296629643816, 88.66182713554364625 ) ) ;
#43654 = CARTESIAN_POINT ( 'NONE',  ( -142.5087559769085033, 59.74468185400780129, 67.81411370576715569 ) ) ;
#43655 = EDGE_CURVE ( 'NONE', #57073, #16392, #29653, .T. ) ;
#43656 = CARTESIAN_POINT ( 'NONE',  ( 70.45466089417030275, 14.52203022703029589, -15.38972110680052374 ) ) ;
#43657 = CARTESIAN_POINT ( 'NONE',  ( -30.94745021534356511, 10.53010394565407637, -35.31719736520184227 ) ) ;
#43658 = CARTESIAN_POINT ( 'NONE',  ( -55.05276343752909440, 15.72344139423347364, -62.06087458892354647 ) ) ;
#43659 = CARTESIAN_POINT ( 'NONE',  ( -71.79230326678022323, 20.88638099735849352, -93.27200592928129197 ) ) ;
#43660 = CARTESIAN_POINT ( 'NONE',  ( -118.4709174626548531, 42.97515378817185194, -14.46299016164537754 ) ) ;
#43661 = EDGE_LOOP ( 'NONE', ( #43714, #29205, #35382, #68426 ) ) ;
#43662 = EDGE_LOOP ( 'NONE', ( #13192, #854 ) ) ;
#43663 = CARTESIAN_POINT ( 'NONE',  ( 32.29578462738145817, 8.602609172809792426, 66.66940855545223599 ) ) ;
#43664 = CARTESIAN_POINT ( 'NONE',  ( 173.7246046907419554, 71.47482343504563573, 65.12733704930907663 ) ) ;
#43665 = CARTESIAN_POINT ( 'NONE',  ( -166.2053056899074761, 81.18967388993343093, -18.28366721520819027 ) ) ;
#43666 = EDGE_CURVE ( 'NONE', #54090, #67063, #36519, .T. ) ;
#43667 = B_SPLINE_CURVE_WITH_KNOTS ( 'NONE', 3,
 ( #51284, #35445, #62165, #3774, #30510, #46682, #35094, #56546, #46329, #35796, #29469, #47032, #9060, #51625, #41759, #67135, #62871, #3432, #51963, #25247, #19967, #61816, #68158, #41418, #45655, #56199, #9406, #63216, #15019, #24897, #14672, #30174, #30865, #8017, #13988, #52308, #25597, #24209, #24559, #36136, #20294, #45993, #56906, #50928 ),
 .UNSPECIFIED., .F., .F.,
 ( 4, 2, 2, 2, 2, 2, 2, 2, 2, 2, 2, 2, 2, 2, 2, 2, 2, 2, 2, 2, 2, 4 ),
 ( 0.000000000000000000, 0.001487235713946774259, 0.002230853570920142415, 0.002974471427893510354, 0.004461707141840224981, 0.005948942855786940043, 0.007436178569733655104, 0.008179796426707028681, 0.008923414283680403125, 0.01041064999762720579, 0.01189788571157400672, 0.01264150356854738637, 0.01338512142552076602, 0.01487235713946755827, 0.01561597499644096394, 0.01635959285341436961, 0.01784682856736117748, 0.01933406428130798882, 0.02007768213828138928, 0.02082129999525479322, 0.02230853570920154905, 0.02379577142314830487 ),
 .UNSPECIFIED. ) ;
#43668 = VECTOR ( 'NONE', #17851, 1000.000000000000000 ) ;
#43669 = PRODUCT_DEFINITION_CONTEXT ( 'detailed design', #44923, 'design' ) ;
#43670 = CARTESIAN_POINT ( 'NONE',  ( 63.01563776193091826, 13.70579113808095073, -23.87614024170608218 ) ) ;
#43671 = ORIENTED_EDGE ( 'NONE', *, *, #39464, .T. ) ;
#43672 = VECTOR ( 'NONE', #60831, 1000.000000000000000 ) ;
#43673 = CARTESIAN_POINT ( 'NONE',  ( 103.0124792097646207, 26.77148435100180990, -45.48088717822322735 ) ) ;
#43674 = CARTESIAN_POINT ( 'NONE',  ( -14.55425570676089286, 7.423011834016143951, 67.78171509784250759 ) ) ;
#43675 = CARTESIAN_POINT ( 'NONE',  ( -79.61931371420118353, 22.68640080971621487, -8.316616331170878951 ) ) ;
#43676 = CARTESIAN_POINT ( 'NONE',  ( -81.56869946242737512, 24.53041000886392808, -89.37576505892265288 ) ) ;
#43677 = CARTESIAN_POINT ( 'NONE',  ( 18.89356949897907967, -62.19351277735682970, 170.0000000000000000 ) ) ;
#43678 = DIRECTION ( 'NONE',  ( 1.387778780781445429E-16, -1.000000000000000000, -3.081487911019577365E-33 ) ) ;
#43679 = FACE_BOUND ( 'NONE', #53968, .T. ) ;
#43680 = CARTESIAN_POINT ( 'NONE',  ( -59.36813706141740710, 15.88103696331963732, -36.57740707826144444 ) ) ;
#43681 = B_SPLINE_CURVE_WITH_KNOTS ( 'NONE', 3,
 ( #58028, #9846, #53072, #26023, #4225, #35544, #52407, #3524, #26367, #30269, #42536, #67905, #8818, #69267, #9155, #30961, #9500, #14437, #63989, #63313, #41167, #3876, #68912, #42197, #20385, #35887, #62961, #25345, #25692, #51718, #31307, #47120, #30613, #24996, #68584, #52063, #46427, #19704, #62626, #46781, #41855, #4560, #68252, #47453, #15121, #36582, #20057, #41509 ),
 .UNSPECIFIED., .F., .F.,
 ( 4, 2, 2, 2, 2, 2, 2, 2, 2, 2, 2, 2, 2, 2, 2, 2, 2, 2, 2, 2, 2, 2, 2, 4 ),
 ( 0.000000000000000000, 0.003619254076116538554, 0.004524067595145629499, 0.005428881114174720010, 0.007238508152232927054, 0.008143321671262040984, 0.009048135190291153179, 0.01085776222834930992, 0.01176257574737839783, 0.01266738926640748400, 0.01357220278543657017, 0.01447701630446565635, 0.01538182982349474426, 0.01628664334252383217, 0.01719145686155291661, 0.01809627038058200452, 0.01900108389961108896, 0.01990589741864017687, 0.02171552445669841513, 0.02262033797572753774, 0.02352515149475665687, 0.02533477853281489514, 0.02714440557087313688, 0.02895403260893137515 ),
 .UNSPECIFIED. ) ;
#43682 = EDGE_LOOP ( 'NONE', ( #34751, #39908, #3680, #13819 ) ) ;
#43683 = FACE_OUTER_BOUND ( 'NONE', #37485, .T. ) ;
#43684 = DIRECTION ( 'NONE',  ( 0.000000000000000000, 0.000000000000000000, 1.000000000000000000 ) ) ;
#43685 = CARTESIAN_POINT ( 'NONE',  ( -48.23766733091050440, 13.99378332280059389, 67.80282971881165111 ) ) ;
#43686 = DIRECTION ( 'NONE',  ( 0.9362348706397369824, 0.3513748240813435175, 0.000000000000000000 ) ) ;
#43687 = DIRECTION ( 'NONE',  ( -0.000000000000000000, -0.000000000000000000, 1.000000000000000000 ) ) ;
#43688 = CARTESIAN_POINT ( 'NONE',  ( -4.374019708349202951, 7.698173713297786769, 84.63809582392633502 ) ) ;
#43689 = ORIENTED_EDGE ( 'NONE', *, *, #18122, .F. ) ;
#43690 = CARTESIAN_POINT ( 'NONE',  ( 56.30011474572734187, 11.21470186335419505, 7.119764699933178953 ) ) ;
#43691 = FACE_OUTER_BOUND ( 'NONE', #48492, .T. ) ;
#43692 = ORIENTED_EDGE ( 'NONE', *, *, #30331, .F. ) ;
#43693 = ORIENTED_EDGE ( 'NONE', *, *, #28029, .T. ) ;
#43694 = CARTESIAN_POINT ( 'NONE',  ( -79.14678386417814693, 22.50468917936073154, -61.96000122218156747 ) ) ;
#43695 = DIRECTION ( 'NONE',  ( 0.000000000000000000, 1.232595164407830672E-32, -1.000000000000000000 ) ) ;
#43696 = CARTESIAN_POINT ( 'NONE',  ( 109.7724924842965635, 28.66436020578542099, 44.61121420573732621 ) ) ;
#43697 = ORIENTED_EDGE ( 'NONE', *, *, #54438, .T. ) ;
#43698 = ORIENTED_EDGE ( 'NONE', *, *, #2444, .F. ) ;
#43699 = DIRECTION ( 'NONE',  ( 0.000000000000000000, 0.000000000000000000, 1.000000000000000000 ) ) ;
#43700 = AXIS2_PLACEMENT_3D ( 'NONE', #26013, #15109, #14067 ) ;
#43701 = CARTESIAN_POINT ( 'NONE',  ( 159.6614743841975042, 60.66237087206238243, 29.72267884793179960 ) ) ;
#43702 = FACE_OUTER_BOUND ( 'NONE', #17883, .T. ) ;
#43703 = CARTESIAN_POINT ( 'NONE',  ( 66.30636076182547356, 14.49616748423542134, 17.22552420475900448 ) ) ;
#43704 = CARTESIAN_POINT ( 'NONE',  ( 91.51282003084290295, 21.14522045960330132, 42.92523528589520510 ) ) ;
#43705 = EDGE_CURVE ( 'NONE', #15521, #41738, #37188, .T. ) ;
#43707 = EDGE_CURVE ( 'NONE', #47435, #34582, #3274, .T. ) ;
#43706 = CARTESIAN_POINT ( 'NONE',  ( 107.2614272668149482, 28.62909081796206934, -9.691944018085198564 ) ) ;
#43708 = CARTESIAN_POINT ( 'NONE',  ( 311.9975424824652350, 172.0000000000000284, 420.0000000000000000 ) ) ;
#43709 = CARTESIAN_POINT ( 'NONE',  ( -153.7711962260935650, 69.23055119419213099, -89.82806832391398189 ) ) ;
#43710 = CARTESIAN_POINT ( 'NONE',  ( 70.26840926437850499, 14.47268499222803584, -95.00000000000133582 ) ) ;
#43711 = AXIS2_PLACEMENT_3D ( 'NONE', #15696, #30850, #42082 ) ;
#43712 = CARTESIAN_POINT ( 'NONE',  ( 93.57270713017220487, 21.90807125275457423, 93.81897079287583097 ) ) ;
#43714 = ORIENTED_EDGE ( 'NONE', *, *, #16522, .F. ) ;
#43713 = CYLINDRICAL_SURFACE ( 'NONE', #36633, 7.500000000000020428 ) ;
#43715 = ORIENTED_EDGE ( 'NONE', *, *, #30439, .T. ) ;
#43716 = VECTOR ( 'NONE', #45180, 1000.000000000000000 ) ;
#43717 = VERTEX_POINT ( 'NONE', #25429 ) ;
#43718 = CARTESIAN_POINT ( 'NONE',  ( 149.0250918491436494, 0.000000000000000000, -41.68900338898718871 ) ) ;
#43719 = CARTESIAN_POINT ( 'NONE',  ( -165.8134318330274652, 80.78594366325573617, 90.28324896190464699 ) ) ;
#43720 = DIRECTION ( 'NONE',  ( 1.000000000000000000, -3.344045254895050726E-17, 0.000000000000000000 ) ) ;
#43721 = CARTESIAN_POINT ( 'NONE',  ( 29.99999999999999645, -27.00000000000000355, 12.00000000000000000 ) ) ;
#43722 = ADVANCED_FACE ( 'NONE', ( #35632 ), #57084, .T. ) ;
#43723 = CARTESIAN_POINT ( 'NONE',  ( -61.52761555060400411, 17.56359742150277725, -46.53362156671873606 ) ) ;
#43724 = EDGE_CURVE ( 'NONE', #52360, #34095, #52818, .T. ) ;
#43725 = CARTESIAN_POINT ( 'NONE',  ( -11.79249160485393233, 8.191429102467060019, -9.703845154134903339 ) ) ;
#43726 = LINE ( 'NONE', #66275, #67967 ) ;
#43727 = PLANE ( 'NONE',  #57853 ) ;
#43728 = VERTEX_POINT ( 'NONE', #51802 ) ;
#43729 = CARTESIAN_POINT ( 'NONE',  ( 4.000000000000011546, -6.928203230275505220, 0.000000000000000000 ) ) ;
#43730 = ORIENTED_EDGE ( 'NONE', *, *, #1668, .F. ) ;
#43731 = VERTEX_POINT ( 'NONE', #46868 ) ;
#43732 = DIRECTION ( 'NONE',  ( -0.6234898018587318180, -0.7818314824680311359, 0.000000000000000000 ) ) ;
#43733 =( NAMED_UNIT ( * ) PLANE_ANGLE_UNIT ( ) SI_UNIT ( $, .RADIAN. ) );
#43734 = CARTESIAN_POINT ( 'NONE',  ( 117.7237061126833026, 32.49927938580613329, 91.44293783028797407 ) ) ;
#43735 = ADVANCED_FACE ( 'NONE', ( #20134 ), #3610, .T. ) ;
#43736 = AXIS2_PLACEMENT_3D ( 'NONE', #40452, #25331, #14066 ) ;
#43737 = CARTESIAN_POINT ( 'NONE',  ( -95.63568360745009045, 29.53168204475776193, -46.00256717322782407 ) ) ;
#43738 = CARTESIAN_POINT ( 'NONE',  ( -109.7816385129979011, 36.75776661907241305, 10.67383622189045767 ) ) ;
#43739 = CARTESIAN_POINT ( 'NONE',  ( 22.89634831467700948, 6.832298124325685507, 39.92007651388386336 ) ) ;
#43740 = CARTESIAN_POINT ( 'NONE',  ( 141.3586046882815026, 47.34625111366350581, -17.18765650132280953 ) ) ;
#43741 = ORIENTED_EDGE ( 'NONE', *, *, #1826, .T. ) ;
#43742 = ORIENTED_EDGE ( 'NONE', *, *, #59241, .T. ) ;
#43743 = ORIENTED_EDGE ( 'NONE', *, *, #36936, .F. ) ;
#43744 =( BOUNDED_CURVE ( )  B_SPLINE_CURVE ( 3, ( #320, #26723, #30709, #43220 ),
 .UNSPECIFIED., .F., .F. ) 
 B_SPLINE_CURVE_WITH_KNOTS ( ( 4, 4 ),
 ( -8.881784197001252323E-16, 1.570796326794900111 ),
 .UNSPECIFIED. ) 
 CURVE ( )  GEOMETRIC_REPRESENTATION_ITEM ( )  RATIONAL_B_SPLINE_CURVE ( ( 1.000000000000000000, 0.8047378541243640493, 0.8047378541243640493, 1.000000000000000000 ) ) 
 REPRESENTATION_ITEM ( '' )  );
#43745 = LINE ( 'NONE', #44816, #55206 ) ;
#43746 = CARTESIAN_POINT ( 'NONE',  ( -10.46803069297986433, 7.077485182625209426, 17.79433764303042764 ) ) ;
#43747 = CARTESIAN_POINT ( 'NONE',  ( 55.90536342106782541, 11.13510150712953539, -18.81323374408498950 ) ) ;
#43748 = EDGE_CURVE ( 'NONE', #60940, #44163, #26103, .T. ) ;
#43749 = DIRECTION ( 'NONE',  ( 0.9989930665413144784, 0.04486483035051863633, 5.102127870520020458E-18 ) ) ;
#43750 = AXIS2_PLACEMENT_3D ( 'NONE', #51797, #61994, #51111 ) ;
#43751 = EDGE_CURVE ( 'NONE', #69327, #32375, #15172, .T. ) ;
#43752 = CARTESIAN_POINT ( 'NONE',  ( 5.799999999999999822, 8.000000000000000000, 0.000000000000000000 ) ) ;
#43753 = EDGE_CURVE ( 'NONE', #34598, #44611, #4557, .T. ) ;
#43754 = ORIENTED_EDGE ( 'NONE', *, *, #49949, .T. ) ;
#43755 = EDGE_CURVE ( 'NONE', #34459, #34109, #16259, .T. ) ;
#43756 = CARTESIAN_POINT ( 'NONE',  ( 188.5842358232186200, 88.03712271786932320, 63.35372157011578764 ) ) ;
#43757 = CARTESIAN_POINT ( 'NONE',  ( 16.78635691501517613, 0.000000000000000000, -46.68900338898716029 ) ) ;
#43758 =( NAMED_UNIT ( * ) SI_UNIT ( $, .STERADIAN. ) SOLID_ANGLE_UNIT ( ) );
#43759 = CARTESIAN_POINT ( 'NONE',  ( -1.455067768715155418, 7.566780179921179794, -38.95200498131430322 ) ) ;
#43760 = DIRECTION ( 'NONE',  ( -0.000000000000000000, 0.000000000000000000, -1.000000000000000000 ) ) ;
#43761 = CARTESIAN_POINT ( 'NONE',  ( -80.31691774066410971, 22.95709084517032039, -35.29547712760505362 ) ) ;
#43762 = CARTESIAN_POINT ( 'NONE',  ( 16.77391662606469325, 6.533867394142987450, 71.81064437024208758 ) ) ;
#43763 = LINE ( 'NONE', #23392, #29846 ) ;
#43764 = CARTESIAN_POINT ( 'NONE',  ( 14.80582440982707482, 6.470883766728822373, -62.41208511885447052 ) ) ;
#43765 = AXIS2_PLACEMENT_3D ( 'NONE', #45815, #68641, #67293 ) ;
#43766 = ORIENTED_EDGE ( 'NONE', *, *, #33919, .T. ) ;
#43767 = CARTESIAN_POINT ( 'NONE',  ( 290.0000000000000568, 0.000000000000000000, 0.000000000000000000 ) ) ;
#43768 = PLANE ( 'NONE',  #55457 ) ;
#43769 = DIRECTION ( 'NONE',  ( -1.000000000000000000, 0.000000000000000000, 0.000000000000000000 ) ) ;
#43770 = FACE_OUTER_BOUND ( 'NONE', #24940, .T. ) ;
#43771 = AXIS2_PLACEMENT_3D ( 'NONE', #13780, #51428, #18718 ) ;
#43772 = CARTESIAN_POINT ( 'NONE',  ( 61.09977118998600076, 13.26754120022605044, -77.32048710585367246 ) ) ;
#43773 = ORIENTED_EDGE ( 'NONE', *, *, #3920, .F. ) ;
#43774 = B_SPLINE_CURVE_WITH_KNOTS ( 'NONE', 3,
 ( #66954, #54981, #18061, #38821, #13474, #50754, #66271, #7517, #12087, #2234, #18398, #49695, #39513, #29644, #44790, #55329, #28969, #7153, #60961, #29301, #8196, #1525, #39854, #1893, #2574, #22988, #45474, #34602, #51109, #12782, #24031, #34244, #61312, #45126, #23683, #23347, #60269, #50414, #13137, #28614, #6799, #2919, #50063, #61655 ),
 .UNSPECIFIED., .F., .F.,
 ( 4, 2, 2, 2, 2, 2, 2, 2, 2, 2, 2, 2, 2, 2, 2, 2, 2, 2, 2, 2, 2, 4 ),
 ( 1.440969542111313559E-17, 0.001533942663855621677, 0.003067885327711229043, 0.004601827991566837493, 0.005368799323494641285, 0.006135770655422445943, 0.007669713319278085618, 0.008436684651205906757, 0.009203655983133728763, 0.01073759864698935890, 0.01150456997891717396, 0.01227154131084498556, 0.01303851264277279542, 0.01380548397470060355, 0.01533942663855623195, 0.01687336930241186209, 0.01840731196626749222, 0.01994125463012312235, 0.02070822596205093569, 0.02147519729397874902, 0.02300913995783437915, 0.02454308262169000582 ),
 .UNSPECIFIED. ) ;
#43775 = VERTEX_POINT ( 'NONE', #12704 ) ;
#43776 = CARTESIAN_POINT ( 'NONE',  ( -133.3122825023497171, 51.57669324886579432, -95.00000000000133582 ) ) ;
#43777 = FACE_OUTER_BOUND ( 'NONE', #33071, .T. ) ;
#43778 = ORIENTED_EDGE ( 'NONE', *, *, #56361, .T. ) ;
#43779 = ORIENTED_EDGE ( 'NONE', *, *, #26236, .F. ) ;
#43780 = CARTESIAN_POINT ( 'NONE',  ( 177.0024338932394414, 74.57605685449961186, -37.41665159782565553 ) ) ;
#43781 = CARTESIAN_POINT ( 'NONE',  ( 313.9975424824652350, 295.8720703627916464, 535.5371946177799600 ) ) ;
#43782 = VERTEX_POINT ( 'NONE', #9069 ) ;
#43783 = CARTESIAN_POINT ( 'NONE',  ( 117.7417271423230147, 33.63613196344608269, 64.49092239129596749 ) ) ;
#43784 = CARTESIAN_POINT ( 'NONE',  ( 140.7888851157409817, 46.97220912571251716, 66.72935928051445842 ) ) ;
#43785 = CARTESIAN_POINT ( 'NONE',  ( -71.16770070143911653, 19.60548673929830343, -43.14023053854354828 ) ) ;
#43786 = CARTESIAN_POINT ( 'NONE',  ( 63.01563776193090405, 13.70579113808097738, 44.81296093922130552 ) ) ;
#43787 = CARTESIAN_POINT ( 'NONE',  ( 91.51282003084287453, 21.14522045960330132, -37.60841648549585159 ) ) ;
#43788 = CARTESIAN_POINT ( 'NONE',  ( -48.58011387679029269, 14.07568064779664141, -19.66872259271415757 ) ) ;
#43789 = EDGE_CURVE ( 'NONE', #50390, #10221, #35452, .T. ) ;
#43790 = ORIENTED_EDGE ( 'NONE', *, *, #22416, .F. ) ;
#43792 = EDGE_CURVE ( 'NONE', #12534, #30930, #68167, .T. ) ;
#43791 = CARTESIAN_POINT ( 'NONE',  ( 8.000000000000000000, -3.098204225878178342, -0.3157906771918749245 ) ) ;
#43793 = DIRECTION ( 'NONE',  ( -0.000000000000000000, 1.000000000000000000, 2.500042656554809847E-16 ) ) ;
#43794 = CARTESIAN_POINT ( 'NONE',  ( -5.999999999999998224, 19.07878402833891229, 4.999999999999997335 ) ) ;
#43795 = DIRECTION ( 'NONE',  ( 1.000000000000000000, 0.000000000000000000, 0.000000000000000000 ) ) ;
#43797 = VERTEX_POINT ( 'NONE', #40717 ) ;
#43796 = DIRECTION ( 'NONE',  ( -0.000000000000000000, 0.5000000000000009992, 0.8660254037844380415 ) ) ;
#43798 = CARTESIAN_POINT ( 'NONE',  ( 61.08522853873729730, 13.26388801693373409, 17.73216832077243410 ) ) ;
#43799 = AXIS2_PLACEMENT_3D ( 'NONE', #25525, #51559, #14268 ) ;
#43800 = VERTEX_POINT ( 'NONE', #51970 ) ;
#43801 = CARTESIAN_POINT ( 'NONE',  ( -144.7571537022064376, 60.25265659240449168, 59.25656382279842660 ) ) ;
#43802 = CARTESIAN_POINT ( 'NONE',  ( 10.55634918610396511, -46.66904755831214402, 85.00100000000000477 ) ) ;
#43803 = CARTESIAN_POINT ( 'NONE',  ( 86.62931800182292363, 20.48449268398425716, -89.51066537983906812 ) ) ;
#43804 = EDGE_CURVE ( 'NONE', #38606, #5953, #14064, .T. ) ;
#43805 = EDGE_CURVE ( 'NONE', #43873, #10912, #28888, .T. ) ;
#43806 = CARTESIAN_POINT ( 'NONE',  ( 92.95016907945944240, 22.74936990452174967, 33.16759907785775141 ) ) ;
#43807 = EDGE_CURVE ( 'NONE', #41847, #62155, #56509, .T. ) ;
#43808 = CARTESIAN_POINT ( 'NONE',  ( 80.30232379693107703, 17.35837133860831827, -20.51189838118990494 ) ) ;
#43809 = CARTESIAN_POINT ( 'NONE',  ( 46.90170507415072620, 10.52318308703818062, 11.06461444427903373 ) ) ;
#43810 = CARTESIAN_POINT ( 'NONE',  ( 93.63037639125408873, 21.92981100938039063, -67.46451625388530715 ) ) ;
#43811 = CARTESIAN_POINT ( 'NONE',  ( 41.72486082342749825, 50.31647622756256766, 43.58025477438756212 ) ) ;
#43812 = CARTESIAN_POINT ( 'NONE',  ( -156.4819242240389769, 70.32841519459755375, -93.23206903001478452 ) ) ;
#43813 = VERTEX_POINT ( 'NONE', #13996 ) ;
#43814 = ORIENTED_EDGE ( 'NONE', *, *, #45983, .T. ) ;
#43815 = EDGE_CURVE ( 'NONE', #42114, #59695, #54900, .T. ) ;
#43816 = CARTESIAN_POINT ( 'NONE',  ( 42.70988075781784232, 8.862408058333477001, 30.66516676936959485 ) ) ;
#43817 = CARTESIAN_POINT ( 'NONE',  ( 12.69192874957005124, 6.421326776602847453, 30.67927649405437407 ) ) ;
#43818 = CARTESIAN_POINT ( 'NONE',  ( -20.55634918610405748, -10.55634918610400597, 85.00100000000000477 ) ) ;
#43819 = CARTESIAN_POINT ( 'NONE',  ( -78.66644367742111399, -170.0000000000000000, -42.61545063171789849 ) ) ;
#43820 = VECTOR ( 'NONE', #20526, 1000.000000000000114 ) ;
#43821 = CARTESIAN_POINT ( 'NONE',  ( 211.4997502125519020, 118.0043045815490501, -46.99967683100181404 ) ) ;
#43822 = FACE_OUTER_BOUND ( 'NONE', #5157, .T. ) ;
#43823 = DIRECTION ( 'NONE',  ( -0.000000000000000000, -1.000000000000000000, -0.000000000000000000 ) ) ;
#43824 = CARTESIAN_POINT ( 'NONE',  ( -125.4463376280758951, 47.40387005565906975, 30.62991178436581663 ) ) ;
#43825 = LINE ( 'NONE', #44888, #66689 ) ;
#43826 = ORIENTED_EDGE ( 'NONE', *, *, #59156, .T. ) ;
#43827 = CARTESIAN_POINT ( 'NONE',  ( 133.8566784816069060, 42.60093787723653236, 2.665790248531674678 ) ) ;
#43828 = VERTEX_POINT ( 'NONE', #56915 ) ;
#43829 = CARTESIAN_POINT ( 'NONE',  ( -9.763294602873864747, 7.024900256480052896, -35.66858442679837538 ) ) ;
#43830 = DIRECTION ( 'NONE',  ( 0.000000000000000000, 0.000000000000000000, 1.000000000000000000 ) ) ;
#43831 = CARTESIAN_POINT ( 'NONE',  ( 87.58754341703161117, 20.81465688423119431, 71.51040371463716383 ) ) ;
#43832 = CARTESIAN_POINT ( 'NONE',  ( 129.4887940973039520, 40.01039828304091373, 43.12603597457647453 ) ) ;
#43833 = CARTESIAN_POINT ( 'NONE',  ( -36.84489839129339828, 53.54860840895182150, 170.0000000000000000 ) ) ;
#43834 = CARTESIAN_POINT ( 'NONE',  ( -20.55634918610408945, -31.11269837220804035, 2.000000000000000000 ) ) ;
#43835 = AXIS2_PLACEMENT_3D ( 'NONE', #33018, #43903, #39688 ) ;
#43836 = DIRECTION ( 'NONE',  ( -0.000000000000000000, -0.000000000000000000, 1.000000000000000000 ) ) ;
#43837 = EDGE_CURVE ( 'NONE', #32464, #22995, #36564, .T. ) ;
#43838 = EDGE_CURVE ( 'NONE', #32720, #58547, #51635, .T. ) ;
#43839 = DIRECTION ( 'NONE',  ( 2.437361367520478414E-16, 5.563118268672117023E-17, 1.000000000000000000 ) ) ;
#43840 = CARTESIAN_POINT ( 'NONE',  ( 210.3791065492700909, 114.4724634728603121, 85.49048150234845878 ) ) ;
#43841 = FACE_OUTER_BOUND ( 'NONE', #51328, .T. ) ;
#43842 = ORIENTED_EDGE ( 'NONE', *, *, #19771, .F. ) ;
#43843 = CARTESIAN_POINT ( 'NONE',  ( 313.9975424824652350, 18.08738615523480675, 402.4289050101931480 ) ) ;
#43844 = DIRECTION ( 'NONE',  ( 0.000000000000000000, -1.000000000000000000, 0.000000000000000000 ) ) ;
#43846 = ADVANCED_FACE ( 'NONE', ( #24905 ), #62536, .F. ) ;
#43845 = CARTESIAN_POINT ( 'NONE',  ( -13.45956523846225039, 8.333781915634244086, 5.814511151728004812 ) ) ;
#43847 = CARTESIAN_POINT ( 'NONE',  ( 45.76405797021009647, 10.34101216371941767, -65.98511464492352729 ) ) ;
#43848 = CARTESIAN_POINT ( 'NONE',  ( -4.725257700475992806, 6.708862164351558910, 44.44922483199589891 ) ) ;
#43849 = DIRECTION ( 'NONE',  ( 0.000000000000000000, 1.000000000000000000, 0.000000000000000000 ) ) ;
#43850 = CARTESIAN_POINT ( 'NONE',  ( 94.05217532500763866, 23.16464989206124159, 89.77431030042610871 ) ) ;
#43851 = ORIENTED_EDGE ( 'NONE', *, *, #47153, .F. ) ;
#43852 = CARTESIAN_POINT ( 'NONE',  ( 542.2259808184915073, 965.7112456033461285, 698.5068267248718712 ) ) ;
#43853 = CIRCLE ( 'NONE', #41614, 21.00000000000000355 ) ;
#43854 = DIRECTION ( 'NONE',  ( -0.000000000000000000, -0.000000000000000000, -1.000000000000000000 ) ) ;
#43855 = FACE_OUTER_BOUND ( 'NONE', #42953, .T. ) ;
#43856 = CARTESIAN_POINT ( 'NONE',  ( -172.3127615181935823, 87.73358064377643473, -49.67956037655144996 ) ) ;
#43857 = CARTESIAN_POINT ( 'NONE',  ( 14.99999999999997158, 0.000000000000000000, -104.9999999999999858 ) ) ;
#43858 = ORIENTED_EDGE ( 'NONE', *, *, #46140, .T. ) ;
#43859 = LINE ( 'NONE', #17124, #34669 ) ;
#43860 = B_SPLINE_CURVE_WITH_KNOTS ( 'NONE', 3,
 ( #29917, #67904, #58027, #46780, #63312, #9845, #41853, #24305, #51377, #30611, #9499, #14083, #25691, #47119, #20055, #9154, #15119, #40464, #61908, #41508, #3193, #3522, #14767, #24995, #35543, #46084, #67554, #19702, #56999, #40809, #30268, #46426, #36920, #11203, #59394, #31635, #48139, #42861, #41200, #37945, #64331, #663, #64684, #15802, #15467, #22113, #26707, #10175, #16142, #43205, #37594, #303, #32672, #43557, #21417, #47452, #65030, #32334 ),
 .UNSPECIFIED., .F., .F.,
 ( 4, 2, 2, 2, 2, 2, 2, 2, 2, 2, 2, 2, 2, 2, 2, 2, 2, 2, 2, 2, 2, 2, 2, 2, 2, 2, 2, 2, 4 ),
 ( 0.000000000000000000, 0.002011202885851239280, 0.003016804328776875616, 0.004022405771702512386, 0.005028007214628148723, 0.006033608657553785060, 0.007039210100479421396, 0.008044811543405057733, 0.009050412986330693202, 0.01005601442925633041, 0.01206721731510760308, 0.01307281875803323855, 0.01407842020095887402, 0.01508402164388450949, 0.01608962308681014669, 0.01709522452973578216, 0.01810082597266142110, 0.02011202885851270244, 0.02111763030143834138, 0.02212323174436398379, 0.02312883318728962620, 0.02413443463021526514, 0.02514003607314090755, 0.02614563751606654649, 0.02715123895899218889, 0.02815684040191783130, 0.03016804328776911265, 0.03117364473069475159, 0.03217924617362039746 ),
 .UNSPECIFIED. ) ;
#43861 = FACE_OUTER_BOUND ( 'NONE', #48584, .T. ) ;
#43862 = DIRECTION ( 'NONE',  ( 1.000000000000000000, 0.000000000000000000, 0.000000000000000000 ) ) ;
#43863 = CARTESIAN_POINT ( 'NONE',  ( -7.336630171688593549, 7.867399454768214895, -77.26262132240753999 ) ) ;
#43864 = LINE ( 'NONE', #43520, #43668 ) ;
#43865 = EDGE_LOOP ( 'NONE', ( #53387, #5423, #66121, #42917 ) ) ;
#43866 = FACE_OUTER_BOUND ( 'NONE', #29863, .T. ) ;
#43867 = CARTESIAN_POINT ( 'NONE',  ( 199.3671895066314619, 99.30947926630328482, -49.12614233709344802 ) ) ;
#43868 = DIRECTION ( 'NONE',  ( 0.000000000000000000, 0.000000000000000000, 1.000000000000000000 ) ) ;
#43869 = CARTESIAN_POINT ( 'NONE',  ( 0.000000000000000000, 35.00000000000000000, 0.000000000000000000 ) ) ;
#43871 = EDGE_LOOP ( 'NONE', ( #51104, #47458, #13954, #9051 ) ) ;
#43870 = DIRECTION ( 'NONE',  ( -0.000000000000000000, -0.000000000000000000, 1.000000000000000000 ) ) ;
#43872 = PLANE ( 'NONE',  #11459 ) ;
#43873 = VERTEX_POINT ( 'NONE', #1451 ) ;
#43874 = EDGE_LOOP ( 'NONE', ( #13904, #11184, #13400, #8848 ) ) ;
#43876 = EDGE_CURVE ( 'NONE', #42155, #49926, #33811, .T. ) ;
#43875 = CARTESIAN_POINT ( 'NONE',  ( -125.0772643754502411, 45.95811963572885617, -88.63583198122191220 ) ) ;
#43877 = DIRECTION ( 'NONE',  ( -0.000000000000000000, 1.000000000000000000, -0.000000000000000000 ) ) ;
#43879 = ORIENTED_EDGE ( 'NONE', *, *, #44800, .T. ) ;
#43878 = CARTESIAN_POINT ( 'NONE',  ( -12.39770133248888584, 8.241491894828993026, -75.72815778851469304 ) ) ;
#43880 = CARTESIAN_POINT ( 'NONE',  ( 0.000000000000000000, 50.00000000000000000, -5.000000000000000000 ) ) ;
#43881 = VECTOR ( 'NONE', #36697, 1000.000000000000000 ) ;
#43882 = CARTESIAN_POINT ( 'NONE',  ( 0.000000000000000000, 0.000000000000000000, 41.38025477438755928 ) ) ;
#43883 = CARTESIAN_POINT ( 'NONE',  ( -76.33235143960693847, 22.51916353135074900, -35.48390396204494124 ) ) ;
#43884 = PRODUCT_DEFINITION_SHAPE ( 'NONE', 'NONE',  #69633 ) ;
#43885 = VERTEX_POINT ( 'NONE', #69176 ) ;
#43886 = DIRECTION ( 'NONE',  ( 0.8191520442889916875, 1.003171929053524623E-16, -0.5735764363510462704 ) ) ;
#43887 = EDGE_CURVE ( 'NONE', #47103, #6327, #68498, .T. ) ;
#43888 = AXIS2_PLACEMENT_3D ( 'NONE', #52967, #63547, #4794 ) ;
#43889 = CARTESIAN_POINT ( 'NONE',  ( -38.93922791710218689, 10.94334660650242341, -16.21455789437017359 ) ) ;
#43890 = CARTESIAN_POINT ( 'NONE',  ( 0.000000000000000000, 0.000000000000000000, 25.70156211871649887 ) ) ;
#43891 = CARTESIAN_POINT ( 'NONE',  ( -35.99019277275119322, 10.38248800679341954, -63.68048773888882153 ) ) ;
#43892 = EDGE_CURVE ( 'NONE', #14549, #33459, #24632, .T. ) ;
#43893 = CARTESIAN_POINT ( 'NONE',  ( 23.28845814680232351, 7.864847136539610872, 63.87262545100447397 ) ) ;
#43894 = ORIENTED_EDGE ( 'NONE', *, *, #37306, .F. ) ;
#43895 = EDGE_CURVE ( 'NONE', #30095, #62805, #58617, .T. ) ;
#43896 = ORIENTED_EDGE ( 'NONE', *, *, #39393, .T. ) ;
#43897 = VERTEX_POINT ( 'NONE', #47369 ) ;
#43898 = AXIS2_PLACEMENT_3D ( 'NONE', #39605, #55072, #22375 ) ;
#43899 = PLANE ( 'NONE',  #53069 ) ;
#43900 = CARTESIAN_POINT ( 'NONE',  ( 86.62931800182293784, -170.0000000000000000, -77.66611478937542756 ) ) ;
#43901 = DIRECTION ( 'NONE',  ( -0.000000000000000000, 0.000000000000000000, -1.000000000000000000 ) ) ;
#43902 = CARTESIAN_POINT ( 'NONE',  ( -31.43908319763709258, 9.591432048623767415, -35.31719736520183517 ) ) ;
#43903 = DIRECTION ( 'NONE',  ( -0.000000000000000000, 0.000000000000000000, 1.000000000000000000 ) ) ;
#43904 = DIRECTION ( 'NONE',  ( -0.000000000000000000, -1.000000000000000000, -0.000000000000000000 ) ) ;
#43905 = DIRECTION ( 'NONE',  ( -6.405487610868040568E-16, -1.000000000000000000, 5.551115123125781470E-17 ) ) ;
#43906 = CARTESIAN_POINT ( 'NONE',  ( -62.39620438142541303, 17.82550490656933917, 89.94779769255055157 ) ) ;
#43907 = CARTESIAN_POINT ( 'NONE',  ( 86.15410276028856629, 19.25894675708889991, 56.55663816294299551 ) ) ;
#43908 = ORIENTED_EDGE ( 'NONE', *, *, #22078, .F. ) ;
#43909 = FACE_OUTER_BOUND ( 'NONE', #33708, .T. ) ;
#43910 = DIRECTION ( 'NONE',  ( -1.000000000000000000, -0.000000000000000000, -0.000000000000000000 ) ) ;
#43911 = CARTESIAN_POINT ( 'NONE',  ( 212.0850679406003678, 117.0583048437722340, -69.33104460838883654 ) ) ;
#43912 = B_SPLINE_CURVE_WITH_KNOTS ( 'NONE', 3,
 ( #551, #38180, #59620, #38894, #11434, #22355, #17058, #11790, #33272, #27976, #49419, #17414, #60337, #28321, #33622, #6871, #67709, #62065, #62424, #24109, #29042, #18821, #8626, #7922, #66681, #13547, #55763, #35002, #50827, #12861, #46233, #56445, #50483, #2305, #45200, #34670, #3336, #23419, #24795, #66341 ),
 .UNSPECIFIED., .F., .F.,
 ( 4, 2, 2, 2, 2, 2, 2, 2, 2, 2, 2, 2, 2, 2, 2, 2, 2, 2, 2, 4 ),
 ( 0.02454308262168999541, 0.02608670964102888234, 0.02685852315069834143, 0.02763033666036780051, 0.02917396367970670826, 0.02994577718937616387, 0.03071759069904561948, 0.03226121771838449948, 0.03303303122805391345, 0.03380484473772334131, 0.03534847175706214845, 0.03689209877640095558, 0.03843572579573976272, 0.03997935281507856986, 0.04152297983441737700, 0.04306660685375618414, 0.04461023387309499821, 0.04615386089243381229, 0.04769748791177262637, 0.04924111493111144044 ),
 .UNSPECIFIED. ) ;
#43913 = CARTESIAN_POINT ( 'NONE',  ( 259.2042601260359334, 188.0000000000000000, 7.478223336038896996 ) ) ;
#43914 = FILL_AREA_STYLE ('',( #54464 ) ) ;
#43915 = CARTESIAN_POINT ( 'NONE',  ( 37.47081272996201307, 8.166145978397519656, 17.82054918726932513 ) ) ;
#43916 = CARTESIAN_POINT ( 'NONE',  ( -49.11825192196924661, 13.17012322555988213, 15.58522413457026623 ) ) ;
#43917 = CARTESIAN_POINT ( 'NONE',  ( 15.55634918610400241, -10.55634918610406281, 2.000000000000001776 ) ) ;
#43918 = CARTESIAN_POINT ( 'NONE',  ( 157.4703587214989113, 58.92748579479258808, -77.96873488960135035 ) ) ;
#43919 = ORIENTED_EDGE ( 'NONE', *, *, #10683, .F. ) ;
#43920 = PLANE ( 'NONE',  #27422 ) ;
#43921 = DIRECTION ( 'NONE',  ( -7.128142269859545174E-15, 0.000000000000000000, 1.000000000000000000 ) ) ;
#43922 = VERTEX_POINT ( 'NONE', #62765 ) ;
#43923 = LINE ( 'NONE', #60112, #21850 ) ;
#43924 = ADVANCED_FACE ( 'NONE', ( #19854 ), #67363, .F. ) ;
#43925 = ORIENTED_EDGE ( 'NONE', *, *, #52485, .F. ) ;
#43926 = DIRECTION ( 'NONE',  ( 1.000000000000000000, 0.000000000000000000, 0.000000000000000000 ) ) ;
#43927 = CARTESIAN_POINT ( 'NONE',  ( 0.000000000000000000, 70.00000000000000000, 0.000000000000000000 ) ) ;
#43928 = CARTESIAN_POINT ( 'NONE',  ( 0.000000000000000000, 0.000000000000000000, 0.000000000000000000 ) ) ;
#43929 = FILL_AREA_STYLE ('',( #65059 ) ) ;
#43930 = CARTESIAN_POINT ( 'NONE',  ( 132.0582325211144905, 40.34869848118181324, -9.383526223381995379 ) ) ;
#43931 = ORIENTED_EDGE ( 'NONE', *, *, #37854, .T. ) ;
#43932 = VECTOR ( 'NONE', #19920, 1000.000000000000000 ) ;
#43933 = ORIENTED_EDGE ( 'NONE', *, *, #42231, .T. ) ;
#43934 = FACE_OUTER_BOUND ( 'NONE', #22291, .T. ) ;
#43935 = VERTEX_POINT ( 'NONE', #3328 ) ;
#43936 = DIRECTION ( 'NONE',  ( -0.000000000000000000, -0.000000000000000000, -1.000000000000000000 ) ) ;
#43937 = CARTESIAN_POINT ( 'NONE',  ( -46.66904755831210139, 6.635317295611287136E-14, 0.000000000000000000 ) ) ;
#43938 = AXIS2_PLACEMENT_3D ( 'NONE', #61786, #13608, #62135 ) ;
#43939 = CARTESIAN_POINT ( 'NONE',  ( 56.30011474572734187, 11.21470186335419683, 60.80886588086055156 ) ) ;
#43940 = CARTESIAN_POINT ( 'NONE',  ( -2.873329055852808622, 7.626065826870669362, 58.80573367209430558 ) ) ;
#43941 = PRODUCT_DEFINITION_SHAPE ( 'NONE', 'NONE',  #69602 ) ;
#43942 = LINE ( 'NONE', #36958, #7755 ) ;
#43943 = CIRCLE ( 'NONE', #60832, 10.00000000000000178 ) ;
#43945 = VECTOR ( 'NONE', #33577, 1000.000000000000000 ) ;
#43944 = FILL_AREA_STYLE_COLOUR ( '', #45168 ) ;
#43946 = ORIENTED_EDGE ( 'NONE', *, *, #26432, .F. ) ;
#43947 = CARTESIAN_POINT ( 'NONE',  ( -124.1094910780272329, 45.33021696310841975, -76.54648126837901145 ) ) ;
#43948 = ORIENTED_EDGE ( 'NONE', *, *, #40820, .T. ) ;
#43949 = VERTEX_POINT ( 'NONE', #51175 ) ;
#43950 = CARTESIAN_POINT ( 'NONE',  ( 437.3372781065085633, 394.9999999999999432, 103.5502958579882460 ) ) ;
#43951 = DIRECTION ( 'NONE',  ( -0.000000000000000000, 0.000000000000000000, -1.000000000000000000 ) ) ;
#43952 = CARTESIAN_POINT ( 'NONE',  ( 6.400000000000000355, -9.237604307034018802, 3.355146209984123968E-17 ) ) ;
#43953 = CARTESIAN_POINT ( 'NONE',  ( 135.6647932137617829, 43.70902528961477884, 17.45871630207848924 ) ) ;
#43954 = CARTESIAN_POINT ( 'NONE',  ( 26.11269837220809364, 15.55634918610396866, 2.000000000000000000 ) ) ;
#43955 = COLOUR_RGB ( '',0.7921568627450980005, 0.8196078431372548767, 0.9333333333333333481 ) ;
#43956 = EDGE_LOOP ( 'NONE', ( #11147, #6456, #6479, #5226, #35463, #68386, #9661, #23859, #59724 ) ) ;
#43957 = EDGE_CURVE ( 'NONE', #17566, #16392, #41312, .T. ) ;
#43958 = CARTESIAN_POINT ( 'NONE',  ( 82.94943325692328528, 18.19803534719806848, 3.827846601591828879 ) ) ;
#43959 = EDGE_CURVE ( 'NONE', #14754, #38713, #19154, .T. ) ;
#43960 = ORIENTED_EDGE ( 'NONE', *, *, #48640, .F. ) ;
#43961 = CARTESIAN_POINT ( 'NONE',  ( -78.18913509716432486, 22.13995206110505976, 45.41820113967313688 ) ) ;
#43962 = ORIENTED_EDGE ( 'NONE', *, *, #66545, .F. ) ;
#43963 = ADVANCED_FACE ( 'NONE', ( #35694 ), #34997, .T. ) ;
#43964 = CARTESIAN_POINT ( 'NONE',  ( 127.3650620767373738, 37.64047374603843110, -93.43272312347599495 ) ) ;
#43965 = ORIENTED_EDGE ( 'NONE', *, *, #4998, .T. ) ;
#43966 = CARTESIAN_POINT ( 'NONE',  ( -124.7710763417278486, 46.96042092553522451, 3.856429859304379093 ) ) ;
#43967 = CARTESIAN_POINT ( 'NONE',  ( 90.31682503704259091, 20.71196693118262644, 16.91658005194965142 ) ) ;
#43968 = ORIENTED_EDGE ( 'NONE', *, *, #49435, .T. ) ;
#43969 = CARTESIAN_POINT ( 'NONE',  ( 44.01696072965949469, 47.84694004974210912, 43.58025477438756923 ) ) ;
#43970 = LINE ( 'NONE', #65452, #31207 ) ;
#43971 = CARTESIAN_POINT ( 'NONE',  ( 36.09469435220862010, 9.015003538710487874, 30.66481460161145378 ) ) ;
#43972 = CARTESIAN_POINT ( 'NONE',  ( -179.8989115484066303, 96.59045402602905028, -38.98901376945831032 ) ) ;
#43973 = CARTESIAN_POINT ( 'NONE',  ( -128.1384526288949814, 47.98891607499720635, -22.74005215996440299 ) ) ;
#43974 = CARTESIAN_POINT ( 'NONE',  ( 427.4999999999999432, -18.06806526123148160, 0.000000000000000000 ) ) ;
#43976 = ADVANCED_FACE ( 'NONE', ( #61717 ), #19497, .T. ) ;
#43975 =( REPRESENTATION_RELATIONSHIP ('NONE','NONE', #40274, #32051 ) REPRESENTATION_RELATIONSHIP_WITH_TRANSFORMATION ( #27337 )SHAPE_REPRESENTATION_RELATIONSHIP( ) );
#43977 = FACE_OUTER_BOUND ( 'NONE', #30305, .T. ) ;
#43978 = VERTEX_POINT ( 'NONE', #51858 ) ;
#43979 = CARTESIAN_POINT ( 'NONE',  ( 0.000000000000000000, -26.09918303830819397, 30.00000000000000000 ) ) ;
#43981 = EDGE_CURVE ( 'NONE', #68666, #22151, #35341, .T. ) ;
#43980 = CARTESIAN_POINT ( 'NONE',  ( -149.5074843970971017, 65.50121172469319220, -76.65738112195568021 ) ) ;
#43982 = EDGE_LOOP ( 'NONE', ( #6287, #37370, #20773, #50302 ) ) ;
#43983 = VECTOR ( 'NONE', #65878, 1000.000000000000000 ) ;
#43984 = FACE_BOUND ( 'NONE', #23160, .T. ) ;
#43985 = CARTESIAN_POINT ( 'NONE',  ( -4.725257700476004352, 6.708862164351561574, -62.92897752985880544 ) ) ;
#43986 = FILL_AREA_STYLE_COLOUR ( '', #18949 ) ;
#43988 = CARTESIAN_POINT ( 'NONE',  ( 19.71799482800311054, 15.56722426018198036, 0.000000000000000000 ) ) ;
#43987 = AXIS2_PLACEMENT_3D ( 'NONE', #4273, #58409, #53123 ) ;
#43989 = CARTESIAN_POINT ( 'NONE',  ( -44.26023579658940577, 48.10138582123773432, 41.38025477438755928 ) ) ;
#43990 = CYLINDRICAL_SURFACE ( 'NONE', #59086, 7.500000000000013323 ) ;
#43991 = DIRECTION ( 'NONE',  ( 0.000000000000000000, 0.000000000000000000, 1.000000000000000000 ) ) ;
#43992 = LINE ( 'NONE', #750, #48264 ) ;
#43993 = CARTESIAN_POINT ( 'NONE',  ( -123.6618353044034819, 46.23845779494351405, -76.43322633536396893 ) ) ;
#43995 = CARTESIAN_POINT ( 'NONE',  ( -13.77312480593389310, 8.361845410302541026, 33.04005123776303066 ) ) ;
#43994 = VECTOR ( 'NONE', #47280, 1000.000000000000000 ) ;
#43996 = CIRCLE ( 'NONE', #13694, 25.12245591505646303 ) ;
#43997 = CARTESIAN_POINT ( 'NONE',  ( 163.1495034066983294, 62.20479872133084598, 14.98979888773876468 ) ) ;
#43998 = CARTESIAN_POINT ( 'NONE',  ( 93.72687053612524721, 23.04134601640626911, -18.95203141322158658 ) ) ;
#43999 = ORIENTED_EDGE ( 'NONE', *, *, #42106, .T. ) ;
#44000 = CARTESIAN_POINT ( 'NONE',  ( -37.52119286077852678, 11.69341290629619934, 6.476620693246999849 ) ) ;
#44001 = ORIENTED_EDGE ( 'NONE', *, *, #8252, .F. ) ;
#44002 = CARTESIAN_POINT ( 'NONE',  ( -444.4229916354184979, 394.6798985497181320, 96.05029585798874336 ) ) ;
#44003 = CARTESIAN_POINT ( 'NONE',  ( 432.4999999999999432, 207.5000000000000284, 380.0000000000000000 ) ) ;
#44004 = CARTESIAN_POINT ( 'NONE',  ( 103.9212167174977282, 27.16063360973579321, 86.75032792527655090 ) ) ;
#44005 = FACE_OUTER_BOUND ( 'NONE', #10405, .T. ) ;
#44006 = CARTESIAN_POINT ( 'NONE',  ( 68.45098769362923008, 13.99935947269946368, -21.54976275930446405 ) ) ;
#44007 = CONICAL_SURFACE ( 'NONE', #52987, 89.99999999999998579, 1.273485274044415583 ) ;
#44008 = CARTESIAN_POINT ( 'NONE',  ( -23.93895920923072396, 9.495000752338448535, -43.05927999758113600 ) ) ;
#44009 = DIRECTION ( 'NONE',  ( 0.000000000000000000, 0.000000000000000000, 1.000000000000000000 ) ) ;
#44010 = LINE ( 'NONE', #10968, #66777 ) ;
#44011 = CARTESIAN_POINT ( 'NONE',  ( -119.1605144823340225, 43.39823405392969846, -18.88291338966152466 ) ) ;
#44012 = EDGE_LOOP ( 'NONE', ( #13196, #46588 ) ) ;
#44013 = ORIENTED_EDGE ( 'NONE', *, *, #3203, .T. ) ;
#44014 = CARTESIAN_POINT ( 'NONE',  ( 36.99999522780155559, 9.122638774496635961, 57.14919926213968182 ) ) ;
#44015 = CARTESIAN_POINT ( 'NONE',  ( 177.7960900018545090, 75.34533826015461955, 70.39765848647137148 ) ) ;
#44016 = CARTESIAN_POINT ( 'NONE',  ( 110.2429982417149432, 28.88204397445230853, -89.61153874658103291 ) ) ;
#44017 = CARTESIAN_POINT ( 'NONE',  ( 15.55634918610397399, -26.11269837220809364, 0.000000000000000000 ) ) ;
#44018 = CARTESIAN_POINT ( 'NONE',  ( -169.8885678771097787, 85.07765565657315676, -22.14949854782897987 ) ) ;
#44019 = DIRECTION ( 'NONE',  ( -1.000000000000000000, 0.000000000000000000, 0.000000000000000000 ) ) ;
#44020 = ORIENTED_EDGE ( 'NONE', *, *, #57657, .F. ) ;
#44021 = CARTESIAN_POINT ( 'NONE',  ( 110.2429982417149574, 29.99119854320846201, -50.92243756565370916 ) ) ;
#44022 = CARTESIAN_POINT ( 'NONE',  ( 188.2086267457325448, 87.61890531228284829, -19.24083152260686447 ) ) ;
#44023 = CARTESIAN_POINT ( 'NONE',  ( -85.34215807311488788, 24.97769003780923924, -12.34335653950498646 ) ) ;
#44024 = LINE ( 'NONE', #1133, #67777 ) ;
#44025 = PLANE ( 'NONE',  #61071 ) ;
#44026 = CARTESIAN_POINT ( 'NONE',  ( 204.6977192012829789, 106.3443248447423173, -9.481380442157895772 ) ) ;
#44027 = FACE_BOUND ( 'NONE', #19530, .T. ) ;
#44028 = CARTESIAN_POINT ( 'NONE',  ( -61.52143283897135007, 16.51181063611435107, -46.52005420056815410 ) ) ;
#44029 = ORIENTED_EDGE ( 'NONE', *, *, #790, .F. ) ;
#44030 = CARTESIAN_POINT ( 'NONE',  ( -64.83840629396348731, 4.580509716059292913, 170.0000000000000000 ) ) ;
#44031 = CARTESIAN_POINT ( 'NONE',  ( 92.53033045403537926, 22.59263332688195547, -47.97690888582502566 ) ) ;
#44032 = AXIS2_PLACEMENT_3D ( 'NONE', #26752, #37290, #16876 ) ;
#44033 = CARTESIAN_POINT ( 'NONE',  ( -51.13576748034040520, 14.70354244225167406, 58.26138747146119101 ) ) ;
#44034 = CYLINDRICAL_SURFACE ( 'NONE', #1783, 5.000000000000004441 ) ;
#44035 = CARTESIAN_POINT ( 'NONE',  ( 152.8430172091322845, 54.14068524174417973, 4.157737500947386700 ) ) ;
#44036 = CARTESIAN_POINT ( 'NONE',  ( -102.2801239173131194, -170.0000000000000000, -35.01457726497591239 ) ) ;
#44037 = EDGE_CURVE ( 'NONE', #67474, #28312, #40959, .T. ) ;
#44038 = AXIS2_PLACEMENT_3D ( 'NONE', #4880, #5229, #58681 ) ;
#44039 = ORIENTED_EDGE ( 'NONE', *, *, #42778, .F. ) ;
#44040 = CARTESIAN_POINT ( 'NONE',  ( 57.39083379741712321, 11.43779987330584191, 5.482692190092026685 ) ) ;
#44041 = CARTESIAN_POINT ( 'NONE',  ( 0.000000000000000000, 0.000000000000000000, 0.000000000000000000 ) ) ;
#44042 = EDGE_CURVE ( 'NONE', #25434, #40816, #16127, .T. ) ;
#44043 = ORIENTED_EDGE ( 'NONE', *, *, #61822, .T. ) ;
#44044 = CIRCLE ( 'NONE', #49667, 5.000000000000004441 ) ;
#44045 = VERTEX_POINT ( 'NONE', #33183 ) ;
#44046 = LINE ( 'NONE', #65526, #10555 ) ;
#44047 = DIRECTION ( 'NONE',  ( 1.000000000000000000, 0.000000000000000000, 0.000000000000000000 ) ) ;
#44048 = ADVANCED_FACE ( 'NONE', ( #22619 ), #28600, .F. ) ;
#44049 = CARTESIAN_POINT ( 'NONE',  ( 90.30732934992394689, 21.77797012484621320, -63.61215870629216340 ) ) ;
#44050 = VERTEX_POINT ( 'NONE', #1880 ) ;
#44051 = EDGE_CURVE ( 'NONE', #7953, #18463, #34230, .T. ) ;
#44052 = VERTEX_POINT ( 'NONE', #50051 ) ;
#44053 = DIRECTION ( 'NONE',  ( 0.000000000000000000, 1.000000000000000000, 0.000000000000000000 ) ) ;
#44054 = CARTESIAN_POINT ( 'NONE',  ( 164.0105905242218682, 64.23277447906895077, 33.22940987375192634 ) ) ;
#44055 = CARTESIAN_POINT ( 'NONE',  ( -154.0833774771448930, 69.51012195447344766, -63.19600284746142194 ) ) ;
#44056 = CARTESIAN_POINT ( 'NONE',  ( 68.62997155117723480, 15.08415013720829378, 15.46527518503070731 ) ) ;
#44057 = CARTESIAN_POINT ( 'NONE',  ( 4.000000000000012434, 6.928203230275504332, -9.500000000000000000 ) ) ;
#44058 = CARTESIAN_POINT ( 'NONE',  ( 103.1534365798308102, 26.83148826706845824, -14.07784702132055443 ) ) ;
#44059 = CARTESIAN_POINT ( 'NONE',  ( 34.43940527065382895, 66.63700071734666608, 170.0000000000000000 ) ) ;
#44060 = CARTESIAN_POINT ( 'NONE',  ( -133.3799602664182373, 52.86209125874978554, -15.03899668926757549 ) ) ;
#44062 = EDGE_CURVE ( 'NONE', #10495, #15418, #60601, .T. ) ;
#44061 = DIRECTION ( 'NONE',  ( -0.000000000000000000, -0.000000000000000000, -1.000000000000000000 ) ) ;
#44063 = LINE ( 'NONE', #17339, #47268 ) ;
#44064 = CARTESIAN_POINT ( 'NONE',  ( 90.10670619348783816, 20.63680950852241125, 84.24788275468904430 ) ) ;
#44066 = ORIENTED_EDGE ( 'NONE', *, *, #43344, .F. ) ;
#44065 = FACE_OUTER_BOUND ( 'NONE', #5671, .T. ) ;
#44067 = EDGE_LOOP ( 'NONE', ( #42020, #18325, #60866, #56969 ) ) ;
#44068 = EDGE_LOOP ( 'NONE', ( #7075, #14587 ) ) ;
#44069 = CARTESIAN_POINT ( 'NONE',  ( -10.23867141318105745, 7.059827648235816433, -23.19163774689041091 ) ) ;
#44070 = CARTESIAN_POINT ( 'NONE',  ( -165.6444900061506758, 80.61247689992478627, 91.39031826811293513 ) ) ;
#44071 = FACE_OUTER_BOUND ( 'NONE', #49465, .T. ) ;
#44072 = CARTESIAN_POINT ( 'NONE',  ( -4.000000000000013323, 6.928203230275504332, 0.000000000000000000 ) ) ;
#44073 = CARTESIAN_POINT ( 'NONE',  ( -57.42826130032239007, 16.37596353166459906, -49.83430089818286035 ) ) ;
#44074 = LINE ( 'NONE', #13478, #5138 ) ;
#44075 = CARTESIAN_POINT ( 'NONE',  ( -74.19961951691011848, 20.67022044985850826, -75.48968614315221259 ) ) ;
#44076 = CARTESIAN_POINT ( 'NONE',  ( 0.000000000000000000, 0.000000000000000000, -2.499999999999970246 ) ) ;
#44077 = ORIENTED_EDGE ( 'NONE', *, *, #10930, .T. ) ;
#44078 = CARTESIAN_POINT ( 'NONE',  ( -62.31345272479883590, -18.49415068377726357, 40.00000000000003553 ) ) ;
#44079 = ORIENTED_EDGE ( 'NONE', *, *, #14468, .T. ) ;
#44080 = ORIENTED_EDGE ( 'NONE', *, *, #47080, .T. ) ;
#44081 = DIRECTION ( 'NONE',  ( 1.000000000000000000, 0.000000000000000000, 0.000000000000000000 ) ) ;
#44082 = VECTOR ( 'NONE', #68791, 1000.000000000000000 ) ;
#44083 = CARTESIAN_POINT ( 'NONE',  ( 447.3372781065086201, 0.000000000000000000, -1.318389841742373392E-13 ) ) ;
#44084 = FACE_OUTER_BOUND ( 'NONE', #50421, .T. ) ;
#44085 = CARTESIAN_POINT ( 'NONE',  ( 1.313474075707213196, 8.479269695850863542, -9.183279549040157974 ) ) ;
#44086 = CIRCLE ( 'NONE', #17125, 10.00000000000000178 ) ;
#44087 = LINE ( 'NONE', #38477, #30452 ) ;
#44088 = DIRECTION ( 'NONE',  ( 0.000000000000000000, 0.000000000000000000, 1.000000000000000000 ) ) ;
#44089 = CARTESIAN_POINT ( 'NONE',  ( 141.3556389957210229, 47.34429831367557284, -16.38285624325062528 ) ) ;
#44090 = ORIENTED_EDGE ( 'NONE', *, *, #3985, .F. ) ;
#44091 = ORIENTED_EDGE ( 'NONE', *, *, #47160, .F. ) ;
#44092 = ORIENTED_EDGE ( 'NONE', *, *, #51610, .T. ) ;
#44093 = CIRCLE ( 'NONE', #40751, 24.99999999999985434 ) ;
#44094 =( NAMED_UNIT ( * ) PLANE_ANGLE_UNIT ( ) SI_UNIT ( $, .RADIAN. ) );
#44095 = CARTESIAN_POINT ( 'NONE',  ( -9.525868120571907127, 7.007646177566257961, 18.07979315870208481 ) ) ;
#44096 = CARTESIAN_POINT ( 'NONE',  ( 26.99999999999999289, -30.00000000000000355, 15.00000000000000000 ) ) ;
#44097 = AXIS2_PLACEMENT_3D ( 'NONE', #5011, #63768, #21198 ) ;
#44098 = CARTESIAN_POINT ( 'NONE',  ( 55.76298701799387203, 11.10663440745154062, -14.40127503394189645 ) ) ;
#44099 = VECTOR ( 'NONE', #54280, 1000.000000000000000 ) ;
#44100 = FACE_OUTER_BOUND ( 'NONE', #55122, .T. ) ;
#44101 = EDGE_LOOP ( 'NONE', ( #26142, #56499, #16458, #31691 ) ) ;
#44102 = CARTESIAN_POINT ( 'NONE',  ( -4.999999999999936939, 31.11269837220806167, 2.000000000000000000 ) ) ;
#44103 = CARTESIAN_POINT ( 'NONE',  ( 204.3129818922373602, 107.5244029525888294, -78.17048162308530834 ) ) ;
#44104 = CARTESIAN_POINT ( 'NONE',  ( -177.2385321673937710, 68.86478131554724769, 312.4362760962256402 ) ) ;
#44105 = EDGE_CURVE ( 'NONE', #14130, #48350, #51132, .T. ) ;
#44106 = CARTESIAN_POINT ( 'NONE',  ( -1.454841858088672613, 7.566772088227303072, -46.88363903783812248 ) ) ;
#44107 = CARTESIAN_POINT ( 'NONE',  ( 103.1653143050726271, 25.74301230421574971, 12.79924877302471842 ) ) ;
#44108 = CARTESIAN_POINT ( 'NONE',  ( -166.3175803736862406, 79.86140754556167565, 14.64531061278483293 ) ) ;
#44109 = CARTESIAN_POINT ( 'NONE',  ( -81.67992981004169906, 23.49232121719083821, -49.48758314069756636 ) ) ;
#44110 = FACE_BOUND ( 'NONE', #22528, .T. ) ;
#44111 = FACE_OUTER_BOUND ( 'NONE', #33910, .T. ) ;
#44112 = VERTEX_POINT ( 'NONE', #23334 ) ;
#44113 = LINE ( 'NONE', #48334, #21489 ) ;
#44114 = CARTESIAN_POINT ( 'NONE',  ( -126.3508039230933093, 46.79479538767115798, -61.75825448869760947 ) ) ;
#44115 = CARTESIAN_POINT ( 'NONE',  ( -128.7810612886106298, 48.42424427998341940, -49.33947501303506300 ) ) ;
#44116 = CARTESIAN_POINT ( 'NONE',  ( -125.8938041572051105, 47.69968343338781835, -34.91370389823391918 ) ) ;
#44117 = LINE ( 'NONE', #45527, #19856 ) ;
#44118 = VERTEX_POINT ( 'NONE', #65903 ) ;
#44119 = ORIENTED_EDGE ( 'NONE', *, *, #11096, .T. ) ;
#44120 = CARTESIAN_POINT ( 'NONE',  ( -102.2801239173131194, -170.0000000000000000, 38.01907450641511588 ) ) ;
#44121 = CARTESIAN_POINT ( 'NONE',  ( -55.05276343752910151, -170.0000000000000000, -23.37177340799619785 ) ) ;
#44122 = EDGE_CURVE ( 'NONE', #39310, #34701, #32951, .T. ) ;
#44123 = ORIENTED_EDGE ( 'NONE', *, *, #40010, .F. ) ;
#44124 = ORIENTED_EDGE ( 'NONE', *, *, #49141, .T. ) ;
#44125 = VECTOR ( 'NONE', #34100, 1000.000000000000000 ) ;
#44126 = CARTESIAN_POINT ( 'NONE',  ( 31.11269837220809364, 15.55634918610396866, 0.000000000000000000 ) ) ;
#44127 = CARTESIAN_POINT ( 'NONE',  ( 0.000000000000000000, 319.5570082923146060, 14.52694631438418860 ) ) ;
#44128 = ORIENTED_EDGE ( 'NONE', *, *, #4761, .F. ) ;
#44129 = CARTESIAN_POINT ( 'NONE',  ( 113.4418023215250173, 31.50656691678297605, 57.15562911881430352 ) ) ;
#44130 = DIRECTION ( 'NONE',  ( -1.000000000000000000, 0.000000000000000000, 0.000000000000000000 ) ) ;
#44131 = CARTESIAN_POINT ( 'NONE',  ( -71.67841390531691559, 19.78168466957078309, -45.35036129474283229 ) ) ;
#44132 = AXIS2_PLACEMENT_3D ( 'NONE', #16924, #65839, #49273 ) ;
#44133 = ADVANCED_FACE ( 'NONE', ( #24716 ), #14150, .F. ) ;
#44134 = CARTESIAN_POINT ( 'NONE',  ( -102.2801239173131194, 33.91021738430207222, -35.01457726497591239 ) ) ;
#44135 = CARTESIAN_POINT ( 'NONE',  ( 447.3372781065087338, 365.0000000000043769, 113.5502958579838122 ) ) ;
#44136 = AXIS2_PLACEMENT_3D ( 'NONE', #24903, #46334, #67811 ) ;
#44137 = CARTESIAN_POINT ( 'NONE',  ( -54.56685407443681157, 15.59259313022788085, -8.371773407996171201 ) ) ;
#44138 = VERTEX_POINT ( 'NONE', #8183 ) ;
#44139 = VECTOR ( 'NONE', #38409, 1000.000000000000000 ) ;
#44140 = DIRECTION ( 'NONE',  ( -0.8160245890732938934, -0.5780171883497599028, 0.000000000000000000 ) ) ;
#44141 = CIRCLE ( 'NONE', #7109, 21.02500000000000213 ) ;
#44142 = PLANE ( 'NONE',  #17881 ) ;
#44143 = EDGE_CURVE ( 'NONE', #50735, #780, #57254, .T. ) ;
#44144 = CARTESIAN_POINT ( 'NONE',  ( -147.3669217311067996, 63.69361261596463919, -49.50424762432383119 ) ) ;
#44145 = CARTESIAN_POINT ( 'NONE',  ( 417.3372781065091317, 395.0000000000065938, -116.4497041420121661 ) ) ;
#44147 = ORIENTED_EDGE ( 'NONE', *, *, #67936, .F. ) ;
#44146 = DIRECTION ( 'NONE',  ( -0.000000000000000000, 1.000000000000000000, -0.000000000000000000 ) ) ;
#44148 = LINE ( 'NONE', #21317, #17321 ) ;
#44149 = CIRCLE ( 'NONE', #31815, 5.000000000000000000 ) ;
#44150 = EDGE_CURVE ( 'NONE', #46943, #6675, #60093, .T. ) ;
#44151 = EDGE_CURVE ( 'NONE', #56795, #65664, #24370, .T. ) ;
#44152 = ORIENTED_EDGE ( 'NONE', *, *, #36949, .T. ) ;
#44153 = CARTESIAN_POINT ( 'NONE',  ( -144.2188519266539970, 59.82027639618912929, 59.74168973493228663 ) ) ;
#44154 = CYLINDRICAL_SURFACE ( 'NONE', #60380, 7.500000000000013323 ) ;
#44155 = FACE_OUTER_BOUND ( 'NONE', #59051, .T. ) ;
#44156 = DIRECTION ( 'NONE',  ( 0.000000000000000000, -0.9997420440737085912, -0.02271222823333338831 ) ) ;
#44157 = CARTESIAN_POINT ( 'NONE',  ( 85.67138972405901143, 19.09593469918316089, -23.93094700892396887 ) ) ;
#44158 = CARTESIAN_POINT ( 'NONE',  ( 544.6745185807129701, 190.0000000000000000, 34.73878747406611467 ) ) ;
#44159 = CARTESIAN_POINT ( 'NONE',  ( -72.29721455218913206, 19.95276341750015803, 0.000000000000000000 ) ) ;
#44160 = CARTESIAN_POINT ( 'NONE',  ( -9.273616082387997395, -77.77273080542778416, 133.5802547743875550 ) ) ;
#44161 = CARTESIAN_POINT ( 'NONE',  ( -2.645453300864630819E-14, -15.55634918610403616, 0.000000000000000000 ) ) ;
#44162 = EDGE_LOOP ( 'NONE', ( #4247, #60694, #35763, #24178 ) ) ;
#44163 = VERTEX_POINT ( 'NONE', #37663 ) ;
#44164 = CARTESIAN_POINT ( 'NONE',  ( 46.84183314611287585, 9.494161546644496852, 38.39310041101741433 ) ) ;
#44165 = CARTESIAN_POINT ( 'NONE',  ( -90.13282190615392153, -1.844136286507718230E-12, 5.000000000000000000 ) ) ;
#44166 = DIRECTION ( 'NONE',  ( -0.000000000000000000, 1.000000000000000000, -0.000000000000000000 ) ) ;
#44167 = CARTESIAN_POINT ( 'NONE',  ( -190.4968431727838833, 108.8425311198514862, 61.08946333816734153 ) ) ;
#44168 = CARTESIAN_POINT ( 'NONE',  ( 208.5936709733498446, 113.6229123546138169, -50.24872299381472374 ) ) ;
#44169 = CARTESIAN_POINT ( 'NONE',  ( -71.57025115638938928, 20.80908992785613520, -71.93917367057966317 ) ) ;
#44170 = CARTESIAN_POINT ( 'NONE',  ( -109.7647482398635645, 36.74843029291201191, 65.41115726635926819 ) ) ;
#44171 = CARTESIAN_POINT ( 'NONE',  ( -28.81317668042939317, 9.175023678939295380, -49.84668732688152915 ) ) ;
#44172 = DIRECTION ( 'NONE',  ( -1.850169831522831466E-16, 1.000000000000000000, 1.110223024625156294E-16 ) ) ;
#44173 = EDGE_LOOP ( 'NONE', ( #50711, #57696, #51993, #32260 ) ) ;
#44174 = CARTESIAN_POINT ( 'NONE',  ( -25.49247221749737591, 9.706368398275740716, 15.46881133980917333 ) ) ;
#44175 = ORIENTED_EDGE ( 'NONE', *, *, #5238, .F. ) ;
#44176 = FACE_OUTER_BOUND ( 'NONE', #18552, .T. ) ;
#44177 = AXIS2_PLACEMENT_3D ( 'NONE', #8322, #66389, #34369 ) ;
#44178 = CARTESIAN_POINT ( 'NONE',  ( -83.28416304016923277, 24.13400259533326775, 85.66394350348330988 ) ) ;
#44179 = CARTESIAN_POINT ( 'NONE',  ( -83.69653436244857403, 24.30167057287990673, 70.33125617411978681 ) ) ;
#44180 = CARTESIAN_POINT ( 'NONE',  ( 131.6115093721024891, 41.25402743071402512, 29.85055241671198090 ) ) ;
#44181 = CARTESIAN_POINT ( 'NONE',  ( 33.75794032130627187, 8.754084575552406378, 15.53265863234151212 ) ) ;
#44182 = LINE ( 'NONE', #50525, #47933 ) ;
#44183 = DIRECTION ( 'NONE',  ( 0.000000000000000000, 0.000000000000000000, 1.000000000000000000 ) ) ;
#44184 = AXIS2_PLACEMENT_3D ( 'NONE', #34616, #31643, #24744 ) ;
#44185 = DIRECTION ( 'NONE',  ( 0.000000000000000000, -0.000000000000000000, 1.000000000000000000 ) ) ;
#44186 = FACE_OUTER_BOUND ( 'NONE', #51869, .T. ) ;
#44187 = DIRECTION ( 'NONE',  ( 1.387778780781445429E-16, -1.000000000000000000, -3.081487911019577365E-33 ) ) ;
#44189 = EDGE_LOOP ( 'NONE', ( #5401, #27767 ) ) ;
#44188 = EDGE_CURVE ( 'NONE', #50693, #52936, #5316, .T. ) ;
#44190 = DIRECTION ( 'NONE',  ( 1.000000000000000000, 0.000000000000000000, 0.000000000000000000 ) ) ;
#44191 =( NAMED_UNIT ( * ) PLANE_ANGLE_UNIT ( ) SI_UNIT ( $, .RADIAN. ) );
#44192 = CARTESIAN_POINT ( 'NONE',  ( -14.84452950307166041, 8.460866451887698148, 8.117316759835038198 ) ) ;
#44193 = VECTOR ( 'NONE', #31117, 1000.000000000000114 ) ;
#44194 = CARTESIAN_POINT ( 'NONE',  ( 284.7439874972685061, -21.94289037477085813, 1.612903297879183961 ) ) ;
#44195 = CARTESIAN_POINT ( 'NONE',  ( 309.8720357909272707, 20.00000000000003197, 256.6193948016162381 ) ) ;
#44196 = VECTOR ( 'NONE', #35586, 1000.000000000000000 ) ;
#44197 = CARTESIAN_POINT ( 'NONE',  ( 86.33664277319749658, 20.38412364599995641, 83.39993048091545802 ) ) ;
#44198 = EDGE_CURVE ( 'NONE', #19302, #41523, #4621, .T. ) ;
#44199 = AXIS2_PLACEMENT_3D ( 'NONE', #3310, #15250, #63437 ) ;
#44200 = ORIENTED_EDGE ( 'NONE', *, *, #38565, .T. ) ;
#44202 = AXIS2_PLACEMENT_3D ( 'NONE', #33746, #11224, #5601 ) ;
#44201 = DIRECTION ( 'NONE',  ( 0.000000000000000000, 0.000000000000000000, 1.000000000000000000 ) ) ;
#44203 = CARTESIAN_POINT ( 'NONE',  ( -55.15976438495154355, 34.41253982194034933, 3.061616997868437868E-16 ) ) ;
#44204 = CARTESIAN_POINT ( 'NONE',  ( -129.6001310305489369, 48.98284622040326042, 17.79976323783206027 ) ) ;
#44205 = CARTESIAN_POINT ( 'NONE',  ( -31.11269837220812207, -31.11269837220801193, 2.000000000000001776 ) ) ;
#44206 = ITEM_DEFINED_TRANSFORMATION ( 'NONE', 'NONE', #60221,  #66832 ) ;
#44207 = CARTESIAN_POINT ( 'NONE',  ( -167.1169587990081595, 80.68480154570059426, 87.50472330615433236 ) ) ;
#44208 = ORIENTED_EDGE ( 'NONE', *, *, #57109, .T. ) ;
#44209 = DIRECTION ( 'NONE',  ( -0.000000000000000000, -0.000000000000000000, -1.000000000000000000 ) ) ;
#44210 = CARTESIAN_POINT ( 'NONE',  ( -6.840981040171511651, 6.828436339979224279, -8.621995243679700494 ) ) ;
#44211 = EDGE_CURVE ( 'NONE', #32779, #8257, #58093, .T. ) ;
#44212 = CARTESIAN_POINT ( 'NONE',  ( -149.5074843970971017, 64.17983161892348676, -22.96827994102829962 ) ) ;
#44213 = CARTESIAN_POINT ( 'NONE',  ( -0.3732240621745021025, 7.527003275829101447, -68.78330978471883839 ) ) ;
#44214 = ADVANCED_FACE ( 'NONE', ( #42930 ), #15866, .F. ) ;
#44215 = FACE_OUTER_BOUND ( 'NONE', #6434, .T. ) ;
#44216 = ADVANCED_FACE ( 'NONE', ( #9914 ), #734, .F. ) ;
#44217 = EDGE_LOOP ( 'NONE', ( #17421, #51575, #48143, #26469 ) ) ;
#44218 = CARTESIAN_POINT ( 'NONE',  ( 161.0086191018871205, 61.75036325654523495, -90.68964922113312355 ) ) ;
#44219 = CARTESIAN_POINT ( 'NONE',  ( 197.3685896092616190, 96.80423329231987850, -45.44928297951660312 ) ) ;
#44220 = CARTESIAN_POINT ( 'NONE',  ( -94.78138776532239262, 30.24234841992714706, 38.55512063273754109 ) ) ;
#44221 = EDGE_CURVE ( 'NONE', #61334, #49747, #55632, .T. ) ;
#44222 = DIRECTION ( 'NONE',  ( -0.4738686624730094610, 0.8805955318567321166, 0.000000000000000000 ) ) ;
#44224 = VERTEX_POINT ( 'NONE', #33091 ) ;
#44223 = CARTESIAN_POINT ( 'NONE',  ( 112.1009898303695849, 30.86414810229296890, 17.54788357748616789 ) ) ;
#44225 = CARTESIAN_POINT ( 'NONE',  ( 254.4165763529819344, -27.00000000000000355, 138.9999999999999716 ) ) ;
#44226 = EDGE_LOOP ( 'NONE', ( #49016, #7621, #50888, #16718, #829, #66280, #11671, #55237, #66824, #23739 ) ) ;
#44227 = ORIENTED_EDGE ( 'NONE', *, *, #49772, .F. ) ;
#44228 = CARTESIAN_POINT ( 'NONE',  ( -71.21970990337017327, 19.62334883444992784, -16.79706233958787820 ) ) ;
#44229 = DIRECTION ( 'NONE',  ( -0.8118923937861950435, -0.5838071093367415143, 0.000000000000000000 ) ) ;
#44230 = AXIS2_PLACEMENT_3D ( 'NONE', #46535, #41957, #9952 ) ;
#44232 = ORIENTED_EDGE ( 'NONE', *, *, #47080, .F. ) ;
#44231 = CARTESIAN_POINT ( 'NONE',  ( -11.14668121284976543, 8.139398342256731311, -63.03362835402993625 ) ) ;
#44233 = CARTESIAN_POINT ( 'NONE',  ( 164.8886903222557407, 63.65672212134879260, 35.77000457521792498 ) ) ;
#44234 = FACE_BOUND ( 'NONE', #17012, .T. ) ;
#44235 = EDGE_CURVE ( 'NONE', #37998, #65969, #18302, .T. ) ;
#44236 = EDGE_CURVE ( 'NONE', #29725, #43378, #59804, .T. ) ;
#44237 = CARTESIAN_POINT ( 'NONE',  ( 266.9165763529819628, 242.0000000000000000, 128.9999999999999716 ) ) ;
#44238 = VECTOR ( 'NONE', #50091, 1000.000000000000114 ) ;
#44239 = ORIENTED_EDGE ( 'NONE', *, *, #17391, .T. ) ;
#44240 = EDGE_CURVE ( 'NONE', #32425, #41408, #11618, .T. ) ;
#44241 = CARTESIAN_POINT ( 'NONE',  ( -142.8234585218669679, 59.99418748542435509, -92.56481087250594442 ) ) ;
#44242 = AXIS2_PLACEMENT_3D ( 'NONE', #54457, #26714, #22469 ) ;
#44243 = CIRCLE ( 'NONE', #13939, 65.00000000000000000 ) ;
#44244 = DIRECTION ( 'NONE',  ( -1.000000000000000000, 0.000000000000000000, 0.000000000000000000 ) ) ;
#44245 = CARTESIAN_POINT ( 'NONE',  ( 150.6506100456012973, 52.53711661296497226, -94.16253627988041330 ) ) ;
#44246 = AXIS2_PLACEMENT_3D ( 'NONE', #49936, #23227, #44676 ) ;
#44247 = DIRECTION ( 'NONE',  ( -1.000000000000000000, 0.000000000000000000, 0.000000000000000000 ) ) ;
#44248 = CARTESIAN_POINT ( 'NONE',  ( 19.54326199789020890, 7.657220834818547317, 57.86229037013161758 ) ) ;
#44249 = ORIENTED_EDGE ( 'NONE', *, *, #26818, .T. ) ;
#44250 = VERTEX_POINT ( 'NONE', #45027 ) ;
#44251 = ORIENTED_EDGE ( 'NONE', *, *, #7799, .F. ) ;
#44252 = CIRCLE ( 'NONE', #30664, 5.000000000000004441 ) ;
#44253 = CARTESIAN_POINT ( 'NONE',  ( 0.000000000000000000, 0.000000000000000000, 8.000000000000000000 ) ) ;
#44254 = CARTESIAN_POINT ( 'NONE',  ( -48.33978239863299819, 12.98353572341707363, 88.09987427823563166 ) ) ;
#44255 = CYLINDRICAL_SURFACE ( 'NONE', #3286, 65.36598343705435354 ) ;
#44256 = CARTESIAN_POINT ( 'NONE',  ( 429.8372781065087338, 400.0000000000067075, -133.9497041420121377 ) ) ;
#44257 = CARTESIAN_POINT ( 'NONE',  ( -101.1432610527352836, 32.20700799924091484, 84.28889895904916330 ) ) ;
#44258 = DIRECTION ( 'NONE',  ( -2.921639538487254261E-16, -1.134144525784205431E-35, -1.000000000000000000 ) ) ;
#44259 = LINE ( 'NONE', #65740, #7014 ) ;
#44260 = CARTESIAN_POINT ( 'NONE',  ( -4.613603609465520172, 74.86839895266042788, 170.0000000000000000 ) ) ;
#44261 = CARTESIAN_POINT ( 'NONE',  ( 79.82127737190242556, 17.20935440217363066, 60.90020036238115608 ) ) ;
#44262 = VERTEX_POINT ( 'NONE', #55229 ) ;
#44263 = CARTESIAN_POINT ( 'NONE',  ( -173.5143455280199873, 87.56649811480131973, -88.40105834567731335 ) ) ;
#44264 = CARTESIAN_POINT ( 'NONE',  ( 10.01137213834967987, -64.59476928204588830, 3.125053320693562722E-16 ) ) ;
#44265 = VERTEX_POINT ( 'NONE', #38359 ) ;
#44266 = DIRECTION ( 'NONE',  ( -0.000000000000000000, -0.000000000000000000, 1.000000000000000000 ) ) ;
#44267 = DIRECTION ( 'NONE',  ( 1.000000000000000000, 0.000000000000000000, -0.000000000000000000 ) ) ;
#44268 = DIRECTION ( 'NONE',  ( -0.000000000000000000, 1.000000000000000000, -0.000000000000000000 ) ) ;
#44269 = CARTESIAN_POINT ( 'NONE',  ( -118.5151419614604720, 43.00218563933587035, 66.33403389341971490 ) ) ;
#44270 = CARTESIAN_POINT ( 'NONE',  ( -52.66507163626137356, 14.05394608175174653, 18.09895399749082401 ) ) ;
#44271 = CARTESIAN_POINT ( 'NONE',  ( 151.1873096904021452, 52.92629247302096474, -39.52043524289759802 ) ) ;
#44272 = CARTESIAN_POINT ( 'NONE',  ( 161.7006237583813402, 62.31514460450497950, -76.67892487292121473 ) ) ;
#44273 = EDGE_LOOP ( 'NONE', ( #46666, #11039, #2102, #710 ) ) ;
#44274 = DIRECTION ( 'NONE',  ( 0.7071067811865476838, -6.441404958702661839E-16, 0.7071067811865474617 ) ) ;
#44275 = CARTESIAN_POINT ( 'NONE',  ( -18.15845058245935562, -17.18344181019548955, 0.000000000000000000 ) ) ;
#44276 = ORIENTED_EDGE ( 'NONE', *, *, #23826, .F. ) ;
#44277 = LINE ( 'NONE', #66125, #7265 ) ;
#44278 = CARTESIAN_POINT ( 'NONE',  ( -0.4701925031012952338, -38.33111675900010340, 13.32819299319724315 ) ) ;
#44279 = EDGE_LOOP ( 'NONE', ( #39100, #51768, #3908 ) ) ;
#44280 = DIRECTION ( 'NONE',  ( 0.000000000000000000, 0.000000000000000000, 1.000000000000000000 ) ) ;
#44281 = CARTESIAN_POINT ( 'NONE',  ( 155.2870855780214754, 57.23765125306422163, -63.27940277120605828 ) ) ;
#44282 = PLANE ( 'NONE',  #44551 ) ;
#44283 = CARTESIAN_POINT ( 'NONE',  ( -36.11269837220806522, 5.000000000000056843, 2.000000000000001776 ) ) ;
#44284 = EDGE_CURVE ( 'NONE', #12932, #38551, #1790, .T. ) ;
#44285 = ORIENTED_EDGE ( 'NONE', *, *, #38935, .T. ) ;
#44286 = AXIS2_PLACEMENT_3D ( 'NONE', #15402, #48082, #63593 ) ;
#44287 = ORIENTED_EDGE ( 'NONE', *, *, #47863, .T. ) ;
#44288 = CYLINDRICAL_SURFACE ( 'NONE', #811, 4.250000000000000000 ) ;
#44289 = VERTEX_POINT ( 'NONE', #34504 ) ;
#44290 = DIRECTION ( 'NONE',  ( 1.000000000000000000, -0.000000000000000000, -0.000000000000000000 ) ) ;
#44291 = DIRECTION ( 'NONE',  ( 1.000000000000000000, 0.000000000000000000, 0.000000000000000000 ) ) ;
#44292 = AXIS2_PLACEMENT_3D ( 'NONE', #18955, #13672, #12638 ) ;
#44293 = CARTESIAN_POINT ( 'NONE',  ( -5.183193881612056408, 7.740932022135017299, 17.79449844124656011 ) ) ;
#44294 = CARTESIAN_POINT ( 'NONE',  ( 98.48662049252135375, -156.6058287036421461, 10.00000000000000000 ) ) ;
#44295 = VECTOR ( 'NONE', #44274, 1000.000000000000000 ) ;
#44296 = EDGE_CURVE ( 'NONE', #4538, #44045, #21981, .T. ) ;
#44297 = DIRECTION ( 'NONE',  ( 0.3513748240813305279, 0.9362348706397417564, 2.500042656554809847E-16 ) ) ;
#44298 = AXIS2_PLACEMENT_3D ( 'NONE', #31871, #63195, #53651 ) ;
#44299 = CARTESIAN_POINT ( 'NONE',  ( 46.66904755831210139, -9.150666335777657423E-14, 85.00100000000000477 ) ) ;
#44300 = ORIENTED_EDGE ( 'NONE', *, *, #60020, .T. ) ;
#44301 = VECTOR ( 'NONE', #43441, 1000.000000000000000 ) ;
#44302 = EDGE_CURVE ( 'NONE', #20626, #13843, #34316, .T. ) ;
#44303 = CARTESIAN_POINT ( 'NONE',  ( -118.6288898061518609, 41.89286798341289852, -71.14046227876613671 ) ) ;
#44304 = ORIENTED_EDGE ( 'NONE', *, *, #69086, .F. ) ;
#44305 = ADVANCED_FACE ( 'NONE', ( #24636 ), #30252, .F. ) ;
#44306 = ORIENTED_EDGE ( 'NONE', *, *, #42487, .T. ) ;
#44307 = PLANE ( 'NONE',  #10924 ) ;
#44308 = DIRECTION ( 'NONE',  ( -0.9174381082928754205, 0.3978785209734126416, 0.000000000000000000 ) ) ;
#44309 = DIRECTION ( 'NONE',  ( 0.000000000000000000, 0.000000000000000000, 1.000000000000000000 ) ) ;
#44310 = CARTESIAN_POINT ( 'NONE',  ( 141.3403471770513420, 46.13063628128489313, -70.93045427954361060 ) ) ;
#44311 = CARTESIAN_POINT ( 'NONE',  ( 46.66904755831207297, -15.55634918610412853, 2.000000000000001776 ) ) ;
#44312 = ORIENTED_EDGE ( 'NONE', *, *, #36868, .T. ) ;
#44313 = CARTESIAN_POINT ( 'NONE',  ( 80.17205177205137545, 17.31791394718354837, 6.544383460469372693 ) ) ;
#44314 = ORIENTED_EDGE ( 'NONE', *, *, #37286, .F. ) ;
#44315 = CARTESIAN_POINT ( 'NONE',  ( 13.14401442664831166, 6.430459733718342008, 44.53740620683903018 ) ) ;
#44316 = EDGE_LOOP ( 'NONE', ( #57835, #50783, #47012, #37460 ) ) ;
#44317 = CARTESIAN_POINT ( 'NONE',  ( 0.000000000000000000, 0.000000000000000000, 40.00000000000003553 ) ) ;
#44318 = ORIENTED_EDGE ( 'NONE', *, *, #29701, .T. ) ;
#44319 = CARTESIAN_POINT ( 'NONE',  ( -145.3279998500303236, 60.71393190715790666, -75.38937528560870760 ) ) ;
#44320 = DIRECTION ( 'NONE',  ( -0.000000000000000000, -0.000000000000000000, -1.000000000000000000 ) ) ;
#44321 = EDGE_CURVE ( 'NONE', #37971, #47893, #51013, .T. ) ;
#44322 = CARTESIAN_POINT ( 'NONE',  ( 10.55634918610411432, 46.66904755831205875, 85.00100000000000477 ) ) ;
#44323 = EDGE_LOOP ( 'NONE', ( #43754, #19928, #37659, #12156 ) ) ;
#44324 = ADVANCED_FACE ( 'NONE', ( #19685 ), #46070, .T. ) ;
#44325 = CARTESIAN_POINT ( 'NONE',  ( -48.00000000000000711, -20.00000000000000355, 4.000000000000000000 ) ) ;
#44326 = CARTESIAN_POINT ( 'NONE',  ( 70.29000978231910324, 15.51935254053008251, 92.85854150907050553 ) ) ;
#44327 = CARTESIAN_POINT ( 'NONE',  ( 36.08914434112043779, 9.014684630517862729, 44.14699482183696944 ) ) ;
#44328 = CARTESIAN_POINT ( 'NONE',  ( -177.1381400275771796, 93.26609858452819424, -48.56046632885807668 ) ) ;
#44329 = CARTESIAN_POINT ( 'NONE',  ( -132.2199390322348904, 50.80243550247269013, -11.50942145384449766 ) ) ;
#44330 = FACE_OUTER_BOUND ( 'NONE', #50206, .T. ) ;
#44331 = DIRECTION ( 'NONE',  ( -0.000000000000000000, 1.000000000000000000, -0.000000000000000000 ) ) ;
#44332 = ORIENTED_EDGE ( 'NONE', *, *, #49191, .F. ) ;
#44333 = DIRECTION ( 'NONE',  ( 0.000000000000000000, 0.000000000000000000, 1.000000000000000000 ) ) ;
#44334 = DIRECTION ( 'NONE',  ( -0.000000000000000000, -0.000000000000000000, -1.000000000000000000 ) ) ;
#44335 = VERTEX_POINT ( 'NONE', #62611 ) ;
#44336 = CARTESIAN_POINT ( 'NONE',  ( -156.9900125991010498, 72.16580261738673130, -42.89949303315771090 ) ) ;
#44337 = CARTESIAN_POINT ( 'NONE',  ( -2.174378755909785355, 6.588636630831476104, -64.80724674333109192 ) ) ;
#44338 = AXIS2_PLACEMENT_3D ( 'NONE', #2662, #24122, #33637 ) ;
#44339 = CONICAL_SURFACE ( 'NONE', #2793, 89.99999999999998579, 1.273485274044415583 ) ;
#44340 = CARTESIAN_POINT ( 'NONE',  ( -175.9864315813574080, 91.91454246454364352, 58.22230986313539347 ) ) ;
#44341 = CARTESIAN_POINT ( 'NONE',  ( 14.94351112032491002, 7.480372597427133563, -89.20804527961313113 ) ) ;
#44342 = CARTESIAN_POINT ( 'NONE',  ( -122.8011284400168108, 45.68452922414293482, -49.26186152409542274 ) ) ;
#44343 = CARTESIAN_POINT ( 'NONE',  ( 181.0840389613909736, -170.0000000000000000, -9.380507075415927432 ) ) ;
#44344 = CARTESIAN_POINT ( 'NONE',  ( -452.6627218934859798, 400.0000000000064801, -111.4497041420121661 ) ) ;
#44345 = VECTOR ( 'NONE', #2009, 1000.000000000000000 ) ;
#44346 = CARTESIAN_POINT ( 'NONE',  ( 112.5088088673474687, 21.56899521162237576, -4.337361123092376758 ) ) ;
#44347 = CARTESIAN_POINT ( 'NONE',  ( -119.2804658695888236, 43.47213805166349943, -72.80517393614263710 ) ) ;
#44348 = VECTOR ( 'NONE', #30241, 1000.000000000000000 ) ;
#44349 = CARTESIAN_POINT ( 'NONE',  ( -9.524904342798459211, 8.016391612076533946, 30.30652578697153388 ) ) ;
#44350 = CARTESIAN_POINT ( 'NONE',  ( 117.4696399285658686, 32.37118663718647582, 8.193927448285345250 ) ) ;
#44351 = CARTESIAN_POINT ( 'NONE',  ( 151.3976820382521851, -170.0000000000000000, 94.99999999999866418 ) ) ;
#44352 = ORIENTED_EDGE ( 'NONE', *, *, #58111, .F. ) ;
#44353 = CARTESIAN_POINT ( 'NONE',  ( -38.88884187334146247, 11.95889603743730234, 9.875062609561268800 ) ) ;
#44354 = ORIENTED_EDGE ( 'NONE', *, *, #65252, .T. ) ;
#44355 = DIRECTION ( 'NONE',  ( 0.000000000000000000, 0.000000000000000000, 1.000000000000000000 ) ) ;
#44356 = CARTESIAN_POINT ( 'NONE',  ( 79.52639011421919690, 18.17129627604989750, -67.70599084128726020 ) ) ;
#44357 = CARTESIAN_POINT ( 'NONE',  ( 117.0726165202673172, 33.29780331829707762, 87.68152807156005224 ) ) ;
#44358 = CARTESIAN_POINT ( 'NONE',  ( -73.43826238111391547, 8.993593295997464589E-15, 26.24939009510892518 ) ) ;
#44359 = CARTESIAN_POINT ( 'NONE',  ( -14.67600094096871111, 7.434177657339199108, 94.42751904206191682 ) ) ;
#44360 = CARTESIAN_POINT ( 'NONE',  ( -26.88635117726413171, 9.904687797303052932, -36.83709584847830598 ) ) ;
#44361 = PRODUCT_RELATED_PRODUCT_CATEGORY ( 'part', '', ( #62996 ) ) ;
#44362 = CARTESIAN_POINT ( 'NONE',  ( -51.82969867401435948, -54.20961478705483927, 0.000000000000000000 ) ) ;
#44363 = LINE ( 'NONE', #65846, #38685 ) ;
#44364 = CARTESIAN_POINT ( 'NONE',  ( 133.8566784816069344, -170.0000000000000000, 37.01034083899534721 ) ) ;
#44365 = ORIENTED_EDGE ( 'NONE', *, *, #60097, .F. ) ;
#44366 = VERTEX_POINT ( 'NONE', #56984 ) ;
#44367 = EDGE_CURVE ( 'NONE', #67063, #54901, #6919, .T. ) ;
#44368 = DIRECTION ( 'NONE',  ( -0.000000000000000000, -0.000000000000000000, -1.000000000000000000 ) ) ;
#44369 = DIRECTION ( 'NONE',  ( 2.168404344971009361E-16, 0.000000000000000000, -1.000000000000000000 ) ) ;
#44370 = CARTESIAN_POINT ( 'NONE',  ( 0.000000000000000000, 0.000000000000000000, 0.000000000000000000 ) ) ;
#44371 = CARTESIAN_POINT ( 'NONE',  ( -52.00772271844017780, -26.43299457339944425, 27.58472369387556000 ) ) ;
#44372 = ADVANCED_FACE ( 'NONE', ( #14063 ), #3862, .F. ) ;
#44373 = LINE ( 'NONE', #39122, #21743 ) ;
#44374 = DIRECTION ( 'NONE',  ( -0.000000000000000000, 1.000000000000000000, -0.000000000000000000 ) ) ;
#44375 = VERTEX_POINT ( 'NONE', #25328 ) ;
#44376 = CARTESIAN_POINT ( 'NONE',  ( 107.0555969502564437, 28.53646637607230829, -50.22783466578279388 ) ) ;
#44377 = CARTESIAN_POINT ( 'NONE',  ( -11.57808265946730231, 7.164483090579921942, 57.96183666591232253 ) ) ;
#44378 = CARTESIAN_POINT ( 'NONE',  ( -86.15441609607630369, 25.31657638323078174, -16.26595699322537314 ) ) ;
#44379 = CARTESIAN_POINT ( 'NONE',  ( -49.42000000000000171, -26.09918303830819397, 15.41169613715280562 ) ) ;
#44380 = CYLINDRICAL_SURFACE ( 'NONE', #4873, 7.500000000000013323 ) ;
#44381 = CARTESIAN_POINT ( 'NONE',  ( 210.1954643503415241, 114.1986276268023772, -11.87401850716117124 ) ) ;
#44382 = FACE_BOUND ( 'NONE', #2762, .T. ) ;
#44383 = CARTESIAN_POINT ( 'NONE',  ( -60.66241560458681192, 16.25736033771447353, -47.71895337534586190 ) ) ;
#44384 = ADVANCED_FACE ( 'NONE', ( #57675 ), #46765, .F. ) ;
#44385 = AXIS2_PLACEMENT_3D ( 'NONE', #63375, #27105, #53136 ) ;
#44386 = EDGE_CURVE ( 'NONE', #42554, #42825, #20041, .T. ) ;
#44387 = ORIENTED_EDGE ( 'NONE', *, *, #3924, .T. ) ;
#44388 = ADVANCED_FACE ( 'NONE', ( #56279 ), #36215, .T. ) ;
#44389 = DIRECTION ( 'NONE',  ( -0.000000000000000000, 0.000000000000000000, -1.000000000000000000 ) ) ;
#44390 = CARTESIAN_POINT ( 'NONE',  ( 90.30840373526892506, 21.77864858272153725, -49.86167802567979379 ) ) ;
#44391 = AXIS2_PLACEMENT_3D ( 'NONE', #68647, #41922, #52132 ) ;
#44392 = CARTESIAN_POINT ( 'NONE',  ( -48.58011387679029980, 14.07568064779664674, 60.86492917867685293 ) ) ;
#44393 = CARTESIAN_POINT ( 'NONE',  ( 86.62931800182292363, 19.42108912189597092, 44.71208757247933363 ) ) ;
#44394 = CARTESIAN_POINT ( 'NONE',  ( 212.0075063341773784, 118.7912820769029594, 61.84339564076807960 ) ) ;
#44395 = DIRECTION ( 'NONE',  ( -0.000000000000000000, 1.000000000000000000, -0.000000000000000000 ) ) ;
#44396 = VECTOR ( 'NONE', #50864, 1000.000000000000000 ) ;
#44397 = CIRCLE ( 'NONE', #619, 200.0000000000000000 ) ;
#44398 = VERTEX_POINT ( 'NONE', #35173 ) ;
#44399 = LINE ( 'NONE', #65885, #55028 ) ;
#44400 = AXIS2_PLACEMENT_3D ( 'NONE', #27536, #48978, #821 ) ;
#44401 = CARTESIAN_POINT ( 'NONE',  ( -14.35185884954381308, -170.0000000000000000, 94.99999999999866418 ) ) ;
#44402 = EDGE_LOOP ( 'NONE', ( #67755, #12606 ) ) ;
#44403 = CARTESIAN_POINT ( 'NONE',  ( 19.71799482800311054, 15.56722426018198036, 0.000000000000000000 ) ) ;
#44404 = ORIENTED_EDGE ( 'NONE', *, *, #4908, .T. ) ;
#44405 = VECTOR ( 'NONE', #31132, 1000.000000000000000 ) ;
#44406 = DIRECTION ( 'NONE',  ( 0.000000000000000000, 0.000000000000000000, -1.000000000000000000 ) ) ;
#44407 = CARTESIAN_POINT ( 'NONE',  ( -62.50103539982528389, 17.85731685071833752, -16.88267018884844362 ) ) ;
#44408 = CARTESIAN_POINT ( 'NONE',  ( 88.28889510440060917, 21.05995314109331318, -62.84815687393930972 ) ) ;
#44409 = APPLICATION_CONTEXT ( 'automotive_design' ) ;
#44410 = ORIENTED_EDGE ( 'NONE', *, *, #33673, .T. ) ;
#44411 = ORIENTED_EDGE ( 'NONE', *, *, #59142, .T. ) ;
#44412 = CARTESIAN_POINT ( 'NONE',  ( -50.92620509423013431, -55.07344309828844331, 43.58025477438756923 ) ) ;
#44413 = LINE ( 'NONE', #60246, #39376 ) ;
#44414 = CARTESIAN_POINT ( 'NONE',  ( 108.3942953861066627, 29.14039925067523384, 2.982985333465853373 ) ) ;
#44415 = CARTESIAN_POINT ( 'NONE',  ( 69.83260694998128315, 15.39825517924929699, 13.60525356106382766 ) ) ;
#44416 = CYLINDRICAL_SURFACE ( 'NONE', #42150, 75.31295361348102801 ) ;
#44417 = EDGE_CURVE ( 'NONE', #51074, #68125, #30943, .T. ) ;
#44418 = CARTESIAN_POINT ( 'NONE',  ( 109.7732660198864494, 29.77277639096406148, -9.077886975189999319 ) ) ;
#44419 = CARTESIAN_POINT ( 'NONE',  ( -54.08816720029308556, 15.46531105893041591, 18.42599816275528113 ) ) ;
#44420 = CARTESIAN_POINT ( 'NONE',  ( -128.3448054685827344, 49.34430406923177514, -22.66102150948377769 ) ) ;
#44421 = CARTESIAN_POINT ( 'NONE',  ( 14.80291736570134375, 7.477373894757628037, 44.96613339589305269 ) ) ;
#44422 = DIRECTION ( 'NONE',  ( -4.906538933386759377E-15, -0.7071067811865474617, -0.7071067811865474617 ) ) ;
#44423 = B_SPLINE_CURVE_WITH_KNOTS ( 'NONE', 3,
 ( #31271, #14402, #4186, #64913, #9464, #20022, #15082, #41477, #36544, #47085, #52369, #43436, #57993, #67868, #68549, #30232, #63620, #57653, #9812, #41125, #20698, #20350, #35852, #41819, #16707, #46389, #57306, #9116, #36888, #38165, #52698, #19665, #4525, #25990, #30574, #52024, #46740, #47419, #53977, #59606, #5804, #68873, #51681, #42158, #68213, #58323, #11084, #27258 ),
 .UNSPECIFIED., .F., .F.,
 ( 4, 2, 2, 2, 2, 2, 2, 2, 2, 2, 2, 2, 2, 2, 2, 2, 2, 2, 2, 2, 2, 2, 2, 4 ),
 ( 0.000000000000000000, 0.003619254076116462226, 0.004524067595145588733, 0.005428881114174714806, 0.007238508152232894094, 0.008143321671262013228, 0.009048135190291132363, 0.01085776222834935155, 0.01176257574737844466, 0.01266738926640753778, 0.01357220278543663089, 0.01447701630446572400, 0.01538182982349481885, 0.01628664334252390850, 0.01719145686155300334, 0.01809627038058209819, 0.01900108389961118957, 0.01990589741864028095, 0.02171552445669847412, 0.02262033797572757937, 0.02352515149475668810, 0.02533477853281489861, 0.02714440557087311259, 0.02895403260893131964 ),
 .UNSPECIFIED. ) ;
#44424 = CARTESIAN_POINT ( 'NONE',  ( 92.18363589146608206, 21.39143322710240724, 85.85047583112388736 ) ) ;
#44426 = ORIENTED_EDGE ( 'NONE', *, *, #52246, .T. ) ;
#44425 = CARTESIAN_POINT ( 'NONE',  ( 0.000000000000000000, 0.000000000000000000, 41.38025477438755928 ) ) ;
#44427 = ORIENTED_EDGE ( 'NONE', *, *, #10375, .F. ) ;
#44428 = ORIENTED_EDGE ( 'NONE', *, *, #54193, .F. ) ;
#44429 = CARTESIAN_POINT ( 'NONE',  ( -15.32520546926283345, 7.495995523981876296, -15.58064402833840489 ) ) ;
#44430 = CARTESIAN_POINT ( 'NONE',  ( -171.2900812578366754, 86.60412786162308407, 84.73309799929434405 ) ) ;
#44431 = CARTESIAN_POINT ( 'NONE',  ( -52.45215874217870322, 13.99961488531757148, -22.91060012390807543 ) ) ;
#44432 = CARTESIAN_POINT ( 'NONE',  ( -74.69807204964297398, 6.722948167756991111, 43.58025477438756212 ) ) ;
#44433 = CARTESIAN_POINT ( 'NONE',  ( -56.02289203441037557, 15.98631679403370320, -35.26344691231105344 ) ) ;
#44434 = CARTESIAN_POINT ( 'NONE',  ( 90.13282190615606737, 1.839221433318906476E-12, -9.999999999999998224 ) ) ;
#44435 = CARTESIAN_POINT ( 'NONE',  ( 181.0840389613909736, 78.60582251573003987, -36.22505766587961062 ) ) ;
#44436 = CARTESIAN_POINT ( 'NONE',  ( -15.26524495591508845, 7.490231452641283205, 36.63582166737488421 ) ) ;
#44437 = ORIENTED_EDGE ( 'NONE', *, *, #22814, .T. ) ;
#44438 = VECTOR ( 'NONE', #18833, 1000.000000000000227 ) ;
#44439 = PLANE ( 'NONE',  #40756 ) ;
#44440 = ORIENTED_EDGE ( 'NONE', *, *, #38350, .F. ) ;
#44441 = EDGE_LOOP ( 'NONE', ( #12106, #27547, #29705, #34887 ) ) ;
#44442 = CARTESIAN_POINT ( 'NONE',  ( 121.4242852856285566, 0.000000000000000000, -30.00000000000000000 ) ) ;
#44443 = AXIS2_PLACEMENT_3D ( 'NONE', #62007, #18412, #52152 ) ;
#44444 = CARTESIAN_POINT ( 'NONE',  ( -55.26629345812349925, 15.78094189665235980, -88.90542517938722256 ) ) ;
#44445 = CARTESIAN_POINT ( 'NONE',  ( -166.0031475600389115, 80.98114714564768235, 40.70217298635069625 ) ) ;
#44446 = CARTESIAN_POINT ( 'NONE',  ( 116.9197133427646804, 33.22079464767576695, -20.03184353198292911 ) ) ;
#44447 = EDGE_CURVE ( 'NONE', #29231, #11589, #41084, .T. ) ;
#44448 = AXIS2_PLACEMENT_3D ( 'NONE', #42049, #4758, #15666 ) ;
#44449 = CARTESIAN_POINT ( 'NONE',  ( 13.24564585880131773, -63.65041531508827433, 3.061616997868437868E-16 ) ) ;
#44450 = CARTESIAN_POINT ( 'NONE',  ( 0.000000000000000000, 0.000000000000000000, 170.0000000000000000 ) ) ;
#44451 =( GEOMETRIC_REPRESENTATION_CONTEXT ( 3 ) GLOBAL_UNCERTAINTY_ASSIGNED_CONTEXT ( ( #22658 ) ) GLOBAL_UNIT_ASSIGNED_CONTEXT ( ( #50619, #40071, #8770 ) ) REPRESENTATION_CONTEXT ( 'NONE', 'WORKASPACE' ) );
#44452 = CARTESIAN_POINT ( 'NONE',  ( 7.533997733929801655, -64.93035244659006366, 43.58025477438756212 ) ) ;
#44453 = ORIENTED_EDGE ( 'NONE', *, *, #24050, .T. ) ;
#44454 = EDGE_CURVE ( 'NONE', #20522, #51166, #38543, .T. ) ;
#44455 = VERTEX_POINT ( 'NONE', #54001 ) ;
#44456 = VECTOR ( 'NONE', #63466, 999.9999999999998863 ) ;
#44457 = ADVANCED_FACE ( 'NONE', ( #17429 ), #33285, .T. ) ;
#44458 = ORIENTED_EDGE ( 'NONE', *, *, #42021, .F. ) ;
#44459 = PLANE ( 'NONE',  #61935 ) ;
#44460 = VECTOR ( 'NONE', #53846, 1000.000000000000000 ) ;
#44461 = CARTESIAN_POINT ( 'NONE',  ( -12.77647591501652791, 7.263973827022344842, 5.115775066274252936 ) ) ;
#44462 = PLANE ( 'NONE',  #3045 ) ;
#44463 = ADVANCED_FACE ( 'NONE', ( #11112 ), #5828, .T. ) ;
#44464 = CARTESIAN_POINT ( 'NONE',  ( 56.53635105806415595, 11.26263375223563656, -20.16170768551763004 ) ) ;
#44466 = EDGE_CURVE ( 'NONE', #65444, #20075, #59986, .T. ) ;
#44465 = UNCERTAINTY_MEASURE_WITH_UNIT (LENGTH_MEASURE( 1.000000000000000082E-05 ), #3673, 'distance_accuracy_value', 'NONE');
#44467 = CARTESIAN_POINT ( 'NONE',  ( 10.00000000000000000, 1.224646799147353256E-15, 170.0010000000000048 ) ) ;
#44468 = CARTESIAN_POINT ( 'NONE',  ( 204.3091227790963273, 107.5190503136782922, 71.05227132923317868 ) ) ;
#44469 = ORIENTED_EDGE ( 'NONE', *, *, #57267, .F. ) ;
#44470 = CARTESIAN_POINT ( 'NONE',  ( -58.75378739419587504, 16.75118858561005908, -76.10252817049797613 ) ) ;
#44471 = CARTESIAN_POINT ( 'NONE',  ( 200.8303160266298732, 102.8412051751308809, -64.23028300416009984 ) ) ;
#44472 =( NAMED_UNIT ( * ) PLANE_ANGLE_UNIT ( ) SI_UNIT ( $, .RADIAN. ) );
#44473 = CARTESIAN_POINT ( 'NONE',  ( -0.7211439451572430048, 7.539282923622932842, -40.50150818776037909 ) ) ;
#44474 = CARTESIAN_POINT ( 'NONE',  ( 127.7121523762017858, 38.99241938113798511, 94.99999999999866418 ) ) ;
#44475 = CARTESIAN_POINT ( 'NONE',  ( -166.4832242797243964, 80.03142989439328403, -92.40010354986478092 ) ) ;
#44476 = LINE ( 'NONE', #34639, #48646 ) ;
#44477 = CARTESIAN_POINT ( 'NONE',  ( 76.57571471437145760, 0.000000000000000000, -20.00000000000000000 ) ) ;
#44478 = CARTESIAN_POINT ( 'NONE',  ( 211.9975424824651782, -5.943947286559811093E-16, 276.7368757365948113 ) ) ;
#44479 = EDGE_CURVE ( 'NONE', #55507, #13050, #64939, .T. ) ;
#44480 = ORIENTED_EDGE ( 'NONE', *, *, #43501, .T. ) ;
#44481 = LINE ( 'NONE', #169, #48437 ) ;
#44482 = CARTESIAN_POINT ( 'NONE',  ( -133.3765738414514601, 51.62252165471728205, -68.68159762529066370 ) ) ;
#44483 = CARTESIAN_POINT ( 'NONE',  ( -104.1225399044495816, 34.86084180570099278, -76.63309873828038121 ) ) ;
#44484 = CARTESIAN_POINT ( 'NONE',  ( 46.42281973867196143, 9.426811321855161907, -67.31512451460598356 ) ) ;
#44485 = LINE ( 'NONE', #55739, #29895 ) ;
#44486 = ORIENTED_EDGE ( 'NONE', *, *, #48258, .T. ) ;
#44487 = VERTEX_POINT ( 'NONE', #12171 ) ;
#44488 = CARTESIAN_POINT ( 'NONE',  ( 0.3157512944461042803, -3.097794232780332724, -8.000000000000001776 ) ) ;
#44489 = CARTESIAN_POINT ( 'NONE',  ( 180.0913586328219083, 77.60790998934250240, 83.05812134022308157 ) ) ;
#44490 = ORIENTED_EDGE ( 'NONE', *, *, #61188, .T. ) ;
#44491 = AXIS2_PLACEMENT_3D ( 'NONE', #28162, #1096, #40124 ) ;
#44492 = ORIENTED_EDGE ( 'NONE', *, *, #68141, .T. ) ;
#44493 = CARTESIAN_POINT ( 'NONE',  ( 174.6127059037622473, 72.30368563770915102, -47.55541787117397234 ) ) ;
#44494 = CARTESIAN_POINT ( 'NONE',  ( -173.9656771507954431, 88.06879734510549440, -61.55650775521367990 ) ) ;
#44495 = CARTESIAN_POINT ( 'NONE',  ( -15.55634918610408945, -26.11269837220804035, 2.000000000000001776 ) ) ;
#44496 = ORIENTED_EDGE ( 'NONE', *, *, #59844, .F. ) ;
#44497 = DIRECTION ( 'NONE',  ( 0.000000000000000000, 0.000000000000000000, 1.000000000000000000 ) ) ;
#44498 = VECTOR ( 'NONE', #54031, 1000.000000000000000 ) ;
#44499 = CARTESIAN_POINT ( 'NONE',  ( -180.5230320745700681, 95.76406004447549947, 10.22830062411841290 ) ) ;
#44500 = DIRECTION ( 'NONE',  ( -0.000000000000000000, -0.000000000000000000, -1.000000000000000000 ) ) ;
#44501 = CARTESIAN_POINT ( 'NONE',  ( 44.99999999999999289, -20.00000000000000355, 4.000000000000000000 ) ) ;
#44502 = VECTOR ( 'NONE', #13948, 1000.000000000000000 ) ;
#44504 = CARTESIAN_POINT ( 'NONE',  ( 30.83327692011752674, 12.90705744104631947, 6.893342932883484764 ) ) ;
#44503 = CONICAL_SURFACE ( 'NONE', #64736, 74.95140232871122521, 0.8777644062502172329 ) ;
#44505 = CARTESIAN_POINT ( 'NONE',  ( -189.9638655956220816, 108.0957249433520957, 35.19133789206601648 ) ) ;
#44506 =( GEOMETRIC_REPRESENTATION_CONTEXT ( 3 ) GLOBAL_UNCERTAINTY_ASSIGNED_CONTEXT ( ( #69019 ) ) GLOBAL_UNIT_ASSIGNED_CONTEXT ( ( #8331, #29095, #17839 ) ) REPRESENTATION_CONTEXT ( 'NONE', 'WORKASPACE' ) );
#44507 = CIRCLE ( 'NONE', #42250, 24.99999999999985434 ) ;
#44508 = ORIENTED_EDGE ( 'NONE', *, *, #13989, .T. ) ;
#44509 = B_SPLINE_CURVE_WITH_KNOTS ( 'NONE', 3,
 ( #58957, #37160, #52646, #25929, #69167, #37857, #58607, #10772, #53325, #5155, #32242, #21672, #7604, #22372, #54721, #27992, #43812, #55420, #49788, #17438 ),
 .UNSPECIFIED., .F., .F.,
 ( 4, 2, 2, 2, 2, 2, 2, 2, 2, 4 ),
 ( 0.01250143415648050441, 0.01409579223316451656, 0.01489297127150652350, 0.01569015030984852871, 0.01887886646321665363, 0.02047322453990072649, 0.02206758261658480283, 0.02286476165492683926, 0.02366194069326887917, 0.02525629876995295203 ),
 .UNSPECIFIED. ) ;
#44510 = DIRECTION ( 'NONE',  ( 0.000000000000000000, 1.000000000000000000, -0.000000000000000000 ) ) ;
#44511 = CIRCLE ( 'NONE', #31070, 74.95140232871122521 ) ;
#44512 = CARTESIAN_POINT ( 'NONE',  ( -71.57025115638937507, 20.80908992785612455, 8.594478100811356214 ) ) ;
#44513 =( REPRESENTATION_RELATIONSHIP ('NONE','NONE', #46031, #36585 ) REPRESENTATION_RELATIONSHIP_WITH_TRANSFORMATION ( #24169 )SHAPE_REPRESENTATION_RELATIONSHIP( ) );
#44514 = CARTESIAN_POINT ( 'NONE',  ( -146.5230751932348312, 62.99205605665035534, -49.20801219754704192 ) ) ;
#44515 = CARTESIAN_POINT ( 'NONE',  ( -170.2856292770789253, 85.50720222068220266, -76.01299923972814554 ) ) ;
#44517 = EDGE_LOOP ( 'NONE', ( #51307, #40515, #59180, #1434 ) ) ;
#44516 = CARTESIAN_POINT ( 'NONE',  ( -132.3337749658410871, 50.88291293015778649, 87.95154732409349663 ) ) ;
#44518 = DIRECTION ( 'NONE',  ( 0.000000000000000000, 0.000000000000000000, 1.000000000000000000 ) ) ;
#44519 = VERTEX_POINT ( 'NONE', #48724 ) ;
#44521 = ADVANCED_FACE ( 'NONE', ( #60350 ), #16731, .T. ) ;
#44520 = CARTESIAN_POINT ( 'NONE',  ( -142.9728934044261734, 58.82891228489262403, 61.34574771090444756 ) ) ;
#44522 = DIRECTION ( 'NONE',  ( 0.000000000000000000, 0.000000000000000000, 1.000000000000000000 ) ) ;
#44523 = CARTESIAN_POINT ( 'NONE',  ( 442.3372781065085633, 399.9999999999998863, 103.5502958579881891 ) ) ;
#44524 = CARTESIAN_POINT ( 'NONE',  ( 183.1865184929770578, 80.75677158533827082, -24.08296830964977531 ) ) ;
#44525 = CARTESIAN_POINT ( 'NONE',  ( 139.7928618793173143, 45.12615179300589574, -12.08803966520795825 ) ) ;
#44526 = CARTESIAN_POINT ( 'NONE',  ( 41.34269507549199574, 9.685203600174691729, 3.308298053325811949 ) ) ;
#44527 = CARTESIAN_POINT ( 'NONE',  ( 432.4999999999999432, 207.5000000000000284, -2.000000000000000000 ) ) ;
#44528 = LINE ( 'NONE', #44160, #7787 ) ;
#44529 = DIRECTION ( 'NONE',  ( 0.000000000000000000, 0.000000000000000000, 1.000000000000000000 ) ) ;
#44530 = VERTEX_POINT ( 'NONE', #43803 ) ;
#44531 = ORIENTED_EDGE ( 'NONE', *, *, #5550, .T. ) ;
#44532 = CARTESIAN_POINT ( 'NONE',  ( 41.81982603358024875, 8.735900550613191484, 44.53007514971749004 ) ) ;
#44533 = CARTESIAN_POINT ( 'NONE',  ( -55.05276343752909440, 15.72344139423348430, 18.47277718246750311 ) ) ;
#44534 = DIRECTION ( 'NONE',  ( -0.000000000000000000, 1.000000000000000000, -0.000000000000000000 ) ) ;
#44535 = DIRECTION ( 'NONE',  ( 1.000000000000000000, 0.000000000000000000, 0.000000000000000000 ) ) ;
#44536 = CARTESIAN_POINT ( 'NONE',  ( 211.3710169359753763, 117.8057917113659272, -47.26017629441455625 ) ) ;
#44537 = CARTESIAN_POINT ( 'NONE',  ( -71.42546113164834765, 20.75891408601218302, -67.44120922730739665 ) ) ;
#44538 = CARTESIAN_POINT ( 'NONE',  ( 1.500000000000013101, 4.499999999999984013, -3.000000000000029310 ) ) ;
#44539 = DIRECTION ( 'NONE',  ( 0.000000000000000000, 0.000000000000000000, 1.000000000000000000 ) ) ;
#44540 = CARTESIAN_POINT ( 'NONE',  ( 163.7464701930790056, 62.69993100427431898, -74.60574447506652973 ) ) ;
#44541 = PRODUCT_DEFINITION_SHAPE ( 'NONE', 'NONE',  #69592 ) ;
#44542 = ORIENTED_EDGE ( 'NONE', *, *, #36645, .F. ) ;
#44543 = DIRECTION ( 'NONE',  ( -0.000000000000000000, -0.000000000000000000, 1.000000000000000000 ) ) ;
#44544 = ADVANCED_FACE ( 'NONE', ( #1259 ), #65279, .F. ) ;
#44545 = ORIENTED_EDGE ( 'NONE', *, *, #17513, .F. ) ;
#44546 = CARTESIAN_POINT ( 'NONE',  ( 109.9975424824652634, 295.6904194069557548, 539.5330678552892323 ) ) ;
#44547 = CARTESIAN_POINT ( 'NONE',  ( -71.74169950304127497, 19.80353288478602636, 88.65348869463956305 ) ) ;
#44548 = CARTESIAN_POINT ( 'NONE',  ( -85.90441187606242579, 25.21188850826090544, 66.79256356289977248 ) ) ;
#44549 = CARTESIAN_POINT ( 'NONE',  ( 133.8566784816069060, 42.60093787723652525, 44.51034083899536142 ) ) ;
#44550 = DIRECTION ( 'NONE',  ( 3.787294545492198744E-16, 0.6427876096865404731, -0.7660444431189771253 ) ) ;
#44551 = AXIS2_PLACEMENT_3D ( 'NONE', #43928, #22140, #27408 ) ;
#44552 = CARTESIAN_POINT ( 'NONE',  ( 0.000000000000000000, 0.000000000000000000, 0.000000000000000000 ) ) ;
#44553 = EDGE_CURVE ( 'NONE', #33141, #27057, #63109, .T. ) ;
#44554 = CARTESIAN_POINT ( 'NONE',  ( -95.04371414958066566, 30.36527049547256141, -17.70897442121572141 ) ) ;
#44555 = AXIS2_PLACEMENT_3D ( 'NONE', #67270, #52452, #25393 ) ;
#44556 = PLANE ( 'NONE',  #37911 ) ;
#44557 = CARTESIAN_POINT ( 'NONE',  ( 34.30379848636039952, 7.801021882850803557, 85.59205753501402114 ) ) ;
#44558 = DIRECTION ( 'NONE',  ( 0.000000000000000000, 0.000000000000000000, 1.000000000000000000 ) ) ;
#44559 = ORIENTED_EDGE ( 'NONE', *, *, #49435, .F. ) ;
#44560 = CARTESIAN_POINT ( 'NONE',  ( 209.3223706822284100, -1.426547569622074412E-15, 276.7520087653757628 ) ) ;
#44561 = DIRECTION ( 'NONE',  ( -0.000000000000000000, -1.000000000000000000, -0.000000000000000000 ) ) ;
#44562 = CARTESIAN_POINT ( 'NONE',  ( -447.6627218934914367, 399.9999999999998863, -136.4497041420118251 ) ) ;
#44563 = DIRECTION ( 'NONE',  ( 0.000000000000000000, 0.000000000000000000, -1.000000000000000000 ) ) ;
#44564 = CARTESIAN_POINT ( 'NONE',  ( 311.9975424824652350, 170.0000000000000284, 401.6295345748407613 ) ) ;
#44565 = DIRECTION ( 'NONE',  ( -0.000000000000000000, -0.000000000000000000, -1.000000000000000000 ) ) ;
#44566 = CARTESIAN_POINT ( 'NONE',  ( 129.1310456962234809, 39.80382822048402858, -22.52299050009668591 ) ) ;
#44567 = ADVANCED_FACE ( 'NONE', ( #4209 ), #25674, .T. ) ;
#44568 = EDGE_LOOP ( 'NONE', ( #26384, #48288, #21461, #27256 ) ) ;
#44569 = APPLICATION_PROTOCOL_DEFINITION ( 'draft international standard', 'automotive_design', 1998, #50279 ) ;
#44570 = CARTESIAN_POINT ( 'NONE',  ( 183.2136430849848239, 6.000000000000000000, -9.435653166495541200 ) ) ;
#44571 = CARTESIAN_POINT ( 'NONE',  ( -38.45778834351241926, 11.87434869453507247, -40.16219554672893821 ) ) ;
#44572 = CARTESIAN_POINT ( 'NONE',  ( -165.7140086129056442, 80.68381997492572566, -43.42740335534784180 ) ) ;
#44573 = CARTESIAN_POINT ( 'NONE',  ( -172.7827862703479411, 86.75267914668864933, 84.51416791675012519 ) ) ;
#44574 = VERTEX_POINT ( 'NONE', #32577 ) ;
#44575 = CARTESIAN_POINT ( 'NONE',  ( -118.6288898061518609, 41.89286798341291274, -44.29591168830246062 ) ) ;
#44576 = CARTESIAN_POINT ( 'NONE',  ( 75.00000000000000000, 1.249999999999979350, 170.0000000000000000 ) ) ;
#44577 = CARTESIAN_POINT ( 'NONE',  ( -143.7151964745329735, 59.41799441280382155, -20.23954929768048316 ) ) ;
#44578 = CARTESIAN_POINT ( 'NONE',  ( -0.3255842968951683791, 7.525381170773409956, -69.27034146520422553 ) ) ;
#44579 = B_SPLINE_CURVE_WITH_KNOTS ( 'NONE', 3,
 ( #25769, #32067, #68330, #26099, #3957, #68655, #63393, #52814, #69352, #20130, #15883, #53503, #58781, #42276, #9581, #9234, #30689, #41583, #15547, #46508, #31381, #63038, #15199, #25074, #36312, #36998, #68991, #4635, #36659, #31717, #19787, #53149, #26449, #47886, #54187, #16226, #32418, #21848, #49265, #38736, #16916, #32757, #49615, #6008 ),
 .UNSPECIFIED., .F., .F.,
 ( 4, 2, 2, 2, 2, 2, 2, 2, 2, 2, 2, 2, 2, 2, 2, 2, 2, 2, 2, 2, 2, 4 ),
 ( 1.430489624538199204E-17, 0.003433139681083844253, 0.004291424601354751865, 0.005149709521625661646, 0.006866279362167396205, 0.007724564282438266954, 0.008582849202709135969, 0.009441134122980008453, 0.01029941904325087920, 0.01201598888379266580, 0.01373255872433445587, 0.01459084364460534744, 0.01544912856487623554, 0.01630741348514712710, 0.01716569840541801520, 0.01888226824595979486, 0.02059883808650157105, 0.02145712300677249038, 0.02231540792704340276, 0.02403197776758514773, 0.02574854760812689616, 0.02746511744866864113 ),
 .UNSPECIFIED. ) ;
#44580 = CARTESIAN_POINT ( 'NONE',  ( -26.69131247781301752, 59.26697088776972322, 40.00000000000003553 ) ) ;
#44581 = VERTEX_POINT ( 'NONE', #20370 ) ;
#44582 = CARTESIAN_POINT ( 'NONE',  ( -62.30163634902122993, 17.79682011226253380, 8.984685373998656743 ) ) ;
#44583 = CARTESIAN_POINT ( 'NONE',  ( 198.7084915431530021, 98.47675983942190214, -48.34816613409072517 ) ) ;
#44584 = CARTESIAN_POINT ( 'NONE',  ( 31.11269837220809364, 20.55634918610396866, 85.00100000000000477 ) ) ;
#44585 = CARTESIAN_POINT ( 'NONE',  ( 17.74393407086869345, 6.570779001277776032, -35.76153089853740141 ) ) ;
#44587 = ORIENTED_EDGE ( 'NONE', *, *, #49458, .F. ) ;
#44586 = CARTESIAN_POINT ( 'NONE',  ( 110.2429982417149574, 29.99119854320843714, 17.76666361527367499 ) ) ;
#44588 = DIRECTION ( 'NONE',  ( 1.000000000000000000, 0.000000000000000000, 0.000000000000000000 ) ) ;
#44589 = VERTEX_POINT ( 'NONE', #9833 ) ;
#44590 = EDGE_LOOP ( 'NONE', ( #23713, #40425 ) ) ;
#44591 = VECTOR ( 'NONE', #1459, 1000.000000000000000 ) ;
#44592 = CARTESIAN_POINT ( 'NONE',  ( 175.5498284945444425, 74.57669191966279243, 31.72087837615354644 ) ) ;
#44593 = CARTESIAN_POINT ( 'NONE',  ( 15.55634918610406103, 20.55634918610400064, 2.000000000000001776 ) ) ;
#44595 = ORIENTED_EDGE ( 'NONE', *, *, #28514, .T. ) ;
#44594 = DIRECTION ( 'NONE',  ( 0.000000000000000000, 0.000000000000000000, 1.000000000000000000 ) ) ;
#44596 = CARTESIAN_POINT ( 'NONE',  ( -41.50537345350708307, 50.04124777106294886, 170.0000000000000000 ) ) ;
#44597 = LINE ( 'NONE', #17870, #32958 ) ;
#44598 = CARTESIAN_POINT ( 'NONE',  ( -31.43908319763709969, 9.591432048623756756, -89.00629854612920155 ) ) ;
#44599 = AXIS2_PLACEMENT_3D ( 'NONE', #59975, #44510, #43449 ) ;
#44600 = ORIENTED_EDGE ( 'NONE', *, *, #27949, .T. ) ;
#44601 = EDGE_CURVE ( 'NONE', #26798, #38050, #47105, .T. ) ;
#44602 = DIRECTION ( 'NONE',  ( -0.000000000000000000, -0.000000000000000000, 1.000000000000000000 ) ) ;
#44603 = ADVANCED_FACE ( 'NONE', ( #44155 ), #47437, .T. ) ;
#44604 = AXIS2_PLACEMENT_3D ( 'NONE', #38542, #38192, #54353 ) ;
#44605 = CARTESIAN_POINT ( 'NONE',  ( -31.43908319763709969, 9.591432048623758533, -23.47264677473818395 ) ) ;
#44606 = DIRECTION ( 'NONE',  ( -1.000000000000000000, 0.000000000000000000, 0.000000000000000000 ) ) ;
#44607 = CARTESIAN_POINT ( 'NONE',  ( -133.0921934900200085, 52.65587531157185452, 13.39783114184680457 ) ) ;
#44608 = CARTESIAN_POINT ( 'NONE',  ( 22.62427395637551086, 7.823784829753559933, 61.26417510860944304 ) ) ;
#44609 = ORIENTED_EDGE ( 'NONE', *, *, #23229, .T. ) ;
#44610 = ORIENTED_EDGE ( 'NONE', *, *, #19714, .F. ) ;
#44611 = VERTEX_POINT ( 'NONE', #68896 ) ;
#44612 = LINE ( 'NONE', #6629, #48534 ) ;
#44613 = CARTESIAN_POINT ( 'NONE',  ( -106.7004823116342322, 36.22460663120047286, 17.25249706529000449 ) ) ;
#44614 = DIRECTION ( 'NONE',  ( 0.000000000000000000, 0.000000000000000000, 1.000000000000000000 ) ) ;
#44615 = B_SPLINE_CURVE_WITH_KNOTS ( 'NONE', 3,
 ( #68747, #68423, #53602, #47291, #63144, #4733 ),
 .UNSPECIFIED., .F., .F.,
 ( 4, 2, 4 ),
 ( 0.03218938496963300727, 0.06469835385212996393, 0.09720732273462692752 ),
 .UNSPECIFIED. ) ;
#44616 = CARTESIAN_POINT ( 'NONE',  ( -37.38262509017739177, 10.64263598035110547, -38.21638920231944070 ) ) ;
#44617 = CARTESIAN_POINT ( 'NONE',  ( -95.27094040074264569, 29.36050931297059208, 94.39711218672647419 ) ) ;
#44618 = CARTESIAN_POINT ( 'NONE',  ( 6.400000000000000355, 4.618802153517004960, 8.000000000000000000 ) ) ;
#44619 = EDGE_CURVE ( 'NONE', #3113, #11742, #15454, .T. ) ;
#44620 = DIRECTION ( 'NONE',  ( 1.000000000000000000, 0.000000000000000000, 0.000000000000000000 ) ) ;
#44621 = CARTESIAN_POINT ( 'NONE',  ( -71.17984086584780812, 20.67393782512343492, -15.25595357977673139 ) ) ;
#44622 = ORIENTED_EDGE ( 'NONE', *, *, #10339, .F. ) ;
#44623 = CARTESIAN_POINT ( 'NONE',  ( 79.19345177405118363, 17.01649702043280499, 65.06721247038061051 ) ) ;
#44624 = EDGE_CURVE ( 'NONE', #14895, #35197, #33202, .T. ) ;
#44625 = ORIENTED_EDGE ( 'NONE', *, *, #46516, .T. ) ;
#44626 = CARTESIAN_POINT ( 'NONE',  ( 39.40195752203892710, 8.409560354027384221, 44.91383430596327742 ) ) ;
#44627 = FACE_OUTER_BOUND ( 'NONE', #9022, .T. ) ;
#44628 = VERTEX_POINT ( 'NONE', #54354 ) ;
#44629 = CARTESIAN_POINT ( 'NONE',  ( 187.2465631085773907, 85.06582225041682932, 41.11322305146563849 ) ) ;
#44630 = DIRECTION ( 'NONE',  ( 0.000000000000000000, 1.000000000000000000, -0.000000000000000000 ) ) ;
#44631 = DIRECTION ( 'NONE',  ( 0.000000000000000000, 0.000000000000000000, 1.000000000000000000 ) ) ;
#44632 = CARTESIAN_POINT ( 'NONE',  ( -121.1841775822197746, 44.65790002524553870, 59.10701985674870684 ) ) ;
#44633 = CARTESIAN_POINT ( 'NONE',  ( -7.825402957745083654, 6.891034867348166060, 30.11558103944718923 ) ) ;
#44634 = EDGE_CURVE ( 'NONE', #29280, #22360, #16367, .T. ) ;
#44635 = FACE_OUTER_BOUND ( 'NONE', #5768, .T. ) ;
#44636 = DIRECTION ( 'NONE',  ( 0.1785568947986229116, 0.9839295885986321100, 2.500042656554809847E-16 ) ) ;
#44637 = ORIENTED_EDGE ( 'NONE', *, *, #41939, .F. ) ;
#44638 = VECTOR ( 'NONE', #46125, 999.9999999999998863 ) ;
#44639 = CARTESIAN_POINT ( 'NONE',  ( -102.7007063459125789, 32.99469082455791380, -88.70367844590325035 ) ) ;
#44640 = DIRECTION ( 'NONE',  ( 0.000000000000000000, 0.000000000000000000, 1.000000000000000000 ) ) ;
#44641 = ORIENTED_EDGE ( 'NONE', *, *, #53374, .T. ) ;
#44642 = LINE ( 'NONE', #22486, #13983 ) ;
#44643 = CARTESIAN_POINT ( 'NONE',  ( -7.825402957745085430, -170.0000000000000000, 3.271030448983517136 ) ) ;
#44644 = DIRECTION ( 'NONE',  ( -5.295264586242884027E-16, -1.000000000000000000, -1.110223024625156294E-16 ) ) ;
#44645 = ORIENTED_EDGE ( 'NONE', *, *, #3263, .T. ) ;
#44646 = CARTESIAN_POINT ( 'NONE',  ( -85.10774223992956422, 24.88053943842882987, 34.06813972546618174 ) ) ;
#44647 = CARTESIAN_POINT ( 'NONE',  ( 311.8713128290285113, 0.000000000000000000, 346.5826552340383842 ) ) ;
#44648 = CARTESIAN_POINT ( 'NONE',  ( 62.04326772936978784, 12.44884401098615534, -50.67314713297363937 ) ) ;
#44649 = VECTOR ( 'NONE', #4581, 1000.000000000000000 ) ;
#44650 = CARTESIAN_POINT ( 'NONE',  ( -26.87327614295024603, 8.886070347947313763, 70.53135286019491446 ) ) ;
#44651 = EDGE_CURVE ( 'NONE', #9244, #14749, #51196, .T. ) ;
#44652 = AXIS2_PLACEMENT_3D ( 'NONE', #2267, #66992, #32959 ) ;
#44653 = ORIENTED_EDGE ( 'NONE', *, *, #21909, .T. ) ;
#44654 = DIRECTION ( 'NONE',  ( -0.3666659887185691469, 0.8092305634045388052, 0.4590228185711541231 ) ) ;
#44655 = ORIENTED_EDGE ( 'NONE', *, *, #10070, .F. ) ;
#44656 = EDGE_CURVE ( 'NONE', #2120, #15985, #49782, .T. ) ;
#44657 = EDGE_CURVE ( 'NONE', #22785, #1784, #18141, .T. ) ;
#44658 = EDGE_CURVE ( 'NONE', #30339, #30745, #63525, .T. ) ;
#44659 = FACE_OUTER_BOUND ( 'NONE', #38599, .T. ) ;
#44660 = STYLED_ITEM ( 'NONE', ( #52883 ), #62812 ) ;
#44661 = VERTEX_POINT ( 'NONE', #12514 ) ;
#44662 = CARTESIAN_POINT ( 'NONE',  ( 32.66883187925818532, 8.640402022338111721, -19.61546109960840667 ) ) ;
#44663 = CARTESIAN_POINT ( 'NONE',  ( 0.000000000000000000, 6.000000000000000000, -3.000000000000030198 ) ) ;
#44664 = CARTESIAN_POINT ( 'NONE',  ( -4.502148936856955608, 7.704491846230414609, 17.51250421026318094 ) ) ;
#44665 = CARTESIAN_POINT ( 'NONE',  ( -6.840165690716692559, 7.836465889224641046, 57.00902819645234842 ) ) ;
#44666 = CIRCLE ( 'NONE', #41296, 5.000000000000004441 ) ;
#44667 = LINE ( 'NONE', #50979, #8910 ) ;
#44668 = CARTESIAN_POINT ( 'NONE',  ( 5.799999999999999822, 0.000000000000000000, 0.000000000000000000 ) ) ;
#44669 = ORIENTED_EDGE ( 'NONE', *, *, #38594, .F. ) ;
#44670 = DIRECTION ( 'NONE',  ( 1.000000000000000000, 0.000000000000000000, 0.000000000000000000 ) ) ;
#44671 = ORIENTED_EDGE ( 'NONE', *, *, #30440, .T. ) ;
#44672 = CARTESIAN_POINT ( 'NONE',  ( 164.3702714028688376, 63.22112480708620552, -13.82798321502299110 ) ) ;
#44673 = DIRECTION ( 'NONE',  ( -1.000000000000000000, 0.000000000000000000, 0.000000000000000000 ) ) ;
#44674 = CARTESIAN_POINT ( 'NONE',  ( 66.72974708835177182, 13.56459745268607087, 57.62319218809916066 ) ) ;
#44675 = CARTESIAN_POINT ( 'NONE',  ( 136.9934874058117771, 43.35050367224292955, -63.53966939834757000 ) ) ;
#44676 = DIRECTION ( 'NONE',  ( -1.000000000000000000, 0.000000000000000000, 0.000000000000000000 ) ) ;
#44677 = ORIENTED_EDGE ( 'NONE', *, *, #27366, .F. ) ;
#44678 = VERTEX_POINT ( 'NONE', #7598 ) ;
#44679 = CARTESIAN_POINT ( 'NONE',  ( 8.480442907658519047, 6.376693431076495777, 39.21954576350441357 ) ) ;
#44680 = ORIENTED_EDGE ( 'NONE', *, *, #19462, .F. ) ;
#44681 = CARTESIAN_POINT ( 'NONE',  ( 64.69738688745238164, 14.10375742873388560, 71.47051169446849883 ) ) ;
#44682 = DIRECTION ( 'NONE',  ( 0.000000000000000000, 0.000000000000000000, 1.000000000000000000 ) ) ;
#44683 = EDGE_LOOP ( 'NONE', ( #37142, #9769, #53642, #56261 ) ) ;
#44684 = CARTESIAN_POINT ( 'NONE',  ( 86.62931800182293784, 20.48449268398423584, 17.86753698201564688 ) ) ;
#44685 = LINE ( 'NONE', #16893, #27182 ) ;
#44686 = CARTESIAN_POINT ( 'NONE',  ( 31.11269837220806522, 4.999999999999936939, 0.000000000000000000 ) ) ;
#44687 = ORIENTED_EDGE ( 'NONE', *, *, #4761, .T. ) ;
#44688 = AXIS2_PLACEMENT_3D ( 'NONE', #12149, #893, #65620 ) ;
#44689 = LINE ( 'NONE', #66167, #19961 ) ;
#44690 = CARTESIAN_POINT ( 'NONE',  ( 70.50468489774748093, 15.57653925086012769, 91.52810434581883214 ) ) ;
#44691 = EDGE_CURVE ( 'NONE', #21788, #60419, #19739, .T. ) ;
#44692 = DIRECTION ( 'NONE',  ( 0.000000000000000000, 0.000000000000000000, 1.000000000000000000 ) ) ;
#44693 = CARTESIAN_POINT ( 'NONE',  ( 66.94365390260637128, 14.65531706601760042, 30.91923626730180530 ) ) ;
#44694 = CARTESIAN_POINT ( 'NONE',  ( -179.9693807058584980, 96.67690106241352055, -92.83178401929812651 ) ) ;
#44695 = CARTESIAN_POINT ( 'NONE',  ( 154.4550750032601627, 55.34393534448157226, 70.62503253431717098 ) ) ;
#44696 = CARTESIAN_POINT ( 'NONE',  ( 126.5880720616305553, 37.20544379858409911, -68.50076568904083274 ) ) ;
#44697 = ORIENTED_EDGE ( 'NONE', *, *, #5490, .T. ) ;
#44698 = CARTESIAN_POINT ( 'NONE',  ( 200.0000000000000000, 0.000000000000000000, -46.99999999999997158 ) ) ;
#44699 = DIRECTION ( 'NONE',  ( 1.387778780781445922E-16, -1.000000000000000000, -1.232595164407830946E-32 ) ) ;
#44700 = ORIENTED_EDGE ( 'NONE', *, *, #39488, .F. ) ;
#44701 = CARTESIAN_POINT ( 'NONE',  ( 444.9999999999999432, -35.00000000000000000, 2.000000000000000000 ) ) ;
#44702 = CONICAL_SURFACE ( 'NONE', #12167, 65.00000000000000000, 0.7853981633974497223 ) ;
#44703 = CARTESIAN_POINT ( 'NONE',  ( 3.660532965668830130, -7.124194613927636865, -5.418258005348944116E-15 ) ) ;
#44704 = CARTESIAN_POINT ( 'NONE',  ( -35.17718245314462422, 11.25729435722175786, 44.22309306491955283 ) ) ;
#44705 = CARTESIAN_POINT ( 'NONE',  ( -196.7348448768811409, -170.0000000000000000, 92.11166915431037694 ) ) ;
#44706 = DIRECTION ( 'NONE',  ( 0.000000000000000000, 0.000000000000000000, 1.000000000000000000 ) ) ;
#44707 = FACE_OUTER_BOUND ( 'NONE', #55149, .T. ) ;
#44708 = CARTESIAN_POINT ( 'NONE',  ( -55.05276343752909440, 14.68156374112637863, -62.06087458892354647 ) ) ;
#44709 = EDGE_CURVE ( 'NONE', #30492, #56234, #44870, .T. ) ;
#44710 = CARTESIAN_POINT ( 'NONE',  ( -0.3252226420479323310, 7.525368746738509529, -16.56025891687170315 ) ) ;
#44711 = EDGE_CURVE ( 'NONE', #60955, #49158, #23070, .T. ) ;
#44712 = CARTESIAN_POINT ( 'NONE',  ( -15.07533778868020491, 8.482826962130840087, 39.55181792566148857 ) ) ;
#44714 = EDGE_CURVE ( 'NONE', #68321, #12229, #45546, .T. ) ;
#44713 = CARTESIAN_POINT ( 'NONE',  ( 110.7114632166112358, 29.09878355652111992, 2.766663615273642129 ) ) ;
#44715 = CARTESIAN_POINT ( 'NONE',  ( -48.39213801251012370, 14.03057237515049138, -92.93003639517210956 ) ) ;
#44716 = ORIENTED_EDGE ( 'NONE', *, *, #2575, .F. ) ;
#44717 = CARTESIAN_POINT ( 'NONE',  ( -102.2801239173131052, 33.91021738430207222, -50.01457726497594081 ) ) ;
#44718 = ORIENTED_EDGE ( 'NONE', *, *, #32783, .F. ) ;
#44719 = CARTESIAN_POINT ( 'NONE',  ( -439.4229916354183274, 388.0000000000020464, 101.0502958579930066 ) ) ;
#44720 = EDGE_CURVE ( 'NONE', #20626, #26255, #33974, .T. ) ;
#44721 = CARTESIAN_POINT ( 'NONE',  ( 79.63513233364423627, 18.20496177163923690, -72.88516583624812029 ) ) ;
#44722 = CARTESIAN_POINT ( 'NONE',  ( 46.64694836521738353, 9.462741877720629802, 62.30350966403887725 ) ) ;
#44723 = DIRECTION ( 'NONE',  ( -0.8160245890732938934, -0.5780171883497599028, 0.000000000000000000 ) ) ;
#44724 = DIRECTION ( 'NONE',  ( -1.000000000000000000, 0.000000000000000000, 0.000000000000000000 ) ) ;
#44725 = ADVANCED_FACE ( 'NONE', ( #28335 ), #7933, .F. ) ;
#44726 = DIRECTION ( 'NONE',  ( 0.000000000000000000, 0.000000000000000000, -1.000000000000000000 ) ) ;
#44727 = CARTESIAN_POINT ( 'NONE',  ( 61.40682472845701767, 13.33642729942792649, -89.57322748555588987 ) ) ;
#44728 = CARTESIAN_POINT ( 'NONE',  ( -119.9771613955297624, 43.90337778233484300, -20.18511414558994943 ) ) ;
#44729 = ORIENTED_EDGE ( 'NONE', *, *, #29550, .T. ) ;
#44730 = ORIENTED_EDGE ( 'NONE', *, *, #35558, .T. ) ;
#44731 = DIRECTION ( 'NONE',  ( 0.000000000000000000, -1.000000000000000000, 0.000000000000000000 ) ) ;
#44732 = DIRECTION ( 'NONE',  ( 0.000000000000000000, 1.000000000000000000, 0.000000000000000000 ) ) ;
#44733 = CARTESIAN_POINT ( 'NONE',  ( 41.04173437458232598, 8.628130879747104132, -89.47880143737668845 ) ) ;
#44734 = CARTESIAN_POINT ( 'NONE',  ( -165.9121868482145601, 80.88751546905562861, 63.07590250008146882 ) ) ;
#44735 = B_SPLINE_CURVE_WITH_KNOTS ( 'NONE', 3,
 ( #12406, #39480, #54953, #60936, #60240, #61633 ),
 .UNSPECIFIED., .F., .F.,
 ( 4, 2, 4 ),
 ( 1.095770181116721450E-06, 0.03239442681617712289, 0.06478775786217312593 ),
 .UNSPECIFIED. ) ;
#44736 = CARTESIAN_POINT ( 'NONE',  ( -172.7173255566597163, 88.18461381371099606, -22.86740657428632773 ) ) ;
#44737 = CARTESIAN_POINT ( 'NONE',  ( 109.9975424824652634, 172.0000000000000284, 536.6193948016162949 ) ) ;
#44738 = ORIENTED_EDGE ( 'NONE', *, *, #7935, .T. ) ;
#44739 = EDGE_CURVE ( 'NONE', #47893, #42894, #7240, .T. ) ;
#44740 = EDGE_CURVE ( 'NONE', #64346, #13447, #55063, .T. ) ;
#44741 = CARTESIAN_POINT ( 'NONE',  ( 108.3942953861066485, 29.14039925067522319, -50.70611584746151834 ) ) ;
#44742 = CARTESIAN_POINT ( 'NONE',  ( 16.77104078056616032, 7.540619757007627655, -35.56757450759191386 ) ) ;
#44743 = CARTESIAN_POINT ( 'NONE',  ( -85.46258339457288855, 25.02772366257409686, -18.95299861283113074 ) ) ;
#44744 = LINE ( 'NONE', #28919, #68937 ) ;
#44745 = CARTESIAN_POINT ( 'NONE',  ( 212.0047492081760083, 116.9348962082588343, -18.70236844209925309 ) ) ;
#44746 = FACE_BOUND ( 'NONE', #9985, .T. ) ;
#44747 = ADVANCED_FACE ( 'NONE', ( #29385 ), #1773, .T. ) ;
#44748 = CARTESIAN_POINT ( 'NONE',  ( -62.45356936877016096, 16.79156452995240656, -43.95760844768815190 ) ) ;
#44749 = VECTOR ( 'NONE', #64459, 1000.000000000000000 ) ;
#44750 = EDGE_LOOP ( 'NONE', ( #68121, #25067, #66950, #66747, #59828, #35430 ) ) ;
#44751 = VECTOR ( 'NONE', #20693, 1000.000000000000000 ) ;
#44752 = FACE_OUTER_BOUND ( 'NONE', #29966, .T. ) ;
#44753 = DIRECTION ( 'NONE',  ( -0.000000000000000000, -0.000000000000000000, -1.000000000000000000 ) ) ;
#44754 = DIRECTION ( 'NONE',  ( -0.000000000000000000, 1.000000000000000000, -0.000000000000000000 ) ) ;
#44755 = DIRECTION ( 'NONE',  ( -0.000000000000000000, -1.000000000000000000, -0.000000000000000000 ) ) ;
#44756 = CARTESIAN_POINT ( 'NONE',  ( 212.0803491126036704, 118.9047894217573287, 64.91680770945086465 ) ) ;
#44757 = LINE ( 'NONE', #27874, #49044 ) ;
#44758 = AXIS2_PLACEMENT_3D ( 'NONE', #53759, #661, #22111 ) ;
#44759 = ORIENTED_EDGE ( 'NONE', *, *, #39557, .T. ) ;
#44760 = CARTESIAN_POINT ( 'NONE',  ( 62.04326772936978784, 12.44884401098615534, 3.015954047953714579 ) ) ;
#44761 = CARTESIAN_POINT ( 'NONE',  ( -60.97727891098333686, 16.35024395194892932, 60.03668883463657124 ) ) ;
#44762 = VERTEX_POINT ( 'NONE', #50148 ) ;
#44763 = DIRECTION ( 'NONE',  ( 0.000000000000000000, 0.000000000000000000, -1.000000000000000000 ) ) ;
#44764 = EDGE_LOOP ( 'NONE', ( #59766, #13708, #3891, #50108 ) ) ;
#44765 = CARTESIAN_POINT ( 'NONE',  ( 51.85299110299497016, -39.21848821248376282, 43.58025477438756923 ) ) ;
#44766 = DIRECTION ( 'NONE',  ( 0.000000000000000000, -1.000000000000000000, 0.000000000000000000 ) ) ;
#44767 = CARTESIAN_POINT ( 'NONE',  ( 93.08073375333746924, 22.79826000593200774, -73.99913914800674775 ) ) ;
#44768 = VERTEX_POINT ( 'NONE', #66354 ) ;
#44769 = ORIENTED_EDGE ( 'NONE', *, *, #6435, .T. ) ;
#44770 = CARTESIAN_POINT ( 'NONE',  ( 42.71680114082827373, 9.880016734137541334, 71.00390679014272166 ) ) ;
#44771 = DIRECTION ( 'NONE',  ( 0.3090169943749446757, 0.9510565162951544194, 0.000000000000000000 ) ) ;
#44772 = CARTESIAN_POINT ( 'NONE',  ( -156.9232798886536671, 72.10386843399172108, -70.31426418089215247 ) ) ;
#44773 = CARTESIAN_POINT ( 'NONE',  ( 70.41705859591012029, 15.55317472777717747, 9.231046305453860512 ) ) ;
#44774 = DIRECTION ( 'NONE',  ( -0.04486483035050447404, -0.9989930665413151445, 0.000000000000000000 ) ) ;
#44775 = ORIENTED_EDGE ( 'NONE', *, *, #58138, .F. ) ;
#44776 = CYLINDRICAL_SURFACE ( 'NONE', #39088, 65.36598343705435354 ) ;
#44777 = EDGE_CURVE ( 'NONE', #36599, #27671, #6881, .T. ) ;
#44778 = CARTESIAN_POINT ( 'NONE',  ( -50.53243683205841563, 14.55237037207940531, 16.97720090376005686 ) ) ;
#44779 = CARTESIAN_POINT ( 'NONE',  ( -130.5811943660945076, 50.88295841537573239, -21.44378994887165391 ) ) ;
#44780 = CARTESIAN_POINT ( 'NONE',  ( -31.90315521289066680, -56.64813493366048647, 3.061616997868437868E-16 ) ) ;
#44781 = CARTESIAN_POINT ( 'NONE',  ( 112.1012908502484464, 29.75117929736499889, -23.84786912706831785 ) ) ;
#44782 = FACE_OUTER_BOUND ( 'NONE', #20424, .T. ) ;
#44784 = ORIENTED_EDGE ( 'NONE', *, *, #53599, .T. ) ;
#44783 = DIRECTION ( 'NONE',  ( 0.000000000000000000, 0.000000000000000000, 1.000000000000000000 ) ) ;
#44785 = ORIENTED_EDGE ( 'NONE', *, *, #36605, .T. ) ;
#44786 = EDGE_LOOP ( 'NONE', ( #19849, #45671, #13753, #50488 ) ) ;
#44787 = CARTESIAN_POINT ( 'NONE',  ( -17.90772993695011550, -72.84144224619156205, 170.0000000000000000 ) ) ;
#44788 = CARTESIAN_POINT ( 'NONE',  ( 175.0696098417090809, 74.11936424544845181, 5.476034315764515270 ) ) ;
#44789 = CARTESIAN_POINT ( 'NONE',  ( -49.43915770973591606, 13.24768844696975023, -10.87398376146266799 ) ) ;
#44790 = CARTESIAN_POINT ( 'NONE',  ( 103.8317086685000135, 26.02720265156214197, -12.67800310554697241 ) ) ;
#44791 = CARTESIAN_POINT ( 'NONE',  ( 199.3671895066314903, 99.30947926630329903, 4.562958843833921030 ) ) ;
#44792 = EDGE_CURVE ( 'NONE', #17510, #56697, #40290, .T. ) ;
#44793 = CARTESIAN_POINT ( 'NONE',  ( 203.9193081356078494, 106.9838505030258489, 82.93253388923811542 ) ) ;
#44794 = CARTESIAN_POINT ( 'NONE',  ( 110.2429982417149574, -170.0000000000000000, -70.26698815611737814 ) ) ;
#44795 = CYLINDRICAL_SURFACE ( 'NONE', #15182, 7.500000000000013323 ) ;
#44796 = CARTESIAN_POINT ( 'NONE',  ( -10.23402954931276554, 7.059791383763806216, 44.72254900470105810 ) ) ;
#44797 = ORIENTED_EDGE ( 'NONE', *, *, #12454, .F. ) ;
#44798 = CARTESIAN_POINT ( 'NONE',  ( 3.000000000000003997, 1.500000000000015321, -48.49999999999998579 ) ) ;
#44799 = ORIENTED_EDGE ( 'NONE', *, *, #15811, .F. ) ;
#44800 = EDGE_CURVE ( 'NONE', #13434, #13335, #12872, .T. ) ;
#44801 = VERTEX_POINT ( 'NONE', #50840 ) ;
#44802 = VECTOR ( 'NONE', #29709, 1000.000000000000000 ) ;
#44803 = ADVANCED_FACE ( 'NONE', ( #24119 ), #8503, .T. ) ;
#44804 = CARTESIAN_POINT ( 'NONE',  ( -147.7895256390024201, 64.04409735547015714, 18.73124213477483480 ) ) ;
#44805 = CARTESIAN_POINT ( 'NONE',  ( 0.000000000000000000, -6.928203230275503444, 4.000000000000010658 ) ) ;
#44806 = CARTESIAN_POINT ( 'NONE',  ( -38.92978047220073279, 11.96698587041122330, 91.90144494392491481 ) ) ;
#44807 = CARTESIAN_POINT ( 'NONE',  ( 0.6543471694412384965, 8.859816792613651515, -9.003584543331202283 ) ) ;
#44808 = AXIS2_PLACEMENT_3D ( 'NONE', #1756, #40079, #45704 ) ;
#44809 = VECTOR ( 'NONE', #22125, 1000.000000000000114 ) ;
#44810 = FACE_OUTER_BOUND ( 'NONE', #4769, .T. ) ;
#44811 = CARTESIAN_POINT ( 'NONE',  ( 39.40195752203892710, 8.409560354027389550, 18.06928371549960133 ) ) ;
#44812 = DIRECTION ( 'NONE',  ( 0.000000000000000000, 0.000000000000000000, -1.000000000000000000 ) ) ;
#44813 = VERTEX_POINT ( 'NONE', #67042 ) ;
#44814 = ORIENTED_EDGE ( 'NONE', *, *, #64725, .F. ) ;
#44815 = ORIENTED_EDGE ( 'NONE', *, *, #21365, .T. ) ;
#44816 = CARTESIAN_POINT ( 'NONE',  ( 313.9975424824652350, 170.0000000000000284, 256.6193948016162381 ) ) ;
#44817 = CARTESIAN_POINT ( 'NONE',  ( -15.26524495591508845, 7.490231452641285870, 9.791271076911209903 ) ) ;
#44818 = DIRECTION ( 'NONE',  ( -0.9639628606958512425, -0.2660368455666826670, 0.000000000000000000 ) ) ;
#44819 = DIRECTION ( 'NONE',  ( -0.000000000000000000, 0.001173758924898823768, 0.9999993111447559313 ) ) ;
#44820 = CARTESIAN_POINT ( 'NONE',  ( -52.68007207639879397, 14.05813534436549972, 30.69840203706294446 ) ) ;
#44821 = CARTESIAN_POINT ( 'NONE',  ( 199.7291770695760817, 101.4092159658447088, 69.17564586952617844 ) ) ;
#44822 = ORIENTED_EDGE ( 'NONE', *, *, #5906, .T. ) ;
#44823 = CARTESIAN_POINT ( 'NONE',  ( 1.951563910473907981E-14, 0.000000000000000000, -144.4497041420118251 ) ) ;
#44824 = CARTESIAN_POINT ( 'NONE',  ( 204.6977192012829789, 108.0580384837235073, -63.17048162308526571 ) ) ;
#44825 =( LENGTH_UNIT ( ) NAMED_UNIT ( * ) SI_UNIT ( .MILLI., .METRE. ) );
#44826 = CARTESIAN_POINT ( 'NONE',  ( -4.072522659361693442, 7.683023425615342461, -49.41625453459061390 ) ) ;
#44827 = CARTESIAN_POINT ( 'NONE',  ( -166.3188283541503267, 79.86268666707380248, 8.306259562134265195 ) ) ;
#44828 = DIRECTION ( 'NONE',  ( 0.7071067811865474617, 0.000000000000000000, -0.7071067811865476838 ) ) ;
#44830 = EDGE_CURVE ( 'NONE', #63892, #64521, #61733, .T. ) ;
#44829 = FACE_BOUND ( 'NONE', #24709, .T. ) ;
#44831 = DIRECTION ( 'NONE',  ( -1.000000000000000000, -0.000000000000000000, -0.000000000000000000 ) ) ;
#44832 = ORIENTED_EDGE ( 'NONE', *, *, #31868, .F. ) ;
#44833 = CARTESIAN_POINT ( 'NONE',  ( 275.3198800741404284, 21.92942769035742145, 1.767193244627905946 ) ) ;
#44834 = LINE ( 'NONE', #23036, #39746 ) ;
#44835 = DIRECTION ( 'NONE',  ( -0.000000000000000000, 0.000000000000000000, 1.000000000000000000 ) ) ;
#44836 = DIRECTION ( 'NONE',  ( 0.4578834044730072383, 0.000000000000000000, -0.8890122540821405739 ) ) ;
#44837 = DIRECTION ( 'NONE',  ( 0.9009688679024218105, -0.4338837391175525693, 0.000000000000000000 ) ) ;
#44838 = ORIENTED_EDGE ( 'NONE', *, *, #16095, .F. ) ;
#44839 = CARTESIAN_POINT ( 'NONE',  ( 187.9868792055843585, 85.87520301053052663, 93.45502771267183562 ) ) ;
#44840 = ORIENTED_EDGE ( 'NONE', *, *, #62074, .T. ) ;
#44841 = VERTEX_POINT ( 'NONE', #36050 ) ;
#44842 = PLANE ( 'NONE',  #465 ) ;
#44843 = CARTESIAN_POINT ( 'NONE',  ( -178.7458319892713803, 93.61502008198020519, -64.08897040876379947 ) ) ;
#44844 = DIRECTION ( 'NONE',  ( -1.000000000000000000, -0.000000000000000000, -0.000000000000000000 ) ) ;
#44845 = ORIENTED_EDGE ( 'NONE', *, *, #54386, .T. ) ;
#44846 = CARTESIAN_POINT ( 'NONE',  ( 115.7731501832036400, 32.64791439093736614, 58.86561899071531911 ) ) ;
#44847 = VECTOR ( 'NONE', #25136, 1000.000000000000000 ) ;
#44848 = DIRECTION ( 'NONE',  ( -0.3090169943749447312, -0.9510565162951544194, 0.000000000000000000 ) ) ;
#44849 = LINE ( 'NONE', #66333, #39843 ) ;
#44850 = CARTESIAN_POINT ( 'NONE',  ( -5.000000000000026645, -10.55634918610403439, 0.000000000000000000 ) ) ;
#44851 = PLANE ( 'NONE',  #42831 ) ;
#44852 = EDGE_CURVE ( 'NONE', #13054, #10843, #36616, .T. ) ;
#44853 = CARTESIAN_POINT ( 'NONE',  ( -47.65155309726506516, 13.85482731128120193, -17.11044809809313705 ) ) ;
#44854 = EDGE_CURVE ( 'NONE', #60938, #49516, #4041, .T. ) ;
#44855 = ADVANCED_FACE ( 'NONE', ( #9314 ), #50070, .T. ) ;
#44856 = VERTEX_POINT ( 'NONE', #20904 ) ;
#44857 = CARTESIAN_POINT ( 'NONE',  ( 29.99999999999999645, 26.99999999999999289, 0.000000000000000000 ) ) ;
#44858 = ADVANCED_FACE ( 'NONE', ( #57506, #25510, #51542, #57164, #31129 ), #46591, .T. ) ;
#44859 = PLANE ( 'NONE',  #34815 ) ;
#44860 = CARTESIAN_POINT ( 'NONE',  ( 44.34263167748004264, 9.103379693481560508, -48.78358003831574052 ) ) ;
#44861 = DIRECTION ( 'NONE',  ( 0.000000000000000000, -1.000000000000000000, 0.000000000000000000 ) ) ;
#44863 = EDGE_LOOP ( 'NONE', ( #13991, #14334, #57171, #35457, #63364 ) ) ;
#44862 = CARTESIAN_POINT ( 'NONE',  ( -132.7788241241227070, 51.19755864769842901, 88.81639056320175030 ) ) ;
#44864 = CARTESIAN_POINT ( 'NONE',  ( 0.000000000000000000, 0.000000000000000000, 30.00000000000000000 ) ) ;
#44865 = EDGE_CURVE ( 'NONE', #31241, #16169, #51875, .T. ) ;
#44866 = AXIS2_PLACEMENT_3D ( 'NONE', #51622, #14670, #24895 ) ;
#44867 = ORIENTED_EDGE ( 'NONE', *, *, #40753, .T. ) ;
#44868 = CARTESIAN_POINT ( 'NONE',  ( -142.3393481102175997, 58.33014244976925511, 62.84203394820867317 ) ) ;
#44869 = CARTESIAN_POINT ( 'NONE',  ( 81.76212856587198985, 18.87332718082997474, 31.50068684092350324 ) ) ;
#44870 = LINE ( 'NONE', #29054, #44438 ) ;
#44871 = B_SPLINE_CURVE_WITH_KNOTS ( 'NONE', 3,
 ( #45530, #24441, #45881, #18802, #19841, #13531, #34984, #40596 ),
 .UNSPECIFIED., .F., .F.,
 ( 4, 2, 2, 4 ),
 ( 0.004673709593152186939, 0.005837709341827670290, 0.007001709090503154508, 0.009329708587854118607 ),
 .UNSPECIFIED. ) ;
#44872 = DIRECTION ( 'NONE',  ( 0.000000000000000000, 0.000000000000000000, -1.000000000000000000 ) ) ;
#44873 = CARTESIAN_POINT ( 'NONE',  ( 137.4117721579687839, 43.61242559081430414, -10.05773480556120525 ) ) ;
#44874 = DIRECTION ( 'NONE',  ( 0.000000000000000000, -1.877893248421448789E-16, 1.000000000000000000 ) ) ;
#44875 = CARTESIAN_POINT ( 'NONE',  ( -180.6021503146988891, 97.45669259943416307, -14.74712103546458764 ) ) ;
#44876 = FACE_OUTER_BOUND ( 'NONE', #52446, .T. ) ;
#44877 = EDGE_LOOP ( 'NONE', ( #30366, #16041, #19390, #40216 ) ) ;
#44878 = EDGE_CURVE ( 'NONE', #30296, #4017, #17888, .T. ) ;
#44879 = ORIENTED_EDGE ( 'NONE', *, *, #33196, .T. ) ;
#44880 = ADVANCED_FACE ( 'NONE', ( #36744 ), #58187, .F. ) ;
#44881 = CARTESIAN_POINT ( 'NONE',  ( 45.90693067088658097, 9.344800815249328707, 41.17893080460214605 ) ) ;
#44882 = DIRECTION ( 'NONE',  ( 1.000000000000000000, 0.000000000000000000, 0.000000000000000000 ) ) ;
#44883 = DIRECTION ( 'NONE',  ( 0.000000000000000000, 0.000000000000000000, -1.000000000000000000 ) ) ;
#44884 = LINE ( 'NONE', #61060, #35566 ) ;
#44885 = CARTESIAN_POINT ( 'NONE',  ( -75.00452312211126582, 22.03104735285382176, -76.00973837158169033 ) ) ;
#44886 = CARTESIAN_POINT ( 'NONE',  ( -106.6781182590523684, 35.07133425426474815, 70.95721658968783174 ) ) ;
#44887 = CARTESIAN_POINT ( 'NONE',  ( -30.47069031368416958, 9.433993659086578276, -50.27049686049341659 ) ) ;
#44888 = CARTESIAN_POINT ( 'NONE',  ( -78.66644367742111399, -170.0000000000000000, -35.11545063171788428 ) ) ;
#44889 = VERTEX_POINT ( 'NONE', #43721 ) ;
#44890 = ORIENTED_EDGE ( 'NONE', *, *, #65264, .F. ) ;
#44891 = EDGE_LOOP ( 'NONE', ( #47797, #68870, #24, #13864 ) ) ;
#44892 = LINE ( 'NONE', #44546, #47600 ) ;
#44893 = DIRECTION ( 'NONE',  ( -0.000000000000000000, 1.000000000000000000, -0.000000000000000000 ) ) ;
#44894 = CARTESIAN_POINT ( 'NONE',  ( -85.45399718454960691, 25.02415453493130926, 67.96308648905946370 ) ) ;
#44895 = CARTESIAN_POINT ( 'NONE',  ( 32.12337157895397866, 7.574134358465434147, -95.00000000000133582 ) ) ;
#44896 = CARTESIAN_POINT ( 'NONE',  ( 8.000000000000007105, 249.8719672152120381, -95.00000000000133582 ) ) ;
#44897 = AXIS2_PLACEMENT_3D ( 'NONE', #21657, #59284, #43450 ) ;
#44898 = CARTESIAN_POINT ( 'NONE',  ( 29.31537757312406356, -16.05900791856644005, 6.893342934923157195 ) ) ;
#44899 = CARTESIAN_POINT ( 'NONE',  ( -95.21085197937823352, 30.44372064875429018, -13.11308433111474692 ) ) ;
#44900 = AXIS2_PLACEMENT_3D ( 'NONE', #30743, #29700, #19141 ) ;
#44901 = CARTESIAN_POINT ( 'NONE',  ( 36.76746179515744473, 8.081433644308901876, 71.28473465010155508 ) ) ;
#44902 = LINE ( 'NONE', #60728, #38268 ) ;
#44903 = FACE_OUTER_BOUND ( 'NONE', #54832, .T. ) ;
#44904 = ORIENTED_EDGE ( 'NONE', *, *, #30411, .F. ) ;
#44905 = CARTESIAN_POINT ( 'NONE',  ( 410.0000000000000000, 190.0000000000000000, -2.000000000000000000 ) ) ;
#44906 = DIRECTION ( 'NONE',  ( -0.000000000000000000, 1.000000000000000000, -0.000000000000000000 ) ) ;
#44907 = CARTESIAN_POINT ( 'NONE',  ( -51.84164840787130402, -39.21024726209533640, 40.00000000000003553 ) ) ;
#44908 = CARTESIAN_POINT ( 'NONE',  ( 284.7429429236411806, -21.94266591301279234, -1.615775360921237747 ) ) ;
#44909 = CARTESIAN_POINT ( 'NONE',  ( -109.7793173546317149, 36.75648380851389163, -69.07549051878955026 ) ) ;
#44910 = CARTESIAN_POINT ( 'NONE',  ( -97.89650780679127706, 30.60899921334456408, -90.10237382125301053 ) ) ;
#44911 = ORIENTED_EDGE ( 'NONE', *, *, #21405, .F. ) ;
#44912 = DIRECTION ( 'NONE',  ( 0.9108602745606093620, 0.4127148655274863742, -7.850123081445130943E-15 ) ) ;
#44913 = VECTOR ( 'NONE', #67228, 1000.000000000000000 ) ;
#44914 = FACE_OUTER_BOUND ( 'NONE', #32512, .T. ) ;
#44915 = CARTESIAN_POINT ( 'NONE',  ( -33.85171821065139852, 11.02091558840054120, -35.69924149714026385 ) ) ;
#44916 = CARTESIAN_POINT ( 'NONE',  ( 31.11269837220800127, -26.11269837220812562, 85.00100000000000477 ) ) ;
#44917 = ITEM_DEFINED_TRANSFORMATION ( 'NONE', 'NONE', #45617,  #66832 ) ;
#44918 = DIRECTION ( 'NONE',  ( -2.241020959626955766E-17, 2.489978219820156880E-16, 1.000000000000000000 ) ) ;
#44919 = ORIENTED_EDGE ( 'NONE', *, *, #30899, .F. ) ;
#44920 = CARTESIAN_POINT ( 'NONE',  ( -31.11269837220801193, 36.11269837220812207, 85.00100000000000477 ) ) ;
#44921 = DIRECTION ( 'NONE',  ( -2.509494923690479143E-16, -1.000000000000000000, -1.496132621402170665E-16 ) ) ;
#44922 = CARTESIAN_POINT ( 'NONE',  ( -142.6736406357357794, 58.59303246027003098, 94.99999999999866418 ) ) ;
#44923 = APPLICATION_CONTEXT ( 'automotive_design' ) ;
#44924 = CARTESIAN_POINT ( 'NONE',  ( -45.00000000000002132, -20.00000000000000355, 0.000000000000000000 ) ) ;
#44925 = VERTEX_POINT ( 'NONE', #48638 ) ;
#44926 = CARTESIAN_POINT ( 'NONE',  ( 158.2042568976887082, 59.50370424804803093, -89.84040114574384006 ) ) ;
#44927 = CARTESIAN_POINT ( 'NONE',  ( -12.71198166530289342, -21.52685583500284139, 0.000000000000000000 ) ) ;
#44928 = CARTESIAN_POINT ( 'NONE',  ( -95.52093927227217307, 30.58993121475388222, 41.27929887050821378 ) ) ;
#44929 = AXIS2_PLACEMENT_3D ( 'NONE', #47292, #30442, #3023 ) ;
#44930 = CARTESIAN_POINT ( 'NONE',  ( 17.48889770758268014, 6.561062909825355227, -50.32774512300183289 ) ) ;
#44932 = ORIENTED_EDGE ( 'NONE', *, *, #48319, .F. ) ;
#44931 = CARTESIAN_POINT ( 'NONE',  ( 117.4806398654733357, 33.50379325299402922, 8.232446593192225492 ) ) ;
#44933 = CARTESIAN_POINT ( 'NONE',  ( 59.29615173875419742, 11.84060224810188267, 30.79565124887290395 ) ) ;
#44934 = EDGE_CURVE ( 'NONE', #22712, #1594, #16652, .T. ) ;
#44935 = ORIENTED_EDGE ( 'NONE', *, *, #51929, .T. ) ;
#44936 = ORIENTED_EDGE ( 'NONE', *, *, #24760, .T. ) ;
#44937 = CARTESIAN_POINT ( 'NONE',  ( 181.0840389613909736, 80.03940679743415387, 44.30859410551141764 ) ) ;
#44938 = ADVANCED_FACE ( 'NONE', ( #64152 ), #58867, .F. ) ;
#44939 = DIRECTION ( 'NONE',  ( 1.000000000000000000, -0.000000000000000000, 0.000000000000000000 ) ) ;
#44941 = ORIENTED_EDGE ( 'NONE', *, *, #29392, .F. ) ;
#44940 = DIRECTION ( 'NONE',  ( 0.000000000000000000, 0.000000000000000000, 1.000000000000000000 ) ) ;
#44942 = CARTESIAN_POINT ( 'NONE',  ( 209.3223706822284100, -1.426547569622074412E-15, 31.44247402469554942 ) ) ;
#44943 = ADVANCED_FACE ( 'NONE', ( #6460 ), #47965, .F. ) ;
#44944 = CARTESIAN_POINT ( 'NONE',  ( -31.43908319763709969, 10.61114334766716105, 45.21645440618919309 ) ) ;
#44945 = VECTOR ( 'NONE', #29444, 1000.000000000000000 ) ;
#44946 = CARTESIAN_POINT ( 'NONE',  ( -71.97171223898807568, 20.94894057408426136, -39.19762039591116576 ) ) ;
#44947 = VERTEX_POINT ( 'NONE', #21581 ) ;
#44948 = CARTESIAN_POINT ( 'NONE',  ( 180.7426746203128687, 79.69150696735539441, -89.91415884680699833 ) ) ;
#44949 = CARTESIAN_POINT ( 'NONE',  ( 140.8855094313933307, 47.03549517811090652, 39.63981015661840956 ) ) ;
#44950 = CARTESIAN_POINT ( 'NONE',  ( -177.1514380519393512, 93.28180884530864603, 44.66195762070336173 ) ) ;
#44951 = CARTESIAN_POINT ( 'NONE',  ( 128.3889472838589541, 39.37765603157611594, 69.01175771905448642 ) ) ;
#44952 = CARTESIAN_POINT ( 'NONE',  ( 100.0000000000000284, 5.000000000000002665, 19.36491673103709488 ) ) ;
#44953 = ADVANCED_FACE ( 'NONE', ( #54633 ), #16994, .T. ) ;
#44954 = VERTEX_POINT ( 'NONE', #69430 ) ;
#44955 = EDGE_LOOP ( 'NONE', ( #18758, #31447, #28124, #37967 ) ) ;
#44956 = ORIENTED_EDGE ( 'NONE', *, *, #31692, .F. ) ;
#44957 = AXIS2_PLACEMENT_3D ( 'NONE', #67814, #30522, #46003 ) ;
#44958 = CARTESIAN_POINT ( 'NONE',  ( 211.7634543339367781, 116.5654349622355141, -95.00000000000133582 ) ) ;
#44959 = FILL_AREA_STYLE_COLOUR ( '', #41398 ) ;
#44960 = CARTESIAN_POINT ( 'NONE',  ( -22.15007140920429407, 31.28689709046298617, 13.32819299319723605 ) ) ;
#44961 = CARTESIAN_POINT ( 'NONE',  ( -99.97240228788317040, 31.62311673723580085, 84.54697963296760577 ) ) ;
#44962 = CARTESIAN_POINT ( 'NONE',  ( -144.3945994505580472, 59.96115386701889349, 32.72843562861698530 ) ) ;
#44963 = DIRECTION ( 'NONE',  ( -0.000000000000000000, -0.000000000000000000, -1.000000000000000000 ) ) ;
#44964 = CARTESIAN_POINT ( 'NONE',  ( -78.66644367742109978, 23.39876645725288640, -23.27090004125422595 ) ) ;
#44965 = ORIENTED_EDGE ( 'NONE', *, *, #19182, .T. ) ;
#44966 = CARTESIAN_POINT ( 'NONE',  ( 84.27368848767932263, 18.63026910897604793, 56.91985697824755874 ) ) ;
#44967 = VERTEX_POINT ( 'NONE', #10338 ) ;
#44968 = CARTESIAN_POINT ( 'NONE',  ( -95.58372570396208801, 30.61946167424475362, -92.79505394063129131 ) ) ;
#44969 = DIRECTION ( 'NONE',  ( 1.644874880248609566E-16, -1.882710788443290569E-16, 1.000000000000000000 ) ) ;
#44970 = ORIENTED_EDGE ( 'NONE', *, *, #60529, .T. ) ;
#44971 = CARTESIAN_POINT ( 'NONE',  ( 209.3223706822284100, 0.000000000000000000, 31.44247402469554942 ) ) ;
#44972 = DIRECTION ( 'NONE',  ( 0.000000000000000000, 0.000000000000000000, 1.000000000000000000 ) ) ;
#44973 = DIRECTION ( 'NONE',  ( -1.000000000000000000, 0.000000000000000000, 0.000000000000000000 ) ) ;
#44974 = CARTESIAN_POINT ( 'NONE',  ( -119.2804658695888236, 43.47213805166352785, 61.41757901617579307 ) ) ;
#44975 = CARTESIAN_POINT ( 'NONE',  ( -9.765753193741732119, 8.033970690975921869, -50.16687931305852288 ) ) ;
#44976 = VECTOR ( 'NONE', #46020, 999.9999999999998863 ) ;
#44977 = CARTESIAN_POINT ( 'NONE',  ( 440.2662102946430309, 395.0000000000043769, 106.4792280461184077 ) ) ;
#44978 = CARTESIAN_POINT ( 'NONE',  ( 442.3372781065085633, 390.0000000000001137, 108.5502958579883170 ) ) ;
#44979 = ORIENTED_EDGE ( 'NONE', *, *, #32153, .F. ) ;
#44980 = DIRECTION ( 'NONE',  ( -0.000000000000000000, 0.000000000000000000, -1.000000000000000000 ) ) ;
#44981 = CARTESIAN_POINT ( 'NONE',  ( -156.0171627975467459, 69.90368824761763733, -11.73444720282849474 ) ) ;
#44982 = ORIENTED_EDGE ( 'NONE', *, *, #61497, .F. ) ;
#44983 = DIRECTION ( 'NONE',  ( -0.000000000000000000, 1.000000000000000000, -0.000000000000000000 ) ) ;
#44984 = LINE ( 'NONE', #66465, #17158 ) ;
#44985 = LINE ( 'NONE', #24593, #7257 ) ;
#44986 = VERTEX_POINT ( 'NONE', #31803 ) ;
#44987 = CARTESIAN_POINT ( 'NONE',  ( -5.000000000000058620, -31.11269837220806878, 85.00100000000000477 ) ) ;
#44988 = CARTESIAN_POINT ( 'NONE',  ( 151.7783534118501905, 54.60545177578659093, -65.57863077677340868 ) ) ;
#44989 = CARTESIAN_POINT ( 'NONE',  ( -2.999999999999992450, 0.000000000000000000, 0.000000000000000000 ) ) ;
#44990 = CARTESIAN_POINT ( 'NONE',  ( 139.7928618793172859, 45.12615179300589574, -38.93259025567166276 ) ) ;
#44991 = ORIENTED_EDGE ( 'NONE', *, *, #18054, .T. ) ;
#44992 = CARTESIAN_POINT ( 'NONE',  ( -41.05116137042202240, 31.37049953149684356, 26.66469104408689006 ) ) ;
#44993 = VERTEX_POINT ( 'NONE', #22284 ) ;
#44994 = DIRECTION ( 'NONE',  ( -0.000000000000000000, -0.000000000000000000, 1.000000000000000000 ) ) ;
#44995 = DIRECTION ( 'NONE',  ( -3.038581678643134250E-64, 1.232595164407830672E-32, 1.000000000000000000 ) ) ;
#44996 = ADVANCED_FACE ( 'NONE', ( #482 ), #42233, .T. ) ;
#44997 = CARTESIAN_POINT ( 'NONE',  ( 141.3587662457627232, 47.34635740004710414, 90.65385063068173110 ) ) ;
#44998 = CARTESIAN_POINT ( 'NONE',  ( -31.90315521289065970, -56.64813493366050068, 41.38025477438755928 ) ) ;
#44999 = CARTESIAN_POINT ( 'NONE',  ( 46.66904755831210139, 4.999999999999909406, 2.000000000000001776 ) ) ;
#45000 = CARTESIAN_POINT ( 'NONE',  ( 0.000000000000000000, 0.000000000000000000, 10.00000000000000000 ) ) ;
#45001 = ORIENTED_EDGE ( 'NONE', *, *, #54068, .T. ) ;
#45002 = DIRECTION ( 'NONE',  ( -0.000000000000000000, 0.02271222823333339177, -0.9997420440737084801 ) ) ;
#45003 = PLANE ( 'NONE',  #55290 ) ;
#45004 = CARTESIAN_POINT ( 'NONE',  ( 48.11816970607299027, -43.69944786993949748, 170.0000000000000000 ) ) ;
#45005 = CARTESIAN_POINT ( 'NONE',  ( 141.3445468829085314, 46.13338528906589886, -69.86407327641063603 ) ) ;
#45006 = DIRECTION ( 'NONE',  ( 0.1785568947986370392, -0.9839295885986295565, 0.000000000000000000 ) ) ;
#45007 = AXIS2_PLACEMENT_3D ( 'NONE', #48485, #59063, #16506 ) ;
#45008 = VECTOR ( 'NONE', #31676, 1000.000000000000000 ) ;
#45009 = ORIENTED_EDGE ( 'NONE', *, *, #56695, .F. ) ;
#45010 = ADVANCED_FACE ( 'NONE', ( #37766 ), #27909, .T. ) ;
#45011 = CARTESIAN_POINT ( 'NONE',  ( 160.2883311361769927, 61.16711613734478448, -9.825516263918585125 ) ) ;
#45012 = EDGE_CURVE ( 'NONE', #16895, #2912, #26870, .T. ) ;
#45013 = VECTOR ( 'NONE', #45726, 1000.000000000000000 ) ;
#45014 = CARTESIAN_POINT ( 'NONE',  ( 14.80582440982707837, 6.470883766728821485, 44.96611724300024804 ) ) ;
#45015 = VERTEX_POINT ( 'NONE', #38109 ) ;
#45016 = CARTESIAN_POINT ( 'NONE',  ( -57.65733424639443427, 15.39521790791523159, -62.52345615960770431 ) ) ;
#45017 = CARTESIAN_POINT ( 'NONE',  ( 128.3516609434389011, 38.19824209820340144, -92.10286917565350961 ) ) ;
#45018 = ORIENTED_EDGE ( 'NONE', *, *, #13355, .T. ) ;
#45019 = CARTESIAN_POINT ( 'NONE',  ( -142.0081215801269536, 58.07066293384865219, -69.45719805043682982 ) ) ;
#45020 = EDGE_CURVE ( 'NONE', #62331, #32020, #11891, .T. ) ;
#45021 = VECTOR ( 'NONE', #14617, 1000.000000000000000 ) ;
#45022 = DIRECTION ( 'NONE',  ( -1.000000000000000000, 0.000000000000000000, 0.000000000000000000 ) ) ;
#45023 = CARTESIAN_POINT ( 'NONE',  ( 157.9160637431159557, 57.99786926216935257, -36.12418429913763873 ) ) ;
#45024 = ORIENTED_EDGE ( 'NONE', *, *, #4914, .F. ) ;
#45025 = CARTESIAN_POINT ( 'NONE',  ( -95.86163447241557378, 30.75089131639700213, 7.262573566396630653 ) ) ;
#45026 = CARTESIAN_POINT ( 'NONE',  ( 70.37411710121934050, 15.54173091717098210, 89.51384947277743720 ) ) ;
#45027 = CARTESIAN_POINT ( 'NONE',  ( -31.11269837220809364, -15.55634918610397754, 0.000000000000000000 ) ) ;
#45028 = CARTESIAN_POINT ( 'NONE',  ( 66.07923263163412742, 14.44036440558002177, 30.46288473904308702 ) ) ;
#45029 = CARTESIAN_POINT ( 'NONE',  ( -132.4951995226844872, 50.99687809989499243, -19.13814356169182318 ) ) ;
#45030 = CARTESIAN_POINT ( 'NONE',  ( -147.5180482799911488, 62.50984070207314858, -88.75905994936287868 ) ) ;
#45031 = CARTESIAN_POINT ( 'NONE',  ( 128.9253503890652723, 38.52561778336672660, -76.02404744399288461 ) ) ;
#45032 = EDGE_CURVE ( 'NONE', #23803, #56265, #59553, .T. ) ;
#45033 = ORIENTED_EDGE ( 'NONE', *, *, #704, .T. ) ;
#45034 = CARTESIAN_POINT ( 'NONE',  ( 139.1306635769909974, 45.89653412152171086, -75.70587900743647936 ) ) ;
#45035 = DIRECTION ( 'NONE',  ( 1.000000000000000000, -0.000000000000000000, 2.168404344971009608E-16 ) ) ;
#45036 = ORIENTED_EDGE ( 'NONE', *, *, #63990, .T. ) ;
#45037 = EDGE_CURVE ( 'NONE', #7248, #59256, #14172, .T. ) ;
#45038 = EDGE_CURVE ( 'NONE', #51213, #8603, #33254, .T. ) ;
#45039 = CARTESIAN_POINT ( 'NONE',  ( -156.8773151811562911, 72.06122063279302381, -40.89328888528041972 ) ) ;
#45040 = CARTESIAN_POINT ( 'NONE',  ( 206.3053863259449656, 110.3084416756849180, -9.610806492142495827 ) ) ;
#45041 = CARTESIAN_POINT ( 'NONE',  ( -38.88884187334145537, 11.95889603743730234, 36.71961320002495199 ) ) ;
#45042 = FACE_OUTER_BOUND ( 'NONE', #23496, .T. ) ;
#45043 = CARTESIAN_POINT ( 'NONE',  ( -1.327237339234996982, 7.561837009978233048, 41.36847194710579600 ) ) ;
#45044 = DIRECTION ( 'NONE',  ( 0.000000000000000000, -1.000000000000000000, 0.000000000000000000 ) ) ;
#45045 = CARTESIAN_POINT ( 'NONE',  ( -47.95468448182521115, 12.89252559348045857, -67.12589513619153081 ) ) ;
#45046 = LINE ( 'NONE', #1809, #46267 ) ;
#45047 = LINE ( 'NONE', #55251, #46724 ) ;
#45048 = CARTESIAN_POINT ( 'NONE',  ( 0.000000000000000000, 35.00000000000000000, 0.000000000000000000 ) ) ;
#45049 = ORIENTED_EDGE ( 'NONE', *, *, #31596, .T. ) ;
#45050 = CARTESIAN_POINT ( 'NONE',  ( -95.52093927227218728, 30.58993121475389287, -39.25435290088285001 ) ) ;
#45051 = ORIENTED_EDGE ( 'NONE', *, *, #64616, .F. ) ;
#45052 = CARTESIAN_POINT ( 'NONE',  ( 103.8317086684999850, 26.02720265156213486, -66.36710428647430149 ) ) ;
#45053 = CARTESIAN_POINT ( 'NONE',  ( 209.9518228411288874, 18.00000000000002842, 31.43423095485942298 ) ) ;
#45054 = CARTESIAN_POINT ( 'NONE',  ( 46.90222083990963853, 9.503928413859233260, 64.49857371303593823 ) ) ;
#45055 = CYLINDRICAL_SURFACE ( 'NONE', #2044, 7.500000000000013323 ) ;
#45056 = CARTESIAN_POINT ( 'NONE',  ( 0.000000000000000000, 0.000000000000000000, 0.000000000000000000 ) ) ;
#45057 = AXIS2_PLACEMENT_3D ( 'NONE', #22501, #66138, #60826 ) ;
#45058 = CARTESIAN_POINT ( 'NONE',  ( 110.2429982417149432, 28.88204397445228722, 44.61121420573733332 ) ) ;
#45059 = VECTOR ( 'NONE', #23314, 1000.000000000000000 ) ;
#45060 = CARTESIAN_POINT ( 'NONE',  ( -77.72491324796695267, 21.96482567905605521, 57.30687935295142665 ) ) ;
#45061 = CARTESIAN_POINT ( 'NONE',  ( -167.9889421625798889, 81.59140042431232587, 59.67682617645385790 ) ) ;
#45062 = ORIENTED_EDGE ( 'NONE', *, *, #67449, .F. ) ;
#45063 = VERTEX_POINT ( 'NONE', #32151 ) ;
#45064 = DIRECTION ( 'NONE',  ( 0.000000000000000000, 0.000000000000000000, -1.000000000000000000 ) ) ;
#45065 = CARTESIAN_POINT ( 'NONE',  ( 173.9413349464226997, 71.67637800842359752, 61.34821181573801141 ) ) ;
#45067 = LINE ( 'NONE', #13417, #52523 ) ;
#45066 = CIRCLE ( 'NONE', #25947, 242.4895526022646379 ) ;
#45068 = VECTOR ( 'NONE', #35468, 1000.000000000000000 ) ;
#45069 = CARTESIAN_POINT ( 'NONE',  ( 103.1534365798308528, 26.83148826706847956, 66.45580475007047028 ) ) ;
#45070 = CARTESIAN_POINT ( 'NONE',  ( -166.0012244511291613, 80.97916541034756222, -17.74230296181466926 ) ) ;
#45071 = VECTOR ( 'NONE', #13910, 1000.000000000000000 ) ;
#45072 = LINE ( 'NONE', #33837, #53232 ) ;
#45073 = ORIENTED_EDGE ( 'NONE', *, *, #59385, .F. ) ;
#45074 = CARTESIAN_POINT ( 'NONE',  ( 103.8055367708241477, 27.11070767929350822, -39.54200133079056911 ) ) ;
#45075 = CARTESIAN_POINT ( 'NONE',  ( 19.11382977197791533, 7.636807742668411336, -36.27859613552720930 ) ) ;
#45076 = DIRECTION ( 'NONE',  ( 1.000000000000000000, 0.000000000000000000, 0.000000000000000000 ) ) ;
#45077 = CARTESIAN_POINT ( 'NONE',  ( 0.000000000000000000, 70.00000000000000000, 0.000000000000000000 ) ) ;
#45078 = CARTESIAN_POINT ( 'NONE',  ( 313.9975424824652350, 295.6904194069557548, 539.5330678552892323 ) ) ;
#45079 = EDGE_CURVE ( 'NONE', #56426, #1003, #67012, .T. ) ;
#45080 = FACE_BOUND ( 'NONE', #54381, .T. ) ;
#45081 = EDGE_CURVE ( 'NONE', #27081, #39681, #1178, .T. ) ;
#45082 = VERTEX_POINT ( 'NONE', #44072 ) ;
#45083 = DIRECTION ( 'NONE',  ( -0.04486483035051862939, 0.9989930665413143673, 0.000000000000000000 ) ) ;
#45084 = CARTESIAN_POINT ( 'NONE',  ( 69.68177367721139603, 20.52767805628179332, 41.38025477438755928 ) ) ;
#45085 = DIRECTION ( 'NONE',  ( 0.6246950475544236214, 0.000000000000000000, 0.7808688094430308313 ) ) ;
#45086 = CARTESIAN_POINT ( 'NONE',  ( -180.3114074031036296, 97.09758726817787533, 9.322656802965427758 ) ) ;
#45087 = CARTESIAN_POINT ( 'NONE',  ( 211.4997502125519304, 118.0043045815490359, 60.37852553085293295 ) ) ;
#45088 = CARTESIAN_POINT ( 'NONE',  ( 86.14852828165525978, 19.25704475759650691, -62.66611478937537782 ) ) ;
#45089 = EDGE_LOOP ( 'NONE', ( #61750, #63480, #36443, #54217 ) ) ;
#45091 = ADVANCED_FACE ( 'NONE', ( #53585 ), #37078, .T. ) ;
#45090 = FACE_OUTER_BOUND ( 'NONE', #63675, .T. ) ;
#45092 = CARTESIAN_POINT ( 'NONE',  ( -4.339467034331206285, -6.732211846623409102, -9.499999999999992895 ) ) ;
#45093 = EDGE_LOOP ( 'NONE', ( #63494, #46933, #32678, #45492, #58218, #40201, #55508, #56526, #32545, #16483, #2818, #28681, #61178, #16009, #50400, #56626, #31390, #1210, #40803, #32029, #7210, #191, #24779, #50763, #58608, #47470, #50239, #21439, #12236, #66635, #44545, #15621, #18510, #49211, #8607, #14658, #18237, #60244, #40492, #12806, #62912, #45786, #49716, #56602, #24780, #48660, #66180, #43089, #27214, #46684, #56921, #15352, #69228, #64823, #51930, #33406, #4585, #66762, #24492, #42263, #44066, #65061, #52769, #37777, #54710, #8442, #39386, #61206, #62655, #43507, #48222, #32732, #49046, #10323, #68634, #41900, #43962, #50847, #25207, #30829, #23486, #57052, #45062, #25565, #68931, #54639, #29815, #10764, #68517 ) ) ;
#45094 = EDGE_CURVE ( 'NONE', #37531, #18323, #43774, .T. ) ;
#45095 = FACE_OUTER_BOUND ( 'NONE', #49006, .T. ) ;
#45096 = ORIENTED_EDGE ( 'NONE', *, *, #41921, .T. ) ;
#45097 = CARTESIAN_POINT ( 'NONE',  ( -84.97622048504841530, 24.82614411847756841, -73.52177815261417493 ) ) ;
#45098 = CARTESIAN_POINT ( 'NONE',  ( -60.47589866267035319, 17.25153113855766662, -21.05818846266538458 ) ) ;
#45099 = CARTESIAN_POINT ( 'NONE',  ( 91.50468583833759340, 22.21368636549397380, -75.88665251703855574 ) ) ;
#45100 = ORIENTED_EDGE ( 'NONE', *, *, #7799, .T. ) ;
#45101 = EDGE_CURVE ( 'NONE', #34747, #54206, #64724, .T. ) ;
#45102 = VECTOR ( 'NONE', #15845, 1000.000000000000000 ) ;
#45103 = ORIENTED_EDGE ( 'NONE', *, *, #43225, .T. ) ;
#45104 = DIRECTION ( 'NONE',  ( 0.000000000000000000, 0.000000000000000000, -1.000000000000000000 ) ) ;
#45105 = CARTESIAN_POINT ( 'NONE',  ( 410.0000000000000000, 190.0000000000000000, 2.000000000000000000 ) ) ;
#45106 = CARTESIAN_POINT ( 'NONE',  ( 102.7414208686707724, 26.65627265923297173, 10.75606379640384525 ) ) ;
#45107 = CONICAL_SURFACE ( 'NONE', #36130, 74.95140232871122521, 0.8777644062502172329 ) ;
#45108 = ORIENTED_EDGE ( 'NONE', *, *, #68677, .T. ) ;
#45109 = PRODUCT ( 'cover', 'cover', '', ( #59258 ) ) ;
#45110 = AXIS2_PLACEMENT_3D ( 'NONE', #62615, #57681, #8806 ) ;
#45111 = CONICAL_SURFACE ( 'NONE', #20411, 74.95140232871122521, 0.8777644062502172329 ) ;
#45112 = CARTESIAN_POINT ( 'NONE',  ( -47.55256438668344288, 13.83151366677316219, 10.73057395638927325 ) ) ;
#45113 = CARTESIAN_POINT ( 'NONE',  ( -129.6079169496901216, 50.20899308323959787, -9.049169391184644695 ) ) ;
#45114 = CARTESIAN_POINT ( 'NONE',  ( -152.6692566860463955, 68.24922339534836624, -89.18787451257621512 ) ) ;
#45115 = CARTESIAN_POINT ( 'NONE',  ( 112.5554747942046134, 29.96654954475020105, -23.71639831171845003 ) ) ;
#45116 = CARTESIAN_POINT ( 'NONE',  ( 93.47084677873587566, 21.86992891175610865, 87.80919612172070288 ) ) ;
#45118 = ORIENTED_EDGE ( 'NONE', *, *, #56861, .T. ) ;
#45117 = CARTESIAN_POINT ( 'NONE',  ( -149.5074843970971301, -170.0000000000000000, -7.968279941028271196 ) ) ;
#45119 = ORIENTED_EDGE ( 'NONE', *, *, #64817, .T. ) ;
#45120 = EDGE_CURVE ( 'NONE', #58381, #1859, #18749, .T. ) ;
#45121 = ADVANCED_FACE ( 'NONE', ( #34932 ), #17715, .F. ) ;
#45122 = ORIENTED_EDGE ( 'NONE', *, *, #66157, .F. ) ;
#45123 = CARTESIAN_POINT ( 'NONE',  ( -8.651394039243120559, 32.28678488987412010, 6.893342931991233158 ) ) ;
#45124 = CARTESIAN_POINT ( 'NONE',  ( 174.9161599490640526, 73.97365196673301568, 5.688883349119021382 ) ) ;
#45125 = CARTESIAN_POINT ( 'NONE',  ( 0.06809871960542919489, -6.146186931204441706, -5.354491962338086886 ) ) ;
#45126 = CARTESIAN_POINT ( 'NONE',  ( 105.4193882736795871, 26.71329717705293660, -22.34225740095065404 ) ) ;
#45127 = EDGE_CURVE ( 'NONE', #67017, #42777, #28249, .T. ) ;
#45128 = CARTESIAN_POINT ( 'NONE',  ( -55.05276343752910151, 14.68156374112636797, 72.16187836339486239 ) ) ;
#45129 = CARTESIAN_POINT ( 'NONE',  ( 210.6189312023034574, 116.6550319566545539, 94.99999999999866418 ) ) ;
#45130 = FACE_OUTER_BOUND ( 'NONE', #15830, .T. ) ;
#45131 = DIRECTION ( 'NONE',  ( 1.000000000000000000, 0.000000000000000000, 0.000000000000000000 ) ) ;
#45132 = DIRECTION ( 'NONE',  ( -1.000000000000000000, 0.000000000000000000, -0.000000000000000000 ) ) ;
#45133 = ORIENTED_EDGE ( 'NONE', *, *, #58910, .T. ) ;
#45134 = CARTESIAN_POINT ( 'NONE',  ( 8.287863202055540057, 7.382585476140731906, -15.68614915429326473 ) ) ;
#45135 = VERTEX_POINT ( 'NONE', #39175 ) ;
#45136 = ORIENTED_EDGE ( 'NONE', *, *, #59414, .F. ) ;
#45137 = CARTESIAN_POINT ( 'NONE',  ( 0.000000000000000000, 0.000000000000000000, 170.0000000000000000 ) ) ;
#45138 = CARTESIAN_POINT ( 'NONE',  ( 6.400000000000000355, -9.237604307034033013, -1.753283555911559014E-16 ) ) ;
#45139 = CARTESIAN_POINT ( 'NONE',  ( -170.2951623264597174, 85.51757001115473145, 45.28173547561066670 ) ) ;
#45140 = CARTESIAN_POINT ( 'NONE',  ( -100.4466073551323007, 31.85873123265079698, -49.80183754970560273 ) ) ;
#45141 = B_SPLINE_CURVE_WITH_KNOTS ( 'NONE', 3,
 ( #9263, #8926, #51496, #52514, #20162, #30374 ),
 .UNSPECIFIED., .F., .F.,
 ( 4, 2, 4 ),
 ( 1.095770181088879689E-06, 0.03239442681617710207, 0.06478775786217311206 ),
 .UNSPECIFIED. ) ;
#45142 = CARTESIAN_POINT ( 'NONE',  ( -109.5142642360664240, 36.61018064014775319, 9.126798092972807197 ) ) ;
#45143 = DIRECTION ( 'NONE',  ( -0.000000000000000000, 1.000000000000000000, -0.000000000000000000 ) ) ;
#45144 = CARTESIAN_POINT ( 'NONE',  ( 135.6647932137618113, 43.70902528961477174, -9.385834288385190405 ) ) ;
#45145 = ORIENTED_EDGE ( 'NONE', *, *, #56996, .F. ) ;
#45146 = VERTEX_POINT ( 'NONE', #60617 ) ;
#45147 = CYLINDRICAL_SURFACE ( 'NONE', #39499, 7.500000000000020428 ) ;
#45148 = CARTESIAN_POINT ( 'NONE',  ( 0.000000000000000000, 6.928203230275506108, 4.000000000000006217 ) ) ;
#45149 = CARTESIAN_POINT ( 'NONE',  ( -30.60309003827974550, 68.41902945196812880, 41.38025477438755928 ) ) ;
#45150 = CARTESIAN_POINT ( 'NONE',  ( 56.30171512200998052, 11.21502580416398587, -13.02431553323698132 ) ) ;
#45151 = UNCERTAINTY_MEASURE_WITH_UNIT (LENGTH_MEASURE( 1.000000000000000082E-05 ), #57453, 'distance_accuracy_value', 'NONE');
#45152 = VECTOR ( 'NONE', #61542, 1000.000000000000000 ) ;
#45153 = CYLINDRICAL_SURFACE ( 'NONE', #10218, 5.000000000000004441 ) ;
#45154 = DIRECTION ( 'NONE',  ( -1.000000000000000000, 0.000000000000000000, 0.000000000000000000 ) ) ;
#45155 = VERTEX_POINT ( 'NONE', #12434 ) ;
#45156 = CARTESIAN_POINT ( 'NONE',  ( 157.4703587214989398, -170.0000000000000000, -24.27963370867398396 ) ) ;
#45157 = CARTESIAN_POINT ( 'NONE',  ( -56.96436614829622158, 16.24647150911285109, -76.81720701772762538 ) ) ;
#45158 = CARTESIAN_POINT ( 'NONE',  ( 199.7286177451875062, 101.4075663537891643, -76.30715059617197937 ) ) ;
#45159 = AXIS2_PLACEMENT_3D ( 'NONE', #51442, #30672, #40191 ) ;
#45160 = DIRECTION ( 'NONE',  ( 0.9808306643139259595, 0.1948620228302647139, -4.930380657631323784E-31 ) ) ;
#45161 = DIRECTION ( 'NONE',  ( 0.000000000000000000, 1.000000000000000000, 0.000000000000000000 ) ) ;
#45162 = SURFACE_STYLE_FILL_AREA ( #23719 ) ;
#45163 = CARTESIAN_POINT ( 'NONE',  ( -167.6413528428655582, 81.22881971256911982, 6.330796842060393281 ) ) ;
#45164 = DIRECTION ( 'NONE',  ( 0.000000000000000000, -1.000000000000000000, 0.000000000000000000 ) ) ;
#45165 = FACE_BOUND ( 'NONE', #49543, .T. ) ;
#45166 = FACE_OUTER_BOUND ( 'NONE', #62501, .T. ) ;
#45167 = VECTOR ( 'NONE', #50496, 1000.000000000000000 ) ;
#45168 = COLOUR_RGB ( '',0.7921568627450980005, 0.8196078431372548767, 0.9333333333333333481 ) ;
#45169 = EDGE_CURVE ( 'NONE', #54143, #34238, #33893, .T. ) ;
#45170 = AXIS2_PLACEMENT_3D ( 'NONE', #54434, #32998, #55139 ) ;
#45171 = CARTESIAN_POINT ( 'NONE',  ( 0.000000000000000000, 0.000000000000000000, 41.38025477438755928 ) ) ;
#45172 = EDGE_LOOP ( 'NONE', ( #56479, #38756, #49867, #34213 ) ) ;
#45173 = CARTESIAN_POINT ( 'NONE',  ( 275.6617573822855434, 21.85836566642199230, 2.507523880400401417 ) ) ;
#45174 = CLOSED_SHELL ( 'NONE', ( #39577, #60253, #60803, #52335, #12584, #43976, #35667, #24699, #14385 ) ) ;
#45175 = CARTESIAN_POINT ( 'NONE',  ( 150.2805372522807374, 53.51147386362154634, 65.90567756530964516 ) ) ;
#45176 = DIRECTION ( 'NONE',  ( -0.000000000000000000, -0.000000000000000000, 1.000000000000000000 ) ) ;
#45177 = LINE ( 'NONE', #1942, #69392 ) ;
#45178 = CYLINDRICAL_SURFACE ( 'NONE', #36728, 99.99999999999994316 ) ;
#45179 = EDGE_LOOP ( 'NONE', ( #19109, #3659 ) ) ;
#45181 = ADVANCED_FACE ( 'NONE', ( #19088 ), #63036, .T. ) ;
#45180 = DIRECTION ( 'NONE',  ( 1.387778780781445922E-16, -1.000000000000000000, -1.232595164407830946E-32 ) ) ;
#45182 = LINE ( 'NONE', #19485, #14733 ) ;
#45183 = ORIENTED_EDGE ( 'NONE', *, *, #66153, .F. ) ;
#45184 = EDGE_LOOP ( 'NONE', ( #38352, #31228, #68303, #12792 ) ) ;
#45185 = EDGE_CURVE ( 'NONE', #37226, #11952, #20463, .T. ) ;
#45186 = DIRECTION ( 'NONE',  ( 0.000000000000000000, 0.000000000000000000, 1.000000000000000000 ) ) ;
#45187 = CARTESIAN_POINT ( 'NONE',  ( 150.9128604434957879, 53.97103482421773890, 33.23130411755268909 ) ) ;
#45188 = EDGE_CURVE ( 'NONE', #26154, #14102, #19785, .T. ) ;
#45189 = LINE ( 'NONE', #66666, #35820 ) ;
#45190 = VERTEX_POINT ( 'NONE', #45826 ) ;
#45191 = LINE ( 'NONE', #8612, #31242 ) ;
#45192 = ADVANCED_FACE ( 'NONE', ( #9579 ), #19430, .F. ) ;
#45193 = CARTESIAN_POINT ( 'NONE',  ( -178.0633751203918678, 92.80295726428050784, 17.12321454651181796 ) ) ;
#45194 = CARTESIAN_POINT ( 'NONE',  ( -0.5183605925912000423, 6.525266619725953454, 9.063124254828315074 ) ) ;
#45195 = DIRECTION ( 'NONE',  ( -4.270088556250601699E-16, -0.000000000000000000, -1.000000000000000000 ) ) ;
#45196 = CARTESIAN_POINT ( 'NONE',  ( -25.49247221749737946, 9.706368398275717624, -11.37573925065449743 ) ) ;
#45197 = LINE ( 'NONE', #13878, #6182 ) ;
#45198 = VERTEX_POINT ( 'NONE', #40541 ) ;
#45199 = SHAPE_REPRESENTATION ( 'SIEVE', ( #66832 ), #5131 ) ;
#45200 = CARTESIAN_POINT ( 'NONE',  ( 113.4493678088378203, 30.39339414805072792, -36.62597440105078306 ) ) ;
#45201 = CARTESIAN_POINT ( 'NONE',  ( -76.33235143960695268, 22.51916353135075255, 18.20519721888241449 ) ) ;
#45202 = CARTESIAN_POINT ( 'NONE',  ( 44.35071890818840501, 9.104600422692270101, -37.46304456836167418 ) ) ;
#45203 = CARTESIAN_POINT ( 'NONE',  ( -172.7173255566597732, 88.18461381371098184, -76.55650775521371543 ) ) ;
#45205 = EDGE_LOOP ( 'NONE', ( #69426, #23870, #52984, #29245, #59169 ) ) ;
#45204 = CARTESIAN_POINT ( 'NONE',  ( -131.5964873355040368, 50.36491837697927565, 86.92810408690877466 ) ) ;
#45206 = CARTESIAN_POINT ( 'NONE',  ( 84.74140601443113496, 18.78541996275573212, -36.05909698884106263 ) ) ;
#45207 = AXIS2_PLACEMENT_3D ( 'NONE', #50987, #39052, #34122 ) ;
#45208 = EDGE_LOOP ( 'NONE', ( #69524, #36600 ) ) ;
#45209 = CIRCLE ( 'NONE', #40741, 242.4895526022646379 ) ;
#45210 = CARTESIAN_POINT ( 'NONE',  ( 45.78444578631987127, 59.41672343742573759, 170.0000000000000000 ) ) ;
#45211 = DIRECTION ( 'NONE',  ( -0.000000000000000000, 1.000000000000000000, 0.000000000000000000 ) ) ;
#45212 = DIRECTION ( 'NONE',  ( 1.000000000000000000, 0.000000000000000000, 0.000000000000000000 ) ) ;
#45213 = EDGE_CURVE ( 'NONE', #24336, #63892, #35625, .T. ) ;
#45214 = CARTESIAN_POINT ( 'NONE',  ( 181.5127080940606277, 79.03904173130082711, -9.380507075415927432 ) ) ;
#45215 = AXIS2_PLACEMENT_3D ( 'NONE', #28181, #11652, #10965 ) ;
#45216 = CARTESIAN_POINT ( 'NONE',  ( -123.6699087229882110, 45.04696784753416239, 57.79816663664966825 ) ) ;
#45217 = CARTESIAN_POINT ( 'NONE',  ( 44.34362023773822870, 10.12115849931653422, 4.905806151721804120 ) ) ;
#45218 = CARTESIAN_POINT ( 'NONE',  ( -178.2328124332057087, 94.56955476227571467, -20.87550340617716671 ) ) ;
#45219 = PLANE ( 'NONE',  #55359 ) ;
#45220 = ORIENTED_EDGE ( 'NONE', *, *, #44553, .T. ) ;
#45221 = ORIENTED_EDGE ( 'NONE', *, *, #7432, .F. ) ;
#45222 = CARTESIAN_POINT ( 'NONE',  ( 103.8093541423579325, 26.01745837747062851, 60.06901032783780892 ) ) ;
#45223 = CIRCLE ( 'NONE', #54179, 23.97499999999999787 ) ;
#45224 = CARTESIAN_POINT ( 'NONE',  ( 164.9534461562627712, 63.71129898458566032, 63.17659111825835083 ) ) ;
#45225 = DIRECTION ( 'NONE',  ( -0.000000000000000000, 1.000000000000000000, -0.000000000000000000 ) ) ;
#45226 = CARTESIAN_POINT ( 'NONE',  ( 66.29961816943398389, 13.45804302849873579, -23.13624938398751141 ) ) ;
#45227 = CARTESIAN_POINT ( 'NONE',  ( 183.9986899696431522, 81.60141257362813860, -50.64888762674885925 ) ) ;
#45228 = CARTESIAN_POINT ( 'NONE',  ( -105.8768181937898589, 34.64545164169047808, 71.46195835557104203 ) ) ;
#45229 = CARTESIAN_POINT ( 'NONE',  ( 24.91130694661015710, -3.250319586706349018, 3.061616997868437868E-16 ) ) ;
#45230 = DIRECTION ( 'NONE',  ( 0.000000000000000000, 0.000000000000000000, 1.000000000000000000 ) ) ;
#45231 = VERTEX_POINT ( 'NONE', #35963 ) ;
#45232 = EDGE_LOOP ( 'NONE', ( #58020, #34944 ) ) ;
#45233 = ORIENTED_EDGE ( 'NONE', *, *, #22710, .T. ) ;
#45234 = FACE_OUTER_BOUND ( 'NONE', #52768, .T. ) ;
#45235 = CARTESIAN_POINT ( 'NONE',  ( -78.08539259565777968, 22.10035297730220805, 84.10499846222364795 ) ) ;
#45236 = DIRECTION ( 'NONE',  ( -0.000000000000000000, -0.000000000000000000, -1.000000000000000000 ) ) ;
#45237 = CARTESIAN_POINT ( 'NONE',  ( 47.74291447196797833, 188.0000000000000000, -75.60236247897087480 ) ) ;
#45238 = CARTESIAN_POINT ( 'NONE',  ( 110.0000000000000284, -21.42428528562853174, -5.000000000000004441 ) ) ;
#45239 = DIRECTION ( 'NONE',  ( -0.000000000000000000, -0.000000000000000000, 1.000000000000000000 ) ) ;
#45240 = LINE ( 'NONE', #66034, #23648 ) ;
#45241 = PRODUCT_DEFINITION ( 'UNKNOWN', '', #55760, #21873 ) ;
#45242 = CARTESIAN_POINT ( 'NONE',  ( 56.94505604581134151, 12.37336791557969917, 32.90170006804437008 ) ) ;
#45243 = LINE ( 'NONE', #7631, #50634 ) ;
#45244 = ORIENTED_EDGE ( 'NONE', *, *, #21045, .T. ) ;
#45245 = CARTESIAN_POINT ( 'NONE',  ( -0.3734056954813056994, 6.520221844775928588, -41.93998480159426379 ) ) ;
#45246 = DIRECTION ( 'NONE',  ( 1.001915251000354105E-14, -1.000000000000000000, -5.551115123135531297E-17 ) ) ;
#45247 = CARTESIAN_POINT ( 'NONE',  ( -189.4223925288096382, 107.3427006758676328, -40.39023558151960458 ) ) ;
#45248 = DIRECTION ( 'NONE',  ( -0.000000000000000000, 0.000000000000000000, -1.000000000000000000 ) ) ;
#45250 = EDGE_CURVE ( 'NONE', #59881, #56091, #30343, .T. ) ;
#45249 = DIRECTION ( 'NONE',  ( -0.000000000000000000, 1.000000000000000000, -0.000000000000000000 ) ) ;
#45251 = CARTESIAN_POINT ( 'NONE',  ( 197.2197025888162045, 96.62026035493818199, 62.89200297478758728 ) ) ;
#45252 = CARTESIAN_POINT ( 'NONE',  ( 128.3889472838589256, 39.37765603157609462, -11.52189405233656139 ) ) ;
#45253 = EDGE_CURVE ( 'NONE', #536, #27491, #18696, .T. ) ;
#45254 = VERTEX_POINT ( 'NONE', #62704 ) ;
#45255 = CONICAL_SURFACE ( 'NONE', #67717, 65.00000000000000000, 0.7853981633974497223 ) ;
#45256 = CARTESIAN_POINT ( 'NONE',  ( -37.98601804829808515, 14.28438006995824772, -11.98601804829809581 ) ) ;
#45257 = CARTESIAN_POINT ( 'NONE',  ( -37.52119286077851967, 11.69341290629620467, -47.21248048768034522 ) ) ;
#45258 = DIRECTION ( 'NONE',  ( 0.000000000000000000, 0.000000000000000000, 1.000000000000000000 ) ) ;
#45259 = ITEM_DEFINED_TRANSFORMATION ( 'NONE', 'NONE', #7469,  #66832 ) ;
#45260 = DIRECTION ( 'NONE',  ( -2.298858655265465393E-16, 9.825793442285913883E-17, 1.000000000000000000 ) ) ;
#45261 = ORIENTED_EDGE ( 'NONE', *, *, #41327, .F. ) ;
#45262 = CARTESIAN_POINT ( 'NONE',  ( -125.4481990864045287, 46.20056605584954923, -49.91370389823396891 ) ) ;
#45263 = AXIS2_PLACEMENT_3D ( 'NONE', #20643, #53683, #36836 ) ;
#45264 = LINE ( 'NONE', #60750, #30245 ) ;
#45265 = AXIS2_PLACEMENT_3D ( 'NONE', #14879, #68021, #46899 ) ;
#45266 = DIRECTION ( 'NONE',  ( -0.000000000000000000, -0.000000000000000000, 1.000000000000000000 ) ) ;
#45267 = VECTOR ( 'NONE', #12827, 1000.000000000000000 ) ;
#45268 = EDGE_CURVE ( 'NONE', #22952, #37048, #45650, .T. ) ;
#45269 = DIRECTION ( 'NONE',  ( 1.850169831522831466E-16, -1.000000000000000000, 5.551115123125781470E-17 ) ) ;
#45270 = EDGE_LOOP ( 'NONE', ( #14854, #27529, #29511, #30391 ) ) ;
#45271 = CARTESIAN_POINT ( 'NONE',  ( -57.42826130032241849, 16.37596353166460617, 3.854800282744499818 ) ) ;
#45272 = CARTESIAN_POINT ( 'NONE',  ( 450.2085304802404835, 190.0000000000000000, -219.9999999999999147 ) ) ;
#45273 = ADVANCED_FACE ( 'NONE', ( #30687 ), #31038, .F. ) ;
#45274 = CARTESIAN_POINT ( 'NONE',  ( -155.5977325361978387, 70.88311713755702215, 42.60514736212469700 ) ) ;
#45275 = VECTOR ( 'NONE', #27644, 1000.000000000000000 ) ;
#45276 = EDGE_CURVE ( 'NONE', #5944, #43052, #8547, .T. ) ;
#45277 = CARTESIAN_POINT ( 'NONE',  ( 22.89234820949994642, 6.832052815347871011, -45.43617115817555430 ) ) ;
#45279 = ORIENTED_EDGE ( 'NONE', *, *, #16382, .F. ) ;
#45278 = CARTESIAN_POINT ( 'NONE',  ( 115.7731501832036685, 32.64791439093737324, 5.176517809787929636 ) ) ;
#45280 = CARTESIAN_POINT ( 'NONE',  ( 58.47673920847984874, 11.66523265296355305, 31.32250200715353827 ) ) ;
#45281 = ORIENTED_EDGE ( 'NONE', *, *, #12373, .T. ) ;
#45282 = VERTEX_POINT ( 'NONE', #56730 ) ;
#45283 = CARTESIAN_POINT ( 'NONE',  ( 174.9161599490640526, 73.97365196673298726, 32.53343393958267882 ) ) ;
#45284 = B_SPLINE_CURVE_WITH_KNOTS ( 'NONE', 3,
 ( #24871, #46308, #19582, #9730, #67786, #52621, #41041, #41733, #14316, #35775, #57226, #9040, #63192, #47336, #14652, #30486, #36114, #57570, #9381, #30841, #52284, #25569, #47008, #20274, #36456, #49062, #63533, #58581, #31869, #5475, #22000, #546, #42419, #48026, #59275, #188, #36805, #4781, #26250, #63878, #6156, #53986, #27618, #26930 ),
 .UNSPECIFIED., .F., .F.,
 ( 4, 2, 2, 2, 2, 2, 2, 2, 2, 2, 2, 2, 2, 2, 2, 2, 2, 2, 2, 2, 2, 4 ),
 ( 0.02495775893651561508, 0.02650251144344300744, 0.02804726395037039979, 0.02959201645729779215, 0.03113676896422518450, 0.03268152147115257339, 0.03345389772461627304, 0.03422627397807997268, 0.03577102648500738585, 0.03654340273847110632, 0.03731577899193481984, 0.03808815524539853337, 0.03886053149886224689, 0.04040528400578969476, 0.04117766025925341522, 0.04195003651271712874, 0.04349478901964452804, 0.04503954152657194121, 0.04581191778003564780, 0.04658429403349935438, 0.04812904654042681613, 0.04967379904735427787 ),
 .UNSPECIFIED. ) ;
#45285 = CARTESIAN_POINT ( 'NONE',  ( 22.30016284075437483, 6.796348835713779124, -66.11047376476241766 ) ) ;
#45287 = VERTEX_POINT ( 'NONE', #67636 ) ;
#45286 = CARTESIAN_POINT ( 'NONE',  ( -10.92576759990585877, 8.121994053275065184, -62.92908167533382624 ) ) ;
#45288 = CARTESIAN_POINT ( 'NONE',  ( 39.40195752203892710, -170.0000000000000000, -69.96436805589145536 ) ) ;
#45289 = DIRECTION ( 'NONE',  ( -0.000000000000000000, -0.000000000000000000, -1.000000000000000000 ) ) ;
#45290 = CARTESIAN_POINT ( 'NONE',  ( -73.81801970646053235, 21.60231032711190480, -36.88809761374765372 ) ) ;
#45291 = EDGE_LOOP ( 'NONE', ( #46184, #18293, #68890, #19219 ) ) ;
#45292 = CARTESIAN_POINT ( 'NONE',  ( 212.1488570093001726, 119.0116247937291121, -71.54201036058580598 ) ) ;
#45293 = CARTESIAN_POINT ( 'NONE',  ( -65.99999999999994316, 29.79383981485516486, -80.00000000000000000 ) ) ;
#45295 = CARTESIAN_POINT ( 'NONE',  ( 116.5100763992442836, 33.01539745157280947, 41.23853340567732317 ) ) ;
#45294 = AXIS2_PLACEMENT_3D ( 'NONE', #9016, #58552, #51911 ) ;
#45296 = CARTESIAN_POINT ( 'NONE',  ( -130.5811943660944223, 50.88295841537571818, 5.400760641591992872 ) ) ;
#45297 = CARTESIAN_POINT ( 'NONE',  ( 16.28382582968306735, 7.523443033994205997, 71.85925826316895382 ) ) ;
#45298 = ORIENTED_EDGE ( 'NONE', *, *, #10246, .F. ) ;
#45299 = VERTEX_POINT ( 'NONE', #68328 ) ;
#45300 = ORIENTED_EDGE ( 'NONE', *, *, #36703, .T. ) ;
#45301 = VECTOR ( 'NONE', #759, 1000.000000000000000 ) ;
#45302 = B_SPLINE_CURVE_WITH_KNOTS ( 'NONE', 3,
 ( #981, #61111, #54776, #17495, #28398, #6602, #49139, #50208, #17854, #28048, #50555, #38608, #23134, #22429, #18547, #34396, #49844, #60756, #60050, #7300, #2034, #12231, #44219, #33346, #49489, #39312, #23488, #44583, #33695, #43867, #1321, #38968, #22776, #60414, #12577, #56174, #65703, #66062 ),
 .UNSPECIFIED., .F., .F.,
 ( 4, 2, 2, 2, 2, 2, 2, 2, 2, 2, 2, 2, 2, 2, 2, 2, 2, 2, 4 ),
 ( 1.387778780781445676E-17, 0.003908178031105357005, 0.005862267046658047216, 0.007816356062210738295, 0.009770445077763428507, 0.01172453409331611872, 0.01270157860109245862, 0.01367862310886879679, 0.01465566761664513669, 0.01563271212442147659, 0.01660975663219781476, 0.01758680113997415639, 0.01954089015552684314, 0.02051793466330320212, 0.02149497917107956457, 0.02344906818663228601, 0.02540315720218501092, 0.02735724621773773235, 0.03126542424884321686 ),
 .UNSPECIFIED. ) ;
#45303 = DIRECTION ( 'NONE',  ( -1.000000000000000000, 0.000000000000000000, 1.261617073437677999E-16 ) ) ;
#45304 = AXIS2_PLACEMENT_3D ( 'NONE', #46179, #62366, #67652 ) ;
#45305 = CARTESIAN_POINT ( 'NONE',  ( -31.43908319763709969, 9.591432048623767415, -50.31719736520186359 ) ) ;
#45306 = CARTESIAN_POINT ( 'NONE',  ( -98.33320668777302842, 30.82058677165679939, 85.32320660558336556 ) ) ;
#45307 = CARTESIAN_POINT ( 'NONE',  ( -147.3641864666714412, 62.38213854487951693, 31.02004508490727375 ) ) ;
#45308 = VECTOR ( 'NONE', #9505, 1000.000000000000000 ) ;
#45309 = CARTESIAN_POINT ( 'NONE',  ( 2.999999999999996003, 2.486033002269127373E-15, 20.30000000000000071 ) ) ;
#45310 = DIRECTION ( 'NONE',  ( 0.000000000000000000, 0.000000000000000000, -1.000000000000000000 ) ) ;
#45311 = EDGE_LOOP ( 'NONE', ( #48689, #8682 ) ) ;
#45313 = CARTESIAN_POINT ( 'NONE',  ( -104.1225399044495958, 34.86084180570100699, 30.74510362357437288 ) ) ;
#45312 = VECTOR ( 'NONE', #54931, 1000.000000000000000 ) ;
#45314 = VERTEX_POINT ( 'NONE', #20128 ) ;
#45315 = CARTESIAN_POINT ( 'NONE',  ( 36.08729376665095145, 8.001156100723207487, 44.15947279111765056 ) ) ;
#45316 = VECTOR ( 'NONE', #38074, 1000.000000000000000 ) ;
#45317 =( LENGTH_UNIT ( ) NAMED_UNIT ( * ) SI_UNIT ( .MILLI., .METRE. ) );
#45318 = DIRECTION ( 'NONE',  ( 0.000000000000000000, 0.000000000000000000, -1.000000000000000000 ) ) ;
#45319 = B_SPLINE_CURVE_WITH_KNOTS ( 'NONE', 3,
 ( #43494, #6213, #27667, #26643, #59328, #48076, #32949, #11479, #16076, #5860, #49461, #49107, #48406, #54390, #22048, #16763, #22748, #65672 ),
 .UNSPECIFIED., .F., .F.,
 ( 4, 2, 2, 2, 2, 2, 2, 2, 4 ),
 ( 0.01015325708522461443, 0.01143429661445663145, 0.01271533614368864848, 0.01399637567292066377, 0.01527741520215268080, 0.01655845473138469609, 0.01783949426061671312, 0.01912053378984873014, 0.02040157331908074717 ),
 .UNSPECIFIED. ) ;
#45320 = CYLINDRICAL_SURFACE ( 'NONE', #27615, 195.0000000000000000 ) ;
#45321 = DIRECTION ( 'NONE',  ( -0.000000000000000000, -0.000000000000000000, -1.000000000000000000 ) ) ;
#45322 = DIRECTION ( 'NONE',  ( -0.000000000000000000, -0.000000000000000000, 1.000000000000000000 ) ) ;
#45323 = CARTESIAN_POINT ( 'NONE',  ( -50.51700111023804851, 13.51182830536852997, 16.96585246969117122 ) ) ;
#45324 = VECTOR ( 'NONE', #34619, 1000.000000000000000 ) ;
#45325 = CARTESIAN_POINT ( 'NONE',  ( -6.774725108395958983, 24.06456107444435233, 0.000000000000000000 ) ) ;
#45326 = EDGE_CURVE ( 'NONE', #48528, #55351, #55745, .T. ) ;
#45327 = VERTEX_POINT ( 'NONE', #4633 ) ;
#45328 = CARTESIAN_POINT ( 'NONE',  ( 25.00000000000000000, 3.061616997868383043E-15, 30.00000000000000000 ) ) ;
#45329 = CARTESIAN_POINT ( 'NONE',  ( 0.000000000000000000, 0.000000000000000000, 0.000000000000000000 ) ) ;
#45330 = ORIENTED_EDGE ( 'NONE', *, *, #5150, .T. ) ;
#45331 = DIRECTION ( 'NONE',  ( -0.000000000000000000, 1.000000000000000000, -0.000000000000000000 ) ) ;
#45332 = CARTESIAN_POINT ( 'NONE',  ( -62.55320287144887459, 17.87319849854532450, 64.89944872409208187 ) ) ;
#45333 = CARTESIAN_POINT ( 'NONE',  ( 204.6977192012829789, -170.0000000000000000, 63.55227132923313604 ) ) ;
#45334 = ORIENTED_EDGE ( 'NONE', *, *, #8129, .F. ) ;
#45335 = DIRECTION ( 'NONE',  ( 0.000000000000000000, 1.000000000000000000, -0.000000000000000000 ) ) ;
#45337 = EDGE_CURVE ( 'NONE', #51958, #1836, #50969, .T. ) ;
#45336 = CARTESIAN_POINT ( 'NONE',  ( 152.2924710224604610, 54.98503313872888043, -65.03745591564339179 ) ) ;
#45338 = CARTESIAN_POINT ( 'NONE',  ( -34.74740905761647269, 10.15745573515589406, 44.46511832658496388 ) ) ;
#45339 = CARTESIAN_POINT ( 'NONE',  ( -29.02794087136069834, 9.207646203414356023, 71.67951027246965623 ) ) ;
#45340 = EDGE_CURVE ( 'NONE', #25681, #60309, #25767, .T. ) ;
#45341 = APPLICATION_CONTEXT ( 'automotive_design' ) ;
#45342 = ORIENTED_EDGE ( 'NONE', *, *, #11125, .F. ) ;
#45343 = EDGE_CURVE ( 'NONE', #51074, #40455, #29997, .T. ) ;
#45344 = CARTESIAN_POINT ( 'NONE',  ( -120.1497954511983437, 42.82624472369556656, 33.27088217181543683 ) ) ;
#45345 = ORIENTED_EDGE ( 'NONE', *, *, #57580, .T. ) ;
#45346 = CARTESIAN_POINT ( 'NONE',  ( 39.40195752203891999, 9.424259417798147354, -8.775266874964067654 ) ) ;
#45347 = DIRECTION ( 'NONE',  ( 0.000000000000000000, -0.7071067811865475727, -0.7071067811865475727 ) ) ;
#45348 = CARTESIAN_POINT ( 'NONE',  ( -417.6627218934913230, 399.9999999999997726, 113.5502958579881891 ) ) ;
#45349 = CARTESIAN_POINT ( 'NONE',  ( 130.8606599820531926, 40.81082399113100934, 83.81639294592298484 ) ) ;
#45350 = B_SPLINE_CURVE_WITH_KNOTS ( 'NONE', 3,
 ( #24828, #68429, #63153, #61755, #52917, #4742, #16338, #5088, #37792, #15988, #20926, #64879, #32178, #27580, #37437, #10030, #21609, #53259, #21958, #27229, #26553, #6119, #49019, #48318, #59235, #58212, #54296, #47986, #31827, #63496, #58890, #38133, #69452, #21269, #42717, #31484, #858, #10360, #10706, #36768, #506, #64174, #53611, #26206, #59575 ),
 .UNSPECIFIED., .F., .F.,
 ( 4, 2, 2, 2, 2, 2, 2, 2, 2, 2, 2, 2, 2, 1, 2, 2, 2, 2, 2, 2, 2, 2, 4 ),
 ( 0.02356759485890609976, 0.02503765354686412689, 0.02577268289084315434, 0.02650771223482217831, 0.02797777092278022279, 0.02944782961073826727, 0.03018285895471728084, 0.03091788829869629440, 0.03238794698665432847, 0.03312297633063336633, 0.03385800567461239030, 0.03532806436257047988, 0.03606309370654951774, 0.03679812305052856253, 0.03753315239450760732, 0.03826818173848664517, 0.03973824042644472782, 0.04120829911440281046, 0.04267835780236089310, 0.04341338714633992402, 0.04414841649031895493, 0.04561847517827700982, 0.04708853386623507165 ),
 .UNSPECIFIED. ) ;
#45351 = CARTESIAN_POINT ( 'NONE',  ( -24.57945280941397215, 9.580546049925253271, -93.35324784431733747 ) ) ;
#45352 = CARTESIAN_POINT ( 'NONE',  ( 15.55634918610403261, -3.079134169858832593E-14, 2.000000000000001776 ) ) ;
#45353 = PRESENTATION_LAYER_ASSIGNMENT (  '', '', ( #36365 ) ) ;
#45354 = ADVANCED_FACE ( 'NONE', ( #3268, #15197 ), #62351, .T. ) ;
#45355 = CARTESIAN_POINT ( 'NONE',  ( -125.4433371161043311, 46.19736518073186460, -61.75825448869758105 ) ) ;
#45356 = ORIENTED_EDGE ( 'NONE', *, *, #10683, .T. ) ;
#45357 = DIRECTION ( 'NONE',  ( 4.314083075427411048E-32, 1.000000000000000000, 6.123233995736763571E-17 ) ) ;
#45358 = FACE_OUTER_BOUND ( 'NONE', #43020, .T. ) ;
#45359 = CARTESIAN_POINT ( 'NONE',  ( -60.41792053122281914, 24.01035990323430624, 170.0000000000000000 ) ) ;
#45360 = CARTESIAN_POINT ( 'NONE',  ( -133.1180864139201390, 52.67432865667906583, -94.03100957856869968 ) ) ;
#45361 = DIRECTION ( 'NONE',  ( -1.000000000000000000, 0.000000000000000000, 0.000000000000000000 ) ) ;
#45362 = VECTOR ( 'NONE', #41189, 1000.000000000000000 ) ;
#45363 = VERTEX_POINT ( 'NONE', #53841 ) ;
#45364 = VECTOR ( 'NONE', #51723, 999.9999999999998863 ) ;
#45365 = LINE ( 'NONE', #29526, #20415 ) ;
#45366 = CIRCLE ( 'NONE', #27367, 65.00000000000000000 ) ;
#45367 = LINE ( 'NONE', #18636, #5913 ) ;
#45368 = VERTEX_POINT ( 'NONE', #59819 ) ;
#45369 = CARTESIAN_POINT ( 'NONE',  ( -452.6627218934912662, 364.9999999999998863, 113.5502958579877912 ) ) ;
#45370 = DIRECTION ( 'NONE',  ( -0.000000000000000000, -1.000000000000000000, -0.000000000000000000 ) ) ;
#45371 = VECTOR ( 'NONE', #4866, 1000.000000000000000 ) ;
#45372 = CIRCLE ( 'NONE', #63351, 25.00000000000145306 ) ;
#45373 = ORIENTED_EDGE ( 'NONE', *, *, #14159, .T. ) ;
#45374 = CARTESIAN_POINT ( 'NONE',  ( 164.8914542114683002, 64.97670918603526502, -44.74542541857194067 ) ) ;
#45375 = CARTESIAN_POINT ( 'NONE',  ( 57.30278335769541087, 48.40406511297401693, 43.58025477438756212 ) ) ;
#45376 = DIRECTION ( 'NONE',  ( 0.000000000000000000, 0.000000000000000000, -1.000000000000000000 ) ) ;
#45377 = CARTESIAN_POINT ( 'NONE',  ( 0.000000000000000000, 0.000000000000000000, -8.000000000000000000 ) ) ;
#45378 = ORIENTED_EDGE ( 'NONE', *, *, #15811, .T. ) ;
#45379 = DIRECTION ( 'NONE',  ( 0.000000000000000000, -1.224646799147351975E-16, 1.000000000000000000 ) ) ;
#45380 = CARTESIAN_POINT ( 'NONE',  ( 64.34362785825726405, 14.01885293761273665, 83.61320876023768278 ) ) ;
#45381 = DIRECTION ( 'NONE',  ( -0.7071067811865543451, -7.105427357601001070E-15, -0.7071067811865408004 ) ) ;
#45382 = CARTESIAN_POINT ( 'NONE',  ( 83.59652366361572717, 19.46709838196855102, -9.613360744613480335 ) ) ;
#45383 = CARTESIAN_POINT ( 'NONE',  ( -133.0808647576834005, 51.41195281028756625, -13.40905688364864190 ) ) ;
#45384 = DIRECTION ( 'NONE',  ( 0.000000000000000000, 0.000000000000000000, 1.000000000000000000 ) ) ;
#45385 = CARTESIAN_POINT ( 'NONE',  ( 126.9201538765324386, 37.39093565120715112, -67.50410470727368306 ) ) ;
#45386 = VERTEX_POINT ( 'NONE', #16914 ) ;
#45387 = CARTESIAN_POINT ( 'NONE',  ( -101.8140949286062096, 33.67224128592400945, 72.36362509687882039 ) ) ;
#45388 = CARTESIAN_POINT ( 'NONE',  ( -15.27594996066617483, 8.502079791899653571, 63.47073034068081654 ) ) ;
#45389 = ORIENTED_EDGE ( 'NONE', *, *, #20941, .F. ) ;
#45390 = FACE_OUTER_BOUND ( 'NONE', #19815, .T. ) ;
#45391 = CARTESIAN_POINT ( 'NONE',  ( 46.66904755831207297, -15.55634918610412853, 2.000000000000001776 ) ) ;
#45392 = CARTESIAN_POINT ( 'NONE',  ( 3.000000000000028866, 0.000000000000000000, -3.000000000000030198 ) ) ;
#45393 = ADVANCED_FACE ( 'NONE', ( #27120 ), #16570, .T. ) ;
#45394 = CARTESIAN_POINT ( 'NONE',  ( -0.5783162822156596716, 7.534184941292927817, 39.56237465081175486 ) ) ;
#45395 = DIRECTION ( 'NONE',  ( -0.000000000000000000, -0.000000000000000000, 1.000000000000000000 ) ) ;
#45396 = PLANE ( 'NONE',  #8992 ) ;
#45397 = CARTESIAN_POINT ( 'NONE',  ( -4.731197926646204088, 7.716745361328043451, -22.90991753403145736 ) ) ;
#45398 = LINE ( 'NONE', #59823, #4049 ) ;
#45399 = CARTESIAN_POINT ( 'NONE',  ( -62.15799747763098537, 16.70234469631017404, 8.520624946596262461 ) ) ;
#45400 = ORIENTED_EDGE ( 'NONE', *, *, #43446, .T. ) ;
#45401 = CIRCLE ( 'NONE', #15076, 25.12245591505646303 ) ;
#45402 = LINE ( 'NONE', #24656, #27323 ) ;
#45403 = ORIENTED_EDGE ( 'NONE', *, *, #62259, .T. ) ;
#45404 = CARTESIAN_POINT ( 'NONE',  ( 104.7034219878852355, 26.40210929103713511, -75.34717264657832914 ) ) ;
#45405 = CARTESIAN_POINT ( 'NONE',  ( 43.96421756700841144, 10.06386361114659955, -22.24800231128863004 ) ) ;
#45406 =( GEOMETRIC_REPRESENTATION_CONTEXT ( 3 ) GLOBAL_UNCERTAINTY_ASSIGNED_CONTEXT ( ( #40922 ) ) GLOBAL_UNIT_ASSIGNED_CONTEXT ( ( #46970, #15649, #20570 ) ) REPRESENTATION_CONTEXT ( 'NONE', 'WORKASPACE' ) );
#45407 = CARTESIAN_POINT ( 'NONE',  ( 43.35980717318837918, 8.957244490220908517, 70.63379478250071486 ) ) ;
#45408 = DIRECTION ( 'NONE',  ( -0.6246950475544236214, 7.650307904307285654E-17, 0.7808688094430308313 ) ) ;
#45409 = DIRECTION ( 'NONE',  ( 0.000000000000000000, 1.000000000000000000, -0.000000000000000000 ) ) ;
#45410 = CARTESIAN_POINT ( 'NONE',  ( 15.55634918610396511, -41.66904755831214402, 2.000000000000001776 ) ) ;
#45411 = AXIS2_PLACEMENT_3D ( 'NONE', #10939, #34458, #49908 ) ;
#45412 = PLANE ( 'NONE',  #42047 ) ;
#45413 = CARTESIAN_POINT ( 'NONE',  ( -169.8842709557924309, 83.59602878049473418, 58.38604360640643876 ) ) ;
#45414 = VERTEX_POINT ( 'NONE', #21496 ) ;
#45415 = ORIENTED_EDGE ( 'NONE', *, *, #53684, .F. ) ;
#45416 = VECTOR ( 'NONE', #24094, 1000.000000000000000 ) ;
#45418 = EDGE_CURVE ( 'NONE', #48695, #22683, #11013, .T. ) ;
#45417 = DIRECTION ( 'NONE',  ( -0.000000000000000000, 1.000000000000000000, -0.000000000000000000 ) ) ;
#45419 = CARTESIAN_POINT ( 'NONE',  ( 447.3372781065085633, 400.0000000000000568, -146.4497041420117966 ) ) ;
#45420 = DIRECTION ( 'NONE',  ( -1.000000000000000000, 0.000000000000000000, 0.000000000000000000 ) ) ;
#45421 = CARTESIAN_POINT ( 'NONE',  ( 103.9685899589048148, 27.18106603025991319, 59.83941942854519169 ) ) ;
#45422 = AXIS2_PLACEMENT_3D ( 'NONE', #69227, #42160, #21728 ) ;
#45423 = LINE ( 'NONE', #8141, #29640 ) ;
#45424 = EDGE_CURVE ( 'NONE', #18637, #53396, #31047, .T. ) ;
#45425 = CARTESIAN_POINT ( 'NONE',  ( 55.91133443650747381, 12.16263767238153193, -18.83026767310629879 ) ) ;
#45426 = VERTEX_POINT ( 'NONE', #4978 ) ;
#45427 = DIRECTION ( 'NONE',  ( -1.334402673828311663E-15, 1.000000000000000000, -1.465981474576325310E-14 ) ) ;
#45428 = CARTESIAN_POINT ( 'NONE',  ( 0.000000000000000000, 0.000000000000000000, -7.000000000000000000 ) ) ;
#45429 = CARTESIAN_POINT ( 'NONE',  ( -84.97622048504842951, 24.82614411847756486, -19.83267697168680499 ) ) ;
#45430 = CARTESIAN_POINT ( 'NONE',  ( 0.000000000000000000, 0.000000000000000000, -4.999999999999997335 ) ) ;
#45431 = CARTESIAN_POINT ( 'NONE',  ( 175.5429257635130682, 74.57009623370763052, -11.80030295197366996 ) ) ;
#45432 = CARTESIAN_POINT ( 'NONE',  ( 9.034661095809960685, 6.378368787883688107, -93.41972067307213479 ) ) ;
#45433 = EDGE_CURVE ( 'NONE', #28173, #60623, #26447, .T. ) ;
#45434 = EDGE_LOOP ( 'NONE', ( #18692, #34587, #8755, #8741 ) ) ;
#45435 = DIRECTION ( 'NONE',  ( 1.000000000000000000, 0.000000000000000000, 0.000000000000000000 ) ) ;
#45436 = DIRECTION ( 'NONE',  ( -0.000000000000000000, -1.000000000000000000, 0.000000000000000000 ) ) ;
#45437 = CARTESIAN_POINT ( 'NONE',  ( -31.11269837220801193, 36.11269837220812207, 2.000000000000001776 ) ) ;
#45438 = CARTESIAN_POINT ( 'NONE',  ( -180.2188652555596775, 96.98354576637426305, 9.036536700887030094 ) ) ;
#45439 = CARTESIAN_POINT ( 'NONE',  ( 152.6560521232695464, 54.00248515670892147, 4.308935166207688461 ) ) ;
#45440 = EDGE_CURVE ( 'NONE', #41688, #56069, #1806, .T. ) ;
#45441 = CARTESIAN_POINT ( 'NONE',  ( 35.43132383622789661, 14.63273331248878506, 13.32819299319723072 ) ) ;
#45442 = ORIENTED_EDGE ( 'NONE', *, *, #41864, .T. ) ;
#45443 = FACE_BOUND ( 'NONE', #36363, .T. ) ;
#45444 = CARTESIAN_POINT ( 'NONE',  ( 200.4574930424075205, 102.3536505870638251, -37.62237834330278474 ) ) ;
#45445 = ORIENTED_EDGE ( 'NONE', *, *, #7644, .F. ) ;
#45446 = CARTESIAN_POINT ( 'NONE',  ( -5.767955557622883589E-14, -26.11269837220806522, 2.000000000000001776 ) ) ;
#45447 = ORIENTED_EDGE ( 'NONE', *, *, #64243, .F. ) ;
#45448 = AXIS2_PLACEMENT_3D ( 'NONE', #31972, #42850, #48126 ) ;
#45449 = CARTESIAN_POINT ( 'NONE',  ( -85.35127931077728647, 24.98147633332999717, -72.86973326730625899 ) ) ;
#45450 = LINE ( 'NONE', #66242, #36629 ) ;
#45451 = CARTESIAN_POINT ( 'NONE',  ( 94.02499804464936517, 23.15433260743126098, -68.89411343564552226 ) ) ;
#45452 = ORIENTED_EDGE ( 'NONE', *, *, #52356, .T. ) ;
#45453 = ORIENTED_EDGE ( 'NONE', *, *, #48905, .F. ) ;
#45454 = CARTESIAN_POINT ( 'NONE',  ( 41.80869235728137312, 9.750404582811606602, 57.13814906687242257 ) ) ;
#45455 = CARTESIAN_POINT ( 'NONE',  ( 0.000000000000000000, 0.000000000000000000, -10.00000000000000000 ) ) ;
#45456 = CARTESIAN_POINT ( 'NONE',  ( 23.23895241123075195, 6.853530908437178049, 9.681958699395883272 ) ) ;
#45457 = ORIENTED_EDGE ( 'NONE', *, *, #56393, .T. ) ;
#45458 = VECTOR ( 'NONE', #4835, 1000.000000000000114 ) ;
#45459 = AXIS2_PLACEMENT_3D ( 'NONE', #1735, #6304, #55533 ) ;
#45460 = CARTESIAN_POINT ( 'NONE',  ( -52.67596829228262578, 15.09584868440939331, -49.84632435105815063 ) ) ;
#45461 = CARTESIAN_POINT ( 'NONE',  ( 59.08202327466404569, 12.82375733818951247, -36.83031859667770647 ) ) ;
#45462 = VECTOR ( 'NONE', #58247, 1000.000000000000000 ) ;
#45463 = CARTESIAN_POINT ( 'NONE',  ( -9.510892918907986271, 8.014150818648904107, -89.24936681866903143 ) ) ;
#45464 = CARTESIAN_POINT ( 'NONE',  ( 46.66904755831212981, 20.55634918610394379, 2.000000000000001776 ) ) ;
#45465 = CARTESIAN_POINT ( 'NONE',  ( 0.000000000000000000, 0.000000000000000000, 5.000000000000000000 ) ) ;
#45467 = ORIENTED_EDGE ( 'NONE', *, *, #3205, .F. ) ;
#45466 = PLANE ( 'NONE',  #1788 ) ;
#45468 = VERTEX_POINT ( 'NONE', #17979 ) ;
#45469 = ORIENTED_EDGE ( 'NONE', *, *, #18507, .F. ) ;
#45470 = CARTESIAN_POINT ( 'NONE',  ( -10.50008313721455089, 40.38642104775755115, 13.79046412294882984 ) ) ;
#45471 = FACE_OUTER_BOUND ( 'NONE', #59038, .T. ) ;
#45472 = CARTESIAN_POINT ( 'NONE',  ( 100.0000000000000284, 0.000000000000000000, 0.000000000000000000 ) ) ;
#45473 = EDGE_CURVE ( 'NONE', #28668, #44925, #17622, .T. ) ;
#45474 = CARTESIAN_POINT ( 'NONE',  ( 102.8458551240039611, 25.60773946375957166, -17.84239502940274846 ) ) ;
#45475 = CARTESIAN_POINT ( 'NONE',  ( 197.3707490726349931, 96.80690576410101755, 11.49558936419983546 ) ) ;
#45476 = DIRECTION ( 'NONE',  ( 0.7100673072878298520, 0.7041338076821838099, 0.000000000000000000 ) ) ;
#45477 = FACE_OUTER_BOUND ( 'NONE', #51119, .T. ) ;
#45478 = DIRECTION ( 'NONE',  ( 0.000000000000000000, 0.000000000000000000, 1.000000000000000000 ) ) ;
#45479 = CARTESIAN_POINT ( 'NONE',  ( -15.32520546926283522, 7.495995523981878073, 38.10845715258894728 ) ) ;
#45481 = EDGE_LOOP ( 'NONE', ( #52131, #15056, #47614, #54261 ) ) ;
#45480 = EDGE_CURVE ( 'NONE', #28072, #13483, #48741, .T. ) ;
#45482 = CARTESIAN_POINT ( 'NONE',  ( 86.62931800182293784, -170.0000000000000000, 56.55663816294300261 ) ) ;
#45483 = ORIENTED_EDGE ( 'NONE', *, *, #31596, .F. ) ;
#45484 = ORIENTED_EDGE ( 'NONE', *, *, #24502, .T. ) ;
#45485 = LINE ( 'NONE', #56743, #608 ) ;
#45486 = CARTESIAN_POINT ( 'NONE',  ( 188.4920037102893957, 87.93425473911915446, -69.36007641940153690 ) ) ;
#45487 = CARTESIAN_POINT ( 'NONE',  ( -34.85264071515286588, 11.19872911336657850, 84.71973201243903873 ) ) ;
#45488 = CARTESIAN_POINT ( 'NONE',  ( -97.47339919287391297, 30.40512551257287299, -36.73650405462576884 ) ) ;
#45489 = CARTESIAN_POINT ( 'NONE',  ( -31.11269837220809364, -15.55634918610397754, 2.000000000000001776 ) ) ;
#45490 = LINE ( 'NONE', #66288, #23600 ) ;
#45491 = CARTESIAN_POINT ( 'NONE',  ( 126.3541873520043737, 37.07520218256170352, -44.02282603433466335 ) ) ;
#45492 = ORIENTED_EDGE ( 'NONE', *, *, #3701, .T. ) ;
#45493 = ADVANCED_FACE ( 'NONE', ( #17261 ), #66186, .T. ) ;
#45494 = ORIENTED_EDGE ( 'NONE', *, *, #960, .T. ) ;
#45495 = EDGE_CURVE ( 'NONE', #51871, #34356, #28526, .T. ) ;
#45496 = AXIS2_PLACEMENT_3D ( 'NONE', #57425, #30349, #9931 ) ;
#45497 = CARTESIAN_POINT ( 'NONE',  ( 187.9556299234372148, 87.33837712034319622, 87.48685922188801101 ) ) ;
#45498 = CARTESIAN_POINT ( 'NONE',  ( -15.22871623201694469, 7.486724405784662473, 9.545765994695932122 ) ) ;
#45499 = CARTESIAN_POINT ( 'NONE',  ( -45.81425895439424067, 46.10914959592843587, 40.00000000000003553 ) ) ;
#45500 = CARTESIAN_POINT ( 'NONE',  ( -28.81317668042940738, 9.175023678939295380, -76.69123791734521944 ) ) ;
#45501 = ADVANCED_FACE ( 'NONE', ( #39772 ), #43990, .F. ) ;
#45502 = AXIS2_PLACEMENT_3D ( 'NONE', #28430, #24483, #25859 ) ;
#45503 = ADVANCED_FACE ( 'NONE', ( #18317 ), #33805, .F. ) ;
#45504 = DIRECTION ( 'NONE',  ( 1.850371928290090422E-16, -1.000000000000000000, -1.110223024625156294E-16 ) ) ;
#45505 = ORIENTED_EDGE ( 'NONE', *, *, #6745, .F. ) ;
#45506 = CARTESIAN_POINT ( 'NONE',  ( 0.000000000000000000, 0.000000000000000000, 2.000000000000001776 ) ) ;
#45507 = AXIS2_PLACEMENT_3D ( 'NONE', #50067, #65202, #11727 ) ;
#45508 = AXIS2_PLACEMENT_3D ( 'NONE', #25892, #25556, #68777 ) ;
#45509 = CARTESIAN_POINT ( 'NONE',  ( -57.43883374585512769, 16.37892664338859205, -62.44644220765625420 ) ) ;
#45510 = CARTESIAN_POINT ( 'NONE',  ( 199.7291770695760533, 101.4092159658447372, -65.04710708279223752 ) ) ;
#45511 = CARTESIAN_POINT ( 'NONE',  ( 278.2349883415517411, -21.49634503089637150, 4.680941717099500465 ) ) ;
#45512 = DIRECTION ( 'NONE',  ( 0.000000000000000000, -0.000000000000000000, -1.000000000000000000 ) ) ;
#45513 = CARTESIAN_POINT ( 'NONE',  ( -166.2028193222418793, 79.74385139484274987, 8.566800144892136260 ) ) ;
#45514 = FACE_OUTER_BOUND ( 'NONE', #14903, .T. ) ;
#45515 = CARTESIAN_POINT ( 'NONE',  ( -47.80896875121164413, 12.85816703949530826, 66.62128856524451237 ) ) ;
#45516 = AXIS2_PLACEMENT_3D ( 'NONE', #6256, #15446, #36897 ) ;
#45517 = VECTOR ( 'NONE', #7590, 1000.000000000000000 ) ;
#45518 = EDGE_CURVE ( 'NONE', #54364, #29971, #29887, .T. ) ;
#45519 = CYLINDRICAL_SURFACE ( 'NONE', #32761, 5.000000000000004441 ) ;
#45520 = ORIENTED_EDGE ( 'NONE', *, *, #20575, .F. ) ;
#45521 = LINE ( 'NONE', #29692, #38317 ) ;
#45522 = CARTESIAN_POINT ( 'NONE',  ( 15.78827728214693416, 7.507518794609596924, -89.20804527961313113 ) ) ;
#45523 = DIRECTION ( 'NONE',  ( 1.000000000000000000, 0.000000000000000000, 0.000000000000000000 ) ) ;
#45524 = EDGE_CURVE ( 'NONE', #58687, #15601, #38733, .T. ) ;
#45525 = LINE ( 'NONE', #55738, #39083 ) ;
#45526 = ADVANCED_FACE ( 'NONE', ( #34516 ), #6718, .F. ) ;
#45527 = CARTESIAN_POINT ( 'NONE',  ( 34.30072871347309871, 36.58596684574257552, -74.30072871347312002 ) ) ;
#45528 = ORIENTED_EDGE ( 'NONE', *, *, #1411, .T. ) ;
#45529 = CARTESIAN_POINT ( 'NONE',  ( -189.2776534485022069, 107.1424877329940841, -95.00000000000133582 ) ) ;
#45530 = CARTESIAN_POINT ( 'NONE',  ( -4.000000000000009770, -6.928203230275505220, 0.000000000000000000 ) ) ;
#45531 = ORIENTED_EDGE ( 'NONE', *, *, #11573, .T. ) ;
#45532 = ORIENTED_EDGE ( 'NONE', *, *, #67592, .F. ) ;
#45533 = CARTESIAN_POINT ( 'NONE',  ( 61.91366885787729046, 28.42865614899000448, 43.58025477438756923 ) ) ;
#45534 = CARTESIAN_POINT ( 'NONE',  ( 150.2060369882285329, 53.45752899907542144, 38.79508757824569898 ) ) ;
#45535 = CARTESIAN_POINT ( 'NONE',  ( 37.92109651401251114, 5.611248309713812610, 13.32819397642332859 ) ) ;
#45536 = ORIENTED_EDGE ( 'NONE', *, *, #14944, .F. ) ;
#45537 = CARTESIAN_POINT ( 'NONE',  ( 10.00000000000000000, 0.000000000000000000, -4.999999999999997335 ) ) ;
#45538 = DIRECTION ( 'NONE',  ( 0.000000000000000000, 0.000000000000000000, 1.000000000000000000 ) ) ;
#45539 = CARTESIAN_POINT ( 'NONE',  ( -0.8011128725815486185, 6.535315321814185729, 13.41110674575676853 ) ) ;
#45540 = CARTESIAN_POINT ( 'NONE',  ( 55.91494169499919309, 12.16343363043256964, -40.79342870396418874 ) ) ;
#45541 = CARTESIAN_POINT ( 'NONE',  ( -80.32755469740932597, 24.04130076192509335, 45.23585681520698643 ) ) ;
#45542 = CARTESIAN_POINT ( 'NONE',  ( 152.9292068394840101, 54.20367164619623424, 84.59218010126255649 ) ) ;
#45543 = CARTESIAN_POINT ( 'NONE',  ( 140.9169160367233360, 45.85398962664667977, 12.74973608567994354 ) ) ;
#45544 = EDGE_LOOP ( 'NONE', ( #50748, #50594, #24223, #48246 ) ) ;
#45545 = CARTESIAN_POINT ( 'NONE',  ( 29.69502258243350923, 57.82046033912877903, 40.00000000000003553 ) ) ;
#45546 = CIRCLE ( 'NONE', #48933, 5.000000000000060396 ) ;
#45547 = CARTESIAN_POINT ( 'NONE',  ( -5.066666666666671759, 8.000000000000000000, -11.86666666666666536 ) ) ;
#45548 = FACE_BOUND ( 'NONE', #25577, .T. ) ;
#45549 = FACE_BOUND ( 'NONE', #33795, .T. ) ;
#45550 = AXIS2_PLACEMENT_3D ( 'NONE', #2164, #8477, #67917 ) ;
#45552 = ORIENTED_EDGE ( 'NONE', *, *, #9122, .F. ) ;
#45551 = CARTESIAN_POINT ( 'NONE',  ( -118.5596554410405616, 41.85073040176283143, 93.41348078571337510 ) ) ;
#45553 = DIRECTION ( 'NONE',  ( 1.000000000000000000, 0.000000000000000000, 0.000000000000000000 ) ) ;
#45554 = VECTOR ( 'NONE', #39280, 1000.000000000000227 ) ;
#45555 = VECTOR ( 'NONE', #22949, 1000.000000000000227 ) ;
#45556 = ORIENTED_EDGE ( 'NONE', *, *, #63546, .F. ) ;
#45557 = CARTESIAN_POINT ( 'NONE',  ( -142.8450945664714880, 58.72815783657286204, 68.52009029614266922 ) ) ;
#45558 = CARTESIAN_POINT ( 'NONE',  ( 82.34401416830216647, 19.05992892018826623, 31.05207311871945564 ) ) ;
#45559 = CARTESIAN_POINT ( 'NONE',  ( 0.000000000000000000, 0.000000000000000000, 40.00000000000003553 ) ) ;
#45560 = AXIS2_PLACEMENT_3D ( 'NONE', #67852, #58645, #68197 ) ;
#45562 = CARTESIAN_POINT ( 'NONE',  ( 188.5843222076478582, 86.53342480589847696, -16.58390079652848570 ) ) ;
#45561 = AXIS2_PLACEMENT_3D ( 'NONE', #36042, #63119, #40971 ) ;
#45563 = CARTESIAN_POINT ( 'NONE',  ( 140.4586216751744701, 45.55624550472997925, -20.24665479566528248 ) ) ;
#45564 = DIRECTION ( 'NONE',  ( 0.000000000000000000, -1.000000000000000000, -2.921639538487254261E-16 ) ) ;
#45565 = CARTESIAN_POINT ( 'NONE',  ( -180.5954680880247452, 97.44843622358463620, -16.00758145678837963 ) ) ;
#45566 = EDGE_CURVE ( 'NONE', #21955, #60768, #65607, .T. ) ;
#45567 = CIRCLE ( 'NONE', #11813, 5.000000000000004441 ) ;
#45568 = CARTESIAN_POINT ( 'NONE',  ( -48.34250119710923599, 14.01879126850789348, 34.45810225024617779 ) ) ;
#45569 = ORIENTED_EDGE ( 'NONE', *, *, #39402, .T. ) ;
#45570 = EDGE_LOOP ( 'NONE', ( #51776, #61305 ) ) ;
#45571 = DIRECTION ( 'NONE',  ( -1.850169831522831466E-16, 1.000000000000000000, 1.110223024625156294E-16 ) ) ;
#45572 = CARTESIAN_POINT ( 'NONE',  ( 19.00668540189186473, 62.54164772954719353, 41.38025477438755928 ) ) ;
#45573 = PLANE ( 'NONE',  #18297 ) ;
#45574 = CARTESIAN_POINT ( 'NONE',  ( 188.4904153916304779, 86.42965364612516055, -44.94447516463474557 ) ) ;
#45575 = CARTESIAN_POINT ( 'NONE',  ( -108.5289085648060592, 36.07014995015114778, 69.01860148035208908 ) ) ;
#45576 = CARTESIAN_POINT ( 'NONE',  ( -24.32937228292060894, 8.531905774118440533, -45.25531289717756778 ) ) ;
#45577 = LINE ( 'NONE', #67395, #43043 ) ;
#45578 = EDGE_LOOP ( 'NONE', ( #61664, #67387 ) ) ;
#45579 = EDGE_CURVE ( 'NONE', #56240, #18531, #8816, .T. ) ;
#45580 = EDGE_LOOP ( 'NONE', ( #34128, #21886 ) ) ;
#45581 = EDGE_CURVE ( 'NONE', #23252, #41022, #35542, .T. ) ;
#45582 = ORIENTED_EDGE ( 'NONE', *, *, #5645, .T. ) ;
#45583 = ADVANCED_FACE ( 'NONE', ( #4222 ), #3874, .F. ) ;
#45584 = LINE ( 'NONE', #17096, #7154 ) ;
#45585 = CARTESIAN_POINT ( 'NONE',  ( -72.02029401400447739, 19.90008195119185075, 88.07226044993944924 ) ) ;
#45586 = CARTESIAN_POINT ( 'NONE',  ( -79.14678386417816114, 22.50468917936073865, 72.26275173013684139 ) ) ;
#45587 = DIRECTION ( 'NONE',  ( -0.000000000000000000, 1.000000000000000000, -0.000000000000000000 ) ) ;
#45588 = LINE ( 'NONE', #61075, #31055 ) ;
#45589 = EDGE_CURVE ( 'NONE', #38519, #55744, #19701, .T. ) ;
#45590 = CARTESIAN_POINT ( 'NONE',  ( -59.96408504033280451, 17.10126854471815605, 43.50660429605553503 ) ) ;
#45591 = CARTESIAN_POINT ( 'NONE',  ( -95.86163447241558799, 30.75089131639704121, -19.58197702406704366 ) ) ;
#45592 = CARTESIAN_POINT ( 'NONE',  ( 58.46823952472681896, 12.69204591816732552, 43.29726459483626400 ) ) ;
#45593 = LINE ( 'NONE', #2687, #37164 ) ;
#45594 = LINE ( 'NONE', #39627, #15139 ) ;
#45595 = VERTEX_POINT ( 'NONE', #3521 ) ;
#45596 = CARTESIAN_POINT ( 'NONE',  ( -6.126800896373026717, 6.786243985899687914, -50.22733277754976911 ) ) ;
#45597 = CARTESIAN_POINT ( 'NONE',  ( 41.71033745877218735, 1.250000000000018652, 13.79046412284416867 ) ) ;
#45598 = DIRECTION ( 'NONE',  ( 0.000000000000000000, -6.123233995736762338E-17, 1.000000000000000000 ) ) ;
#45599 = DIRECTION ( 'NONE',  ( -0.000000000000000000, 0.000000000000000000, -1.000000000000000000 ) ) ;
#45600 = CARTESIAN_POINT ( 'NONE',  ( 284.9673805781174565, -21.99252023018708968, 0.6578219585122039303 ) ) ;
#45601 = LINE ( 'NONE', #66392, #52433 ) ;
#45602 = B_SPLINE_CURVE_WITH_KNOTS ( 'NONE', 3,
 ( #57840, #46939, #3002, #47273, #20536, #52213, #67372, #25154, #25502, #20204, #31119, #30078, #35704, #41660, #67712, #63118, #19162, #25841, #62068, #19867, #46582, #42005, #52555, #4380, #56809, #3339, #24799, #46236, #19510, #68063, #40970, #62777, #14581, #37754, #64494, #21240, #26861, #48629, #59544, #15960, #42351, #20895, #31454, #59202, #10670, #26172, #52888, #42686, #5054, #16305, #4713, #58512, #6086, #11021, #48286, #32485 ),
 .UNSPECIFIED., .F., .F.,
 ( 4, 2, 2, 2, 2, 2, 2, 2, 2, 2, 2, 2, 2, 2, 2, 2, 2, 2, 2, 2, 2, 2, 2, 2, 2, 2, 2, 4 ),
 ( 0.000000000000000000, 0.001959203338812263041, 0.002938805008218370492, 0.003918406677624477509, 0.004898008347030584526, 0.005877610016436692411, 0.006857211685842799428, 0.007836813355248906446, 0.008816415024655013463, 0.009796016694061120481, 0.01175522003287333452, 0.01273482170227945888, 0.01371442337168558498, 0.01469402504109170761, 0.01567362671049783371, 0.01763283004931008244, 0.01959203338812233117, 0.02057163505752843818, 0.02155123672693454520, 0.02253083839634065569, 0.02351044006574676271, 0.02546964340455896286, 0.02644924507396507682, 0.02742884674337118731, 0.02840844841277729779, 0.02938805008218340481, 0.03036765175158951877, 0.03134725342099562578 ),
 .UNSPECIFIED. ) ;
#45603 = CARTESIAN_POINT ( 'NONE',  ( 126.4219470349615619, 38.26519385429182307, -15.65615810876642655 ) ) ;
#45604 = AXIS2_PLACEMENT_3D ( 'NONE', #49430, #63296, #4545 ) ;
#45605 = ORIENTED_EDGE ( 'NONE', *, *, #10010, .F. ) ;
#45606 = CIRCLE ( 'NONE', #56863, 5.000000000000004441 ) ;
#45607 = CARTESIAN_POINT ( 'NONE',  ( 676.6563798336520676, 863.5652367862173833, 653.5068267248699385 ) ) ;
#45608 = CARTESIAN_POINT ( 'NONE',  ( 126.3732561463888402, 38.23795180971328023, -44.08787207326391666 ) ) ;
#45609 = CARTESIAN_POINT ( 'NONE',  ( -38.68632430131782485, 11.91908191268691475, -40.87075332870919198 ) ) ;
#45610 = EDGE_CURVE ( 'NONE', #7485, #49653, #8555, .T. ) ;
#45611 = DIRECTION ( 'NONE',  ( -0.000000000000000000, -1.000000000000000000, -0.000000000000000000 ) ) ;
#45612 = ITEM_DEFINED_TRANSFORMATION ( 'NONE', 'NONE', #69092,  #66832 ) ;
#45613 = CARTESIAN_POINT ( 'NONE',  ( -174.2769963701057634, 88.42283341462002966, 84.58341184452997652 ) ) ;
#45614 = ORIENTED_EDGE ( 'NONE', *, *, #13111, .F. ) ;
#45616 = CARTESIAN_POINT ( 'NONE',  ( 126.6464677212869532, 38.39096133771045061, 8.034511553305282661 ) ) ;
#45615 = VECTOR ( 'NONE', #45249, 1000.000000000000000 ) ;
#45617 = AXIS2_PLACEMENT_3D ( 'NONE', #50192, #49829, #34378 ) ;
#45618 = EDGE_CURVE ( 'NONE', #9937, #31046, #46779, .T. ) ;
#45619 = B_SPLINE_CURVE_WITH_KNOTS ( 'NONE', 3,
 ( #50134, #1959, #27972, #49416, #38890, #66336, #18128, #34310, #55758, #7584, #29038, #23750, #45196, #66675, #18472, #52206, #68053, #30758, #36030, #3670, #34999, #57488, #9295, #61719, #56440, #62061, #29369, #13876, #63107, #4022, #46576, #19857, #41314, #25491, #7919, #40961, #40271, #3331, #8959, #46230, #30406, #20196, #30072, #67706 ),
 .UNSPECIFIED., .F., .F.,
 ( 4, 2, 2, 2, 2, 2, 2, 2, 2, 2, 2, 2, 2, 2, 2, 2, 2, 2, 2, 2, 2, 4 ),
 ( 6.938893903907227607E-18, 0.001473754749730481336, 0.002210632124595723631, 0.002947509499460966142, 0.004421264249191440322, 0.005895018998921913202, 0.007368773748652386081, 0.008105651123517621653, 0.008842528498382856358, 0.01031628324811331883, 0.01179003799784377957, 0.01252691537270901080, 0.01326379274757424551, 0.01473754749730471839, 0.01547442487216995656, 0.01621130224703519473, 0.01768505699676566414, 0.01915881174649614049, 0.01989568912136138040, 0.02063256649622662031, 0.02210632124595709319, 0.02358007599568756954 ),
 .UNSPECIFIED. ) ;
#45620 = CARTESIAN_POINT ( 'NONE',  ( 6.400000000000000355, 4.618802153517004960, 8.000000000000000000 ) ) ;
#45621 = VECTOR ( 'NONE', #65190, 1000.000000000000000 ) ;
#45622 = AXIS2_PLACEMENT_3D ( 'NONE', #3802, #15394, #46016 ) ;
#45623 = CARTESIAN_POINT ( 'NONE',  ( 198.4045886930829283, 99.71425793793709147, 5.774369385283677047 ) ) ;
#45624 = EDGE_LOOP ( 'NONE', ( #53392, #48606 ) ) ;
#45625 = SHAPE_REPRESENTATION ( 'key2', ( #66832 ), #63539 ) ;
#45626 = VECTOR ( 'NONE', #48559, 1000.000000000000000 ) ;
#45627 = CARTESIAN_POINT ( 'NONE',  ( 163.5430354047457229, 63.84092878795252801, 94.99999999999866418 ) ) ;
#45628 = ORIENTED_EDGE ( 'NONE', *, *, #23537, .T. ) ;
#45629 = CARTESIAN_POINT ( 'NONE',  ( -55.05276343752909440, 15.72344139423348430, 18.47277718246750311 ) ) ;
#45630 = LINE ( 'NONE', #9377, #36226 ) ;
#45631 = CARTESIAN_POINT ( 'NONE',  ( 0.000000000000000000, 0.000000000000000000, 41.38025477438755928 ) ) ;
#45632 = DIRECTION ( 'NONE',  ( 0.000000000000000000, -0.000000000000000000, -1.000000000000000000 ) ) ;
#45633 = CARTESIAN_POINT ( 'NONE',  ( 0.000000000000000000, 0.000000000000000000, 0.000000000000000000 ) ) ;
#45635 = VERTEX_POINT ( 'NONE', #63311 ) ;
#45634 = FACE_OUTER_BOUND ( 'NONE', #24406, .T. ) ;
#45636 = CARTESIAN_POINT ( 'NONE',  ( 55.57657751403269941, 11.06944050856661832, 36.32677378882770824 ) ) ;
#45637 = VERTEX_POINT ( 'NONE', #20054 ) ;
#45638 = ORIENTED_EDGE ( 'NONE', *, *, #66493, .T. ) ;
#45639 = CARTESIAN_POINT ( 'NONE',  ( -168.0052514572427071, 83.06849406765624622, 16.96694403013009733 ) ) ;
#45640 = CARTESIAN_POINT ( 'NONE',  ( 19.74724861314306068, 6.659670522263893666, -76.23824785690877093 ) ) ;
#45642 = ORIENTED_EDGE ( 'NONE', *, *, #30434, .T. ) ;
#45641 = CARTESIAN_POINT ( 'NONE',  ( -132.9227230387960788, 52.53474289881227577, 67.59429576175594434 ) ) ;
#45643 = CARTESIAN_POINT ( 'NONE',  ( -95.90733500870057071, 30.77270007533267560, 87.74079889594401038 ) ) ;
#45644 = CARTESIAN_POINT ( 'NONE',  ( 24.36509522349078338, -70.94296747916756374, 170.0000000000000000 ) ) ;
#45645 = FACE_BOUND ( 'NONE', #53654, .T. ) ;
#45646 = PRODUCT_RELATED_PRODUCT_CATEGORY ( 'part', '', ( #45109 ) ) ;
#45647 = ORIENTED_EDGE ( 'NONE', *, *, #10938, .T. ) ;
#45648 = DIRECTION ( 'NONE',  ( -0.2225209339563042066, -0.9749279121818259508, 0.000000000000000000 ) ) ;
#45649 = EDGE_CURVE ( 'NONE', #34130, #24352, #67243, .T. ) ;
#45650 = CIRCLE ( 'NONE', #1830, 25.12245591505646303 ) ;
#45651 = FACE_OUTER_BOUND ( 'NONE', #15509, .T. ) ;
#45652 = ADVANCED_FACE ( 'NONE', ( #53413 ), #26365, .F. ) ;
#45653 = CARTESIAN_POINT ( 'NONE',  ( 181.0840389613909451, 80.03940679743416808, -9.380507075415923879 ) ) ;
#45654 = CARTESIAN_POINT ( 'NONE',  ( -133.1566699306513328, 52.70203339370770124, 9.385161963150576270 ) ) ;
#45655 = CARTESIAN_POINT ( 'NONE',  ( 70.41705859591009187, 15.55317472777717569, -71.30260546593714821 ) ) ;
#45656 = ORIENTED_EDGE ( 'NONE', *, *, #46793, .F. ) ;
#45657 = ORIENTED_EDGE ( 'NONE', *, *, #68920, .F. ) ;
#45658 = CIRCLE ( 'NONE', #46808, 0.3000000000000051514 ) ;
#45659 = DIRECTION ( 'NONE',  ( -1.000000000000000000, 0.000000000000000000, 0.000000000000000000 ) ) ;
#45660 = DIRECTION ( 'NONE',  ( 0.000000000000000000, 0.000000000000000000, 1.000000000000000000 ) ) ;
#45661 = CIRCLE ( 'NONE', #16428, 74.99999999999998579 ) ;
#45662 = CARTESIAN_POINT ( 'NONE',  ( -48.19921232700619385, 12.95035395002356182, -93.32826121341297210 ) ) ;
#45663 = CARTESIAN_POINT ( 'NONE',  ( -56.44201257846585662, -32.26641783793645857, 170.0000000000000000 ) ) ;
#45664 = VECTOR ( 'NONE', #6186, 1000.000000000000000 ) ;
#45665 = CARTESIAN_POINT ( 'NONE',  ( -148.6426981422628728, 63.44891673852537650, 30.75816665846506481 ) ) ;
#45666 = CARTESIAN_POINT ( 'NONE',  ( -129.6165111262477296, 48.99406349865701316, 58.44935411866086383 ) ) ;
#45667 = CARTESIAN_POINT ( 'NONE',  ( -76.79042791651912125, 22.68960395613480330, -8.505398727429060557 ) ) ;
#45668 = EDGE_CURVE ( 'NONE', #19424, #27213, #10174, .T. ) ;
#45669 = ORIENTED_EDGE ( 'NONE', *, *, #62234, .F. ) ;
#45670 = CARTESIAN_POINT ( 'NONE',  ( -102.2801239173131194, 33.91021738430207932, 45.51907450641513009 ) ) ;
#45671 = ORIENTED_EDGE ( 'NONE', *, *, #64306, .T. ) ;
#45673 = AXIS2_PLACEMENT_3D ( 'NONE', #17094, #22740, #40222 ) ;
#45672 = CARTESIAN_POINT ( 'NONE',  ( 33.44527180510250020, 7.709232309484709944, 32.83041950400863840 ) ) ;
#45674 = CARTESIAN_POINT ( 'NONE',  ( 84.05289558242219528, 19.61733656419350424, 57.00898428369665538 ) ) ;
#45675 = EDGE_CURVE ( 'NONE', #11610, #69411, #15465, .T. ) ;
#45676 = ORIENTED_EDGE ( 'NONE', *, *, #20546, .T. ) ;
#45677 = LINE ( 'NONE', #1721, #14978 ) ;
#45678 = CARTESIAN_POINT ( 'NONE',  ( -449.7337897053572533, 365.0000000000064233, -143.5207719538776132 ) ) ;
#45679 = EDGE_CURVE ( 'NONE', #50613, #34211, #27380, .T. ) ;
#45680 = LINE ( 'NONE', #40392, #26628 ) ;
#45681 = CARTESIAN_POINT ( 'NONE',  ( -11.57950265606958062, 8.174070387114795722, -36.42061191550288157 ) ) ;
#45682 = CARTESIAN_POINT ( 'NONE',  ( 154.4429418375332830, 55.33424769452791736, -50.50089971109889575 ) ) ;
#45683 = EDGE_LOOP ( 'NONE', ( #21701, #67299, #32643 ) ) ;
#45684 = CARTESIAN_POINT ( 'NONE',  ( -108.6232015645744866, 36.12159103445661401, -92.19520623112163094 ) ) ;
#45685 = CARTESIAN_POINT ( 'NONE',  ( -156.8764584803562343, 70.69066846313523911, -16.89224324630464835 ) ) ;
#45686 = ORIENTED_EDGE ( 'NONE', *, *, #12645, .T. ) ;
#45687 = DIRECTION ( 'NONE',  ( 0.000000000000000000, 1.000000000000000000, -0.000000000000000000 ) ) ;
#45688 = CARTESIAN_POINT ( 'NONE',  ( -60.47589866267034608, 17.25153113855766307, 59.47546330872564369 ) ) ;
#45689 = DIRECTION ( 'NONE',  ( 0.9959742939952382912, 0.08963930890344089242, -0.000000000000000000 ) ) ;
#45690 = EDGE_LOOP ( 'NONE', ( #42758, #46484, #68234, #15113 ) ) ;
#45691 = DIRECTION ( 'NONE',  ( -0.7227948638273878901, -0.6910626489868685329, 2.500042656554810833E-16 ) ) ;
#45692 = CARTESIAN_POINT ( 'NONE',  ( 152.8373718734504507, 55.38925997611392660, -64.55073842685702346 ) ) ;
#45693 = CARTESIAN_POINT ( 'NONE',  ( -31.43908319763709969, 9.591432048623765638, 30.21645440618916112 ) ) ;
#45694 = CARTESIAN_POINT ( 'NONE',  ( 139.2921620648436942, 44.80435067172502528, -48.71413097721568874 ) ) ;
#45695 = ORIENTED_EDGE ( 'NONE', *, *, #9206, .F. ) ;
#45696 = DIRECTION ( 'NONE',  ( 9.989315170677463157E-15, -1.000000000000000000, -4.052314039881817428E-15 ) ) ;
#45697 = CARTESIAN_POINT ( 'NONE',  ( -152.9008427825210390, 68.45483453645053373, 58.37314777991063153 ) ) ;
#45698 = CARTESIAN_POINT ( 'NONE',  ( -120.4816138481825050, 43.03185659245511374, 32.90506872955344875 ) ) ;
#45699 = VERTEX_POINT ( 'NONE', #37943 ) ;
#45700 = LINE ( 'NONE', #62576, #59342 ) ;
#45701 = CARTESIAN_POINT ( 'NONE',  ( 127.7775657355649486, 39.02916686230897625, 86.25207957938988557 ) ) ;
#45702 = EDGE_CURVE ( 'NONE', #54393, #47483, #47805, .T. ) ;
#45703 = PRODUCT ( 'stator', 'stator', '', ( #47664 ) ) ;
#45704 = DIRECTION ( 'NONE',  ( -1.000000000000000000, 0.000000000000000000, 0.000000000000000000 ) ) ;
#45705 = DIRECTION ( 'NONE',  ( -0.000000000000000000, -0.000000000000000000, -1.000000000000000000 ) ) ;
#45706 = AXIS2_PLACEMENT_3D ( 'NONE', #58358, #53070, #10863 ) ;
#45707 = DIRECTION ( 'NONE',  ( 1.000000000000000000, 0.000000000000000000, 0.000000000000000000 ) ) ;
#45708 = VERTEX_POINT ( 'NONE', #54095 ) ;
#45709 = CARTESIAN_POINT ( 'NONE',  ( 164.8886903222556839, 63.65672212134877839, -17.91909660570943430 ) ) ;
#45710 = CARTESIAN_POINT ( 'NONE',  ( 151.3797687388446889, -65.65103187525450323, 0.000000000000000000 ) ) ;
#45711 = AXIS2_PLACEMENT_3D ( 'NONE', #31841, #20587, #15322 ) ;
#45712 = CARTESIAN_POINT ( 'NONE',  ( 68.93219921887765622, 14.12322281954860514, 59.54178852774079189 ) ) ;
#45713 = CARTESIAN_POINT ( 'NONE',  ( 141.3400002717723112, 47.33399859146520328, 10.73346743848780704 ) ) ;
#45714 = DIRECTION ( 'NONE',  ( 1.000000000000000000, 0.000000000000000000, 0.000000000000000000 ) ) ;
#45715 = AXIS2_PLACEMENT_3D ( 'NONE', #45877, #52531, #2976 ) ;
#45716 = ORIENTED_EDGE ( 'NONE', *, *, #15075, .T. ) ;
#45717 = AXIS2_PLACEMENT_3D ( 'NONE', #34532, #8126, #7083 ) ;
#45718 = CARTESIAN_POINT ( 'NONE',  ( 164.6561571795775194, 64.77723933022095082, -14.56007165210607646 ) ) ;
#45719 = EDGE_LOOP ( 'NONE', ( #68129, #22864, #54055, #59549, #20262, #38201, #46497, #17862, #45261, #40861, #13432, #1981, #58284, #38387, #24543 ) ) ;
#45720 = AXIS2_PLACEMENT_3D ( 'NONE', #68891, #53057, #47104 ) ;
#45721 = CARTESIAN_POINT ( 'NONE',  ( 68.62997155117719217, 15.08415013720828668, 69.15437636595807191 ) ) ;
#45722 = CARTESIAN_POINT ( 'NONE',  ( 134.5554110091750601, 41.84687667739064665, 83.20593790981784821 ) ) ;
#45723 = EDGE_LOOP ( 'NONE', ( #43697, #26634, #12442, #58985 ) ) ;
#45724 = CARTESIAN_POINT ( 'NONE',  ( 163.7403496014744633, 64.00600007368876732, -47.74785624616011148 ) ) ;
#45725 = FACE_BOUND ( 'NONE', #11507, .T. ) ;
#45726 = DIRECTION ( 'NONE',  ( 0.8090169943749422332, 0.5877852522924802425, -0.000000000000000000 ) ) ;
#45727 = CARTESIAN_POINT ( 'NONE',  ( 157.9130201331580849, 57.99550255803048771, -51.12418429913767426 ) ) ;
#45728 = ORIENTED_EDGE ( 'NONE', *, *, #67658, .F. ) ;
#45729 = CARTESIAN_POINT ( 'NONE',  ( -64.83840629396345889, -4.580509716060185532, 170.0000000000000000 ) ) ;
#45730 = ADVANCED_FACE ( 'NONE', ( #36919 ), #24330, .T. ) ;
#45731 = CARTESIAN_POINT ( 'NONE',  ( 67.36631071204163845, 14.76099193472943405, 84.85725114640790423 ) ) ;
#45732 = CARTESIAN_POINT ( 'NONE',  ( 0.000000000000000000, 0.000000000000000000, 43.58025477438756212 ) ) ;
#45733 = CARTESIAN_POINT ( 'NONE',  ( 79.52639011421921111, 18.17129627604990816, -14.01688966035989559 ) ) ;
#45734 = EDGE_CURVE ( 'NONE', #53508, #14782, #42297, .T. ) ;
#45735 = CARTESIAN_POINT ( 'NONE',  ( -166.7068579965637127, 80.26142964949322334, 34.42591652138479930 ) ) ;
#45736 = CARTESIAN_POINT ( 'NONE',  ( -145.2470175691743748, 60.64833472287889293, -89.82575223439511092 ) ) ;
#45737 = CARTESIAN_POINT ( 'NONE',  ( 129.1137093889808511, 38.63348691920620581, -76.18274731194584604 ) ) ;
#45738 = ORIENTED_EDGE ( 'NONE', *, *, #24400, .F. ) ;
#45739 = DIRECTION ( 'NONE',  ( -0.5508969814521065267, 0.8345732537212999791, 0.000000000000000000 ) ) ;
#45740 = CARTESIAN_POINT ( 'NONE',  ( -11.56945424397728495, 8.173256823723111353, 57.95689558190326096 ) ) ;
#45741 = ORIENTED_EDGE ( 'NONE', *, *, #13653, .F. ) ;
#45742 = ADVANCED_FACE ( 'NONE', ( #42860 ), #64330, .F. ) ;
#45743 = PLANE ( 'NONE',  #32852 ) ;
#45744 = DIRECTION ( 'NONE',  ( 0.000000000000000000, 0.000000000000000000, 1.000000000000000000 ) ) ;
#45745 = CARTESIAN_POINT ( 'NONE',  ( 209.9518228411288874, 190.0000000000000000, 31.43423095485942298 ) ) ;
#45746 = CARTESIAN_POINT ( 'NONE',  ( -0.5658006089934878302, 7.533733779014709420, 35.66903967604532255 ) ) ;
#45747 = VECTOR ( 'NONE', #22166, 1000.000000000000000 ) ;
#45748 = DIRECTION ( 'NONE',  ( -0.8118923937861950435, -0.5838071093367415143, 0.000000000000000000 ) ) ;
#45749 = CARTESIAN_POINT ( 'NONE',  ( -48.56549579811110817, 13.03742088415616429, -65.76502786008495605 ) ) ;
#45750 = CARTESIAN_POINT ( 'NONE',  ( -7.336630171688593549, 7.867399454768229106, -23.57352014148015584 ) ) ;
#45751 = CARTESIAN_POINT ( 'NONE',  ( 175.5406524085946103, 73.17873692326776336, 4.886636635488581071 ) ) ;
#45752 = CARTESIAN_POINT ( 'NONE',  ( -59.95707852844800811, 16.05120821151901822, 5.276972445045120530 ) ) ;
#45753 = ORIENTED_EDGE ( 'NONE', *, *, #67944, .T. ) ;
#45754 = VECTOR ( 'NONE', #16074, 1000.000000000000000 ) ;
#45755 = CARTESIAN_POINT ( 'NONE',  ( -97.86516199987804043, 31.71158167298306907, -48.59635491045797551 ) ) ;
#45756 = ORIENTED_EDGE ( 'NONE', *, *, #27435, .F. ) ;
#45757 = CARTESIAN_POINT ( 'NONE',  ( 103.0026233023292974, 25.67408295205787283, -72.29030188102200327 ) ) ;
#45759 = EDGE_CURVE ( 'NONE', #58934, #42033, #59044, .T. ) ;
#45758 = APPLICATION_CONTEXT ( 'automotive_design' ) ;
#45760 = CARTESIAN_POINT ( 'NONE',  ( -56.44201257846585662, -32.26641783793645857, 170.0000000000000000 ) ) ;
#45761 = CIRCLE ( 'NONE', #64881, 54.03875030502680943 ) ;
#45762 = EDGE_CURVE ( 'NONE', #25024, #61751, #26566, .T. ) ;
#45763 = CARTESIAN_POINT ( 'NONE',  ( 63.01563776193091826, 12.67277567978500308, 2.968410348757589023 ) ) ;
#45764 = CARTESIAN_POINT ( 'NONE',  ( 5.354491962338135735, -6.146186931204420389, -9.431901280394560771 ) ) ;
#45765 = CARTESIAN_POINT ( 'NONE',  ( 450.2085304802404266, 190.0000000000000000, -250.0000000000000000 ) ) ;
#45766 = CIRCLE ( 'NONE', #6440, 242.4895526022646379 ) ;
#45767 = DIRECTION ( 'NONE',  ( -0.000000000000000000, -0.000000000000000000, 1.000000000000000000 ) ) ;
#45769 = VECTOR ( 'NONE', #22529, 1000.000000000000000 ) ;
#45768 = CARTESIAN_POINT ( 'NONE',  ( -24.53636015449789554, 60.58612729876395520, 43.58025477438756212 ) ) ;
#45770 = CARTESIAN_POINT ( 'NONE',  ( -173.1211646369891071, 87.12891641440857882, 57.66624519710472185 ) ) ;
#45771 = ORIENTED_EDGE ( 'NONE', *, *, #39313, .T. ) ;
#45772 = ORIENTED_EDGE ( 'NONE', *, *, #50653, .F. ) ;
#45773 = CARTESIAN_POINT ( 'NONE',  ( 442.3372781065089612, 370.0000000000065938, -141.4497041420121661 ) ) ;
#45774 = DIRECTION ( 'NONE',  ( -1.000000000000000000, -0.000000000000000000, -0.000000000000000000 ) ) ;
#45775 = CARTESIAN_POINT ( 'NONE',  ( 175.8963338753314360, 73.51705463274396379, -11.45839974079307666 ) ) ;
#45776 = CARTESIAN_POINT ( 'NONE',  ( -172.3127615181935539, 87.73358064377640630, 57.69864198530328991 ) ) ;
#45777 = LINE ( 'NONE', #40837, #63342 ) ;
#45778 = CARTESIAN_POINT ( 'NONE',  ( 57.41085175769454452, 12.46982565415947519, -21.36584457835558126 ) ) ;
#45779 = VERTEX_POINT ( 'NONE', #16489 ) ;
#45780 = CARTESIAN_POINT ( 'NONE',  ( -30.00000000000000355, 26.99999999999999289, 15.00000000000000000 ) ) ;
#45781 = CARTESIAN_POINT ( 'NONE',  ( 19.54452863209719382, 7.657034792877148277, -36.50889906614686709 ) ) ;
#45782 = CARTESIAN_POINT ( 'NONE',  ( 8.537735592981553268, 7.383000420390735563, 66.29318622724315446 ) ) ;
#45783 = CARTESIAN_POINT ( 'NONE',  ( 0.000000000000000000, 0.000000000000000000, 380.0000000000000000 ) ) ;
#45784 = FACE_BOUND ( 'NONE', #1402, .T. ) ;
#45785 = VERTEX_POINT ( 'NONE', #59393 ) ;
#45786 = ORIENTED_EDGE ( 'NONE', *, *, #68458, .F. ) ;
#45787 = CARTESIAN_POINT ( 'NONE',  ( -7.486743542470036594, 64.58150799671129505, 3.061616997868437868E-16 ) ) ;
#45788 = CARTESIAN_POINT ( 'NONE',  ( 0.000000000000000000, 0.000000000000000000, 41.38025477438755928 ) ) ;
#45789 = B_SPLINE_CURVE_WITH_KNOTS ( 'NONE', 3,
 ( #39975, #29423, #45597, #8672, #67082, #7280 ),
 .UNSPECIFIED., .F., .F.,
 ( 4, 2, 4 ),
 ( 0.03218932424835717343, 0.06469830966704906428, 0.09720729508574096900 ),
 .UNSPECIFIED. ) ;
#45790 = CARTESIAN_POINT ( 'NONE',  ( 37.70910994512003356, 9.209110272746707793, -77.27493779074411862 ) ) ;
#45791 = CARTESIAN_POINT ( 'NONE',  ( -178.2448732545370547, 94.58403736950704399, 16.97374245720416752 ) ) ;
#45792 = CARTESIAN_POINT ( 'NONE',  ( 8.619049365873218349, 6.376996852107025937, 88.97686130232474966 ) ) ;
#45793 = DIRECTION ( 'NONE',  ( 0.000000000000000000, -1.000000000000000000, 0.000000000000000000 ) ) ;
#45794 = CIRCLE ( 'NONE', #15466, 74.95140232871122521 ) ;
#45795 = ORIENTED_EDGE ( 'NONE', *, *, #3578, .T. ) ;
#45796 = DIRECTION ( 'NONE',  ( -0.000000000000000000, 1.000000000000000000, -0.000000000000000000 ) ) ;
#45797 = CARTESIAN_POINT ( 'NONE',  ( 197.2199569260503722, 98.22436319491366419, -43.16215066073257844 ) ) ;
#45798 = ORIENTED_EDGE ( 'NONE', *, *, #29372, .F. ) ;
#45800 = DIRECTION ( 'NONE',  ( -0.000000000000000000, 1.000000000000000000, -0.000000000000000000 ) ) ;
#45799 = CIRCLE ( 'NONE', #64876, 8.000000000000000000 ) ;
#45801 = EDGE_LOOP ( 'NONE', ( #68335, #36979, #35937, #3553 ) ) ;
#45802 = CARTESIAN_POINT ( 'NONE',  ( -84.55373779407977963, 24.65190748253136377, -74.13279789683143406 ) ) ;
#45803 = DIRECTION ( 'NONE',  ( 1.000000000000000000, -1.604841615724182364E-15, -4.270088556250601699E-16 ) ) ;
#45804 = CARTESIAN_POINT ( 'NONE',  ( 87.10672734544988316, 20.64813880796638301, -77.66611478937542756 ) ) ;
#45805 = EDGE_LOOP ( 'NONE', ( #27728, #7225, #11693 ) ) ;
#45806 = VECTOR ( 'NONE', #12837, 1000.000000000000000 ) ;
#45807 = ORIENTED_EDGE ( 'NONE', *, *, #17533, .T. ) ;
#45808 = CARTESIAN_POINT ( 'NONE',  ( 43.35536254672140899, 9.973606330917817786, 57.88029466200895001 ) ) ;
#45809 = CARTESIAN_POINT ( 'NONE',  ( -103.9557308419433639, 34.77357682180773679, -88.88104893678155349 ) ) ;
#45810 = CARTESIAN_POINT ( 'NONE',  ( 23.24028701062093205, 6.853614888934259852, 11.64810109089808066 ) ) ;
#45811 = VERTEX_POINT ( 'NONE', #662 ) ;
#45812 = EDGE_CURVE ( 'NONE', #30796, #32425, #22112, .T. ) ;
#45813 = AXIS2_PLACEMENT_3D ( 'NONE', #35271, #8546, #20127 ) ;
#45814 = CARTESIAN_POINT ( 'NONE',  ( 64.16679220703368003, 10.37413986118183828, 170.0000000000000000 ) ) ;
#45815 = CARTESIAN_POINT ( 'NONE',  ( 6.400000000000000355, 4.618802153517001408, -8.000000000000000000 ) ) ;
#45816 = CARTESIAN_POINT ( 'NONE',  ( 117.6865880453676141, 32.48051379280605744, -17.63313866224432758 ) ) ;
#45817 = CARTESIAN_POINT ( 'NONE',  ( 81.04027388895735839, 18.64386073872848826, -38.29630275601382294 ) ) ;
#45819 = VERTEX_POINT ( 'NONE', #11539 ) ;
#45818 = CARTESIAN_POINT ( 'NONE',  ( -168.2905794219380198, 83.36949033555949029, -90.14733823562677628 ) ) ;
#45820 = EDGE_LOOP ( 'NONE', ( #13855, #24925, #57925, #64 ) ) ;
#45821 = EDGE_CURVE ( 'NONE', #7307, #46840, #1011, .T. ) ;
#45822 = ORIENTED_EDGE ( 'NONE', *, *, #11286, .T. ) ;
#45823 = CARTESIAN_POINT ( 'NONE',  ( 45.04360969585142271, 9.210232288266691825, 15.53527602477098135 ) ) ;
#45824 = CARTESIAN_POINT ( 'NONE',  ( -11.76013739941318548, -57.14197750166816547, 27.58472369372398347 ) ) ;
#45825 = CARTESIAN_POINT ( 'NONE',  ( -51.35181696773306470, 13.72007042346227124, -22.41355051264525500 ) ) ;
#45826 = CARTESIAN_POINT ( 'NONE',  ( 410.0000000000000000, 0.000000000000000000, 380.0000000000000000 ) ) ;
#45827 = CARTESIAN_POINT ( 'NONE',  ( 199.7278513351970730, 99.76879341361765796, 15.49925635273226376 ) ) ;
#45828 = CARTESIAN_POINT ( 'NONE',  ( -25.25491181982865285, 8.657665838245407031, -92.24093140373469168 ) ) ;
#45829 = CARTESIAN_POINT ( 'NONE',  ( 207.0530270305075078, 111.3805688245614363, 83.25676956866661271 ) ) ;
#45830 = LINE ( 'NONE', #4309, #34392 ) ;
#45831 = CARTESIAN_POINT ( 'NONE',  ( -75.64857587248464199, 21.19501514561450506, -62.58980599074443063 ) ) ;
#45832 = CARTESIAN_POINT ( 'NONE',  ( -15.32550079334879278, 7.496023944924843363, 37.37366452483693990 ) ) ;
#45833 = ORIENTED_EDGE ( 'NONE', *, *, #38766, .T. ) ;
#45834 = DIRECTION ( 'NONE',  ( 1.000000000000000000, 0.000000000000000000, -7.703719777548943412E-34 ) ) ;
#45835 = ORIENTED_EDGE ( 'NONE', *, *, #45908, .T. ) ;
#45836 = CARTESIAN_POINT ( 'NONE',  ( 197.6145711261844724, 97.10888456119684520, -19.52788035905484776 ) ) ;
#45837 = ORIENTED_EDGE ( 'NONE', *, *, #60667, .F. ) ;
#45838 = EDGE_CURVE ( 'NONE', #22362, #56285, #32195, .T. ) ;
#45839 = FACE_OUTER_BOUND ( 'NONE', #48360, .T. ) ;
#45840 = CARTESIAN_POINT ( 'NONE',  ( 185.1710994180822638, 84.30654632312744923, -64.26513029063508498 ) ) ;
#45841 = CARTESIAN_POINT ( 'NONE',  ( -165.6208371326873703, 80.58821715390999429, 38.02385811616766631 ) ) ;
#45842 = LINE ( 'NONE', #7870, #9364 ) ;
#45843 = DIRECTION ( 'NONE',  ( 0.8584487936018728726, -0.5128992774058949156, 0.000000000000000000 ) ) ;
#45844 = DIRECTION ( 'NONE',  ( 0.5128992774059071280, -0.8584487936018655452, 0.000000000000000000 ) ) ;
#45845 = CARTESIAN_POINT ( 'NONE',  ( 8.683910719548894264, 7.383368463746302623, -45.43529509856040249 ) ) ;
#45846 = CARTESIAN_POINT ( 'NONE',  ( 130.7260704202054455, 39.56565398554878499, -50.35476434615378594 ) ) ;
#45847 = VERTEX_POINT ( 'NONE', #2065 ) ;
#45849 = EDGE_LOOP ( 'NONE', ( #28061, #7395, #19225, #9932 ) ) ;
#45848 = ADVANCED_BREP_SHAPE_REPRESENTATION ( '', ( #17567, #66832 ), #621 ) ;
#45850 = CARTESIAN_POINT ( 'NONE',  ( 188.0498085889633728, 87.44272287964741963, 93.28420891864679731 ) ) ;
#45851 = CARTESIAN_POINT ( 'NONE',  ( 0.4964154566687906112, 4.996589667937374912, 7.345652830558760726 ) ) ;
#45852 = FACE_OUTER_BOUND ( 'NONE', #8838, .T. ) ;
#45853 = DIRECTION ( 'NONE',  ( 0.000000000000000000, 0.000000000000000000, 1.000000000000000000 ) ) ;
#45854 = B_SPLINE_CURVE_WITH_KNOTS ( 'NONE', 3,
 ( #18140, #13558, #8285, #34681, #50147, #7597, #39595, #2316, #1607, #45558, #50494, #44869, #39253, #29053, #1972, #62078, #40622, #7239, #66353, #39937, #13897, #7932, #18485, #61394, #61046, #35360, #56820, #56116, #67041, #65997, #8636, #34329, #12871, #55777, #24468, #35012, #60697, #49781, #23069, #2657, #12513, #23766, #33973, #50839 ),
 .UNSPECIFIED., .F., .F.,
 ( 4, 2, 2, 2, 2, 2, 2, 2, 2, 2, 2, 2, 2, 2, 2, 2, 2, 2, 2, 2, 2, 4 ),
 ( 0.02416815208377490892, 0.02567033257376875877, 0.02642142281876568716, 0.02717251306376261208, 0.02867469355375646192, 0.02942578379875337297, 0.03017687404375027707, 0.03167905453374409569, 0.03318123502373791778, 0.03393232526873483229, 0.03468341551373174680, 0.03618559600372561053, 0.03693668624872255279, 0.03768777649371949506, 0.03918995698371335878, 0.04069213747370722944, 0.04219431796370108623, 0.04369649845369495689, 0.04444758869869189222, 0.04519867894368882755, 0.04670085943368268433, 0.04820303992367654111 ),
 .UNSPECIFIED. ) ;
#45855 = AXIS2_PLACEMENT_3D ( 'NONE', #27426, #14555, #21459 ) ;
#45856 = UNCERTAINTY_MEASURE_WITH_UNIT (LENGTH_MEASURE( 1.000000000000000082E-05 ), #67079, 'distance_accuracy_value', 'NONE');
#45857 = CARTESIAN_POINT ( 'NONE',  ( 10.83418588031599228, 6.392467435475930770, 5.017533756073925488 ) ) ;
#45858 = ORIENTED_EDGE ( 'NONE', *, *, #66289, .F. ) ;
#45859 = CIRCLE ( 'NONE', #16619, 10.00000000000000178 ) ;
#45860 = DIRECTION ( 'NONE',  ( 0.000000000000000000, -3.697785493223491743E-32, 1.000000000000000000 ) ) ;
#45861 = DIRECTION ( 'NONE',  ( -1.387778780781445922E-16, 1.000000000000000000, 1.232595164407830946E-32 ) ) ;
#45862 = CARTESIAN_POINT ( 'NONE',  ( 200.4590013143046292, 102.3556155835302945, -76.87509902206629420 ) ) ;
#45863 = CARTESIAN_POINT ( 'NONE',  ( -178.7458319892713519, 93.61502008198021940, -37.24441981830012338 ) ) ;
#45864 = CARTESIAN_POINT ( 'NONE',  ( 8.171862737214143024, -51.01496555961261237, 26.66469066592268078 ) ) ;
#45865 = CARTESIAN_POINT ( 'NONE',  ( -23.95089599695169014, 9.496585844566174828, 64.07248978537857909 ) ) ;
#45866 = CARTESIAN_POINT ( 'NONE',  ( 106.6934359423128598, 21.67676124233545565, 3.764605836381888615 ) ) ;
#45867 = CARTESIAN_POINT ( 'NONE',  ( -49.11825192196928214, 13.17012322555986970, 69.27432531549762018 ) ) ;
#45868 = AXIS2_PLACEMENT_3D ( 'NONE', #38205, #60709, #54369 ) ;
#45869 = CARTESIAN_POINT ( 'NONE',  ( -5.885876544836654567, 6.772369038004114827, 57.21109972859309778 ) ) ;
#45870 = VERTEX_POINT ( 'NONE', #6981 ) ;
#45871 = LINE ( 'NONE', #62040, #9165 ) ;
#45872 = CARTESIAN_POINT ( 'NONE',  ( -128.7810612886105446, 48.42424427998344783, -76.18402560349873909 ) ) ;
#45873 = CARTESIAN_POINT ( 'NONE',  ( -15.55634918610396866, 31.11269837220809009, 85.00100000000000477 ) ) ;
#45874 = CARTESIAN_POINT ( 'NONE',  ( -53.13004807512037786, 14.17398740785106526, -35.45065378176567350 ) ) ;
#45875 = B_SPLINE_CURVE_WITH_KNOTS ( 'NONE', 3,
 ( #5687, #16596, #48931, #21524, #38052, #44014, #27147, #5357, #66, #32781, #10972, #11309, #65142, #33135, #419, #16249, #38760, #42969, #1466, #21870, #43315, #64792, #33493, #16936, #59497, #28188, #60202, #773, #43663, #38400, #59841, #54209, #11662, #6033, #22225, #54569, #54916, #39118, #6396, #6740, #48578, #32438, #64440, #65491, #27848 ),
 .UNSPECIFIED., .F., .F.,
 ( 4, 2, 2, 2, 2, 2, 2, 2, 2, 2, 2, 2, 2, 1, 2, 2, 2, 2, 2, 2, 2, 2, 4 ),
 ( 0.02356759485890611364, 0.02503765354686409914, 0.02577268289084310229, 0.02650771223482210198, 0.02797777092278013258, 0.02944782961073816319, 0.03018285895471718369, 0.03091788829869620420, 0.03238794698665421745, 0.03312297633063322755, 0.03385800567461224458, 0.03532806436257030641, 0.03606309370654933733, 0.03679812305052836824, 0.03753315239450739915, 0.03826818173848643700, 0.03973824042644454047, 0.04120829911440264393, 0.04267835780236074045, 0.04341338714633979912, 0.04414841649031885779, 0.04561847517827697512, 0.04708853386623509246 ),
 .UNSPECIFIED. ) ;
#45876 = DIRECTION ( 'NONE',  ( 0.000000000000000000, 0.000000000000000000, -1.000000000000000000 ) ) ;
#45877 = CARTESIAN_POINT ( 'NONE',  ( 99.71998884745383407, 0.000000000000000000, 7.478223336038896996 ) ) ;
#45878 = EDGE_CURVE ( 'NONE', #3054, #42365, #13529, .T. ) ;
#45879 = VERTEX_POINT ( 'NONE', #44256 ) ;
#45880 = CARTESIAN_POINT ( 'NONE',  ( -189.3836756007636950, 107.2890649608328459, -94.27226266387080500 ) ) ;
#45881 = CARTESIAN_POINT ( 'NONE',  ( -4.680456609903986376, -6.535341423375604641, -0.01688885742777731375 ) ) ;
#45882 = ORIENTED_EDGE ( 'NONE', *, *, #51556, .T. ) ;
#45883 = EDGE_CURVE ( 'NONE', #7537, #42749, #28433, .T. ) ;
#45884 = EDGE_LOOP ( 'NONE', ( #40965, #7864, #8951, #29122 ) ) ;
#45885 = DIRECTION ( 'NONE',  ( -0.000000000000000000, -0.000000000000000000, 1.000000000000000000 ) ) ;
#45886 = CARTESIAN_POINT ( 'NONE',  ( 155.7167524447090443, 57.56687707799948583, 44.21502333676962593 ) ) ;
#45887 = LINE ( 'NONE', #30398, #50475 ) ;
#45888 = ORIENTED_EDGE ( 'NONE', *, *, #46938, .F. ) ;
#45889 = DIRECTION ( 'NONE',  ( 0.04486483035051862939, -0.9989930665413143673, 0.000000000000000000 ) ) ;
#45890 = CARTESIAN_POINT ( 'NONE',  ( -180.6011569556095537, 95.85968111394264213, 10.84709140346148715 ) ) ;
#45891 = CARTESIAN_POINT ( 'NONE',  ( -2.355184675731022192, 6.596450510445357907, 5.634252349864039999 ) ) ;
#45892 = CARTESIAN_POINT ( 'NONE',  ( 57.07246224906423748, 12.39953617563784682, -38.61949813100464013 ) ) ;
#45893 = CARTESIAN_POINT ( 'NONE',  ( -60.41792053122248518, -24.01035990323518021, 43.58025477438756923 ) ) ;
#45894 = CARTESIAN_POINT ( 'NONE',  ( 157.2737841094199780, 57.49822297871171628, 83.09519871651045264 ) ) ;
#45895 = CARTESIAN_POINT ( 'NONE',  ( 136.9934874058118339, 43.35050367224294376, 16.99398237304345827 ) ) ;
#45896 = EDGE_CURVE ( 'NONE', #59205, #30284, #51278, .T. ) ;
#45897 = ORIENTED_EDGE ( 'NONE', *, *, #16102, .F. ) ;
#45898 = ADVANCED_FACE ( 'NONE', ( #38288 ), #24214, .F. ) ;
#45899 = AXIS2_PLACEMENT_3D ( 'NONE', #32112, #437, #60228 ) ;
#45900 = DIRECTION ( 'NONE',  ( -0.000000000000000000, -1.000000000000000000, -0.000000000000000000 ) ) ;
#45901 = CARTESIAN_POINT ( 'NONE',  ( -76.79042791651912125, 22.68960395613480330, 18.33915186303461553 ) ) ;
#45902 = CARTESIAN_POINT ( 'NONE',  ( 23.05216796272336666, 9.986758404124199018, 3.061616997868437868E-16 ) ) ;
#45903 = AXIS2_PLACEMENT_3D ( 'NONE', #54060, #22079, #6943 ) ;
#45904 = CARTESIAN_POINT ( 'NONE',  ( -190.6985136298601731, 109.1272424661242582, -95.00000000000133582 ) ) ;
#45906 = ORIENTED_EDGE ( 'NONE', *, *, #498, .T. ) ;
#45905 = CARTESIAN_POINT ( 'NONE',  ( -22.50000000000003197, 207.5000000000000284, 378.0000000000000000 ) ) ;
#45907 = CARTESIAN_POINT ( 'NONE',  ( 81.74909803672913711, 17.81295302817862947, -49.03814682348451726 ) ) ;
#45908 = EDGE_CURVE ( 'NONE', #42155, #64838, #61495, .T. ) ;
#45909 = ORIENTED_EDGE ( 'NONE', *, *, #24838, .F. ) ;
#45910 = CARTESIAN_POINT ( 'NONE',  ( -149.5074843970971017, 64.17983161892347255, 72.56537183036277838 ) ) ;
#45911 = CARTESIAN_POINT ( 'NONE',  ( 157.4703587214989398, -170.0000000000000000, 2.564916881789689462 ) ) ;
#45912 = DIRECTION ( 'NONE',  ( 0.000000000000000000, 0.000000000000000000, 1.000000000000000000 ) ) ;
#45913 = DIRECTION ( 'NONE',  ( 1.387778780781445429E-16, -1.000000000000000000, -3.081487911019577365E-33 ) ) ;
#45914 = LINE ( 'NONE', #56825, #55656 ) ;
#45915 = CARTESIAN_POINT ( 'NONE',  ( -80.31482177285911916, 24.03632224640838544, -23.09139861995610232 ) ) ;
#45916 = CARTESIAN_POINT ( 'NONE',  ( -173.1211646369891355, 88.63826465341151106, -22.86740657428632773 ) ) ;
#45917 = CARTESIAN_POINT ( 'NONE',  ( -52.00092620775817664, 14.92276858858357258, 30.96201563046714256 ) ) ;
#45918 = VERTEX_POINT ( 'NONE', #56914 ) ;
#45919 = EDGE_LOOP ( 'NONE', ( #13267, #17540, #2502, #51118 ) ) ;
#45920 = EDGE_CURVE ( 'NONE', #19652, #42528, #1879, .T. ) ;
#45921 = CARTESIAN_POINT ( 'NONE',  ( -109.7811201291769692, 37.90784085457602970, 11.40485209265354172 ) ) ;
#45922 = CARTESIAN_POINT ( 'NONE',  ( 103.8317086684999850, 26.02720265156212776, 67.85564866584407184 ) ) ;
#45923 = CARTESIAN_POINT ( 'NONE',  ( 164.0158927577712973, 62.92463143894071465, 60.05433321578705375 ) ) ;
#45925 = ADVANCED_FACE ( 'NONE', ( #3104 ), #40379, .F. ) ;
#45924 = CARTESIAN_POINT ( 'NONE',  ( -190.4966031023458584, 108.8421921967458985, 69.44444822291313812 ) ) ;
#45926 = EDGE_CURVE ( 'NONE', #8631, #17554, #18633, .T. ) ;
#45927 = CARTESIAN_POINT ( 'NONE',  ( 187.5272808203428383, 85.37192123373907293, -47.60191362853060326 ) ) ;
#45928 = FACE_OUTER_BOUND ( 'NONE', #57703, .T. ) ;
#45929 = CARTESIAN_POINT ( 'NONE',  ( -142.1220711180391731, 59.43943186025860825, 90.55661759554712376 ) ) ;
#45930 = ORIENTED_EDGE ( 'NONE', *, *, #60873, .T. ) ;
#45931 = ORIENTED_EDGE ( 'NONE', *, *, #59368, .T. ) ;
#45932 = VERTEX_POINT ( 'NONE', #24566 ) ;
#45933 = CARTESIAN_POINT ( 'NONE',  ( -7.825402957745087207, -170.0000000000000000, 64.46013162991090439 ) ) ;
#45934 = CARTESIAN_POINT ( 'NONE',  ( 181.0840389613909736, 78.60582251573003987, -89.91415884680696990 ) ) ;
#45935 = CARTESIAN_POINT ( 'NONE',  ( 68.93219921887762780, 14.12322281954860337, -47.83641383411398351 ) ) ;
#45936 = LINE ( 'NONE', #67401, #35569 ) ;
#45937 = CARTESIAN_POINT ( 'NONE',  ( 8.000000000000007105, 249.8719672152120381, 94.99999999999866418 ) ) ;
#45938 = CARTESIAN_POINT ( 'NONE',  ( -94.83794676023107684, 30.26879337035744300, -14.60722893403272415 ) ) ;
#45939 = CARTESIAN_POINT ( 'NONE',  ( 55.99998955208976525, 12.18058389017405041, 39.97614766549666143 ) ) ;
#45940 = CARTESIAN_POINT ( 'NONE',  ( 32.64625186056120043, 7.626510506539066370, 94.42831398130083187 ) ) ;
#45941 = ORIENTED_EDGE ( 'NONE', *, *, #18110, .F. ) ;
#45942 = CARTESIAN_POINT ( 'NONE',  ( -0.5183605925911975998, 6.525266619725955231, -44.62597692609903532 ) ) ;
#45943 = LINE ( 'NONE', #56151, #8204 ) ;
#45944 = CARTESIAN_POINT ( 'NONE',  ( -121.5921196778231348, 43.72569502503144179, 5.113650806495113166 ) ) ;
#45945 = DIRECTION ( 'NONE',  ( 0.000000000000000000, 0.000000000000000000, 1.000000000000000000 ) ) ;
#45946 = LINE ( 'NONE', #19560, #33062 ) ;
#45947 = CARTESIAN_POINT ( 'NONE',  ( 19.10949903373831305, 7.636938177523838078, -22.90343416015605271 ) ) ;
#45948 = LINE ( 'NONE', #7283, #54674 ) ;
#45949 = VECTOR ( 'NONE', #23414, 1000.000000000000000 ) ;
#45950 = CIRCLE ( 'NONE', #27967, 10.00000000000000000 ) ;
#45951 = ORIENTED_EDGE ( 'NONE', *, *, #56209, .T. ) ;
#45952 = DIRECTION ( 'NONE',  ( -0.9108602745606090290, -0.4127148655274874289, 6.801596970299575131E-15 ) ) ;
#45953 = DIRECTION ( 'NONE',  ( -1.000000000000000000, 0.000000000000000000, 0.000000000000000000 ) ) ;
#45954 = CARTESIAN_POINT ( 'NONE',  ( -128.1384526288950099, 47.98891607499718504, 4.104498430499266881 ) ) ;
#45955 = CARTESIAN_POINT ( 'NONE',  ( 266.9165763529819628, -52.00000000000000711, 108.9999999999999858 ) ) ;
#45956 = VECTOR ( 'NONE', #21131, 1000.000000000000114 ) ;
#45957 = CONTEXT_DEPENDENT_SHAPE_REPRESENTATION ( #15749, #6851 ) ;
#45958 = CARTESIAN_POINT ( 'NONE',  ( 0.000000000000000000, 0.000000000000000000, -5.000000000000000000 ) ) ;
#45959 = EDGE_LOOP ( 'NONE', ( #1903, #23848, #7649, #59670, #27474 ) ) ;
#45960 = CARTESIAN_POINT ( 'NONE',  ( 133.8566784816069060, 42.60093787723653236, 2.665790248531674678 ) ) ;
#45961 = ADVANCED_FACE ( 'NONE', ( #2752 ), #18929, .F. ) ;
#45962 = ORIENTED_EDGE ( 'NONE', *, *, #30054, .F. ) ;
#45963 = DIRECTION ( 'NONE',  ( 1.000000000000000000, 0.000000000000000000, 0.000000000000000000 ) ) ;
#45964 = CARTESIAN_POINT ( 'NONE',  ( 203.1423857108908351, 105.9238244286949708, 2.515585502045935673 ) ) ;
#45965 = ORIENTED_EDGE ( 'NONE', *, *, #21999, .T. ) ;
#45966 = EDGE_CURVE ( 'NONE', #11222, #327, #36145, .T. ) ;
#45967 = CARTESIAN_POINT ( 'NONE',  ( 154.6089187792045436, 56.72139871926570009, 83.65894979668894393 ) ) ;
#45968 = EDGE_LOOP ( 'NONE', ( #7450, #47033, #63469, #51852 ) ) ;
#45969 = CARTESIAN_POINT ( 'NONE',  ( 130.7457207912711112, 40.74300766298684096, -77.20782277390614468 ) ) ;
#45970 = LINE ( 'NONE', #57222, #67668 ) ;
#45971 = CARTESIAN_POINT ( 'NONE',  ( -156.6644740249450365, 71.86407434531899696, 35.96180702756684866 ) ) ;
#45972 = CARTESIAN_POINT ( 'NONE',  ( 0.000000000000000000, 0.000000000000000000, 43.58025477438756212 ) ) ;
#45973 = CARTESIAN_POINT ( 'NONE',  ( 0.000000000000000000, 0.000000000000000000, 5.000000000000000000 ) ) ;
#45975 = EDGE_LOOP ( 'NONE', ( #33654, #39060, #16472, #17758 ) ) ;
#45974 = DIRECTION ( 'NONE',  ( -0.4338837391175656699, 0.9009688679024155933, 0.000000000000000000 ) ) ;
#45976 = ADVANCED_FACE ( 'NONE', ( #35803 ), #35100, .F. ) ;
#45977 = CARTESIAN_POINT ( 'NONE',  ( 56.53776994993147298, 11.26292242501182628, 41.10093067265479050 ) ) ;
#45978 = EDGE_LOOP ( 'NONE', ( #5558, #10314 ) ) ;
#45980 = EDGE_LOOP ( 'NONE', ( #11851, #11817, #10139 ) ) ;
#45979 = EDGE_CURVE ( 'NONE', #67324, #63280, #46689, .T. ) ;
#45981 = CARTESIAN_POINT ( 'NONE',  ( -165.7149569557575717, 80.68479365246975021, 12.69795252626694726 ) ) ;
#45982 = CARTESIAN_POINT ( 'NONE',  ( 22.53041628628730209, 6.810083298012988173, -66.54146030137279411 ) ) ;
#45983 = EDGE_CURVE ( 'NONE', #27607, #60636, #57603, .T. ) ;
#45985 = ORIENTED_EDGE ( 'NONE', *, *, #15651, .F. ) ;
#45984 = CARTESIAN_POINT ( 'NONE',  ( -133.3220917939970036, 52.82057604964899156, 66.03414425393503961 ) ) ;
#45986 = CARTESIAN_POINT ( 'NONE',  ( -95.74211766252655309, 30.69445205485278905, 88.01871795480677463 ) ) ;
#45987 = CARTESIAN_POINT ( 'NONE',  ( -78.19438069111008360, 23.21811806230640585, -50.11545063171791270 ) ) ;
#45988 = ORIENTED_EDGE ( 'NONE', *, *, #59678, .T. ) ;
#45989 = CARTESIAN_POINT ( 'NONE',  ( 179.7110760798946103, 78.65068260568622804, -90.03270647271450855 ) ) ;
#45990 = CARTESIAN_POINT ( 'NONE',  ( 140.0820590176526252, 46.51134312115248548, 32.82017767266312802 ) ) ;
#45991 = DIRECTION ( 'NONE',  ( 0.000000000000000000, 1.000000000000000000, -0.000000000000000000 ) ) ;
#45992 = CARTESIAN_POINT ( 'NONE',  ( -131.3096895243911320, 51.39228038925229924, 16.48646959509930454 ) ) ;
#45993 = CARTESIAN_POINT ( 'NONE',  ( 63.99027454648602031, 13.93445177372599275, -77.51741006307621262 ) ) ;
#45994 = ORIENTED_EDGE ( 'NONE', *, *, #24778, .F. ) ;
#45995 = ORIENTED_EDGE ( 'NONE', *, *, #11262, .F. ) ;
#45996 = CARTESIAN_POINT ( 'NONE',  ( -148.6471085600700235, 64.76880961642447687, -22.93139458300547062 ) ) ;
#45998 = EDGE_CURVE ( 'NONE', #62436, #10617, #47027, .T. ) ;
#45997 = CARTESIAN_POINT ( 'NONE',  ( 104.0290905220488469, 27.20720373712009987, 94.99999999999866418 ) ) ;
#45999 = EDGE_CURVE ( 'NONE', #16122, #62233, #52314, .T. ) ;
#46000 = VECTOR ( 'NONE', #58238, 1000.000000000000000 ) ;
#46001 = DIRECTION ( 'NONE',  ( -0.000000000000000000, 1.000000000000000000, -0.000000000000000000 ) ) ;
#46002 = CARTESIAN_POINT ( 'NONE',  ( -52.14348496666676169, 14.95896524672374106, -89.47939421337314059 ) ) ;
#46003 = DIRECTION ( 'NONE',  ( 0.000000000000000000, 0.000000000000000000, 1.000000000000000000 ) ) ;
#46004 = EDGE_CURVE ( 'NONE', #22806, #9149, #4811, .T. ) ;
#46005 = CARTESIAN_POINT ( 'NONE',  ( 70.26639875985992489, 15.51307715494295891, -41.23871606255404032 ) ) ;
#46006 = CARTESIAN_POINT ( 'NONE',  ( -122.3994536713185681, 45.42826354555018042, 44.76030098624846687 ) ) ;
#46007 = CARTESIAN_POINT ( 'NONE',  ( 206.6955592216989714, 109.1214665502617578, 56.31174107073355373 ) ) ;
#46008 = ORIENTED_EDGE ( 'NONE', *, *, #65129, .T. ) ;
#46009 = CARTESIAN_POINT ( 'NONE',  ( -109.7156874346698032, 37.87149323084329211, 39.03482595553440859 ) ) ;
#46010 = ORIENTED_EDGE ( 'NONE', *, *, #37497, .T. ) ;
#46011 = CARTESIAN_POINT ( 'NONE',  ( -37.92511097250854135, 10.74631978746599614, 14.64581220136760109 ) ) ;
#46012 = EDGE_LOOP ( 'NONE', ( #66839, #50096 ) ) ;
#46013 = CARTESIAN_POINT ( 'NONE',  ( -5.000000000000058620, -31.11269837220806878, 85.00100000000000477 ) ) ;
#46014 = FACE_OUTER_BOUND ( 'NONE', #27595, .T. ) ;
#46015 = CARTESIAN_POINT ( 'NONE',  ( 112.3013380801407237, 395.0000000000010800, 96.05029585798746439 ) ) ;
#46016 = DIRECTION ( 'NONE',  ( -1.000000000000000000, 0.000000000000000000, 0.000000000000000000 ) ) ;
#46017 = DIRECTION ( 'NONE',  ( 0.000000000000000000, 0.000000000000000000, -1.000000000000000000 ) ) ;
#46018 = CARTESIAN_POINT ( 'NONE',  ( -9.779603649692296230, 8.034615131607072414, -35.66029398720795029 ) ) ;
#46019 = VECTOR ( 'NONE', #16212, 1000.000000000000000 ) ;
#46020 = DIRECTION ( 'NONE',  ( -0.1785568947986229393, -0.9839295885986322210, 0.000000000000000000 ) ) ;
#46021 = ORIENTED_EDGE ( 'NONE', *, *, #52002, .T. ) ;
#46022 = CARTESIAN_POINT ( 'NONE',  ( -108.9724455943903934, 36.31238718243987051, -92.78713564447804174 ) ) ;
#46023 = ORIENTED_EDGE ( 'NONE', *, *, #28231, .T. ) ;
#46024 = CARTESIAN_POINT ( 'NONE',  ( -56.97107423601133291, 15.20373812575556194, 30.55074923349853577 ) ) ;
#46025 = CARTESIAN_POINT ( 'NONE',  ( -61.52761555060400411, 17.56359742150279857, 60.84458079513598250 ) ) ;
#46026 = CARTESIAN_POINT ( 'NONE',  ( -74.69807204964287450, -6.722948167758066695, 0.000000000000000000 ) ) ;
#46027 = ORIENTED_EDGE ( 'NONE', *, *, #62367, .F. ) ;
#46028 = DIRECTION ( 'NONE',  ( -0.000000000000000000, -0.000000000000000000, -1.000000000000000000 ) ) ;
#46029 = CARTESIAN_POINT ( 'NONE',  ( -15.22871623201694113, 7.486724405784663361, -70.98788577669509436 ) ) ;
#46030 = CARTESIAN_POINT ( 'NONE',  ( -37.07086358537073068, 10.58360809068249786, 42.69363681085601314 ) ) ;
#46031 = SHAPE_REPRESENTATION ( 'motor assembly', ( #39895, #27519, #9564, #37660, #16280, #69092, #38789 ), #47761 ) ;
#46032 = CARTESIAN_POINT ( 'NONE',  ( 141.0645618855930081, 45.95036951196539832, -45.66291655381088077 ) ) ;
#46033 = VERTEX_POINT ( 'NONE', #9760 ) ;
#46034 =( LENGTH_UNIT ( ) NAMED_UNIT ( * ) SI_UNIT ( .MILLI., .METRE. ) );
#46035 = CARTESIAN_POINT ( 'NONE',  ( -40.53976144614951949, -9.891532800627171440, 13.79046340968177553 ) ) ;
#46036 = CARTESIAN_POINT ( 'NONE',  ( -125.4433371161043880, 46.19736518073188591, 45.61994787315710909 ) ) ;
#46037 = CARTESIAN_POINT ( 'NONE',  ( -60.97011009284707939, 16.34812508431679490, -38.08186052385045883 ) ) ;
#46038 = ORIENTED_EDGE ( 'NONE', *, *, #13125, .F. ) ;
#46039 = CARTESIAN_POINT ( 'NONE',  ( 8.000000000000007105, 249.8719672152120381, -95.00000000000133582 ) ) ;
#46040 = CARTESIAN_POINT ( 'NONE',  ( 93.08533330311587406, 21.72562315962719381, 60.20712453432130218 ) ) ;
#46041 = CARTESIAN_POINT ( 'NONE',  ( -4.337405327941355360, 24.62086340933515416, 0.000000000000000000 ) ) ;
#46042 = CARTESIAN_POINT ( 'NONE',  ( 91.76185853696540562, 21.23554806651647908, -91.48147536935182700 ) ) ;
#46043 = EDGE_CURVE ( 'NONE', #66949, #65005, #53509, .T. ) ;
#46044 = CARTESIAN_POINT ( 'NONE',  ( -125.8938041572051105, 46.49392987655492959, -61.75825448869760237 ) ) ;
#46045 = ORIENTED_EDGE ( 'NONE', *, *, #2975, .T. ) ;
#46046 = CARTESIAN_POINT ( 'NONE',  ( 198.4017331595409246, 98.09114638179336509, 32.62335811823028564 ) ) ;
#46047 = PLANE ( 'NONE',  #30604 ) ;
#46048 = CARTESIAN_POINT ( 'NONE',  ( 69.74037587279242700, 14.33355757956376308, 67.51542470792016104 ) ) ;
#46049 = CARTESIAN_POINT ( 'NONE',  ( 187.8408212037641363, 85.71485242454924958, -94.12920833377788199 ) ) ;
#46050 = CARTESIAN_POINT ( 'NONE',  ( -2.000000000000000000, 0.000000000000000000, 378.0000000000000000 ) ) ;
#46051 = AXIS2_PLACEMENT_3D ( 'NONE', #59520, #11338, #54239 ) ;
#46052 = ORIENTED_EDGE ( 'NONE', *, *, #63990, .F. ) ;
#46053 = ADVANCED_FACE ( 'NONE', ( #10431 ), #48060, .T. ) ;
#46054 = CARTESIAN_POINT ( 'NONE',  ( 160.4986104110022609, 61.33701824525267199, -9.914387348297012181 ) ) ;
#46055 = ORIENTED_EDGE ( 'NONE', *, *, #2544, .T. ) ;
#46056 = CARTESIAN_POINT ( 'NONE',  ( 69.83260694998124052, 15.39825517924928633, 67.29435474199121359 ) ) ;
#46057 = CARTESIAN_POINT ( 'NONE',  ( 130.8547135988932837, 39.64036133002733919, 83.79612325623102720 ) ) ;
#46058 = EDGE_CURVE ( 'NONE', #18538, #65633, #32591, .T. ) ;
#46059 = ADVANCED_FACE ( 'NONE', ( #32252 ), #31552, .T. ) ;
#46061 = ORIENTED_EDGE ( 'NONE', *, *, #46259, .T. ) ;
#46060 = DIRECTION ( 'NONE',  ( 0.000000000000000000, 0.000000000000000000, -1.000000000000000000 ) ) ;
#46062 = CARTESIAN_POINT ( 'NONE',  ( 164.9540180502650628, 65.02981548735053252, -43.05572303975047532 ) ) ;
#46063 = AXIS2_PLACEMENT_3D ( 'NONE', #36997, #6372, #16224 ) ;
#46064 = FACE_OUTER_BOUND ( 'NONE', #7036, .T. ) ;
#46065 = EDGE_CURVE ( 'NONE', #5954, #29355, #26838, .T. ) ;
#46066 = CARTESIAN_POINT ( 'NONE',  ( 158.3595886390531859, 58.34525996025800509, -51.08445656034285065 ) ) ;
#46067 = ORIENTED_EDGE ( 'NONE', *, *, #52804, .F. ) ;
#46068 = LINE ( 'NONE', #66508, #28856 ) ;
#46069 = CARTESIAN_POINT ( 'NONE',  ( 56.05126732939165635, 12.19092237165827797, 93.80575097029306164 ) ) ;
#46070 = PLANE ( 'NONE',  #21937 ) ;
#46071 = CARTESIAN_POINT ( 'NONE',  ( 80.16761386260783695, 18.37011649821943848, -20.31712373240189606 ) ) ;
#46072 = CARTESIAN_POINT ( 'NONE',  ( -176.9221788447023584, 93.01200774825315420, -89.43217687938971494 ) ) ;
#46073 = CARTESIAN_POINT ( 'NONE',  ( 154.4429418375333114, 55.33424769452792447, 56.87730265075583702 ) ) ;
#46074 = CARTESIAN_POINT ( 'NONE',  ( 93.08174259058947086, 22.79847752828721141, 41.06691016658683679 ) ) ;
#46075 = ORIENTED_EDGE ( 'NONE', *, *, #52860, .F. ) ;
#46076 = CARTESIAN_POINT ( 'NONE',  ( -95.60805465865861663, 30.63099276904602775, 61.40042467303059226 ) ) ;
#46077 = CARTESIAN_POINT ( 'NONE',  ( -13.77312480593388955, 8.361845410302542803, 59.88460182822674227 ) ) ;
#46078 = ORIENTED_EDGE ( 'NONE', *, *, #65531, .T. ) ;
#46079 = VECTOR ( 'NONE', #13571, 1000.000000000000000 ) ;
#46080 = CARTESIAN_POINT ( 'NONE',  ( 150.4542242713869484, 53.63744268572191487, -14.11560879282218650 ) ) ;
#46081 = CARTESIAN_POINT ( 'NONE',  ( 1.310872448937990153, -8.480771745766427117, -0.3173508448886726563 ) ) ;
#46082 =( NAMED_UNIT ( * ) SI_UNIT ( $, .STERADIAN. ) SOLID_ANGLE_UNIT ( ) );
#46083 = CARTESIAN_POINT ( 'NONE',  ( 31.11269837220812562, 36.11269837220800838, 2.000000000000001776 ) ) ;
#46084 = CARTESIAN_POINT ( 'NONE',  ( 61.40252071262365519, 12.30418078306080432, 83.67024983266009031 ) ) ;
#46085 = EDGE_CURVE ( 'NONE', #39331, #5030, #52990, .T. ) ;
#46086 = CARTESIAN_POINT ( 'NONE',  ( -54.08504625707234226, 14.42374043447185450, -62.10766578188960807 ) ) ;
#46087 = CARTESIAN_POINT ( 'NONE',  ( -1.866625526081660214, 7.583073082893622363, -11.49243256803911706 ) ) ;
#46088 = CARTESIAN_POINT ( 'NONE',  ( 177.5945652320813792, 75.14951358071816401, 16.60670449205189669 ) ) ;
#46089 = CARTESIAN_POINT ( 'NONE',  ( -31.43908319763709969, 10.61114334766715928, -50.31719736520186359 ) ) ;
#46090 = EDGE_LOOP ( 'NONE', ( #37435, #42031, #41001, #3615 ) ) ;
#46091 = CARTESIAN_POINT ( 'NONE',  ( -20.93485882276935328, -13.66498028065569059, 0.000000000000000000 ) ) ;
#46092 = VERTEX_POINT ( 'NONE', #60370 ) ;
#46093 = CARTESIAN_POINT ( 'NONE',  ( 106.6228877857910931, 27.24245963308690932, -63.68110863517714648 ) ) ;
#46094 = CARTESIAN_POINT ( 'NONE',  ( 45.76405797021010358, 10.34101216371941945, -12.29601346399615736 ) ) ;
#46095 = CARTESIAN_POINT ( 'NONE',  ( 45.04360969585140850, 9.210232288266707812, 69.22437720569834596 ) ) ;
#46096 = CARTESIAN_POINT ( 'NONE',  ( -7.486743542469089796, -64.58150799671139453, 41.38025477438755928 ) ) ;
#46097 = CARTESIAN_POINT ( 'NONE',  ( -0.3308315265093308422, 6.518779160332018208, 90.59193596399374826 ) ) ;
#46098 = AXIS2_PLACEMENT_3D ( 'NONE', #56522, #51263, #4446 ) ;
#46099 = CARTESIAN_POINT ( 'NONE',  ( -109.7790042512817905, 37.90666514836946988, -15.96121214152020151 ) ) ;
#46100 = ORIENTED_EDGE ( 'NONE', *, *, #34487, .T. ) ;
#46101 = CARTESIAN_POINT ( 'NONE',  ( -25.00000000000000000, 0.000000000000000000, 30.00000000000000000 ) ) ;
#46102 = CARTESIAN_POINT ( 'NONE',  ( -171.0814041607219735, 84.88598211196834598, 57.93652428202116766 ) ) ;
#46103 = EDGE_LOOP ( 'NONE', ( #14802, #16331, #10923, #36774 ) ) ;
#46104 = ORIENTED_EDGE ( 'NONE', *, *, #60819, .F. ) ;
#46105 = FACE_OUTER_BOUND ( 'NONE', #47723, .T. ) ;
#46106 = DIRECTION ( 'NONE',  ( 0.000000000000000000, 0.000000000000000000, 1.000000000000000000 ) ) ;
#46107 = CARTESIAN_POINT ( 'NONE',  ( -47.07758065111505630, -21.28397262622344499, 26.66469104408689361 ) ) ;
#46108 = CARTESIAN_POINT ( 'NONE',  ( 105.2529848321548229, 27.73895015262025510, 58.35137084276885133 ) ) ;
#46109 = DIRECTION ( 'NONE',  ( 1.000000000000000000, 1.387778780781445676E-16, -1.110223024625156294E-16 ) ) ;
#46110 = AXIS2_PLACEMENT_3D ( 'NONE', #64955, #6200, #49093 ) ;
#46111 = CARTESIAN_POINT ( 'NONE',  ( 62.05396267233470553, 13.48332220860127251, -23.83009510918770602 ) ) ;
#46112 = ORIENTED_EDGE ( 'NONE', *, *, #16639, .T. ) ;
#46113 = LINE ( 'NONE', #13425, #26672 ) ;
#46114 = PRODUCT_DEFINITION ( 'UNKNOWN', '', #4097, #6401 ) ;
#46115 = ORIENTED_EDGE ( 'NONE', *, *, #58413, .T. ) ;
#46116 = CARTESIAN_POINT ( 'NONE',  ( 16.27775141556967498, 7.523247835309956777, -50.51894409868579316 ) ) ;
#46117 = CARTESIAN_POINT ( 'NONE',  ( -146.1201263095600211, 62.66021356509619977, 44.91613754074177933 ) ) ;
#46118 = CARTESIAN_POINT ( 'NONE',  ( 212.1700216741374447, 117.1889356120871497, 35.98003273437689131 ) ) ;
#46119 = FACE_BOUND ( 'NONE', #23786, .T. ) ;
#46120 = EDGE_CURVE ( 'NONE', #9716, #53253, #37797, .T. ) ;
#46121 = EDGE_CURVE ( 'NONE', #65685, #50735, #55428, .T. ) ;
#46122 = EDGE_CURVE ( 'NONE', #68798, #68305, #44884, .T. ) ;
#46123 = ORIENTED_EDGE ( 'NONE', *, *, #16522, .T. ) ;
#46124 = EDGE_LOOP ( 'NONE', ( #1519, #21732, #53327, #40318 ) ) ;
#46125 = DIRECTION ( 'NONE',  ( 0.9362348706397369824, 0.3513748240813435175, 0.000000000000000000 ) ) ;
#46126 = CARTESIAN_POINT ( 'NONE',  ( -133.4012201662767154, 52.87735233434317905, 91.74459345490905093 ) ) ;
#46127 = CARTESIAN_POINT ( 'NONE',  ( 1.005827167100601827, 0.000000000000000000, -9.949286995052577964 ) ) ;
#46128 = CARTESIAN_POINT ( 'NONE',  ( 133.8566784816069060, 42.60093787723652525, -36.02331093239566684 ) ) ;
#46129 = CARTESIAN_POINT ( 'NONE',  ( 9.116793664011934695, 6.378730188587224958, 87.76143697225847973 ) ) ;
#46130 = VECTOR ( 'NONE', #50957, 999.9999999999998863 ) ;
#46131 = CARTESIAN_POINT ( 'NONE',  ( 79.92465405224848496, 17.24122384219593584, -66.76821263654514382 ) ) ;
#46132 = ORIENTED_EDGE ( 'NONE', *, *, #28778, .T. ) ;
#46133 = LINE ( 'NONE', #35592, #65135 ) ;
#46134 = DIRECTION ( 'NONE',  ( 1.000000000000000000, 0.000000000000000000, 0.000000000000000000 ) ) ;
#46135 = EDGE_LOOP ( 'NONE', ( #38654, #26305 ) ) ;
#46136 = DIRECTION ( 'NONE',  ( -0.000000000000000000, -6.405132834375902056E-16, 1.000000000000000000 ) ) ;
#46137 = ORIENTED_EDGE ( 'NONE', *, *, #42335, .T. ) ;
#46138 = CARTESIAN_POINT ( 'NONE',  ( -85.09761763353358788, 24.87634954265997678, -65.59306203265751378 ) ) ;
#46139 = DIRECTION ( 'NONE',  ( -0.000000000000000000, 1.000000000000000000, -0.000000000000000000 ) ) ;
#46140 = EDGE_CURVE ( 'NONE', #47483, #23762, #6199, .T. ) ;
#46141 = EDGE_LOOP ( 'NONE', ( #64386, #12688 ) ) ;
#46142 = EDGE_CURVE ( 'NONE', #34747, #49220, #27300, .T. ) ;
#46143 = ORIENTED_EDGE ( 'NONE', *, *, #5645, .F. ) ;
#46144 = CARTESIAN_POINT ( 'NONE',  ( 42.48820792780865219, 9.847387255477759282, 57.41842209376518014 ) ) ;
#46145 = CYLINDRICAL_SURFACE ( 'NONE', #50571, 65.00000000000000000 ) ;
#46146 = EDGE_CURVE ( 'NONE', #43260, #69361, #54672, .T. ) ;
#46147 = CARTESIAN_POINT ( 'NONE',  ( 21.73827885904429991, 6.764046335627708295, 6.097589566770120761 ) ) ;
#46148 = ORIENTED_EDGE ( 'NONE', *, *, #26436, .T. ) ;
#46149 = CARTESIAN_POINT ( 'NONE',  ( -34.56779088559552804, 10.12574264174958927, 84.58167098002580531 ) ) ;
#46150 = CARTESIAN_POINT ( 'NONE',  ( 180.6713229637342408, 79.61878926895391828, -78.06960825634332934 ) ) ;
#46151 = CARTESIAN_POINT ( 'NONE',  ( -443.1884682831975510, 394.9771332441898721, -125.6405780647352231 ) ) ;
#46152 = CARTESIAN_POINT ( 'NONE',  ( 114.6890011751076202, 30.99337387307411262, -10.51847467832273431 ) ) ;
#46153 = CARTESIAN_POINT ( 'NONE',  ( 84.97658021689287011, 19.92447159015900837, -50.64111290637077900 ) ) ;
#46154 = DIRECTION ( 'NONE',  ( -0.000000000000000000, 1.000000000000000000, -0.000000000000000000 ) ) ;
#46155 = VERTEX_POINT ( 'NONE', #27651 ) ;
#46156 = CIRCLE ( 'NONE', #47256, 24.99999999999985434 ) ;
#46157 = ORIENTED_EDGE ( 'NONE', *, *, #12499, .T. ) ;
#46158 = CARTESIAN_POINT ( 'NONE',  ( 45.34143264614439772, 9.256465810451190990, 5.983062029440628926 ) ) ;
#46160 = CARTESIAN_POINT ( 'NONE',  ( -178.9955247929450195, 95.48949252708244728, 87.33860847132339700 ) ) ;
#46159 = AXIS2_PLACEMENT_3D ( 'NONE', #19142, #57136, #36017 ) ;
#46161 = CARTESIAN_POINT ( 'NONE',  ( -61.41100614348687969, 43.07262267896646790, 170.0000000000000000 ) ) ;
#46162 = DIRECTION ( 'NONE',  ( -0.3738650651659383151, 0.9230658208099267181, -0.09041240789275074852 ) ) ;
#46163 = CARTESIAN_POINT ( 'NONE',  ( 137.5001123695281819, 43.66803101819199640, -90.64561015475420902 ) ) ;
#46164 = CARTESIAN_POINT ( 'NONE',  ( -31.43908319763709969, 9.591432048623756756, -89.00629854612920155 ) ) ;
#46165 = CARTESIAN_POINT ( 'NONE',  ( 211.6185147280479839, 118.1878708275672381, 93.29378292525510119 ) ) ;
#46167 = CARTESIAN_POINT ( 'NONE',  ( 212.0803491126036420, 118.9047894217572860, 38.07225711898713172 ) ) ;
#46166 = AXIS2_PLACEMENT_3D ( 'NONE', #64493, #64843, #5737 ) ;
#46168 = CARTESIAN_POINT ( 'NONE',  ( 15.55634918610411610, 51.66904755831205875, 85.00100000000000477 ) ) ;
#46169 = CARTESIAN_POINT ( 'NONE',  ( -108.5289085648060308, 36.07014995015116199, 42.17405088988840589 ) ) ;
#46170 = ORIENTED_EDGE ( 'NONE', *, *, #33239, .T. ) ;
#46171 = CARTESIAN_POINT ( 'NONE',  ( 9.275903038161098735, 7.385619229189522628, -12.42222294732710530 ) ) ;
#46172 = ORIENTED_EDGE ( 'NONE', *, *, #44852, .T. ) ;
#46173 = CARTESIAN_POINT ( 'NONE',  ( 197.1980152960110502, 96.59350208824305639, -16.64405865593795752 ) ) ;
#46174 = ORIENTED_EDGE ( 'NONE', *, *, #50125, .T. ) ;
#46175 = FACE_OUTER_BOUND ( 'NONE', #17207, .T. ) ;
#46176 = DIRECTION ( 'NONE',  ( 0.000000000000000000, 0.000000000000000000, -1.000000000000000000 ) ) ;
#46177 = CARTESIAN_POINT ( 'NONE',  ( -145.9181947914995021, 62.49417193455356312, 71.65474024834820455 ) ) ;
#46178 = AXIS2_PLACEMENT_3D ( 'NONE', #36994, #68326, #25070 ) ;
#46179 = CARTESIAN_POINT ( 'NONE',  ( -149.5074843970971301, -170.0000000000000000, -69.15738112195565179 ) ) ;
#46180 = CARTESIAN_POINT ( 'NONE',  ( 37.70762885381311946, 8.195134395012285466, -35.80965490857880695 ) ) ;
#46181 = CARTESIAN_POINT ( 'NONE',  ( -103.2169245450825770, 33.25885825286822950, 3.718631916029228268 ) ) ;
#46182 = CARTESIAN_POINT ( 'NONE',  ( 8.337549025192453556, 7.382630697225777361, -44.00666453551739465 ) ) ;
#46183 = CARTESIAN_POINT ( 'NONE',  ( 0.000000000000000000, 0.000000000000000000, 170.0000000000000000 ) ) ;
#46184 = ORIENTED_EDGE ( 'NONE', *, *, #30107, .F. ) ;
#46185 = ORIENTED_EDGE ( 'NONE', *, *, #55358, .F. ) ;
#46186 = DIRECTION ( 'NONE',  ( 0.000000000000000000, -0.000000000000000000, -1.000000000000000000 ) ) ;
#46187 = CARTESIAN_POINT ( 'NONE',  ( -23.03840347525647658, 9.707315041312055470, 0.000000000000000000 ) ) ;
#46188 = DIRECTION ( 'NONE',  ( 1.000000000000000000, 0.000000000000000000, -0.000000000000000000 ) ) ;
#46189 = DIRECTION ( 'NONE',  ( -1.000000000000000000, 0.000000000000000000, 0.000000000000000000 ) ) ;
#46190 = EDGE_CURVE ( 'NONE', #37097, #19981, #625, .T. ) ;
#46191 = CARTESIAN_POINT ( 'NONE',  ( 8.000000000000007105, 249.8719672152120381, -95.00000000000133582 ) ) ;
#46192 = CARTESIAN_POINT ( 'NONE',  ( -102.2801239173131194, -170.0000000000000000, 11.17452391595143091 ) ) ;
#46193 = CARTESIAN_POINT ( 'NONE',  ( 177.7889574972182345, 75.33777460203563692, -77.32201188078130372 ) ) ;
#46194 = CARTESIAN_POINT ( 'NONE',  ( 279.3475734619033233, -21.43178884250801630, 4.968175626252045340 ) ) ;
#46195 = CARTESIAN_POINT ( 'NONE',  ( 93.70675391435744928, 21.95852801827563283, -18.97173053105346341 ) ) ;
#46196 = CARTESIAN_POINT ( 'NONE',  ( -29.04400972079233156, 10.22852224114065400, 71.67251108405717730 ) ) ;
#46197 = CARTESIAN_POINT ( 'NONE',  ( -14.86595946517991429, -20.25193917588099524, 0.000000000000000000 ) ) ;
#46198 = DIRECTION ( 'NONE',  ( -0.000000000000000000, 1.000000000000000000, -0.000000000000000000 ) ) ;
#46199 = ADVANCED_FACE ( 'NONE', ( #4320 ), #61419, .T. ) ;
#46200 = EDGE_CURVE ( 'NONE', #3462, #38900, #3972, .T. ) ;
#46201 = DIRECTION ( 'NONE',  ( 1.000000000000000000, 0.000000000000000000, 0.000000000000000000 ) ) ;
#46202 = ORIENTED_EDGE ( 'NONE', *, *, #29460, .T. ) ;
#46203 = CARTESIAN_POINT ( 'NONE',  ( 275.6635354938838987, 21.85802876872917366, -2.510136981039510662 ) ) ;
#46204 = ADVANCED_FACE ( 'NONE', ( #25089 ), #42292, .T. ) ;
#46205 = CIRCLE ( 'NONE', #50685, 245.3095347406802489 ) ;
#46206 = CARTESIAN_POINT ( 'NONE',  ( -126.3458714439411068, 46.79154809309480356, -76.75825448869765921 ) ) ;
#46207 = CARTESIAN_POINT ( 'NONE',  ( 188.9999999999999432, 192.0000000000000000, 72.99999999999998579 ) ) ;
#46208 = CARTESIAN_POINT ( 'NONE',  ( -48.33725449172838751, 12.98311179783358860, -46.09223612232730716 ) ) ;
#46209 = LINE ( 'NONE', #39906, #31202 ) ;
#46210 = PLANE ( 'NONE',  #33367 ) ;
#46211 = CIRCLE ( 'NONE', #20402, 20.00000000000000000 ) ;
#46212 = ORIENTED_EDGE ( 'NONE', *, *, #14609, .T. ) ;
#46213 = CARTESIAN_POINT ( 'NONE',  ( -189.9209858985310291, 108.0357717895543743, -92.64894649195353793 ) ) ;
#46214 = LINE ( 'NONE', #67694, #3491 ) ;
#46215 = ORIENTED_EDGE ( 'NONE', *, *, #29609, .F. ) ;
#46216 = CIRCLE ( 'NONE', #66484, 5.000000000000004441 ) ;
#46217 = CIRCLE ( 'NONE', #15887, 8.000000000000000000 ) ;
#46218 = ORIENTED_EDGE ( 'NONE', *, *, #43090, .T. ) ;
#46219 = CARTESIAN_POINT ( 'NONE',  ( 0.000000000000000000, 0.000000000000000000, 170.0000000000000000 ) ) ;
#46220 = DIRECTION ( 'NONE',  ( -0.000000000000000000, 1.000000000000000000, -0.000000000000000000 ) ) ;
#46221 = CARTESIAN_POINT ( 'NONE',  ( 157.4703587214989113, 58.92748579479258808, 56.25401806271706562 ) ) ;
#46222 = ADVANCED_FACE ( 'NONE', ( #68343 ), #69008, .T. ) ;
#46223 = VERTEX_POINT ( 'NONE', #14522 ) ;
#46224 = DIRECTION ( 'NONE',  ( 1.000000000000000000, 0.000000000000000000, 0.000000000000000000 ) ) ;
#46225 = LINE ( 'NONE', #25828, #36775 ) ;
#46226 = DIRECTION ( 'NONE',  ( 0.000000000000000000, 0.02271222823333339177, -0.9997420440737084801 ) ) ;
#46227 = AXIS2_PLACEMENT_3D ( 'NONE', #49008, #60628, #32504 ) ;
#46228 = CARTESIAN_POINT ( 'NONE',  ( 61.33840119549016379, 13.32121602003046767, -50.53478291774639786 ) ) ;
#46229 = LINE ( 'NONE', #64482, #59534 ) ;
#46230 = CARTESIAN_POINT ( 'NONE',  ( -29.03891846981456837, 10.22741474064059020, -23.09507797556338105 ) ) ;
#46231 = CARTESIAN_POINT ( 'NONE',  ( 141.2811136745703209, 46.09188267874202438, 9.070541501198734480 ) ) ;
#46232 = ORIENTED_EDGE ( 'NONE', *, *, #33358, .F. ) ;
#46233 = CARTESIAN_POINT ( 'NONE',  ( 115.7746371641014917, 31.52600568297706118, -38.33433772466845113 ) ) ;
#46234 = LINE ( 'NONE', #9299, #13464 ) ;
#46235 = CARTESIAN_POINT ( 'NONE',  ( 46.89006465517228861, 9.501960077668737625, -42.63097907811025067 ) ) ;
#46236 = CARTESIAN_POINT ( 'NONE',  ( -78.09558237016243254, 23.18089682183424571, 84.12268224481751133 ) ) ;
#46238 = VERTEX_POINT ( 'NONE', #7612 ) ;
#46237 = CARTESIAN_POINT ( 'NONE',  ( -118.4451797092949477, 41.78112676557538663, 92.74816161723661878 ) ) ;
#46239 = CARTESIAN_POINT ( 'NONE',  ( 44.01696072965949469, 47.84694004974210912, 170.0000000000000000 ) ) ;
#46240 = ORIENTED_EDGE ( 'NONE', *, *, #48903, .F. ) ;
#46241 = ORIENTED_EDGE ( 'NONE', *, *, #63993, .T. ) ;
#46242 = CARTESIAN_POINT ( 'NONE',  ( -142.0902782307734924, 58.13494170556001706, 63.91892788494654809 ) ) ;
#46243 = CARTESIAN_POINT ( 'NONE',  ( 4.360227497916021377, -41.50063969896140037, 13.79046340968177731 ) ) ;
#46244 = CARTESIAN_POINT ( 'NONE',  ( 197.2197025888162329, 96.62026035493821041, -71.33074997753084290 ) ) ;
#46245 = CARTESIAN_POINT ( 'NONE',  ( 188.5662303205147055, 86.51341602961787203, -16.28199567469592424 ) ) ;
#46246 = CARTESIAN_POINT ( 'NONE',  ( -118.8504142000305279, 42.02789424825279951, 67.55506623760311413 ) ) ;
#46247 = CARTESIAN_POINT ( 'NONE',  ( -86.11230725916331608, 26.39026888680172434, -16.80460309939184071 ) ) ;
#46248 = DIRECTION ( 'NONE',  ( -1.000000000000000000, -0.000000000000000000, -0.000000000000000000 ) ) ;
#46249 = CARTESIAN_POINT ( 'NONE',  ( -154.7934364910360614, 68.79594655117534785, -36.98658425784656600 ) ) ;
#46250 = ORIENTED_EDGE ( 'NONE', *, *, #24669, .T. ) ;
#46251 =( REPRESENTATION_RELATIONSHIP ('NONE','NONE', #40274, #64925 ) REPRESENTATION_RELATIONSHIP_WITH_TRANSFORMATION ( #59350 )SHAPE_REPRESENTATION_RELATIONSHIP( ) );
#46252 = VERTEX_POINT ( 'NONE', #41264 ) ;
#46253 = DIRECTION ( 'NONE',  ( 1.000000000000000000, 0.000000000000000000, 0.000000000000000000 ) ) ;
#46254 = AXIS2_PLACEMENT_3D ( 'NONE', #58829, #54941, #6760 ) ;
#46255 = CARTESIAN_POINT ( 'NONE',  ( 103.0026233023292832, 25.67408295205786928, 61.93245107129636295 ) ) ;
#46256 = CARTESIAN_POINT ( 'NONE',  ( 164.8407099662994995, 63.61629583487393802, 62.33837009251364947 ) ) ;
#46257 = CARTESIAN_POINT ( 'NONE',  ( -2.999999999999992450, 0.000000000000000000, 0.000000000000000000 ) ) ;
#46258 = VECTOR ( 'NONE', #66165, 1000.000000000000000 ) ;
#46259 = EDGE_CURVE ( 'NONE', #2957, #11118, #9248, .T. ) ;
#46260 = FACE_OUTER_BOUND ( 'NONE', #58874, .T. ) ;
#46261 = CARTESIAN_POINT ( 'NONE',  ( -452.6627218934913799, 400.0000000000079581, 113.5502958579925803 ) ) ;
#46262 = CARTESIAN_POINT ( 'NONE',  ( 164.4728833318992258, 63.30716077995682411, -67.76901369371475425 ) ) ;
#46263 = ORIENTED_EDGE ( 'NONE', *, *, #52387, .T. ) ;
#46264 = PRODUCT_DEFINITION_SHAPE ( 'NONE', 'NONE',  #69588 ) ;
#46265 = ORIENTED_EDGE ( 'NONE', *, *, #15982, .T. ) ;
#46266 = VERTEX_POINT ( 'NONE', #15563 ) ;
#46267 = VECTOR ( 'NONE', #17982, 1000.000000000000227 ) ;
#46268 = CARTESIAN_POINT ( 'NONE',  ( -153.1031717208031750, 68.63449618039565792, -22.05411808047816891 ) ) ;
#46269 = CARTESIAN_POINT ( 'NONE',  ( -84.23431294393863311, 24.52078568147205573, 59.71377569600485913 ) ) ;
#46270 = CARTESIAN_POINT ( 'NONE',  ( 64.94794467308301478, 13.12874966082104855, -35.95744817871243981 ) ) ;
#46271 = LINE ( 'NONE', #57534, #51287 ) ;
#46272 = AXIS2_PLACEMENT_3D ( 'NONE', #20717, #68563, #68887 ) ;
#46273 = CARTESIAN_POINT ( 'NONE',  ( -56.73868929054669508, 16.18382781951277494, 45.12942635042991668 ) ) ;
#46274 = DIRECTION ( 'NONE',  ( -0.000000000000000000, 0.9989683093773507050, 0.04541273895899262947 ) ) ;
#46275 = CARTESIAN_POINT ( 'NONE',  ( 34.45500533947588195, 7.817363290423888778, 69.91678222496804551 ) ) ;
#46276 = CARTESIAN_POINT ( 'NONE',  ( 8.336882341125877005, 6.376438415325264231, -17.15788629728112724 ) ) ;
#46277 =( LENGTH_UNIT ( ) NAMED_UNIT ( * ) SI_UNIT ( .MILLI., .METRE. ) );
#46278 = EDGE_LOOP ( 'NONE', ( #15823, #34875, #53814, #57477, #11276, #36824, #4393, #3819, #10500 ) ) ;
#46279 = CARTESIAN_POINT ( 'NONE',  ( 57.61205590192970050, -9.184630597077863001, 27.58472369370706545 ) ) ;
#46280 = FACE_BOUND ( 'NONE', #7683, .T. ) ;
#46281 = CARTESIAN_POINT ( 'NONE',  ( -122.3745688183165754, 44.21964839958060622, 17.91535119075751581 ) ) ;
#46282 = CARTESIAN_POINT ( 'NONE',  ( 64.94794467308304320, 13.12874966082103079, -62.80199876917609458 ) ) ;
#46283 = CARTESIAN_POINT ( 'NONE',  ( -447.6627218934913799, 389.9999999999998295, -141.4497041420118535 ) ) ;
#46284 = CARTESIAN_POINT ( 'NONE',  ( 22.51849650178395024, 7.817407610814550267, -12.85559206638460950 ) ) ;
#46285 = CARTESIAN_POINT ( 'NONE',  ( 197.3059626281005592, 96.72682679064189415, 64.86311202157818911 ) ) ;
#46286 = EDGE_CURVE ( 'NONE', #54192, #5133, #61410, .T. ) ;
#46287 = EDGE_LOOP ( 'NONE', ( #52292, #38435, #63147, #69258 ) ) ;
#46288 = APPLICATION_PROTOCOL_DEFINITION ( 'draft international standard', 'automotive_design', 1998, #38134 ) ;
#46289 = ADVANCED_FACE ( 'NONE', ( #63409 ), #68670, .F. ) ;
#46290 = FACE_OUTER_BOUND ( 'NONE', #67928, .T. ) ;
#46291 = CARTESIAN_POINT ( 'NONE',  ( -65.36598343705435354, 0.000000000000000000, 41.38025477438755928 ) ) ;
#46292 = DIRECTION ( 'NONE',  ( 0.000000000000000000, 0.000000000000000000, 1.000000000000000000 ) ) ;
#46293 = CARTESIAN_POINT ( 'NONE',  ( 187.6511924654682844, 87.00187850361888309, -47.35777523915407983 ) ) ;
#46294 = ORIENTED_EDGE ( 'NONE', *, *, #12875, .T. ) ;
#46295 = EDGE_LOOP ( 'NONE', ( #61392, #8935, #5069, #44091 ) ) ;
#46296 = CARTESIAN_POINT ( 'NONE',  ( 0.000000000000000000, 0.000000000000000000, 0.000000000000000000 ) ) ;
#46297 = DIRECTION ( 'NONE',  ( 0.000000000000000000, 0.000000000000000000, -1.000000000000000000 ) ) ;
#46298 = VERTEX_POINT ( 'NONE', #63056 ) ;
#46299 = CARTESIAN_POINT ( 'NONE',  ( 112.3013380801408800, 395.0000000000065938, -128.9497041420121093 ) ) ;
#46300 = EDGE_CURVE ( 'NONE', #68618, #61781, #15212, .T. ) ;
#46301 = EDGE_LOOP ( 'NONE', ( #11535, #15944 ) ) ;
#46302 = CARTESIAN_POINT ( 'NONE',  ( -60.98168946575808747, 17.40090852531920262, 15.59240914876137651 ) ) ;
#46303 = CARTESIAN_POINT ( 'NONE',  ( 259.4165763529819060, 225.8585178651493948, 108.9999999999999858 ) ) ;
#46304 = DIRECTION ( 'NONE',  ( -0.000000000000000000, -0.000000000000000000, -1.000000000000000000 ) ) ;
#46305 = CIRCLE ( 'NONE', #33969, 23.50000000000000000 ) ;
#46306 = EDGE_CURVE ( 'NONE', #56091, #63790, #52155, .T. ) ;
#46307 = EDGE_CURVE ( 'NONE', #68321, #4215, #41945, .T. ) ;
#46308 = CARTESIAN_POINT ( 'NONE',  ( -101.8191498210054959, 32.54686850610963234, 30.51907450641511232 ) ) ;
#46309 = CARTESIAN_POINT ( 'NONE',  ( -78.66644367742111399, -170.0000000000000000, -96.30455181264525777 ) ) ;
#46310 = CIRCLE ( 'NONE', #11443, 65.36598343705435354 ) ;
#46312 = ORIENTED_EDGE ( 'NONE', *, *, #2163, .T. ) ;
#46311 = CARTESIAN_POINT ( 'NONE',  ( -65.13282190615095146, -1.847197903505587038E-12, 5.000000000000000000 ) ) ;
#46313 = CARTESIAN_POINT ( 'NONE',  ( 55.76066037845577483, 11.10616952318092210, 35.34777878534185902 ) ) ;
#46314 = EDGE_LOOP ( 'NONE', ( #50436, #23733, #9744, #30193 ) ) ;
#46315 = ORIENTED_EDGE ( 'NONE', *, *, #15787, .T. ) ;
#46316 = CARTESIAN_POINT ( 'NONE',  ( 179.4074606910091916, 78.34362448405029511, 44.16935534552229115 ) ) ;
#46317 = B_SPLINE_CURVE_WITH_KNOTS ( 'NONE', 3,
 ( #16555, #22882, #65096, #23245, #38011, #11616 ),
 .UNSPECIFIED., .F., .F.,
 ( 4, 2, 4 ),
 ( 2.380731631042988191E-07, 0.002336973833157630128, 0.004673709593152156581 ),
 .UNSPECIFIED. ) ;
#46318 = CARTESIAN_POINT ( 'NONE',  ( 21.42484406671928454, 6.746536496442161912, -74.81728185975761392 ) ) ;
#46320 = VERTEX_POINT ( 'NONE', #46879 ) ;
#46319 = CARTESIAN_POINT ( 'NONE',  ( -128.9843070188473177, 49.78011598923035308, 58.11564453485428317 ) ) ;
#46321 = CARTESIAN_POINT ( 'NONE',  ( -100.8612319006215472, 33.19127816346582449, 84.33756607052741572 ) ) ;
#46322 = AXIS2_PLACEMENT_3D ( 'NONE', #50399, #27894, #1160 ) ;
#46323 = CARTESIAN_POINT ( 'NONE',  ( 31.11269837220806522, 4.999999999999936939, 85.00100000000000477 ) ) ;
#46324 = ORIENTED_EDGE ( 'NONE', *, *, #57657, .T. ) ;
#46325 = CARTESIAN_POINT ( 'NONE',  ( 211.8382652195006415, 118.5282575235989668, -68.35397587044393219 ) ) ;
#46326 = CARTESIAN_POINT ( 'NONE',  ( 134.3182571105339207, 42.88121222759020412, 44.51034083899536142 ) ) ;
#46327 = DIRECTION ( 'NONE',  ( 0.000000000000000000, 0.000000000000000000, -1.000000000000000000 ) ) ;
#46328 = DIRECTION ( 'NONE',  ( 0.000000000000000000, 0.000000000000000000, 1.000000000000000000 ) ) ;
#46329 = CARTESIAN_POINT ( 'NONE',  ( 66.73467315386237431, 14.60276727483218018, -63.53416605551942808 ) ) ;
#46330 = EDGE_LOOP ( 'NONE', ( #5945, #68139, #67100, #888 ) ) ;
#46331 = EDGE_LOOP ( 'NONE', ( #57098, #13339, #51780, #65627, #10534, #37140 ) ) ;
#46332 = CARTESIAN_POINT ( 'NONE',  ( 187.0823097343935331, 84.88801889414973800, 94.99999999999866418 ) ) ;
#46333 = CARTESIAN_POINT ( 'NONE',  ( -170.2801941679960009, 84.02053682015869640, -49.16597572273842331 ) ) ;
#46334 = DIRECTION ( 'NONE',  ( 1.000000000000000000, 0.000000000000000000, 1.110223024625156294E-16 ) ) ;
#46335 = CARTESIAN_POINT ( 'NONE',  ( 46.66904755831212981, 15.55634918610394379, 85.00100000000000477 ) ) ;
#46336 = CARTESIAN_POINT ( 'NONE',  ( -52.95640735647533148, 15.16886689662459275, -89.20118622082404158 ) ) ;
#46337 = ADVANCED_FACE ( 'NONE', ( #14861 ), #36326, .T. ) ;
#46338 = CARTESIAN_POINT ( 'NONE',  ( 15.78827728214693416, -170.0000000000000000, -69.86349468914949057 ) ) ;
#46339 = CARTESIAN_POINT ( 'NONE',  ( -149.5074843970971017, 64.17983161892347255, 45.72082123989907387 ) ) ;
#46340 = CARTESIAN_POINT ( 'NONE',  ( -125.8938041572051105, 47.69968343338781835, 45.61994787315711619 ) ) ;
#46341 = CARTESIAN_POINT ( 'NONE',  ( -165.6212796729685124, 79.15047440262054579, -69.36342526124160202 ) ) ;
#46342 = VERTEX_POINT ( 'NONE', #52501 ) ;
#46343 = CARTESIAN_POINT ( 'NONE',  ( -106.4728934171453858, 36.10295170132725673, 31.79594541829927579 ) ) ;
#46344 = VERTEX_POINT ( 'NONE', #20481 ) ;
#46345 = EDGE_CURVE ( 'NONE', #45819, #50285, #2558, .T. ) ;
#46346 = CARTESIAN_POINT ( 'NONE',  ( -38.84150381976579069, 10.92416363971238802, 9.640924607406274660 ) ) ;
#46347 = CARTESIAN_POINT ( 'NONE',  ( -783.0172411895269988, -622.0000000000060254, 10.00000000000000000 ) ) ;
#46348 = ORIENTED_EDGE ( 'NONE', *, *, #21045, .F. ) ;
#46349 = CARTESIAN_POINT ( 'NONE',  ( -82.52059008511432125, 23.82719274235528317, -89.86705382797902075 ) ) ;
#46350 = CARTESIAN_POINT ( 'NONE',  ( 51.39999999999999858, 0.000000000000000000, 4.171999999999999709 ) ) ;
#46351 = CARTESIAN_POINT ( 'NONE',  ( -15.67984581961064450, 63.08044415722863363, 170.0000000000000000 ) ) ;
#46352 = SURFACE_SIDE_STYLE ('',( #51649 ) ) ;
#46353 = CARTESIAN_POINT ( 'NONE',  ( -417.6627218934913230, 219.4906275429376308, 111.5502958579881749 ) ) ;
#46354 = CARTESIAN_POINT ( 'NONE',  ( -8.810383862755514883, 7.965311326754783927, -35.46662548705337059 ) ) ;
#46355 = CARTESIAN_POINT ( 'NONE',  ( -37.52119286077854099, 11.69341290629620289, -20.36792989721667269 ) ) ;
#46356 = ORIENTED_EDGE ( 'NONE', *, *, #46932, .T. ) ;
#46357 = CARTESIAN_POINT ( 'NONE',  ( -123.8554280348324852, 46.36425916468965625, -88.88211011207803836 ) ) ;
#46358 = ORIENTED_EDGE ( 'NONE', *, *, #50280, .F. ) ;
#46359 = DIRECTION ( 'NONE',  ( -0.000000000000000000, -1.000000000000000000, -0.000000000000000000 ) ) ;
#46360 = CARTESIAN_POINT ( 'NONE',  ( -56.02289203441036847, 15.98631679403369255, 72.11475544954369354 ) ) ;
#46361 = CARTESIAN_POINT ( 'NONE',  ( -24.70911172866235006, 8.583078995053019966, 7.525281538729513997 ) ) ;
#46362 = VERTEX_POINT ( 'NONE', #21184 ) ;
#46363 = EDGE_CURVE ( 'NONE', #4738, #59256, #20985, .T. ) ;
#46364 = PLANE ( 'NONE',  #64830 ) ;
#46365 = CARTESIAN_POINT ( 'NONE',  ( -60.43659296547055249, 16.19120964214080161, -91.16608923734209213 ) ) ;
#46366 = CARTESIAN_POINT ( 'NONE',  ( -38.26732153931116898, 10.81230693396213915, 34.60420372569744529 ) ) ;
#46367 = AXIS2_PLACEMENT_3D ( 'NONE', #53705, #31245, #37191 ) ;
#46368 = EDGE_CURVE ( 'NONE', #47148, #1332, #37343, .T. ) ;
#46369 = CARTESIAN_POINT ( 'NONE',  ( 153.2208437558771834, 55.67531116261156399, -37.42660832897070122 ) ) ;
#46370 = VECTOR ( 'NONE', #5102, 1000.000000000000000 ) ;
#46371 = EDGE_CURVE ( 'NONE', #28945, #35894, #63680, .T. ) ;
#46372 = VERTEX_POINT ( 'NONE', #32082 ) ;
#46374 = VECTOR ( 'NONE', #7940, 1000.000000000000000 ) ;
#46373 = CARTESIAN_POINT ( 'NONE',  ( 848.0071894358293321, 992.0915846175178103, 794.5748919861007380 ) ) ;
#46375 = ADVANCED_FACE ( 'NONE', ( #26804 ), #42959, .T. ) ;
#46376 = CARTESIAN_POINT ( 'NONE',  ( -156.9262190792700267, 72.10659547035874084, 66.20392794627127842 ) ) ;
#46377 = CARTESIAN_POINT ( 'NONE',  ( -124.3331814159187587, 45.47486189329070783, 30.78061265518531187 ) ) ;
#46378 = CYLINDRICAL_SURFACE ( 'NONE', #5185, 65.00000000000000000 ) ;
#46379 = ORIENTED_EDGE ( 'NONE', *, *, #26459, .F. ) ;
#46380 = CARTESIAN_POINT ( 'NONE',  ( -180.4651598106647725, 97.28730001475653921, -67.50490632099327115 ) ) ;
#46381 = CARTESIAN_POINT ( 'NONE',  ( 126.5079999146319381, 38.31335175111690461, 89.15821877620250291 ) ) ;
#46382 = CARTESIAN_POINT ( 'NONE',  ( 117.3110050642448243, 32.29133253383016466, 34.55243254091307392 ) ) ;
#46383 = LINE ( 'NONE', #67862, #18058 ) ;
#46384 = CARTESIAN_POINT ( 'NONE',  ( -124.3250225421925563, 45.46958056770279910, -61.92067255773788048 ) ) ;
#46385 = EDGE_CURVE ( 'NONE', #21805, #31627, #11951, .T. ) ;
#46386 = ORIENTED_EDGE ( 'NONE', *, *, #24217, .F. ) ;
#46387 = LINE ( 'NONE', #43522, #848 ) ;
#46388 = CARTESIAN_POINT ( 'NONE',  ( 61.28323125814129213, -21.66484633135379667, 170.0000000000000000 ) ) ;
#46389 = CARTESIAN_POINT ( 'NONE',  ( 188.4918087359956758, 87.93403732562659059, 35.59746311784228112 ) ) ;
#46390 = CARTESIAN_POINT ( 'NONE',  ( 185.7741388806743998, 83.47871114541692350, -91.54853474465144814 ) ) ;
#46391 = CARTESIAN_POINT ( 'NONE',  ( -78.66644367742111399, 22.32174330031316956, -8.270900041254197532 ) ) ;
#46392 = ADVANCED_FACE ( 'NONE', ( #16589 ), #38045, .F. ) ;
#46393 = EDGE_CURVE ( 'NONE', #50563, #12932, #48924, .T. ) ;
#46394 = ORIENTED_EDGE ( 'NONE', *, *, #8526, .T. ) ;
#46395 = CARTESIAN_POINT ( 'NONE',  ( 160.9099843287285410, 61.67000084894971934, -23.46024577593901483 ) ) ;
#46396 = EDGE_LOOP ( 'NONE', ( #15159, #26397, #11233, #31490 ) ) ;
#46397 = CARTESIAN_POINT ( 'NONE',  ( 68.94948716683069279, 15.16699441119056679, 59.54438869000860279 ) ) ;
#46398 = CARTESIAN_POINT ( 'NONE',  ( 127.7121523762017858, 37.83617439506281244, 94.99999999999866418 ) ) ;
#46399 = STYLED_ITEM ( 'NONE', ( #244 ), #41060 ) ;
#46400 = AXIS2_PLACEMENT_3D ( 'NONE', #578, #51806, #35974 ) ;
#46402 = ORIENTED_EDGE ( 'NONE', *, *, #25350, .T. ) ;
#46401 = CARTESIAN_POINT ( 'NONE',  ( 200.0000000000000000, 3.000000000000030198, -46.99999999999997158 ) ) ;
#46403 = CARTESIAN_POINT ( 'NONE',  ( -142.0902782307735492, 58.13494170556001706, -70.30382506737186077 ) ) ;
#46404 = LINE ( 'NONE', #2471, #54130 ) ;
#46405 = CARTESIAN_POINT ( 'NONE',  ( 162.1014732644455307, 61.34312237409766055, -37.70552761938252928 ) ) ;
#46406 = ORIENTED_EDGE ( 'NONE', *, *, #43482, .F. ) ;
#46407 = LINE ( 'NONE', #55942, #47910 ) ;
#46408 = VECTOR ( 'NONE', #49503, 1000.000000000000000 ) ;
#46409 = VECTOR ( 'NONE', #62915, 1000.000000000000000 ) ;
#46410 = CARTESIAN_POINT ( 'NONE',  ( -129.3963145237380843, 48.84337839101545597, 44.75594546263260298 ) ) ;
#46411 = CARTESIAN_POINT ( 'NONE',  ( 151.7945360828342700, 54.61722255954529004, -92.39293117455194704 ) ) ;
#46412 = CARTESIAN_POINT ( 'NONE',  ( 82.95856197793165165, 19.25847567427441831, -23.03551787981482235 ) ) ;
#46413 = CARTESIAN_POINT ( 'NONE',  ( -167.1540252468941787, 80.72321878831098729, 33.77097442923315640 ) ) ;
#46414 = AXIS2_PLACEMENT_3D ( 'NONE', #24764, #30039, #67677 ) ;
#46415 = CARTESIAN_POINT ( 'NONE',  ( 151.7819978880463339, 53.35998893001570309, 58.85968254170387581 ) ) ;
#46416 = DIRECTION ( 'NONE',  ( -1.000000000000000000, 0.000000000000000000, 0.000000000000000000 ) ) ;
#46417 = EDGE_LOOP ( 'NONE', ( #37638, #25651, #26809, #43193 ) ) ;
#46418 = CARTESIAN_POINT ( 'NONE',  ( -62.97854483871577713, 16.08424353203677271, 40.00000000000003553 ) ) ;
#46419 = DIRECTION ( 'NONE',  ( 0.000000000000000000, 0.000000000000000000, 1.000000000000000000 ) ) ;
#46420 = VERTEX_POINT ( 'NONE', #11651 ) ;
#46421 = AXIS2_PLACEMENT_3D ( 'NONE', #65302, #45230, #34353 ) ;
#46422 = CARTESIAN_POINT ( 'NONE',  ( 157.4703587214989113, 58.92748579479260229, -9.279633708673953763 ) ) ;
#46423 = CARTESIAN_POINT ( 'NONE',  ( 212.1734186221015648, 119.0499290057855291, -16.28920841871465441 ) ) ;
#46424 = CARTESIAN_POINT ( 'NONE',  ( 103.8325688302027459, 27.12251147381403271, 33.20992942965430927 ) ) ;
#46425 = CARTESIAN_POINT ( 'NONE',  ( -2.172839205444465183, 7.595638683704371452, 32.66141357948582424 ) ) ;
#46426 = CARTESIAN_POINT ( 'NONE',  ( 64.33924340318904456, 12.98343211571920008, 83.61250075476556276 ) ) ;
#46427 = CARTESIAN_POINT ( 'NONE',  ( 186.2680729609085120, 85.48839327635670315, 4.523648567817806665 ) ) ;
#46428 = CARTESIAN_POINT ( 'NONE',  ( 212.1931396682533659, 117.2245435827729665, -43.51221325195484724 ) ) ;
#46429 = CARTESIAN_POINT ( 'NONE',  ( 174.9053416555736646, 72.57849647436442808, 5.682350544106838264 ) ) ;
#46430 = CARTESIAN_POINT ( 'NONE',  ( -62.48965350618345838, 16.80247907725182088, 11.97533722146177304 ) ) ;
#46432 = ORIENTED_EDGE ( 'NONE', *, *, #57584, .F. ) ;
#46431 = SHAPE_REPRESENTATION ( 'Belt1-2', ( #66832 ), #16381 ) ;
#46433 = EDGE_CURVE ( 'NONE', #51614, #47553, #54558, .T. ) ;
#46434 = DIRECTION ( 'NONE',  ( 0.000000000000000000, 0.000000000000000000, 1.000000000000000000 ) ) ;
#46435 = ORIENTED_EDGE ( 'NONE', *, *, #18567, .F. ) ;
#46436 = CARTESIAN_POINT ( 'NONE',  ( 103.4696172145934980, 25.87254488218942328, -67.03655338143190079 ) ) ;
#46437 = DIRECTION ( 'NONE',  ( 0.4578834044730072383, 0.000000000000000000, -0.8890122540821405739 ) ) ;
#46438 = CARTESIAN_POINT ( 'NONE',  ( -75.43953471071002070, 21.11829282998125734, 4.286557885301053084 ) ) ;
#46439 = CARTESIAN_POINT ( 'NONE',  ( -31.86754543663846562, 9.661758835099860221, -89.00629854612918734 ) ) ;
#46440 = CARTESIAN_POINT ( 'NONE',  ( -13.97284672409966433, 7.369429924072608884, 86.95875599126263467 ) ) ;
#46441 = PLANE ( 'NONE',  #51304 ) ;
#46442 = ORIENTED_EDGE ( 'NONE', *, *, #44709, .T. ) ;
#46443 = CARTESIAN_POINT ( 'NONE',  ( -71.41745561414265353, 19.69148172991712542, 66.75175318804630820 ) ) ;
#46444 = CARTESIAN_POINT ( 'NONE',  ( -166.9982296371935035, 80.56207291422410322, 60.82688077875437216 ) ) ;
#46445 = ORIENTED_EDGE ( 'NONE', *, *, #56638, .T. ) ;
#46446 = ORIENTED_EDGE ( 'NONE', *, *, #64944, .T. ) ;
#46447 = EDGE_CURVE ( 'NONE', #60851, #34064, #60548, .T. ) ;
#46448 = CARTESIAN_POINT ( 'NONE',  ( 26.99999999999999645, -27.00000000000000355, 0.000000000000000000 ) ) ;
#46449 = CYLINDRICAL_SURFACE ( 'NONE', #61372, 65.00000000000000000 ) ;
#46450 = CARTESIAN_POINT ( 'NONE',  ( 175.5406524085946103, 73.17873692326779178, -21.95791395497509413 ) ) ;
#46451 = CARTESIAN_POINT ( 'NONE',  ( -168.0003605155415300, 83.06333427281273885, 59.68102058965342849 ) ) ;
#46452 = PLANE ( 'NONE',  #53218 ) ;
#46453 = ADVANCED_FACE ( 'NONE', ( #7445 ), #29239, .F. ) ;
#46454 = EDGE_CURVE ( 'NONE', #2615, #68299, #67115, .T. ) ;
#46455 = AXIS2_PLACEMENT_3D ( 'NONE', #28445, #22823, #1719 ) ;
#46456 = EDGE_LOOP ( 'NONE', ( #68789, #17181, #40869, #12776, #40987, #59863, #4113, #43549, #34383 ) ) ;
#46457 = CARTESIAN_POINT ( 'NONE',  ( 110.2429982417149432, 29.99119854320846201, -35.92243756565368784 ) ) ;
#46458 = EDGE_LOOP ( 'NONE', ( #10292, #34621, #25156, #68175 ) ) ;
#46459 = CARTESIAN_POINT ( 'NONE',  ( 210.4897348480409391, 114.6382060222044856, 5.092056172177173323 ) ) ;
#46460 = CARTESIAN_POINT ( 'NONE',  ( 9.837735240994035735, 7.389327806910502616, 59.78739175200453104 ) ) ;
#46461 = CONICAL_SURFACE ( 'NONE', #10499, 74.95140232871122521, 0.8777644062502172329 ) ;
#46462 =( NAMED_UNIT ( * ) SI_UNIT ( $, .STERADIAN. ) SOLID_ANGLE_UNIT ( ) );
#46463 = DIRECTION ( 'NONE',  ( 1.000000000000000000, 0.000000000000000000, 0.000000000000000000 ) ) ;
#46464 = AXIS2_PLACEMENT_3D ( 'NONE', #55799, #7622, #2338 ) ;
#46465 = ORIENTED_EDGE ( 'NONE', *, *, #56947, .F. ) ;
#46466 = VERTEX_POINT ( 'NONE', #34179 ) ;
#46467 = CARTESIAN_POINT ( 'NONE',  ( 115.0000633975120365, -22.00001440852518897, 0.3259197091964680659 ) ) ;
#46468 = DIRECTION ( 'NONE',  ( 0.000000000000000000, 0.000000000000000000, 1.000000000000000000 ) ) ;
#46469 = AXIS2_PLACEMENT_3D ( 'NONE', #20754, #22053, #36248 ) ;
#46470 = CARTESIAN_POINT ( 'NONE',  ( 32.66883187925818532, 8.640402022338115273, -73.30456228053577661 ) ) ;
#46471 = DIRECTION ( 'NONE',  ( -0.000000000000000000, 1.000000000000000000, -0.000000000000000000 ) ) ;
#46472 = CARTESIAN_POINT ( 'NONE',  ( 19.82795039379812607, 6.663502596869125050, 84.87619840072350996 ) ) ;
#46473 = EDGE_CURVE ( 'NONE', #8003, #41002, #66201, .T. ) ;
#46474 = CARTESIAN_POINT ( 'NONE',  ( 80.30232379693109124, 17.35837133860834314, -74.20099956211727488 ) ) ;
#46475 = ORIENTED_EDGE ( 'NONE', *, *, #1768, .F. ) ;
#46476 = EDGE_CURVE ( 'NONE', #64497, #695, #56959, .T. ) ;
#46477 = DIRECTION ( 'NONE',  ( 0.000000000000000000, 0.000000000000000000, 1.000000000000000000 ) ) ;
#46478 = B_SPLINE_CURVE_WITH_KNOTS ( 'NONE', 3,
 ( #54250, #6072, #48976, #44414, #65897, #22268, #60597, #16974, #27893, #49328, #12417, #55312, #1159, #65536, #17329, #38804, #62689, #40525, #29284, #61974, #40873, #45106, #14147, #13794, #62328, #8534, #29978, #14490, #67616, #19416, #35946, #35608, #35252, #66592, #56711, #13118, #41227, #39835, #52119, #7836 ),
 .UNSPECIFIED., .F., .F.,
 ( 4, 2, 2, 2, 2, 2, 2, 2, 2, 2, 2, 2, 2, 2, 2, 2, 2, 2, 2, 4 ),
 ( 0.02472759712254455136, 0.02626001169882804381, 0.02779242627511153627, 0.02932484085139502872, 0.03009104813953675933, 0.03085725542767848995, 0.03238967000396195117, 0.03315587729210368872, 0.03392208458024543322, 0.03545449915652893608, 0.03698691373281243200, 0.03851932830909592792, 0.04005174288537943078, 0.04158415746166292670, 0.04311657203794642262, 0.04464898661422991855, 0.04541519390237166998, 0.04618140119051342141, 0.04771381576679691733, 0.04924623034308041325 ),
 .UNSPECIFIED. ) ;
#46479 = CARTESIAN_POINT ( 'NONE',  ( 198.8752826725511227, 100.3130050945023584, -48.56026461867841704 ) ) ;
#46480 = ORIENTED_EDGE ( 'NONE', *, *, #6365, .T. ) ;
#46481 = CARTESIAN_POINT ( 'NONE',  ( -82.93267503967653909, 23.99263498936122474, 17.24672781033775948 ) ) ;
#46482 = EDGE_LOOP ( 'NONE', ( #38114, #1738, #47833, #50721 ) ) ;
#46483 = DIRECTION ( 'NONE',  ( -0.000000000000000000, -0.000000000000000000, -1.000000000000000000 ) ) ;
#46484 = ORIENTED_EDGE ( 'NONE', *, *, #45038, .T. ) ;
#46485 = EDGE_LOOP ( 'NONE', ( #51550, #29677, #64512, #35790 ) ) ;
#46486 = LINE ( 'NONE', #57395, #7194 ) ;
#46487 = CARTESIAN_POINT ( 'NONE',  ( 0.000000000000000000, 70.00000000000000000, 0.000000000000000000 ) ) ;
#46488 = CARTESIAN_POINT ( 'NONE',  ( 22.80839748737788497, 6.826915557457463812, 8.019082751123264075 ) ) ;
#46489 = EDGE_LOOP ( 'NONE', ( #35161, #29781, #66566, #32926 ) ) ;
#46490 = CARTESIAN_POINT ( 'NONE',  ( -25.17576297385273065, 8.646815144065621794, 87.26720278706356737 ) ) ;
#46491 = CARTESIAN_POINT ( 'NONE',  ( -53.13788504024112314, 15.21566150156364294, 3.705312443272094303 ) ) ;
#46492 = COLOUR_RGB ( '',0.7921568627450980005, 0.8196078431372548767, 0.9333333333333333481 ) ;
#46493 = FACE_BOUND ( 'NONE', #61988, .T. ) ;
#46494 = CARTESIAN_POINT ( 'NONE',  ( 104.7147873368644753, 26.40702926859708910, -38.33007957820842648 ) ) ;
#46495 = CARTESIAN_POINT ( 'NONE',  ( 84.72546926745367557, 19.84015517905185888, -36.05123878307442453 ) ) ;
#46496 = CARTESIAN_POINT ( 'NONE',  ( -165.6754884515988522, 80.64428675972324356, -95.00000000000133582 ) ) ;
#46497 = ORIENTED_EDGE ( 'NONE', *, *, #40793, .T. ) ;
#46498 = VECTOR ( 'NONE', #9001, 1000.000000000000000 ) ;
#46500 = ORIENTED_EDGE ( 'NONE', *, *, #29645, .T. ) ;
#46499 = PRODUCT_DEFINITION ( 'UNKNOWN', '', #48996, #64099 ) ;
#46501 = VECTOR ( 'NONE', #27149, 1000.000000000000000 ) ;
#46502 = CARTESIAN_POINT ( 'NONE',  ( -85.64924756730684408, 26.19583280090852639, -72.20824660844574794 ) ) ;
#46503 = CARTESIAN_POINT ( 'NONE',  ( 174.1422537179814753, 73.24254491731250027, 7.110486902026410760 ) ) ;
#46504 = CARTESIAN_POINT ( 'NONE',  ( -31.11269837220806878, 5.000000000000056843, 85.00100000000000477 ) ) ;
#46505 = DIRECTION ( 'NONE',  ( -0.000000000000000000, -0.000000000000000000, -1.000000000000000000 ) ) ;
#46506 = CARTESIAN_POINT ( 'NONE',  ( 126.3580543567275356, 37.07735301062817967, 10.46969542368406536 ) ) ;
#46507 = VECTOR ( 'NONE', #3892, 1000.000000000000000 ) ;
#46508 = CARTESIAN_POINT ( 'NONE',  ( -156.9406434201984268, 70.74968524571472983, 12.52616388493933464 ) ) ;
#46509 = CARTESIAN_POINT ( 'NONE',  ( 25.09133896793783336, 1.250000000000021982, 3.061616997868437868E-16 ) ) ;
#46510 = EDGE_CURVE ( 'NONE', #5640, #65549, #39438, .T. ) ;
#46511 = AXIS2_PLACEMENT_3D ( 'NONE', #56791, #45885, #34657 ) ;
#46512 = CARTESIAN_POINT ( 'NONE',  ( 210.9608386442062624, 117.1762372255315938, 40.84185146199625649 ) ) ;
#46513 = CARTESIAN_POINT ( 'NONE',  ( -84.21836162213170951, 25.60181819557222838, 59.69698668375344397 ) ) ;
#46514 = DIRECTION ( 'NONE',  ( -0.000000000000000000, 1.000000000000000000, -0.000000000000000000 ) ) ;
#46515 = ORIENTED_EDGE ( 'NONE', *, *, #48997, .T. ) ;
#46516 = EDGE_CURVE ( 'NONE', #60552, #53918, #22914, .T. ) ;
#46518 = CONICAL_SURFACE ( 'NONE', #36480, 74.95140232871122521, 0.8777644062502172329 ) ;
#46517 = ITEM_DEFINED_TRANSFORMATION ( 'NONE', 'NONE', #6237,  #66832 ) ;
#46519 = CARTESIAN_POINT ( 'NONE',  ( 9.837735240994035735, 7.389327806910502616, -20.74626001938653630 ) ) ;
#46520 = ORIENTED_EDGE ( 'NONE', *, *, #29727, .T. ) ;
#46521 = CARTESIAN_POINT ( 'NONE',  ( 45.80999061969644970, 10.34829880103435507, 94.99999999999866418 ) ) ;
#46522 = ORIENTED_EDGE ( 'NONE', *, *, #8977, .F. ) ;
#46523 = CYLINDRICAL_SURFACE ( 'NONE', #68064, 5.000000000000000888 ) ;
#46524 = AXIS2_PLACEMENT_3D ( 'NONE', #49030, #16691, #37804 ) ;
#46525 = CARTESIAN_POINT ( 'NONE',  ( -142.8556048422595381, 60.01994222009837898, 68.54020186033872619 ) ) ;
#46526 = CARTESIAN_POINT ( 'NONE',  ( 37.76691715686636996, 29.79383981485516841, -24.99999999999999645 ) ) ;
#46527 = CARTESIAN_POINT ( 'NONE',  ( -29.03891846981456126, 10.22741474064058487, 3.749472614900290601 ) ) ;
#46528 = CARTESIAN_POINT ( 'NONE',  ( 149.0250918491436778, 0.000000000000000000, -9.435653166495526989 ) ) ;
#46529 = DIRECTION ( 'NONE',  ( 1.110223024625156294E-16, 3.697785493223491743E-32, -1.000000000000000000 ) ) ;
#46530 = CARTESIAN_POINT ( 'NONE',  ( -7.825402957745087207, -170.0000000000000000, -96.60717191287118055 ) ) ;
#46531 = VERTEX_POINT ( 'NONE', #55265 ) ;
#46532 = VERTEX_POINT ( 'NONE', #60891 ) ;
#46533 = EDGE_CURVE ( 'NONE', #18069, #21122, #51040, .T. ) ;
#46534 = CARTESIAN_POINT ( 'NONE',  ( -34.39099631177282390, 10.00000000000000000, -4.638432934570702075E-15 ) ) ;
#46535 = CARTESIAN_POINT ( 'NONE',  ( 0.000000000000000000, 0.000000000000000000, 0.000000000000000000 ) ) ;
#46536 = CARTESIAN_POINT ( 'NONE',  ( -30.46060138092288838, 9.432375387772216513, -62.20961696371778515 ) ) ;
#46537 = EDGE_CURVE ( 'NONE', #31926, #21875, #9806, .T. ) ;
#46538 = EDGE_CURVE ( 'NONE', #18591, #2403, #13176, .T. ) ;
#46539 = CARTESIAN_POINT ( 'NONE',  ( 11.21653854975268949, 6.397128675385708618, 16.63585048340505423 ) ) ;
#46540 = DIRECTION ( 'NONE',  ( 0.000000000000000000, 1.000000000000000000, 0.000000000000000000 ) ) ;
#46541 = CARTESIAN_POINT ( 'NONE',  ( 6.400000000000000355, 0.000000000000000000, 8.000000000000000000 ) ) ;
#46542 = CARTESIAN_POINT ( 'NONE',  ( 207.4610690199662315, 111.9701171077052209, 16.84735845215860905 ) ) ;
#46543 =( NAMED_UNIT ( * ) SI_UNIT ( $, .STERADIAN. ) SOLID_ANGLE_UNIT ( ) );
#46544 = CARTESIAN_POINT ( 'NONE',  ( -179.6470915626257465, 94.69856161161348496, -45.91846509321587178 ) ) ;
#46545 = CARTESIAN_POINT ( 'NONE',  ( 89.88695630745283438, 20.55793566325394650, -9.704490825940514043 ) ) ;
#46546 = CARTESIAN_POINT ( 'NONE',  ( -26.50207385662994497, 9.849226639603646305, 58.89342097685724298 ) ) ;
#46547 = CYLINDRICAL_SURFACE ( 'NONE', #62137, 7.500000000000020428 ) ;
#46548 = CARTESIAN_POINT ( 'NONE',  ( -50.51700111023803430, 13.51182830536854595, 70.65495365061850919 ) ) ;
#46549 = VECTOR ( 'NONE', #47694, 1000.000000000000000 ) ;
#46550 = CARTESIAN_POINT ( 'NONE',  ( -0.7215816834507520205, 6.532459459468099361, 62.04215831576383522 ) ) ;
#46551 = EDGE_LOOP ( 'NONE', ( #38177, #60608, #6699, #23141 ) ) ;
#46552 = PLANE ( 'NONE',  #10295 ) ;
#46553 = CARTESIAN_POINT ( 'NONE',  ( 151.1827182658834090, 54.16800928478853194, 59.63366074271394979 ) ) ;
#46554 = CARTESIAN_POINT ( 'NONE',  ( -108.0902552660050446, 36.97681740369920078, -74.12781022651168428 ) ) ;
#46555 = CARTESIAN_POINT ( 'NONE',  ( -48.57297291660696459, 13.03920345822338689, -46.52532158187338496 ) ) ;
#46556 = CARTESIAN_POINT ( 'NONE',  ( 112.3013380801408658, 388.0000000000065370, 91.05029585798857283 ) ) ;
#46557 = FACE_OUTER_BOUND ( 'NONE', #66264, .T. ) ;
#46558 = AXIS2_PLACEMENT_3D ( 'NONE', #2355, #45599, #65060 ) ;
#46559 = ORIENTED_EDGE ( 'NONE', *, *, #19324, .F. ) ;
#46560 = VECTOR ( 'NONE', #26978, 1000.000000000000000 ) ;
#46561 = EDGE_CURVE ( 'NONE', #21979, #43731, #28541, .T. ) ;
#46562 = CARTESIAN_POINT ( 'NONE',  ( -190.0608188262619365, 108.2310236786209146, -92.36485475830178871 ) ) ;
#46563 = PLANE ( 'NONE',  #34982 ) ;
#46564 = ORIENTED_EDGE ( 'NONE', *, *, #14775, .T. ) ;
#46565 = EDGE_LOOP ( 'NONE', ( #48530, #29156, #41063, #42636 ) ) ;
#46566 = VECTOR ( 'NONE', #53213, 1000.000000000000000 ) ;
#46567 = CARTESIAN_POINT ( 'NONE',  ( 181.0840389613909736, 78.60582251573005408, -51.22505766587963905 ) ) ;
#46568 = DIRECTION ( 'NONE',  ( -0.7530714660036099684, -0.6579387259397138088, 0.000000000000000000 ) ) ;
#46569 = CARTESIAN_POINT ( 'NONE',  ( 8.000000000000007105, 249.8719672152120381, -95.00000000000133582 ) ) ;
#46570 = ORIENTED_EDGE ( 'NONE', *, *, #29371, .F. ) ;
#46571 = FACE_OUTER_BOUND ( 'NONE', #3221, .T. ) ;
#46572 = CARTESIAN_POINT ( 'NONE',  ( -55.54058841405665703, 14.81234591756537888, -62.06087458892353936 ) ) ;
#46573 = CARTESIAN_POINT ( 'NONE',  ( 50.59696802070018151, -10.45241205790868477, 26.66469104408688295 ) ) ;
#46574 = CARTESIAN_POINT ( 'NONE',  ( 56.94505604581134861, 12.37336791557970095, -47.63195170334665818 ) ) ;
#46575 = CARTESIAN_POINT ( 'NONE',  ( -85.35172689181703731, 26.07142112926218758, 34.48212782639603802 ) ) ;
#46576 = CARTESIAN_POINT ( 'NONE',  ( -25.07735481787161191, 9.648965052008778187, -19.95240735271818622 ) ) ;
#46577 = CARTESIAN_POINT ( 'NONE',  ( 133.8566784816069628, 41.42467568809806977, 17.66579024853170310 ) ) ;
#46578 = ORIENTED_EDGE ( 'NONE', *, *, #9301, .T. ) ;
#46579 =( NAMED_UNIT ( * ) PLANE_ANGLE_UNIT ( ) SI_UNIT ( $, .RADIAN. ) );
#46580 = CARTESIAN_POINT ( 'NONE',  ( 8.670103207226933506, 6.377073801252349128, 61.94615088279628878 ) ) ;
#46581 = CARTESIAN_POINT ( 'NONE',  ( 200.4590013143046576, 102.3556155835303088, 30.50310333978841726 ) ) ;
#46582 = CARTESIAN_POINT ( 'NONE',  ( -74.59410384915268821, 21.88130278302777754, 85.27819964176909195 ) ) ;
#46584 = VERTEX_POINT ( 'NONE', #23277 ) ;
#46583 = LINE ( 'NONE', #24113, #18612 ) ;
#46585 = CARTESIAN_POINT ( 'NONE',  ( 49.99999999999998579, 19.99999999999996447, 1.999999999999984457 ) ) ;
#46586 = ORIENTED_EDGE ( 'NONE', *, *, #10230, .T. ) ;
#46587 = ADVANCED_FACE ( 'NONE', ( #34870 ), #18330, .F. ) ;
#46588 = ORIENTED_EDGE ( 'NONE', *, *, #64406, .F. ) ;
#46589 = CARTESIAN_POINT ( 'NONE',  ( -145.3109762780891288, 60.69959559383374170, 71.29862809856072658 ) ) ;
#46590 = FACE_OUTER_BOUND ( 'NONE', #6206, .T. ) ;
#46591 = PLANE ( 'NONE',  #30996 ) ;
#46592 = LINE ( 'NONE', #30088, #42888 ) ;
#46593 = EDGE_CURVE ( 'NONE', #21766, #17523, #30222, .T. ) ;
#46594 = CARTESIAN_POINT ( 'NONE',  ( -121.1775535805057160, 43.46577565517554831, 70.81645009186183870 ) ) ;
#46595 = DIRECTION ( 'NONE',  ( 1.000000000000000000, 0.000000000000000000, -0.000000000000000000 ) ) ;
#46596 = CARTESIAN_POINT ( 'NONE',  ( 23.09119322872580682, 7.852465917941087170, -95.00000000000133582 ) ) ;
#46597 = CIRCLE ( 'NONE', #55583, 5.000000000000000888 ) ;
#46598 = EDGE_CURVE ( 'NONE', #44052, #41887, #67969, .T. ) ;
#46599 = LINE ( 'NONE', #13903, #50905 ) ;
#46600 = EDGE_LOOP ( 'NONE', ( #54914, #12204, #67980, #40630 ) ) ;
#46601 = EDGE_LOOP ( 'NONE', ( #39473, #16835, #33351, #5117 ) ) ;
#46602 = CARTESIAN_POINT ( 'NONE',  ( -109.0291978193666722, 37.49173305805087608, 7.893610283594471255 ) ) ;
#46603 = CIRCLE ( 'NONE', #45502, 74.99999999999998579 ) ;
#46604 = EDGE_CURVE ( 'NONE', #6351, #28945, #30282, .T. ) ;
#46605 = CARTESIAN_POINT ( 'NONE',  ( 105.8203563788590742, 26.88901185006200123, 70.01787404090897837 ) ) ;
#46606 = CARTESIAN_POINT ( 'NONE',  ( 111.8863762173178316, 29.64954938250774674, 83.47565785988531673 ) ) ;
#46607 = CARTESIAN_POINT ( 'NONE',  ( -189.2346268516247108, 107.0830361517164846, 65.47910114476307797 ) ) ;
#46608 = AXIS2_PLACEMENT_3D ( 'NONE', #920, #20049, #15794 ) ;
#46609 = AXIS2_PLACEMENT_3D ( 'NONE', #11063, #69461, #26217 ) ;
#46610 = CARTESIAN_POINT ( 'NONE',  ( 181.5072453427590915, 79.03352099595188918, -51.22505766587964615 ) ) ;
#46611 = CARTESIAN_POINT ( 'NONE',  ( 110.2429982417149574, -170.0000000000000000, -16.57788697519001175 ) ) ;
#46612 = VECTOR ( 'NONE', #50265, 1000.000000000000000 ) ;
#46613 = CARTESIAN_POINT ( 'NONE',  ( -142.3799050480288031, 59.64294364584055330, 89.55052947415697417 ) ) ;
#46614 = ORIENTED_EDGE ( 'NONE', *, *, #29230, .F. ) ;
#46615 = EDGE_LOOP ( 'NONE', ( #36043, #28915 ) ) ;
#46616 = VECTOR ( 'NONE', #64485, 1000.000000000000000 ) ;
#46617 = ORIENTED_EDGE ( 'NONE', *, *, #52976, .F. ) ;
#46618 = AXIS2_PLACEMENT_3D ( 'NONE', #57155, #30415, #41322 ) ;
#46619 = DIRECTION ( 'NONE',  ( 1.000000000000000000, 0.000000000000000000, 0.000000000000000000 ) ) ;
#46620 = CARTESIAN_POINT ( 'NONE',  ( 24.17157287525367693, 0.000000000000000000, 2.000000000000001776 ) ) ;
#46621 = EDGE_CURVE ( 'NONE', #66651, #62757, #63324, .T. ) ;
#46622 = CARTESIAN_POINT ( 'NONE',  ( 65.40032188136233060, 13.23841673691966925, -50.33562451376164404 ) ) ;
#46623 = CARTESIAN_POINT ( 'NONE',  ( 107.7840330814956786, -21.53650026154319264, 4.493931093091683593 ) ) ;
#46624 = CARTESIAN_POINT ( 'NONE',  ( -62.50103539982530521, 17.85731685071834107, 36.80643099207888724 ) ) ;
#46625 = CARTESIAN_POINT ( 'NONE',  ( -38.93938005333175312, 11.96888249046461361, -69.42206000664089061 ) ) ;
#46626 = CARTESIAN_POINT ( 'NONE',  ( 34.83825437341839404, 7.859462995505743343, 58.28670175242805129 ) ) ;
#46627 = CARTESIAN_POINT ( 'NONE',  ( 45.76539630260660374, 9.322640236743859887, 87.11983195816242187 ) ) ;
#46628 =( LENGTH_UNIT ( ) NAMED_UNIT ( * ) SI_UNIT ( .MILLI., .METRE. ) );
#46629 = B_SPLINE_CURVE_WITH_KNOTS ( 'NONE', 3,
 ( #34393, #40679, #35414, #18544 ),
 .UNSPECIFIED., .F., .F.,
 ( 4, 4 ),
 ( 0.1259919275528356697, 0.1829744153748743274 ),
 .UNSPECIFIED. ) ;
#46630 = EDGE_LOOP ( 'NONE', ( #35265, #3006, #13227, #64368 ) ) ;
#46631 = CARTESIAN_POINT ( 'NONE',  ( 0.000000000000000000, 0.000000000000000000, 41.38025477438755928 ) ) ;
#46632 = CARTESIAN_POINT ( 'NONE',  ( 188.2950202724320832, 86.21411212788221690, 61.57030577803965343 ) ) ;
#46633 = CARTESIAN_POINT ( 'NONE',  ( -124.3250225421926132, 45.46958056770283463, 18.61297921365314778 ) ) ;
#46634 = CARTESIAN_POINT ( 'NONE',  ( 68.63487067129267416, 14.04635751989140147, -65.07391997778475456 ) ) ;
#46635 = CARTESIAN_POINT ( 'NONE',  ( 15.78827728214693416, 6.500811158483284835, 56.85925826316891829 ) ) ;
#46636 = DIRECTION ( 'NONE',  ( -1.000000000000000000, 0.000000000000000000, 0.000000000000000000 ) ) ;
#46637 = CARTESIAN_POINT ( 'NONE',  ( 204.6977192012829789, 106.3443248447423599, 56.05227132923312183 ) ) ;
#46638 = ORIENTED_EDGE ( 'NONE', *, *, #56377, .F. ) ;
#46639 = CARTESIAN_POINT ( 'NONE',  ( 187.9007786055418592, 85.78077355327279463, 13.10349074316396489 ) ) ;
#46640 = PRODUCT_CONTEXT ( 'NONE', #48895, 'mechanical' ) ;
#46641 = CARTESIAN_POINT ( 'NONE',  ( 130.7457207912711112, 40.74300766298684806, -50.36327218344248280 ) ) ;
#46642 = CARTESIAN_POINT ( 'NONE',  ( -127.6861178856153742, 47.68458428355324941, -35.11711282288931812 ) ) ;
#46643 = B_SPLINE_CURVE_WITH_KNOTS ( 'NONE', 3,
 ( #19449, #31400, #9944, #46180, #14184, #9250, #52831, #68004, #47213, #52157, #19809, #47548, #20148, #67653, #62720, #35984, #46883, #63411, #40913, #58128, #4653, #4324, #56748, #19105, #40559, #41600, #3287, #57439, #57783, #9598, #41947, #35644, #41265, #25787, #3620, #20483, #24745, #62011, #62369, #25444, #30707, #13829, #8567, #57094, #8911 ),
 .UNSPECIFIED., .F., .F.,
 ( 4, 2, 2, 2, 2, 2, 2, 2, 1, 2, 2, 2, 2, 2, 2, 2, 2, 2, 2, 2, 2, 2, 4 ),
 ( 0.000000000000000000, 0.001470449819620675991, 0.002205674729431024612, 0.002940899639241372800, 0.004411349458862050092, 0.005881799278482727385, 0.007352249098103403810, 0.008087474007913734650, 0.008822698917724065490, 0.009557923827534394595, 0.01029314873734472544, 0.01176359855696536630, 0.01249882346677567459, 0.01323404837658598461, 0.01470449819620660813, 0.01543972310601693203, 0.01617494801582725766, 0.01764539783544792628, 0.01911584765506859490, 0.01985107256487891880, 0.02058629747468924617, 0.02205674729430990091, 0.02352719711393055912 ),
 .UNSPECIFIED. ) ;
#46644 = CARTESIAN_POINT ( 'NONE',  ( -104.5740066103012822, 35.09687312794777370, -49.65903324600630953 ) ) ;
#46645 = CARTESIAN_POINT ( 'NONE',  ( 184.5867277229703518, 83.68414666546578928, -37.08944934118979830 ) ) ;
#46646 = VERTEX_POINT ( 'NONE', #35204 ) ;
#46647 = EDGE_LOOP ( 'NONE', ( #40955, #42621, #44249, #2773 ) ) ;
#46648 = CARTESIAN_POINT ( 'NONE',  ( -147.7845268487069461, 62.73119438705056439, -8.155966956317975303 ) ) ;
#46649 = LINE ( 'NONE', #20265, #30456 ) ;
#46650 = ORIENTED_EDGE ( 'NONE', *, *, #62017, .F. ) ;
#46651 = VECTOR ( 'NONE', #30521, 1000.000000000000000 ) ;
#46652 = CARTESIAN_POINT ( 'NONE',  ( 163.4829520545006289, 63.79049927423832855, 86.10267534221468111 ) ) ;
#46653 = ORIENTED_EDGE ( 'NONE', *, *, #18122, .T. ) ;
#46654 = CARTESIAN_POINT ( 'NONE',  ( -62.55320287144887459, 17.87319849854529608, 11.21034754316474746 ) ) ;
#46655 = CARTESIAN_POINT ( 'NONE',  ( 129.1381264900934411, 38.64720302602604107, 42.86026151076471535 ) ) ;
#46656 = VECTOR ( 'NONE', #3616, 1000.000000000000000 ) ;
#46657 = CARTESIAN_POINT ( 'NONE',  ( -152.9008427825210674, 68.45483453645054794, 31.52859718944691636 ) ) ;
#46658 = LINE ( 'NONE', #8699, #21387 ) ;
#46659 = VECTOR ( 'NONE', #39317, 1000.000000000000000 ) ;
#46661 = CARTESIAN_POINT ( 'NONE',  ( -102.2801239173131194, -170.0000000000000000, -96.20367844590329298 ) ) ;
#46660 = AXIS2_PLACEMENT_3D ( 'NONE', #173, #43769, #11771 ) ;
#46663 = EDGE_LOOP ( 'NONE', ( #15099, #57461, #5308, #4833 ) ) ;
#46662 = CARTESIAN_POINT ( 'NONE',  ( 10.00000000000000000, 1.224646799147353256E-15, 2.000000000000001776 ) ) ;
#46664 = PLANE ( 'NONE',  #38443 ) ;
#46665 = AXIS2_PLACEMENT_3D ( 'NONE', #35006, #35353, #19511 ) ;
#46666 = ORIENTED_EDGE ( 'NONE', *, *, #41457, .T. ) ;
#46667 = ORIENTED_EDGE ( 'NONE', *, *, #11749, .F. ) ;
#46668 = CARTESIAN_POINT ( 'NONE',  ( -171.0950923142954139, 86.38958441093225815, 4.243329981061625844 ) ) ;
#46669 = VECTOR ( 'NONE', #38455, 1000.000000000000000 ) ;
#46670 = APPLICATION_CONTEXT ( 'automotive_design' ) ;
#46671 = CARTESIAN_POINT ( 'NONE',  ( -33.12934624031570507, 10.89552623243536900, -89.18697688497687182 ) ) ;
#46673 = ORIENTED_EDGE ( 'NONE', *, *, #54127, .F. ) ;
#46672 = CARTESIAN_POINT ( 'NONE',  ( -133.1640943168119122, 52.70734926280008636, 66.82601452699702804 ) ) ;
#46674 = CARTESIAN_POINT ( 'NONE',  ( -109.7346721907204028, 37.88203613721440632, 90.81995025446376246 ) ) ;
#46675 = DIRECTION ( 'NONE',  ( -1.000000000000000000, 0.000000000000000000, 0.000000000000000000 ) ) ;
#46676 = ORIENTED_EDGE ( 'NONE', *, *, #9399, .F. ) ;
#46677 = CARTESIAN_POINT ( 'NONE',  ( -56.96214175905168275, 15.20165595797839408, -8.614853995199030834 ) ) ;
#46678 = EDGE_CURVE ( 'NONE', #42865, #2737, #57355, .T. ) ;
#46679 = CARTESIAN_POINT ( 'NONE',  ( -129.3970594949620079, 50.06339481638098476, -75.90617434883772319 ) ) ;
#46680 = CARTESIAN_POINT ( 'NONE',  ( 117.3145357257065342, 33.41973663092564095, 39.66135912721455981 ) ) ;
#46681 = FACE_BOUND ( 'NONE', #15924, .T. ) ;
#46682 = CARTESIAN_POINT ( 'NONE',  ( 65.39792658623289867, 14.27332852928128126, -62.94950063402156104 ) ) ;
#46683 = VERTEX_POINT ( 'NONE', #35901 ) ;
#46684 = ORIENTED_EDGE ( 'NONE', *, *, #38763, .F. ) ;
#46685 = EDGE_CURVE ( 'NONE', #44375, #63280, #10881, .T. ) ;
#46686 = LINE ( 'NONE', #67139, #2361 ) ;
#46687 = CARTESIAN_POINT ( 'NONE',  ( 68.07999999999999829, -36.09918303830819752, 30.00000000000000000 ) ) ;
#46688 = FACE_BOUND ( 'NONE', #68032, .T. ) ;
#46689 = LINE ( 'NONE', #25604, #65902 ) ;
#46690 = CARTESIAN_POINT ( 'NONE',  ( -47.68562151781910785, 13.86286849776707797, -95.00000000000133582 ) ) ;
#46691 = DIRECTION ( 'NONE',  ( -0.000000000000000000, -0.000000000000000000, 1.000000000000000000 ) ) ;
#46692 = CARTESIAN_POINT ( 'NONE',  ( 0.7145311798163209716, 4.618802153517001408, -8.000000000000000000 ) ) ;
#46693 = LINE ( 'NONE', #19977, #63199 ) ;
#46694 = CARTESIAN_POINT ( 'NONE',  ( 211.0967808702090736, 115.5516932918876876, 59.63059121463253121 ) ) ;
#46695 = ORIENTED_EDGE ( 'NONE', *, *, #40363, .F. ) ;
#46696 = CARTESIAN_POINT ( 'NONE',  ( -108.9444157621018405, 37.44493815491210853, 41.49818020471239777 ) ) ;
#46697 = ORIENTED_EDGE ( 'NONE', *, *, #10246, .T. ) ;
#46698 = AXIS2_PLACEMENT_3D ( 'NONE', #68410, #25163, #30777 ) ;
#46699 = CARTESIAN_POINT ( 'NONE',  ( -180.3451190839052458, 95.54664796532459548, -93.86486230744075954 ) ) ;
#46700 = CARTESIAN_POINT ( 'NONE',  ( 84.72546926745364715, 19.84015517905186243, 71.32696357878030824 ) ) ;
#46701 = ORIENTED_EDGE ( 'NONE', *, *, #60091, .T. ) ;
#46702 = DIRECTION ( 'NONE',  ( 0.000000000000000000, 0.000000000000000000, 1.000000000000000000 ) ) ;
#46703 = EDGE_CURVE ( 'NONE', #30998, #68286, #5935, .T. ) ;
#46704 = DIRECTION ( 'NONE',  ( 0.000000000000000000, 0.000000000000000000, 1.000000000000000000 ) ) ;
#46705 = CARTESIAN_POINT ( 'NONE',  ( 37.46876540261052924, 9.179568636624020783, 3.318579510039644909 ) ) ;
#46707 = FACE_OUTER_BOUND ( 'NONE', #14020, .T. ) ;
#46706 = VECTOR ( 'NONE', #28538, 1000.000000000000114 ) ;
#46708 = CARTESIAN_POINT ( 'NONE',  ( 32.90953848114694580, 7.653665824624198422, 6.806373642810018332 ) ) ;
#46709 = CARTESIAN_POINT ( 'NONE',  ( -13.29455179262033404, 8.319166883236668752, -48.05598062864418551 ) ) ;
#46710 = CARTESIAN_POINT ( 'NONE',  ( -33.83721310978700814, 11.01869210665939036, -23.08310314977254052 ) ) ;
#46711 = AXIS2_PLACEMENT_3D ( 'NONE', #22672, #56078, #60656 ) ;
#46712 = AXIS2_PLACEMENT_3D ( 'NONE', #45873, #29694, #24433 ) ;
#46713 = VERTEX_POINT ( 'NONE', #42874 ) ;
#46714 = CARTESIAN_POINT ( 'NONE',  ( -125.8938041572051105, 47.69968343338781125, -88.60280507916129977 ) ) ;
#46715 = ORIENTED_EDGE ( 'NONE', *, *, #65101, .T. ) ;
#46716 = CARTESIAN_POINT ( 'NONE',  ( -61.39252081892701796, 16.47343302442957835, 33.80259966407439265 ) ) ;
#46717 = CARTESIAN_POINT ( 'NONE',  ( 11.82929895397812992, 7.412564870773605818, -76.23824787671220804 ) ) ;
#46718 = CARTESIAN_POINT ( 'NONE',  ( -24.93568128341082968, 8.613819379861695325, 14.63976890511303885 ) ) ;
#46719 = CARTESIAN_POINT ( 'NONE',  ( 412.3372781065086201, 400.0000000000000568, -146.4497041420118251 ) ) ;
#46720 = AXIS2_PLACEMENT_3D ( 'NONE', #7845, #50746, #24022 ) ;
#46721 = CARTESIAN_POINT ( 'NONE',  ( -14.76369756425704161, 7.442560416198670481, -66.88354962501738044 ) ) ;
#46722 = CARTESIAN_POINT ( 'NONE',  ( -94.85061234775061223, 29.16417548023185091, -16.72803334679694487 ) ) ;
#46723 = CARTESIAN_POINT ( 'NONE',  ( 92.91022130985207639, 22.73448145304546131, 94.99999999999866418 ) ) ;
#46724 = VECTOR ( 'NONE', #65832, 1000.000000000000000 ) ;
#46725 = EDGE_LOOP ( 'NONE', ( #64874, #23040, #32352, #64304 ) ) ;
#46726 = DIRECTION ( 'NONE',  ( -0.9999999288524208385, -0.0003772202979824376039, -2.172978322886182090E-16 ) ) ;
#46727 = CARTESIAN_POINT ( 'NONE',  ( -32.53122335971237788, -7.681316725934842715, 6.893343212288939093 ) ) ;
#46728 = CARTESIAN_POINT ( 'NONE',  ( 174.6242782760049863, 73.69713439533575183, -13.06059959078580412 ) ) ;
#46729 = CARTESIAN_POINT ( 'NONE',  ( -118.8504142000305421, 42.02789424825277109, 40.71051564713940962 ) ) ;
#46730 = LINE ( 'NONE', #63263, #718 ) ;
#46731 = VERTEX_POINT ( 'NONE', #21432 ) ;
#46732 = CARTESIAN_POINT ( 'NONE',  ( -178.2448732545370831, 94.58403736950704399, -63.55990931418686785 ) ) ;
#46733 = CARTESIAN_POINT ( 'NONE',  ( 127.3286037854883830, 38.77506637992906491, 94.40897935295708976 ) ) ;
#46734 = CARTESIAN_POINT ( 'NONE',  ( 201.4634861300068565, 103.6729577544787162, -90.70809642864092837 ) ) ;
#46735 = DIRECTION ( 'NONE',  ( 0.000000000000000000, 0.000000000000000000, -1.000000000000000000 ) ) ;
#46736 = CARTESIAN_POINT ( 'NONE',  ( -118.4063383664800142, 41.75753822095642676, -68.74786715921418079 ) ) ;
#46737 = ORIENTED_EDGE ( 'NONE', *, *, #62259, .F. ) ;
#46738 = DIRECTION ( 'NONE',  ( -0.000000000000000000, 1.000000000000000000, -0.000000000000000000 ) ) ;
#46739 = CARTESIAN_POINT ( 'NONE',  ( 117.4830770399667870, 32.37795270233553424, -68.24308158718707773 ) ) ;
#46740 = CARTESIAN_POINT ( 'NONE',  ( 186.2680729609085120, 85.48839327635674579, 31.36819915828147742 ) ) ;
#46741 = CARTESIAN_POINT ( 'NONE',  ( 187.5166849924263204, 85.36068406478833026, -93.55154100713149035 ) ) ;
#46742 = CARTESIAN_POINT ( 'NONE',  ( 0.000000000000000000, 0.000000000000000000, 0.000000000000000000 ) ) ;
#46743 = VERTEX_POINT ( 'NONE', #47819 ) ;
#46744 = ADVANCED_FACE ( 'NONE', ( #20750 ), #5595, .F. ) ;
#46745 = CARTESIAN_POINT ( 'NONE',  ( 175.5498284945444709, 74.57669191966282085, 58.56542896661724029 ) ) ;
#46746 = ORIENTED_EDGE ( 'NONE', *, *, #58200, .T. ) ;
#46747 = EDGE_CURVE ( 'NONE', #48407, #28889, #7556, .T. ) ;
#46748 = VECTOR ( 'NONE', #46162, 1000.000000000000000 ) ;
#46749 = DIRECTION ( 'NONE',  ( 0.000000000000000000, 0.000000000000000000, -1.000000000000000000 ) ) ;
#46750 = CARTESIAN_POINT ( 'NONE',  ( 141.0679329045600809, 45.95256892154834816, 92.79094832732447173 ) ) ;
#46751 = AXIS2_PLACEMENT_3D ( 'NONE', #59740, #33031, #60098 ) ;
#46753 = ORIENTED_EDGE ( 'NONE', *, *, #46345, .T. ) ;
#46752 = CARTESIAN_POINT ( 'NONE',  ( 157.4703587214989113, 58.92748579479258808, 2.564916881789689462 ) ) ;
#46754 = CARTESIAN_POINT ( 'NONE',  ( -179.0654441437004891, 93.99779465816536117, 33.74156010598665745 ) ) ;
#46755 = DIRECTION ( 'NONE',  ( -0.000000000000000000, -0.000000000000000000, -1.000000000000000000 ) ) ;
#46756 = CARTESIAN_POINT ( 'NONE',  ( 115.0606351894211485, 32.29586232625066344, -49.19153966712070059 ) ) ;
#46757 = AXIS2_PLACEMENT_3D ( 'NONE', #25805, #47235, #53881 ) ;
#46758 = AXIS2_PLACEMENT_3D ( 'NONE', #42909, #11252, #37292 ) ;
#46759 = ORIENTED_EDGE ( 'NONE', *, *, #25989, .F. ) ;
#46760 = DIRECTION ( 'NONE',  ( 0.6427876096865403621, -0.7660444431189770143, 1.393823445737823288E-16 ) ) ;
#46761 = EDGE_CURVE ( 'NONE', #68971, #2402, #22141, .T. ) ;
#46762 = VECTOR ( 'NONE', #46867, 1000.000000000000000 ) ;
#46763 = EDGE_CURVE ( 'NONE', #58078, #53458, #19897, .T. ) ;
#46764 = CARTESIAN_POINT ( 'NONE',  ( -132.8123438040339863, 51.22132183644641401, 41.02731276053570753 ) ) ;
#46765 = PLANE ( 'NONE',  #38829 ) ;
#46766 = AXIS2_PLACEMENT_3D ( 'NONE', #39113, #55267, #44726 ) ;
#46767 = DIRECTION ( 'NONE',  ( -0.8090169943749422332, -0.5877852522924802425, 0.000000000000000000 ) ) ;
#46768 = CARTESIAN_POINT ( 'NONE',  ( -169.1041038606267080, 82.76530082651281361, 31.97253426586447844 ) ) ;
#46769 = CARTESIAN_POINT ( 'NONE',  ( 150.4544126017351005, 52.39556706174411715, 61.08955027113243119 ) ) ;
#46770 = LINE ( 'NONE', #14423, #2395 ) ;
#46771 = ORIENTED_EDGE ( 'NONE', *, *, #58535, .T. ) ;
#46772 = CARTESIAN_POINT ( 'NONE',  ( -102.2801239173131052, 33.91021738430207222, 72.36362509687883460 ) ) ;
#46773 = DIRECTION ( 'NONE',  ( -0.000000000000000000, 1.000000000000000000, -0.000000000000000000 ) ) ;
#46774 = ORIENTED_EDGE ( 'NONE', *, *, #20668, .T. ) ;
#46775 = ADVANCED_FACE ( 'NONE', ( #64342 ), #4915, .T. ) ;
#46776 = CARTESIAN_POINT ( 'NONE',  ( 151.8005253678161921, 54.62151558044535449, -21.71570063336847412 ) ) ;
#46777 = CARTESIAN_POINT ( 'NONE',  ( -51.16680845348332696, 13.67385610796032402, 85.08383212419218466 ) ) ;
#46778 = CARTESIAN_POINT ( 'NONE',  ( 105.8229724512850964, 27.98935528750252288, 31.04713432260220429 ) ) ;
#46779 = LINE ( 'NONE', #2838, #26513 ) ;
#46780 = CARTESIAN_POINT ( 'NONE',  ( 55.74003717006368674, 11.10204531284817264, 92.85377417485183571 ) ) ;
#46781 = CARTESIAN_POINT ( 'NONE',  ( 185.1660960081723886, 84.30194217633003007, 3.668103655852483325 ) ) ;
#46782 = CARTESIAN_POINT ( 'NONE',  ( 210.5178985598940926, 114.6803933586780886, -39.08928032852175960 ) ) ;
#46783 = CARTESIAN_POINT ( 'NONE',  ( 179.4207200232660568, 76.93724985992177778, 17.32800239155928068 ) ) ;
#46784 = ORIENTED_EDGE ( 'NONE', *, *, #2884, .F. ) ;
#46785 = CARTESIAN_POINT ( 'NONE',  ( 133.8566784816069344, -170.0000000000000000, 90.69944201992272781 ) ) ;
#46786 = ORIENTED_EDGE ( 'NONE', *, *, #54208, .T. ) ;
#46787 = CARTESIAN_POINT ( 'NONE',  ( -71.26746920569851795, 20.70422440535243069, 63.50986984570365479 ) ) ;
#46788 = EDGE_CURVE ( 'NONE', #42318, #6225, #11217, .T. ) ;
#46789 = CARTESIAN_POINT ( 'NONE',  ( 58.09436971064712907, 11.58462396079456802, -64.38444416366542100 ) ) ;
#46790 = DIRECTION ( 'NONE',  ( 0.000000000000000000, 0.000000000000000000, 1.000000000000000000 ) ) ;
#46791 = CARTESIAN_POINT ( 'NONE',  ( 429.8372781065087338, 400.0000000000066507, 96.05029585798857283 ) ) ;
#46792 = CARTESIAN_POINT ( 'NONE',  ( -12.63247621924076114, 7.251801145016834482, 85.53860919323375356 ) ) ;
#46793 = EDGE_CURVE ( 'NONE', #36510, #46532, #57133, .T. ) ;
#46794 = EDGE_CURVE ( 'NONE', #32375, #51688, #60101, .T. ) ;
#46795 = EDGE_CURVE ( 'NONE', #48827, #64204, #49540, .T. ) ;
#46796 = CARTESIAN_POINT ( 'NONE',  ( -109.5157885508426716, 37.76058765671429995, -13.62891770046948636 ) ) ;
#46797 = ORIENTED_EDGE ( 'NONE', *, *, #23109, .F. ) ;
#46798 = CARTESIAN_POINT ( 'NONE',  ( -78.18913509716429644, 22.13995206110505265, 72.26275173013681297 ) ) ;
#46799 = CARTESIAN_POINT ( 'NONE',  ( -171.0758681675585251, 84.87997360100519018, 72.39440660477549727 ) ) ;
#46800 = ORIENTED_EDGE ( 'NONE', *, *, #64965, .F. ) ;
#46801 = EDGE_LOOP ( 'NONE', ( #11001, #51528 ) ) ;
#46802 = CARTESIAN_POINT ( 'NONE',  ( -8.000000000000001776, 0.000000000000000000, 0.000000000000000000 ) ) ;
#46803 = FACE_OUTER_BOUND ( 'NONE', #40864, .T. ) ;
#46804 = CARTESIAN_POINT ( 'NONE',  ( 178.1903523079566583, 75.72906488635184985, -23.81340345046014306 ) ) ;
#46805 = VECTOR ( 'NONE', #69264, 1000.000000000000000 ) ;
#46806 = FACE_OUTER_BOUND ( 'NONE', #17093, .T. ) ;
#46807 = CARTESIAN_POINT ( 'NONE',  ( -417.6627218934917778, 400.0000000000064801, -111.4497041420121661 ) ) ;
#46808 = AXIS2_PLACEMENT_3D ( 'NONE', #8764, #51324, #14023 ) ;
#46809 = ORIENTED_EDGE ( 'NONE', *, *, #13966, .F. ) ;
#46810 = CARTESIAN_POINT ( 'NONE',  ( -5.000000000000000000, 5.000000000000000000, 2.000000000000001776 ) ) ;
#46811 = AXIS2_PLACEMENT_3D ( 'NONE', #30534, #24916, #3800 ) ;
#46812 = EDGE_LOOP ( 'NONE', ( #26602, #13290, #24696, #65911 ) ) ;
#46813 = CARTESIAN_POINT ( 'NONE',  ( 212.1535111375854683, 117.1635556319084657, 10.69408520456943990 ) ) ;
#46814 = CARTESIAN_POINT ( 'NONE',  ( 8.767814708128303991, 7.383611927972574485, 61.70909310710061391 ) ) ;
#46815 =( LENGTH_UNIT ( ) NAMED_UNIT ( * ) SI_UNIT ( .MILLI., .METRE. ) );
#46816 = LINE ( 'NONE', #68284, #20553 ) ;
#46817 = ORIENTED_EDGE ( 'NONE', *, *, #20893, .T. ) ;
#46818 = AXIS2_PLACEMENT_3D ( 'NONE', #21077, #15786, #26693 ) ;
#46819 = ORIENTED_EDGE ( 'NONE', *, *, #276, .F. ) ;
#46820 = ORIENTED_EDGE ( 'NONE', *, *, #54768, .F. ) ;
#46821 = DIRECTION ( 'NONE',  ( 0.000000000000000000, 0.000000000000000000, 1.000000000000000000 ) ) ;
#46822 = CARTESIAN_POINT ( 'NONE',  ( 65.02478361689782105, -37.39438481343979959, 170.0000000000000000 ) ) ;
#46823 = CARTESIAN_POINT ( 'NONE',  ( -166.9969673948021125, 80.56076768517786491, -11.02977705128494357 ) ) ;
#46824 = CARTESIAN_POINT ( 'NONE',  ( -173.1211646369891071, 88.63826465341152527, 18.97714401617737323 ) ) ;
#46825 = CARTESIAN_POINT ( 'NONE',  ( 23.20798354347975589, 6.851551394716612897, 89.92625127541417385 ) ) ;
#46826 = DIRECTION ( 'NONE',  ( 1.020422603260505347E-14, -1.000000000000000000, -5.551115123125782702E-17 ) ) ;
#46827 = ORIENTED_EDGE ( 'NONE', *, *, #42167, .F. ) ;
#46828 = CARTESIAN_POINT ( 'NONE',  ( 4.165045035621076863, -64.88046627338039229, 170.0000000000000000 ) ) ;
#46829 = CARTESIAN_POINT ( 'NONE',  ( -100.4262673593280368, 31.84860241619272969, 72.14605430199947023 ) ) ;
#46830 = EDGE_LOOP ( 'NONE', ( #3028, #67417, #63440, #11729 ) ) ;
#46831 = CARTESIAN_POINT ( 'NONE',  ( -85.34215807311491631, 24.97769003780923569, 14.50119405095866831 ) ) ;
#46832 = VERTEX_POINT ( 'NONE', #17550 ) ;
#46833 = EDGE_CURVE ( 'NONE', #49487, #58090, #49899, .T. ) ;
#46834 = LINE ( 'NONE', #20437, #27620 ) ;
#46835 = EDGE_LOOP ( 'NONE', ( #5299, #56334, #58046, #1815 ) ) ;
#46836 = VERTEX_POINT ( 'NONE', #44633 ) ;
#46837 = CARTESIAN_POINT ( 'NONE',  ( 46.12582897016705630, 10.39833982076225460, 67.59008823216548478 ) ) ;
#46838 = CARTESIAN_POINT ( 'NONE',  ( -106.3047475500521557, 36.01269213589261398, -89.86034216495879434 ) ) ;
#46839 = CARTESIAN_POINT ( 'NONE',  ( 130.7260704202054455, 39.56565398554879920, 57.02343801570094683 ) ) ;
#46840 = VERTEX_POINT ( 'NONE', #39706 ) ;
#46841 = EDGE_CURVE ( 'NONE', #44889, #51452, #10889, .T. ) ;
#46842 = PRODUCT_DEFINITION_SHAPE ( 'NONE', 'NONE',  #69614 ) ;
#46843 = EDGE_CURVE ( 'NONE', #3682, #34095, #41910, .T. ) ;
#46844 = ADVANCED_FACE ( 'NONE', ( #20320 ), #24234, .F. ) ;
#46845 = CARTESIAN_POINT ( 'NONE',  ( -24.22878282689200446, 8.518516047505652722, 93.49511739771224939 ) ) ;
#46846 = VECTOR ( 'NONE', #12277, 1000.000000000000000 ) ;
#46847 = CARTESIAN_POINT ( 'NONE',  ( 176.6156959113760365, 75.60152827082544036, -64.52720677928732584 ) ) ;
#46848 = CARTESIAN_POINT ( 'NONE',  ( 442.3372781065084496, 390.0000000000043201, 108.5502958579838690 ) ) ;
#46849 = CARTESIAN_POINT ( 'NONE',  ( 106.6192711434718632, 27.24117154335862168, -49.99331757005764842 ) ) ;
#46850 = EDGE_CURVE ( 'NONE', #6017, #61415, #67156, .T. ) ;
#46851 = DIRECTION ( 'NONE',  ( 0.000000000000000000, 0.000000000000000000, -1.000000000000000000 ) ) ;
#46852 = AXIS2_PLACEMENT_3D ( 'NONE', #5787, #27244, #48678 ) ;
#46853 = CARTESIAN_POINT ( 'NONE',  ( 209.3223706822284100, 0.000000000000000000, 31.44247402469554942 ) ) ;
#46854 = ORIENTED_EDGE ( 'NONE', *, *, #36518, .T. ) ;
#46855 = EDGE_CURVE ( 'NONE', #45414, #42599, #47758, .T. ) ;
#46856 = CIRCLE ( 'NONE', #15437, 99.99999999999994316 ) ;
#46857 = CARTESIAN_POINT ( 'NONE',  ( 45.82394788922800899, 46.11928342727495078, 41.38025477438755928 ) ) ;
#46858 = CARTESIAN_POINT ( 'NONE',  ( -81.23268307104842734, 24.39742801172155140, -76.51131192360561784 ) ) ;
#46859 = DIRECTION ( 'NONE',  ( -1.000000000000000000, 0.000000000000000000, 0.000000000000000000 ) ) ;
#46860 = CARTESIAN_POINT ( 'NONE',  ( 133.8566784816069060, 42.60093787723656789, -89.71241211332301191 ) ) ;
#46861 = DIRECTION ( 'NONE',  ( -0.4338837391175525693, -0.9009688679024218105, 2.500042656554809354E-16 ) ) ;
#46862 = CIRCLE ( 'NONE', #5286, 5.000000000000004441 ) ;
#46863 = CARTESIAN_POINT ( 'NONE',  ( 126.3737790127712799, 37.08609730334947585, 10.73674426291554873 ) ) ;
#46864 = LINE ( 'NONE', #64071, #68481 ) ;
#46865 = CARTESIAN_POINT ( 'NONE',  ( -120.0051930351106932, 43.92079660368833061, -64.60660167447554159 ) ) ;
#46866 = LINE ( 'NONE', #41252, #61338 ) ;
#46867 = DIRECTION ( 'NONE',  ( -0.000000000000000000, 1.000000000000000000, -0.000000000000000000 ) ) ;
#46868 = CARTESIAN_POINT ( 'NONE',  ( 10.55634918610409656, 36.11269837220803680, 2.000000000000001776 ) ) ;
#46869 = EDGE_LOOP ( 'NONE', ( #32126, #6172, #60390, #1121 ) ) ;
#46870 = VECTOR ( 'NONE', #27985, 1000.000000000000000 ) ;
#46871 = ITEM_DEFINED_TRANSFORMATION ( 'NONE', 'NONE', #62440,  #66832 ) ;
#46872 = CARTESIAN_POINT ( 'NONE',  ( -57.54960251878999600, 16.40992651131772817, 84.42727806790901468 ) ) ;
#46873 = ORIENTED_EDGE ( 'NONE', *, *, #61849, .T. ) ;
#46874 = CARTESIAN_POINT ( 'NONE',  ( 201.6034029841262907, 102.1956603101140928, -10.13592553938994101 ) ) ;
#46875 = ORIENTED_EDGE ( 'NONE', *, *, #66338, .F. ) ;
#46876 = CARTESIAN_POINT ( 'NONE',  ( 16.77480716385437276, 7.540753720029939267, -77.31445149746915035 ) ) ;
#46877 = DIRECTION ( 'NONE',  ( 0.000000000000000000, 0.000000000000000000, 1.000000000000000000 ) ) ;
#46878 = CARTESIAN_POINT ( 'NONE',  ( -422.6627218934913230, 399.9999999999997726, 108.5502958579881891 ) ) ;
#46879 = CARTESIAN_POINT ( 'NONE',  ( 65.00000000000000000, 0.000000000000000000, 85.00000000000000000 ) ) ;
#46880 = ADVANCED_FACE ( 'NONE', ( #4157 ), #14365, .F. ) ;
#46881 = EDGE_CURVE ( 'NONE', #29599, #5435, #25272, .T. ) ;
#46882 = CARTESIAN_POINT ( 'NONE',  ( 140.7888851157410386, 46.97220912571248874, -40.64884308134027435 ) ) ;
#46883 = CARTESIAN_POINT ( 'NONE',  ( 32.46582151331404731, 7.608418548522502434, -40.23543673364789441 ) ) ;
#46884 = CARTESIAN_POINT ( 'NONE',  ( 197.5101196254995841, 96.97937853946277187, 92.57920919658415926 ) ) ;
#46885 = CARTESIAN_POINT ( 'NONE',  ( 8.537735592981560373, 7.383000420390740004, -41.08501613461158541 ) ) ;
#46886 = DIRECTION ( 'NONE',  ( 0.000000000000000000, 0.000000000000000000, -1.000000000000000000 ) ) ;
#46887 = EDGE_CURVE ( 'NONE', #34711, #57676, #58092, .T. ) ;
#46888 = FACE_OUTER_BOUND ( 'NONE', #59519, .T. ) ;
#46889 = ORIENTED_EDGE ( 'NONE', *, *, #14460, .F. ) ;
#46890 = VERTEX_POINT ( 'NONE', #9432 ) ;
#46891 = CARTESIAN_POINT ( 'NONE',  ( 173.7992108938316846, 72.92047568072842978, 88.67055234059489521 ) ) ;
#46892 = FACE_OUTER_BOUND ( 'NONE', #44863, .T. ) ;
#46893 = CARTESIAN_POINT ( 'NONE',  ( 9.827939172326075834, 6.382931149346554811, 15.24920466621778203 ) ) ;
#46894 = DIRECTION ( 'NONE',  ( 0.000000000000000000, 0.000000000000000000, 1.000000000000000000 ) ) ;
#46895 = B_SPLINE_CURVE_WITH_KNOTS ( 'NONE', 3,
 ( #67932, #8490, #30984, #19033, #51740, #2862, #47141, #14791, #30291, #41187, #45775, #35912, #52081, #13756, #3546, #63334, #8841, #19377, #62649, #62293, #25017, #51051, #29939, #35214, #3901, #35565, #36254, #51405, #9523, #68273, #15144, #46450, #62983, #19729, #25369, #9177, #57364, #14457, #46804, #14105, #57710, #3217, #24329, #36603 ),
 .UNSPECIFIED., .F., .F.,
 ( 4, 2, 2, 2, 2, 2, 2, 2, 2, 2, 2, 2, 2, 2, 2, 2, 2, 2, 2, 2, 2, 4 ),
 ( 0.000000000000000000, 0.003518733725596298340, 0.004398417156995381057, 0.005278100588394462472, 0.007037467451192679080, 0.007917150882591750954, 0.008796834313990822829, 0.01055620117678900995, 0.01231556803958719880, 0.01319525147098629322, 0.01407493490238538765, 0.01495461833378448034, 0.01583430176518357130, 0.01671398519658266746, 0.01759366862798176015, 0.01935303549077993165, 0.02111240235357809969, 0.02199208578497716463, 0.02287176921637622609, 0.02463113607917437331, 0.02639050294197252053, 0.02814986980477066775 ),
 .UNSPECIFIED. ) ;
#46896 = DIRECTION ( 'NONE',  ( 0.000000000000000000, 0.7660444431189770143, 0.6427876096865403621 ) ) ;
#46897 = PLANE ( 'NONE',  #22564 ) ;
#46898 = VECTOR ( 'NONE', #46821, 1000.000000000000000 ) ;
#46899 = DIRECTION ( 'NONE',  ( -1.000000000000000000, 0.000000000000000000, 0.000000000000000000 ) ) ;
#46900 = CARTESIAN_POINT ( 'NONE',  ( -125.0000000000000000, 0.000000000000000000, -5.000000000000000000 ) ) ;
#46901 = CARTESIAN_POINT ( 'NONE',  ( -24.60892750534350881, 9.584951112520228023, 61.45297857596762725 ) ) ;
#46902 = DIRECTION ( 'NONE',  ( 1.000000000000000000, 0.000000000000000000, 0.000000000000000000 ) ) ;
#46903 = LINE ( 'NONE', #19831, #53467 ) ;
#46904 = VECTOR ( 'NONE', #61604, 1000.000000000000000 ) ;
#46905 = ORIENTED_EDGE ( 'NONE', *, *, #8425, .T. ) ;
#46906 = CARTESIAN_POINT ( 'NONE',  ( 21.98745393275290638, -71.71550996510497100, 43.58025477438756212 ) ) ;
#46907 = CARTESIAN_POINT ( 'NONE',  ( 3.565943279261457821, 0.000000000000000000, -2.293637981077754073 ) ) ;
#46908 = CARTESIAN_POINT ( 'NONE',  ( -71.96466849523078224, 21.15771699336999845, 43.58025477438756212 ) ) ;
#46909 = FACE_OUTER_BOUND ( 'NONE', #1579, .T. ) ;
#46910 = CYLINDRICAL_SURFACE ( 'NONE', #54822, 7.500000000000027534 ) ;
#46911 = CARTESIAN_POINT ( 'NONE',  ( 15.55634918610400241, -15.55634918610406103, 85.00100000000000477 ) ) ;
#46912 = VECTOR ( 'NONE', #65901, 1000.000000000000114 ) ;
#46913 = VECTOR ( 'NONE', #27108, 1000.000000000000000 ) ;
#46914 = ORIENTED_EDGE ( 'NONE', *, *, #42833, .T. ) ;
#46915 = CARTESIAN_POINT ( 'NONE',  ( -190.3636887049961786, 108.6554956426205933, -91.83124475734037162 ) ) ;
#46916 = CARTESIAN_POINT ( 'NONE',  ( -59.36813706141737867, 15.88103696331963377, 70.80079528359327412 ) ) ;
#46917 = EDGE_LOOP ( 'NONE', ( #39261, #23579, #37265, #15294 ) ) ;
#46918 = AXIS2_PLACEMENT_3D ( 'NONE', #48738, #11822, #27997 ) ;
#46919 = ORIENTED_EDGE ( 'NONE', *, *, #58139, .F. ) ;
#46920 = EDGE_CURVE ( 'NONE', #31642, #44050, #25621, .T. ) ;
#46921 = FACE_OUTER_BOUND ( 'NONE', #38244, .T. ) ;
#46922 = CARTESIAN_POINT ( 'NONE',  ( -175.9970298498767534, 90.38640259140140643, -75.99633293260467326 ) ) ;
#46923 = CARTESIAN_POINT ( 'NONE',  ( 138.7757999158632742, 45.66865872093048750, -91.53672265411847775 ) ) ;
#46924 = VERTEX_POINT ( 'NONE', #50955 ) ;
#46925 = DIRECTION ( 'NONE',  ( -0.000000000000000000, -0.000000000000000000, -1.000000000000000000 ) ) ;
#46926 = DIRECTION ( 'NONE',  ( 0.3090169943749447312, 0.9510565162951545304, 0.000000000000000000 ) ) ;
#46927 = B_SPLINE_CURVE_WITH_KNOTS ( 'NONE', 3,
 ( #26065, #63350, #9191, #20094, #24689, #14804, #9541, #62308, #52101, #67948, #35928, #19743, #35585, #41206, #3916, #41890, #20776, #31000, #42238, #57729, #52448, #14122, #58072, #47157, #63701, #30650, #15161, #25388, #4265, #25728, #36268, #57380, #3232, #41547, #68621, #62665, #8857, #63002, #8507, #57043, #67597, #20426, #47492, #40855, #46126, #68289, #36622, #14473, #36966, #9890, #30307, #31343 ),
 .UNSPECIFIED., .F., .F.,
 ( 4, 2, 2, 2, 2, 2, 2, 2, 2, 2, 2, 2, 2, 2, 2, 2, 2, 2, 2, 2, 2, 2, 2, 2, 2, 4 ),
 ( 0.000000000000000000, 0.002032670951089465741, 0.003049006426634202297, 0.004065341902178939287, 0.005081677377723675844, 0.006098012853268411533, 0.007114348328813148090, 0.008130683804357885514, 0.009147019279902621203, 0.01016335475544735863, 0.01219602570653683001, 0.01422869665762630312, 0.01626136760871577797, 0.01727770308426054835, 0.01829403855980532220, 0.02032670951089484562, 0.02134304498643961254, 0.02235938046198437598, 0.02337571593752914290, 0.02439205141307390634, 0.02642472236416344364, 0.02845739331525297400, 0.02947372879079776173, 0.03049006426634255293, 0.03150639974188734066, 0.03252273521743212492 ),
 .UNSPECIFIED. ) ;
#46928 = CARTESIAN_POINT ( 'NONE',  ( 55.52751777340358785, 12.08567914268656374, -42.73101172783196233 ) ) ;
#46929 = CARTESIAN_POINT ( 'NONE',  ( -84.21836162213176635, 25.60181819557222127, 32.85243609328976788 ) ) ;
#46930 = CARTESIAN_POINT ( 'NONE',  ( 150.9834489474288830, 52.77764236634784112, 94.42848054783445377 ) ) ;
#46931 = CARTESIAN_POINT ( 'NONE',  ( 94.06703982324142999, 22.09435144471462564, 38.20947434515352370 ) ) ;
#46932 = EDGE_CURVE ( 'NONE', #22488, #14559, #57957, .T. ) ;
#46933 = ORIENTED_EDGE ( 'NONE', *, *, #17569, .T. ) ;
#46934 = CARTESIAN_POINT ( 'NONE',  ( 15.78827728214693060, 6.500811158483329244, 71.85925826316895382 ) ) ;
#46935 = EDGE_CURVE ( 'NONE', #10376, #37117, #64824, .T. ) ;
#46936 = CARTESIAN_POINT ( 'NONE',  ( -29.74902699556086816, 10.33856194202125600, 45.02758640895530817 ) ) ;
#46937 = DIRECTION ( 'NONE',  ( 0.7071067811865475727, 0.000000000000000000, -0.7071067811865475727 ) ) ;
#46938 = EDGE_CURVE ( 'NONE', #2243, #41180, #64614, .T. ) ;
#46939 = CARTESIAN_POINT ( 'NONE',  ( -71.68176805937196150, 20.84773878116192947, 94.41661040422935969 ) ) ;
#46941 = ORIENTED_EDGE ( 'NONE', *, *, #67054, .F. ) ;
#46940 = LINE ( 'NONE', #50833, #2891 ) ;
#46942 = CARTESIAN_POINT ( 'NONE',  ( 63.50537371531940778, 13.81987663608981798, 44.81296093922130552 ) ) ;
#46943 = VERTEX_POINT ( 'NONE', #31239 ) ;
#46944 = VERTEX_POINT ( 'NONE', #37185 ) ;
#46945 = SURFACE_STYLE_USAGE ( .BOTH. , #10675 ) ;
#46946 = AXIS2_PLACEMENT_3D ( 'NONE', #49755, #55751, #33259 ) ;
#46947 = DIRECTION ( 'NONE',  ( -1.000000000000000000, 0.000000000000000000, 0.000000000000000000 ) ) ;
#46948 = CARTESIAN_POINT ( 'NONE',  ( 197.9847015768255005, 97.56951352050450055, -67.31407702796413162 ) ) ;
#46949 = CARTESIAN_POINT ( 'NONE',  ( -35.17296606710974061, 11.25626711331309338, 58.03790650501060355 ) ) ;
#46950 = FACE_OUTER_BOUND ( 'NONE', #49688, .T. ) ;
#46951 = CARTESIAN_POINT ( 'NONE',  ( -84.53753601793930272, 25.73343139558518544, -20.46458922348523046 ) ) ;
#46952 = FACE_OUTER_BOUND ( 'NONE', #14189, .T. ) ;
#46953 = CARTESIAN_POINT ( 'NONE',  ( -156.4960819023051783, 70.34114605623875605, -39.53833954081760993 ) ) ;
#46954 = VERTEX_POINT ( 'NONE', #594 ) ;
#46955 = VERTEX_POINT ( 'NONE', #69194 ) ;
#46956 = VECTOR ( 'NONE', #45611, 1000.000000000000000 ) ;
#46957 = CARTESIAN_POINT ( 'NONE',  ( -109.4995148930278361, 37.75156937139181679, 9.075767506675283869 ) ) ;
#46958 = DIRECTION ( 'NONE',  ( -0.000000000000000000, -0.000000000000000000, -1.000000000000000000 ) ) ;
#46959 = LINE ( 'NONE', #37091, #55967 ) ;
#46960 = CARTESIAN_POINT ( 'NONE',  ( -190.3061188229048639, 108.5745819235682035, 69.14762690905678255 ) ) ;
#46961 = VECTOR ( 'NONE', #34680, 1000.000000000000000 ) ;
#46962 = CYLINDRICAL_SURFACE ( 'NONE', #34885, 298.0000000000000000 ) ;
#46963 = CARTESIAN_POINT ( 'NONE',  ( 427.4999999999999432, -18.06806526123148160, 378.0000000000000000 ) ) ;
#46964 = EDGE_CURVE ( 'NONE', #56852, #51103, #64266, .T. ) ;
#46965 = DIRECTION ( 'NONE',  ( -0.000000000000000000, -1.000000000000000000, -0.000000000000000000 ) ) ;
#46966 = ORIENTED_EDGE ( 'NONE', *, *, #43751, .F. ) ;
#46967 = ORIENTED_EDGE ( 'NONE', *, *, #49054, .T. ) ;
#46968 = ORIENTED_EDGE ( 'NONE', *, *, #12395, .T. ) ;
#46969 = AXIS2_PLACEMENT_3D ( 'NONE', #48384, #11123, #54012 ) ;
#46970 =( LENGTH_UNIT ( ) NAMED_UNIT ( * ) SI_UNIT ( .MILLI., .METRE. ) );
#46971 = CARTESIAN_POINT ( 'NONE',  ( -84.55373779407986490, 24.65190748253135666, 60.08995505548700322 ) ) ;
#46972 = CARTESIAN_POINT ( 'NONE',  ( 105.1611065714564006, -21.96385652020509838, 1.300672318859854126 ) ) ;
#46973 = CYLINDRICAL_SURFACE ( 'NONE', #68578, 65.36598343705435354 ) ;
#46974 = CARTESIAN_POINT ( 'NONE',  ( -152.2964402771109178, 66.58174574061953876, -8.502547355955140773 ) ) ;
#46975 = CARTESIAN_POINT ( 'NONE',  ( 33.75639351246965703, 7.742023566824295600, 59.29622260418393154 ) ) ;
#46976 = CARTESIAN_POINT ( 'NONE',  ( -2.116120943112233199, 74.98056102853672655, 73.58025477438756923 ) ) ;
#46977 = ORIENTED_EDGE ( 'NONE', *, *, #32324, .T. ) ;
#46978 = CARTESIAN_POINT ( 'NONE',  ( 16.77480716385437276, 7.540753720029938378, 3.219200273921916544 ) ) ;
#46979 = PLANE ( 'NONE',  #5965 ) ;
#46980 = CARTESIAN_POINT ( 'NONE',  ( -122.7930600691577752, 44.48546375740916403, 18.12006331166574924 ) ) ;
#46981 = CARTESIAN_POINT ( 'NONE',  ( 63.01563776193091826, 12.67277567978498709, -62.56524142263340593 ) ) ;
#46982 = CARTESIAN_POINT ( 'NONE',  ( 16.27765348919938049, 6.516472002017813736, 56.85925826316893961 ) ) ;
#46983 = FACE_OUTER_BOUND ( 'NONE', #2858, .T. ) ;
#46984 = CARTESIAN_POINT ( 'NONE',  ( 8.288696687633805738, 7.382586467017838494, 10.16927303540167671 ) ) ;
#46985 = ORIENTED_EDGE ( 'NONE', *, *, #46881, .F. ) ;
#46986 = CYLINDRICAL_SURFACE ( 'NONE', #10245, 7.500000000000013323 ) ;
#46987 = APPLICATION_PROTOCOL_DEFINITION ( 'draft international standard', 'automotive_design', 1998, #33642 ) ;
#46988 = CARTESIAN_POINT ( 'NONE',  ( 131.6115093721024607, 41.25402743071400380, -50.68309935467904381 ) ) ;
#46989 = LINE ( 'NONE', #3394, #61278 ) ;
#46990 = DIRECTION ( 'NONE',  ( -1.000000000000000000, 0.000000000000000000, 0.000000000000000000 ) ) ;
#46991 = ITEM_DEFINED_TRANSFORMATION ( 'NONE', 'NONE', #38789,  #66832 ) ;
#46992 = CARTESIAN_POINT ( 'NONE',  ( 187.5246323291927126, 86.86207184872510823, -39.84316934690760803 ) ) ;
#46993 = ORIENTED_EDGE ( 'NONE', *, *, #37286, .T. ) ;
#46994 = ORIENTED_EDGE ( 'NONE', *, *, #1780, .T. ) ;
#46995 = EDGE_CURVE ( 'NONE', #55150, #1969, #53350, .T. ) ;
#46996 = PLANE ( 'NONE',  #42631 ) ;
#46997 = EDGE_CURVE ( 'NONE', #47125, #31823, #54717, .T. ) ;
#46998 = DIRECTION ( 'NONE',  ( 0.000000000000000000, 0.000000000000000000, -1.000000000000000000 ) ) ;
#46999 = EDGE_LOOP ( 'NONE', ( #21022, #7765 ) ) ;
#47000 = VECTOR ( 'NONE', #23820, 1000.000000000000000 ) ;
#47001 = EDGE_CURVE ( 'NONE', #20206, #6708, #53006, .T. ) ;
#47002 = CARTESIAN_POINT ( 'NONE',  ( 115.0692128464502559, 31.17922615202196113, 69.71731335093312509 ) ) ;
#47003 = VERTEX_POINT ( 'NONE', #21351 ) ;
#47004 = CARTESIAN_POINT ( 'NONE',  ( -62.41727141396691536, 17.83188754031767687, 12.45580772492516708 ) ) ;
#47005 = CARTESIAN_POINT ( 'NONE',  ( 126.6395826915640015, 37.23416510613628105, 34.95296513652632342 ) ) ;
#47006 = CIRCLE ( 'NONE', #16665, 21.50000000000000000 ) ;
#47007 = DIRECTION ( 'NONE',  ( 3.989004196750126251E-18, -3.181124695048441435E-18, -1.000000000000000000 ) ) ;
#47008 = CARTESIAN_POINT ( 'NONE',  ( -94.79166046756729713, 29.13671350128076654, 38.51002725759197887 ) ) ;
#47009 = AXIS2_PLACEMENT_3D ( 'NONE', #6714, #26785, #28159 ) ;
#47010 = LINE ( 'NONE', #8352, #19304 ) ;
#47012 = ORIENTED_EDGE ( 'NONE', *, *, #16520, .F. ) ;
#47011 = CARTESIAN_POINT ( 'NONE',  ( 48.39383208188379371, 43.94028683479089636, 3.125053320693570118E-16 ) ) ;
#47013 = CARTESIAN_POINT ( 'NONE',  ( 30.12852347772543027, -74.98256102853682137, 73.58025477438755502 ) ) ;
#47014 = ORIENTED_EDGE ( 'NONE', *, *, #37624, .T. ) ;
#47015 = ORIENTED_EDGE ( 'NONE', *, *, #9957, .F. ) ;
#47016 = CARTESIAN_POINT ( 'NONE',  ( -168.0003605155415869, 83.06333427281272463, 5.991919408726039009 ) ) ;
#47017 = CARTESIAN_POINT ( 'NONE',  ( 39.51413990058172487, 0.000000000000000000, 2.347205688660291667 ) ) ;
#47018 = ADVANCED_FACE ( 'NONE', ( #26642 ), #17633, .T. ) ;
#47019 = CARTESIAN_POINT ( 'NONE',  ( -148.6426892915312408, 64.76241938621075178, -34.81283053149196860 ) ) ;
#47020 = EDGE_CURVE ( 'NONE', #3542, #24590, #57863, .T. ) ;
#47021 = EDGE_CURVE ( 'NONE', #22570, #2304, #44182, .T. ) ;
#47023 = VERTEX_POINT ( 'NONE', #49459 ) ;
#47022 = CARTESIAN_POINT ( 'NONE',  ( -132.8150886319751294, 52.45790550853839562, 62.06390996835829554 ) ) ;
#47024 = DIRECTION ( 'NONE',  ( 0.000000000000000000, 0.000000000000000000, 1.000000000000000000 ) ) ;
#47025 = CARTESIAN_POINT ( 'NONE',  ( 209.3223706822284100, 172.0000000000000284, 276.7520087653757628 ) ) ;
#47026 = EDGE_LOOP ( 'NONE', ( #60917, #598 ) ) ;
#47027 = B_SPLINE_CURVE_WITH_KNOTS ( 'NONE', 3,
 ( #4137, #40036, #8024, #223 ),
 .UNSPECIFIED., .F., .F.,
 ( 4, 4 ),
 ( 9.900409499100981944E-07, 0.05658314289920114704 ),
 .UNSPECIFIED. ) ;
#47028 = CARTESIAN_POINT ( 'NONE',  ( -61.75629144857964548, 16.58190704077737720, -12.49911615342323579 ) ) ;
#47029 = CARTESIAN_POINT ( 'NONE',  ( -133.2787743207941276, 52.78950725740546090, -67.92237397683200584 ) ) ;
#47030 = CARTESIAN_POINT ( 'NONE',  ( 61.01086442919169883, 12.21637211111878862, -89.67119804626783264 ) ) ;
#47031 = DIRECTION ( 'NONE',  ( 0.000000000000000000, 0.000000000000000000, -1.000000000000000000 ) ) ;
#47032 = CARTESIAN_POINT ( 'NONE',  ( 68.62997155117719217, 15.08415013720829023, -65.06837658636030142 ) ) ;
#47033 = ORIENTED_EDGE ( 'NONE', *, *, #10290, .T. ) ;
#47034 = ORIENTED_EDGE ( 'NONE', *, *, #43837, .F. ) ;
#47035 = CARTESIAN_POINT ( 'NONE',  ( 184.0013086981202548, 81.60415045669142842, -63.64686322466085500 ) ) ;
#47036 = CARTESIAN_POINT ( 'NONE',  ( -165.9122696334865168, 79.44688201528256855, -44.30228794590340868 ) ) ;
#47037 = DIRECTION ( 'NONE',  ( -0.4738686624730094610, 0.8805955318567321166, 0.000000000000000000 ) ) ;
#47038 = DIRECTION ( 'NONE',  ( -0.000000000000000000, -6.405132834375902056E-16, 1.000000000000000000 ) ) ;
#47039 = CARTESIAN_POINT ( 'NONE',  ( -71.57660578921961303, 20.81129687646280146, 40.41523763771648703 ) ) ;
#47040 = CARTESIAN_POINT ( 'NONE',  ( 544.6745185807129701, 2.000000000000001776, 34.73878747406611467 ) ) ;
#47041 = CARTESIAN_POINT ( 'NONE',  ( 5.007715329123879543E-16, -9.237604307034043671, -9.500000000000000000 ) ) ;
#47042 = CARTESIAN_POINT ( 'NONE',  ( -450.6627218934913230, 0.000000000000000000, -6.938893903907228378E-15 ) ) ;
#47043 = CARTESIAN_POINT ( 'NONE',  ( -169.8842709557924593, 83.59602878049473418, -75.83670934591202695 ) ) ;
#47044 = ORIENTED_EDGE ( 'NONE', *, *, #23180, .F. ) ;
#47045 = CARTESIAN_POINT ( 'NONE',  ( -149.5074843970971301, -170.0000000000000000, -42.31283053149197571 ) ) ;
#47046 = ORIENTED_EDGE ( 'NONE', *, *, #46621, .T. ) ;
#47047 = CARTESIAN_POINT ( 'NONE',  ( -38.55214349681827457, 10.86754840574841907, 8.443293971405456233 ) ) ;
#47048 = FACE_OUTER_BOUND ( 'NONE', #2676, .T. ) ;
#47049 = CARTESIAN_POINT ( 'NONE',  ( 19.00668540189274225, -62.54164772954691642, 41.38025477438755928 ) ) ;
#47050 = CARTESIAN_POINT ( 'NONE',  ( -64.61430802170492882, 7.070445451047391749, 170.0000000000000000 ) ) ;
#47051 = CARTESIAN_POINT ( 'NONE',  ( 32.90051628396145844, 8.664124555952446016, 6.797922165733859323 ) ) ;
#47052 = VECTOR ( 'NONE', #54332, 1000.000000000000227 ) ;
#47053 = B_SPLINE_CURVE_WITH_KNOTS ( 'NONE', 3,
 ( #3144, #35839, #8771, #8057, #41801, #24256, #68198, #40411, #62211, #45697, #67502, #63260, #8413, #57291, #15066, #30217, #25290, #67176, #52007, #9447, #3822, #30907, #35489, #52354, #51669, #35139, #4170, #62571, #3475, #46376, #25638, #47070, #61858, #67853, #13681, #36523, #19299, #64284, #68859, #48421, #31939, #63604, #63941, #48772, #52684, #42140, #20683, #43160 ),
 .UNSPECIFIED., .F., .F.,
 ( 4, 2, 2, 2, 2, 2, 2, 2, 2, 2, 2, 2, 2, 2, 2, 2, 2, 2, 2, 2, 2, 2, 2, 4 ),
 ( 0.02698595842317762922, 0.02784423243973397494, 0.02870250645629031719, 0.03041905448940304679, 0.03127732850595942027, 0.03213560252251579374, 0.03385215055562854763, 0.03471042457218491417, 0.03556869858874128071, 0.03728524662185400684, 0.03814352063841035256, 0.03900179465496669828, 0.03986006867152304400, 0.04071834268807938972, 0.04157661670463573544, 0.04243489072119208810, 0.04415143875430482118, 0.04500971277086116690, 0.04586798678741751956, 0.04758453482053019712, 0.04930108285364286774, 0.05101763088675554531, 0.05273417891986822287, 0.05445072695298090043 ),
 .UNSPECIFIED. ) ;
#47054 = CARTESIAN_POINT ( 'NONE',  ( 149.0250918491436494, 6.000000000000000000, -41.68900338898718871 ) ) ;
#47055 = CARTESIAN_POINT ( 'NONE',  ( 50.97490815085634352, 6.000000000000000000, -9.435653166495500344 ) ) ;
#47056 = CARTESIAN_POINT ( 'NONE',  ( -13.47517652744367034, 8.334971000693554899, -37.96130542306915601 ) ) ;
#47057 = CARTESIAN_POINT ( 'NONE',  ( -31.43908319763709969, 10.61114334766716105, -23.47264677473818395 ) ) ;
#47058 = ORIENTED_EDGE ( 'NONE', *, *, #26379, .T. ) ;
#47059 = DIRECTION ( 'NONE',  ( -0.000000000000000000, 0.000000000000000000, -1.000000000000000000 ) ) ;
#47060 = VERTEX_POINT ( 'NONE', #54389 ) ;
#47061 = CARTESIAN_POINT ( 'NONE',  ( 63.01563776193091826, 13.70579113808095251, 56.65751152968497451 ) ) ;
#47062 = CARTESIAN_POINT ( 'NONE',  ( 9.819093282782493048, 7.389085782749409859, -65.29636817529980419 ) ) ;
#47063 = CARTESIAN_POINT ( 'NONE',  ( -28.81317668042940028, 9.175023678939295380, 3.842413854045814148 ) ) ;
#47064 = PLANE ( 'NONE',  #54724 ) ;
#47065 = CARTESIAN_POINT ( 'NONE',  ( -61.71141560932036185, 16.56840812182238309, -92.92626464638486539 ) ) ;
#47066 = DIRECTION ( 'NONE',  ( 0.000000000000000000, 0.000000000000000000, -1.000000000000000000 ) ) ;
#47067 = CARTESIAN_POINT ( 'NONE',  ( 152.1153500913667074, 54.85403770686896507, -38.36719606911704972 ) ) ;
#47068 = ORIENTED_EDGE ( 'NONE', *, *, #63763, .F. ) ;
#47069 = DIRECTION ( 'NONE',  ( 0.1884548733085519845, -2.077167649210491653E-15, 0.9820818503191358628 ) ) ;
#47070 = CARTESIAN_POINT ( 'NONE',  ( -156.6862310659955995, 71.88416263379568250, 67.30894339101347157 ) ) ;
#47071 = CARTESIAN_POINT ( 'NONE',  ( 181.0840389613909736, 80.03940679743416808, -24.38050707541595230 ) ) ;
#47072 = CARTESIAN_POINT ( 'NONE',  ( -105.4487797565984408, 35.55724615608638572, 58.04979929862538768 ) ) ;
#47073 = CARTESIAN_POINT ( 'NONE',  ( -126.7944042662568478, 48.29830493043728268, -49.87326901552447822 ) ) ;
#47074 = ORIENTED_EDGE ( 'NONE', *, *, #64995, .T. ) ;
#47075 = CARTESIAN_POINT ( 'NONE',  ( -30.00000000000000355, 26.99999999999999289, 0.000000000000000000 ) ) ;
#47076 = CARTESIAN_POINT ( 'NONE',  ( 88.30010642107258434, 19.99780058782975090, 71.37213675879502262 ) ) ;
#47077 = CARTESIAN_POINT ( 'NONE',  ( 117.3281529665582070, 32.29994712002881840, 39.62392251532779142 ) ) ;
#47078 = EDGE_CURVE ( 'NONE', #41738, #51274, #23797, .T. ) ;
#47079 =( LENGTH_UNIT ( ) NAMED_UNIT ( * ) SI_UNIT ( .MILLI., .METRE. ) );
#47080 = EDGE_CURVE ( 'NONE', #20436, #65848, #945, .T. ) ;
#47081 = FACE_OUTER_BOUND ( 'NONE', #16158, .T. ) ;
#47082 = ORIENTED_EDGE ( 'NONE', *, *, #6808, .T. ) ;
#47083 = CARTESIAN_POINT ( 'NONE',  ( -196.7348448768811409, -170.0000000000000000, 65.26711856384670796 ) ) ;
#47084 = DIRECTION ( 'NONE',  ( 0.5407162030609372616, -0.6444004775717707689, 0.5407162030609375947 ) ) ;
#47085 = CARTESIAN_POINT ( 'NONE',  ( 186.0827296088606602, 85.28826835108064586, 42.40481399445034327 ) ) ;
#47086 = CARTESIAN_POINT ( 'NONE',  ( 158.3636111008086687, 59.62671916656142201, 17.56491688178971700 ) ) ;
#47087 = EDGE_CURVE ( 'NONE', #19070, #38482, #6212, .T. ) ;
#47088 = CARTESIAN_POINT ( 'NONE',  ( 15.55634918610411610, 46.66904755831205875, 2.000000000000001776 ) ) ;
#47089 = VECTOR ( 'NONE', #68816, 1000.000000000000114 ) ;
#47090 = ORIENTED_EDGE ( 'NONE', *, *, #5770, .F. ) ;
#47091 = CARTESIAN_POINT ( 'NONE',  ( 177.0110682437507990, 75.98481089748385386, 57.33934894850843023 ) ) ;
#47092 = EDGE_LOOP ( 'NONE', ( #51116, #3611, #60587, #20752 ) ) ;
#47093 = CARTESIAN_POINT ( 'NONE',  ( -109.7290872258107157, 36.72869630780159156, -43.53384799749126444 ) ) ;
#47094 = CARTESIAN_POINT ( 'NONE',  ( 136.9580891181123548, 43.32873266151486291, 83.86339557539821499 ) ) ;
#47095 = EDGE_CURVE ( 'NONE', #31811, #63882, #55805, .T. ) ;
#47096 = CARTESIAN_POINT ( 'NONE',  ( -62.48965350618345127, 16.80247907725180667, 38.81988781192542604 ) ) ;
#47098 = ORIENTED_EDGE ( 'NONE', *, *, #27892, .F. ) ;
#47097 = CARTESIAN_POINT ( 'NONE',  ( 157.2533363798600021, 58.75760182111575602, 2.564916881789686798 ) ) ;
#47099 = CYLINDRICAL_SURFACE ( 'NONE', #4967, 7.500000000000013323 ) ;
#47100 = LINE ( 'NONE', #36900, #42891 ) ;
#47101 = VECTOR ( 'NONE', #68126, 1000.000000000000114 ) ;
#47102 = CARTESIAN_POINT ( 'NONE',  ( 112.5612011511790058, 31.08353758940340938, -50.57087292189984140 ) ) ;
#47103 = VERTEX_POINT ( 'NONE', #50176 ) ;
#47104 = DIRECTION ( 'NONE',  ( 0.000000000000000000, 0.000000000000000000, 1.000000000000000000 ) ) ;
#47105 = LINE ( 'NONE', #43460, #6224 ) ;
#47106 = ORIENTED_EDGE ( 'NONE', *, *, #14076, .F. ) ;
#47107 = CARTESIAN_POINT ( 'NONE',  ( 141.2811136745702640, 46.09188267874201728, 62.75964268212607067 ) ) ;
#47108 = CARTESIAN_POINT ( 'NONE',  ( -165.7138623879809529, 79.24467249981145756, 39.53662309097534688 ) ) ;
#47109 = DIRECTION ( 'NONE',  ( 1.000000000000000000, 0.000000000000000000, -0.000000000000000000 ) ) ;
#47110 = CARTESIAN_POINT ( 'NONE',  ( 91.49210130311617206, 22.20929244416437953, 42.92723601512285114 ) ) ;
#47111 = ORIENTED_EDGE ( 'NONE', *, *, #32636, .T. ) ;
#47112 = CARTESIAN_POINT ( 'NONE',  ( 44.34689728705969003, 10.12166135033765180, 16.22939414383014878 ) ) ;
#47113 = VERTEX_POINT ( 'NONE', #7628 ) ;
#47114 = AXIS2_PLACEMENT_3D ( 'NONE', #53489, #21829, #736 ) ;
#47115 = CARTESIAN_POINT ( 'NONE',  ( 157.0357419681844249, 58.58786672900117765, -24.27023266159657666 ) ) ;
#47116 = CARTESIAN_POINT ( 'NONE',  ( -58.12888781187205467, 15.52769087903062406, 84.65900618614021766 ) ) ;
#47117 = DIRECTION ( 'NONE',  ( 1.357354004350931427E-18, 4.918261777702530142E-18, -1.000000000000000000 ) ) ;
#47118 = CARTESIAN_POINT ( 'NONE',  ( 31.11269837220812562, 36.11269837220800838, 0.000000000000000000 ) ) ;
#47119 = CARTESIAN_POINT ( 'NONE',  ( 56.17239497942856019, 11.18888580659344179, 87.91446924145196817 ) ) ;
#47120 = CARTESIAN_POINT ( 'NONE',  ( 187.6511924654682559, 87.00187850361885467, 6.331325941773287447 ) ) ;
#47121 = CARTESIAN_POINT ( 'NONE',  ( 42.52268486319166385, -51.31691592985912109, 34.48241824003540046 ) ) ;
#47122 = CARTESIAN_POINT ( 'NONE',  ( -53.60725281709914469, 37.40286400928249577, 41.38025477438755928 ) ) ;
#47123 = ORIENTED_EDGE ( 'NONE', *, *, #16966, .F. ) ;
#47124 = CARTESIAN_POINT ( 'NONE',  ( 19.00668540189185407, 62.54164772954719353, 43.58025477438756212 ) ) ;
#47125 = VERTEX_POINT ( 'NONE', #12544 ) ;
#47126 = CARTESIAN_POINT ( 'NONE',  ( -71.97658551692138929, 20.95070248419152747, 61.36288391214083049 ) ) ;
#47127 = CARTESIAN_POINT ( 'NONE',  ( 43.35536254672138057, 9.973606330917816010, -22.65335710938210312 ) ) ;
#47128 = FILL_AREA_STYLE ('',( #15130 ) ) ;
#47129 = DIRECTION ( 'NONE',  ( -0.000000000000000000, -0.000000000000000000, -1.000000000000000000 ) ) ;
#47130 = CARTESIAN_POINT ( 'NONE',  ( 20.35964562795319566, 7.697260051881317899, 43.48066962168281435 ) ) ;
#47131 = CIRCLE ( 'NONE', #38136, 5.000000000000000888 ) ;
#47132 = CARTESIAN_POINT ( 'NONE',  ( -104.5740066103012254, 35.09687312794776659, -22.81448265554261212 ) ) ;
#47133 = ORIENTED_EDGE ( 'NONE', *, *, #54366, .T. ) ;
#47134 = EDGE_CURVE ( 'NONE', #40013, #12323, #25109, .T. ) ;
#47135 = CARTESIAN_POINT ( 'NONE',  ( -74.40004226286976063, 20.74218500375953766, 58.58967130592457551 ) ) ;
#47136 = LINE ( 'NONE', #53437, #7169 ) ;
#47137 = ORIENTED_EDGE ( 'NONE', *, *, #26604, .T. ) ;
#47138 = ORIENTED_EDGE ( 'NONE', *, *, #4897, .T. ) ;
#47139 = CARTESIAN_POINT ( 'NONE',  ( -154.0718453320783397, 68.14976693162391541, 32.26507081757433326 ) ) ;
#47140 = CARTESIAN_POINT ( 'NONE',  ( 56.30171512200996631, 11.21502580416395567, -39.86886612370064853 ) ) ;
#47141 = CARTESIAN_POINT ( 'NONE',  ( 177.5945652320813792, 75.14951358071813559, -10.23784609841178295 ) ) ;
#47142 = CARTESIAN_POINT ( 'NONE',  ( -36.84489839129265931, -53.54860840895233309, 40.00000000000003553 ) ) ;
#47143 = CARTESIAN_POINT ( 'NONE',  ( -144.7571537022063808, 60.25265659240449168, 5.567462641871050444 ) ) ;
#47144 = AXIS2_PLACEMENT_3D ( 'NONE', #36299, #41916, #51448 ) ;
#47145 = ORIENTED_EDGE ( 'NONE', *, *, #38611, .F. ) ;
#47146 = AXIS2_PLACEMENT_3D ( 'NONE', #6247, #63359, #68296 ) ;
#47147 = CARTESIAN_POINT ( 'NONE',  ( -127.6894679065405427, 48.89973668460849865, 45.41578626271343211 ) ) ;
#47148 = VERTEX_POINT ( 'NONE', #22397 ) ;
#47149 = CARTESIAN_POINT ( 'NONE',  ( 16.77480716385436921, 7.540753720029938378, -50.46990090700543874 ) ) ;
#47150 = CARTESIAN_POINT ( 'NONE',  ( -143.7133518487516994, 60.70463114991425613, 42.98969525936463043 ) ) ;
#47151 = SURFACE_STYLE_FILL_AREA ( #51416 ) ;
#47152 = CARTESIAN_POINT ( 'NONE',  ( 0.000000000000000000, 0.000000000000000000, -2.000000000000000000 ) ) ;
#47153 = EDGE_CURVE ( 'NONE', #15461, #68402, #2344, .T. ) ;
#47154 = ORIENTED_EDGE ( 'NONE', *, *, #2529, .T. ) ;
#47155 = ORIENTED_EDGE ( 'NONE', *, *, #44236, .T. ) ;
#47156 = CARTESIAN_POINT ( 'NONE',  ( 114.9681307937126320, -21.99268844340181417, -0.6535439379101506407 ) ) ;
#47157 = CARTESIAN_POINT ( 'NONE',  ( -124.8392882614943602, 47.00413044825191378, 84.36113447088062856 ) ) ;
#47158 = LINE ( 'NONE', #20777, #40850 ) ;
#47159 = CARTESIAN_POINT ( 'NONE',  ( -180.0154536325058245, 96.73346874014741559, 14.44416461865400869 ) ) ;
#47160 = EDGE_CURVE ( 'NONE', #9547, #56182, #26666, .T. ) ;
#47161 = CARTESIAN_POINT ( 'NONE',  ( 14.15607123919027188, 6.453851046686879478, 83.87628020752921998 ) ) ;
#47162 = AXIS2_PLACEMENT_3D ( 'NONE', #17530, #28434, #22462 ) ;
#47164 = EDGE_CURVE ( 'NONE', #35337, #23974, #51384, .T. ) ;
#47163 = CARTESIAN_POINT ( 'NONE',  ( 10.70820696327198895, 7.397428319378121842, 85.67662758554656932 ) ) ;
#47165 = ORIENTED_EDGE ( 'NONE', *, *, #55836, .F. ) ;
#47166 = CARTESIAN_POINT ( 'NONE',  ( 64.16679220703369424, 10.37413986118183828, 40.00000000000003553 ) ) ;
#47167 = CARTESIAN_POINT ( 'NONE',  ( -101.8191498210055101, 32.54686850610961812, 57.36362509687882039 ) ) ;
#47168 = VERTEX_POINT ( 'NONE', #22747 ) ;
#47169 = CARTESIAN_POINT ( 'NONE',  ( -79.14127775978542445, 22.50259208414362178, 3.573650549209442584 ) ) ;
#47170 = VERTEX_POINT ( 'NONE', #43834 ) ;
#47171 = LINE ( 'NONE', #61966, #34270 ) ;
#47173 = ORIENTED_EDGE ( 'NONE', *, *, #33182, .F. ) ;
#47172 = EDGE_CURVE ( 'NONE', #53408, #43885, #34572, .T. ) ;
#47174 = ORIENTED_EDGE ( 'NONE', *, *, #10333, .T. ) ;
#47175 = CARTESIAN_POINT ( 'NONE',  ( -121.5928001448269100, 44.91559452735374691, 17.43750400987426374 ) ) ;
#47176 = VECTOR ( 'NONE', #60373, 1000.000000000000000 ) ;
#47177 = EDGE_CURVE ( 'NONE', #41403, #47540, #7273, .T. ) ;
#47179 = EDGE_CURVE ( 'NONE', #26262, #2286, #60019, .T. ) ;
#47178 = CARTESIAN_POINT ( 'NONE',  ( -180.5230320745700396, 95.76406004447548526, 63.91740180504579172 ) ) ;
#47180 = CARTESIAN_POINT ( 'NONE',  ( 127.4750938923429402, 37.70245908594340989, 59.90632388648024431 ) ) ;
#47181 = ORIENTED_EDGE ( 'NONE', *, *, #11076, .T. ) ;
#47182 = DIRECTION ( 'NONE',  ( -0.000000000000000000, 1.000000000000000000, -0.000000000000000000 ) ) ;
#47183 = CARTESIAN_POINT ( 'NONE',  ( -51.77779688167512262, 14.86590802019196822, 4.221165638100599082 ) ) ;
#47184 = CARTESIAN_POINT ( 'NONE',  ( 8.000000000000001776, 0.000000000000000000, -9.500000000000000000 ) ) ;
#47185 = CARTESIAN_POINT ( 'NONE',  ( 105.2506154496929582, 26.63995206619728506, -37.82003446714997352 ) ) ;
#47186 = B_SPLINE_CURVE_WITH_KNOTS ( 'NONE', 3,
 ( #8098, #13721, #29548, #35177, #60519, #2825, #66174, #56631, #34151, #51365, #24294, #12336, #45736, #50659, #18306, #33793, #28871, #45030, #67214, #7056, #28513, #2479 ),
 .UNSPECIFIED., .F., .F.,
 ( 4, 2, 2, 2, 2, 2, 2, 2, 2, 2, 4 ),
 ( 0.000000000000000000, 0.001562679269560080398, 0.003125358539120160796, 0.003906698173900237207, 0.004688037808680313619, 0.006250717078240390981, 0.007032056713020401473, 0.007813396347800413699, 0.009376075617360434683, 0.01093875488692046954, 0.01250143415648050441 ),
 .UNSPECIFIED. ) ;
#47187 = CARTESIAN_POINT ( 'NONE',  ( -28.13852122803040601, 9.072484007196642608, 30.96421423579666765 ) ) ;
#47188 = COLOUR_RGB ( '',0.7921568627450980005, 0.8196078431372548767, 0.9333333333333333481 ) ;
#47189 = CARTESIAN_POINT ( 'NONE',  ( -15.55634918610400597, 15.55634918610405748, 2.000000000000001776 ) ) ;
#47190 = ORIENTED_EDGE ( 'NONE', *, *, #63698, .T. ) ;
#47191 = AXIS2_PLACEMENT_3D ( 'NONE', #44501, #33262, #6523 ) ;
#47192 = CARTESIAN_POINT ( 'NONE',  ( 0.000000000000000000, 0.000000000000000000, 0.000000000000000000 ) ) ;
#47193 = CARTESIAN_POINT ( 'NONE',  ( -82.32006615997346444, 24.83050031643766076, -76.02779720937938635 ) ) ;
#47194 = CARTESIAN_POINT ( 'NONE',  ( 174.6242782760050432, 73.69713439533578025, 13.78395099967788440 ) ) ;
#47195 = FACE_OUTER_BOUND ( 'NONE', #20123, .T. ) ;
#47196 = CARTESIAN_POINT ( 'NONE',  ( 36.64089410029661309, -65.45232906116366678, 170.0000000000000000 ) ) ;
#47197 = CARTESIAN_POINT ( 'NONE',  ( 127.4953815656694758, 37.71366486045442201, 14.17018500853721008 ) ) ;
#47198 = CARTESIAN_POINT ( 'NONE',  ( 35.12301194579454489, 7.891331172724800780, -90.63528273682473468 ) ) ;
#47199 = LINE ( 'NONE', #14846, #13692 ) ;
#47200 = CARTESIAN_POINT ( 'NONE',  ( 210.6584452238134588, 116.7138338345753539, 32.12903558767059309 ) ) ;
#47201 = CARTESIAN_POINT ( 'NONE',  ( 162.7921669283191761, 61.91024532638674316, 4.774496695581312622 ) ) ;
#47202 = CARTESIAN_POINT ( 'NONE',  ( -108.0980548770427561, 35.83569586822708430, 42.77788030405751840 ) ) ;
#47203 = VERTEX_POINT ( 'NONE', #65314 ) ;
#47204 = CARTESIAN_POINT ( 'NONE',  ( -58.96642505241147347, 16.81239758210119817, 85.10078055707477063 ) ) ;
#47205 = EDGE_LOOP ( 'NONE', ( #61807, #22741, #22334, #10145, #38440, #14868, #1299 ) ) ;
#47206 = DIRECTION ( 'NONE',  ( 0.000000000000000000, 0.000000000000000000, 1.000000000000000000 ) ) ;
#47207 = EDGE_LOOP ( 'NONE', ( #45415, #52508 ) ) ;
#47208 = CARTESIAN_POINT ( 'NONE',  ( 23.23965501943000689, 7.861749956303023978, -70.84722685082371640 ) ) ;
#47209 = CARTESIAN_POINT ( 'NONE',  ( -4.999999999999936939, 31.11269837220806167, 85.00100000000000477 ) ) ;
#47210 = CARTESIAN_POINT ( 'NONE',  ( -144.3939084932120807, 61.25241660819417433, 70.55718103091443538 ) ) ;
#47211 = DIRECTION ( 'NONE',  ( -0.000000000000000000, -0.000000000000000000, -1.000000000000000000 ) ) ;
#47212 = CARTESIAN_POINT ( 'NONE',  ( 141.1220430186942565, 47.19066702031172866, -41.64338897693998831 ) ) ;
#47213 = CARTESIAN_POINT ( 'NONE',  ( 35.65685430025424552, 7.951642554322392087, -36.60339655490213318 ) ) ;
#47214 = ADVANCED_FACE ( 'NONE', ( #12199 ), #55091, .F. ) ;
#47215 = CARTESIAN_POINT ( 'NONE',  ( 150.0889146124742695, 52.13243511955543141, -44.98044688291916060 ) ) ;
#47216 = DIRECTION ( 'NONE',  ( -0.8118923937861950435, -0.5838071093367415143, 0.000000000000000000 ) ) ;
#47217 = CARTESIAN_POINT ( 'NONE',  ( -35.00000000000002842, 225.0000000000000000, -2.000000000000000000 ) ) ;
#47218 = VERTEX_POINT ( 'NONE', #6916 ) ;
#47219 = ORIENTED_EDGE ( 'NONE', *, *, #62771, .T. ) ;
#47220 = ADVANCED_FACE ( 'NONE', ( #28366 ), #23102, .T. ) ;
#47221 = CARTESIAN_POINT ( 'NONE',  ( 177.3158870624719725, 76.28207752284875198, 84.00542473672297206 ) ) ;
#47222 = FACE_OUTER_BOUND ( 'NONE', #52701, .T. ) ;
#47223 = FACE_OUTER_BOUND ( 'NONE', #7494, .T. ) ;
#47224 = UNCERTAINTY_MEASURE_WITH_UNIT (LENGTH_MEASURE( 1.000000000000000082E-05 ), #27565, 'distance_accuracy_value', 'NONE');
#47225 = AXIS2_PLACEMENT_3D ( 'NONE', #3125, #19282, #24585 ) ;
#47226 = CARTESIAN_POINT ( 'NONE',  ( 0.000000000000000000, 0.000000000000000000, 0.000000000000000000 ) ) ;
#47227 = CARTESIAN_POINT ( 'NONE',  ( 46.12611922993086466, 10.39838587005582404, -73.29553601737912061 ) ) ;
#47228 = PLANE ( 'NONE',  #43565 ) ;
#47229 = CARTESIAN_POINT ( 'NONE',  ( 173.6718135456486607, 71.42581476597408141, -69.38831629246477917 ) ) ;
#47230 = LINE ( 'NONE', #69024, #29542 ) ;
#47231 = CARTESIAN_POINT ( 'NONE',  ( 94.12811352634520290, 22.11743943276051638, -17.00099467980526313 ) ) ;
#47232 = CARTESIAN_POINT ( 'NONE',  ( -29.51272929882557605, 10.30144624948894361, 71.81352569274244502 ) ) ;
#47233 = CARTESIAN_POINT ( 'NONE',  ( -20.55634918610403261, 5.000000000000028422, 2.000000000000001776 ) ) ;
#47234 = EDGE_CURVE ( 'NONE', #59875, #47585, #66380, .T. ) ;
#47235 = DIRECTION ( 'NONE',  ( 1.000000000000000000, 0.000000000000000000, 0.000000000000000000 ) ) ;
#47236 = EDGE_CURVE ( 'NONE', #66025, #11003, #29079, .T. ) ;
#47237 = EDGE_CURVE ( 'NONE', #64405, #60938, #62464, .T. ) ;
#47238 = EDGE_LOOP ( 'NONE', ( #27043, #9736, #44738, #7148 ) ) ;
#47239 = CARTESIAN_POINT ( 'NONE',  ( 126.4318266066171930, 38.27072266789465260, 9.074042217399220789 ) ) ;
#47240 = DIRECTION ( 'NONE',  ( -0.000000000000000000, -0.000000000000000000, -1.000000000000000000 ) ) ;
#47241 = LINE ( 'NONE', #9972, #50997 ) ;
#47242 = CARTESIAN_POINT ( 'NONE',  ( -109.5157885508426716, 37.76058765671429285, -67.31801888139685275 ) ) ;
#47243 = CARTESIAN_POINT ( 'NONE',  ( -51.77439426130689526, 13.82695438436704016, -35.96638716134758340 ) ) ;
#47244 = CARTESIAN_POINT ( 'NONE',  ( 60.82895951008336510, 30.68107831874607072, 0.000000000000000000 ) ) ;
#47245 = EDGE_LOOP ( 'NONE', ( #3495, #54792 ) ) ;
#47246 = DIRECTION ( 'NONE',  ( 0.000000000000000000, -1.000000000000000000, 0.000000000000000000 ) ) ;
#47247 = CARTESIAN_POINT ( 'NONE',  ( -59.94781924509481286, 16.04872117907065743, 70.34947420817375985 ) ) ;
#47248 = ORIENTED_EDGE ( 'NONE', *, *, #36950, .T. ) ;
#47249 = ORIENTED_EDGE ( 'NONE', *, *, #55104, .F. ) ;
#47250 = CARTESIAN_POINT ( 'NONE',  ( 32.21871194187785648, 8.594856915925895180, 88.92095415218777532 ) ) ;
#47251 = CARTESIAN_POINT ( 'NONE',  ( -15.67984581961064450, 63.08044415722863363, 40.00000000000003553 ) ) ;
#47252 = CARTESIAN_POINT ( 'NONE',  ( 110.2429982417149432, 28.88204397445228722, 44.61121420573733332 ) ) ;
#47253 = VERTEX_POINT ( 'NONE', #35388 ) ;
#47254 = CARTESIAN_POINT ( 'NONE',  ( 0.000000000000000000, 0.000000000000000000, -9.500000000000000000 ) ) ;
#47255 = DIRECTION ( 'NONE',  ( 0.000000000000000000, 0.000000000000000000, -1.000000000000000000 ) ) ;
#47256 = AXIS2_PLACEMENT_3D ( 'NONE', #53951, #5443, #65229 ) ;
#47257 = CARTESIAN_POINT ( 'NONE',  ( 33.44983424733138122, 7.709709042132399937, -11.68551422328344280 ) ) ;
#47258 = EDGE_CURVE ( 'NONE', #36885, #17268, #62852, .T. ) ;
#47260 = EDGE_CURVE ( 'NONE', #29791, #67595, #69334, .T. ) ;
#47259 = DIRECTION ( 'NONE',  ( 1.110223024625156294E-16, 3.697785493223491743E-32, -1.000000000000000000 ) ) ;
#47261 = EDGE_CURVE ( 'NONE', #47170, #65715, #30451, .T. ) ;
#47262 = CARTESIAN_POINT ( 'NONE',  ( -153.1031717208031750, 68.63449618039564371, -75.74321926140552819 ) ) ;
#47263 = CARTESIAN_POINT ( 'NONE',  ( 90.91465859190770971, 20.92790537681856478, 31.05212256305487983 ) ) ;
#47264 = VECTOR ( 'NONE', #5621, 1000.000000000000000 ) ;
#47265 = EDGE_CURVE ( 'NONE', #22725, #39170, #32295, .T. ) ;
#47266 = PRODUCT_DEFINITION_SHAPE ( 'NONE', 'NONE',  #8730 ) ;
#47267 = ORIENTED_EDGE ( 'NONE', *, *, #63761, .F. ) ;
#47268 = VECTOR ( 'NONE', #116, 1000.000000000000000 ) ;
#47269 = LINE ( 'NONE', #9298, #37919 ) ;
#47270 = CARTESIAN_POINT ( 'NONE',  ( 8.848532605049253874, 6.377649401037234433, 67.23478819807002083 ) ) ;
#47271 = DIRECTION ( 'NONE',  ( 0.000000000000000000, 1.000000000000000000, -0.000000000000000000 ) ) ;
#47272 = CARTESIAN_POINT ( 'NONE',  ( 199.2049631873263422, 100.7347227143600037, 41.82079194744246564 ) ) ;
#47273 = CARTESIAN_POINT ( 'NONE',  ( -71.26176386603191304, 20.70224608353110796, 92.84341710835518313 ) ) ;
#47275 = ORIENTED_EDGE ( 'NONE', *, *, #35419, .F. ) ;
#47274 = DIRECTION ( 'NONE',  ( 0.5773502691896258421, -0.5773502691896258421, -0.5773502691896258421 ) ) ;
#47276 = ORIENTED_EDGE ( 'NONE', *, *, #24142, .F. ) ;
#47277 = ORIENTED_EDGE ( 'NONE', *, *, #25645, .T. ) ;
#47278 = CARTESIAN_POINT ( 'NONE',  ( 86.62931800182293784, 19.42108912189596381, 56.55663816294300261 ) ) ;
#47279 = CARTESIAN_POINT ( 'NONE',  ( 197.3054165770396082, 96.72615186924558373, -71.97836107770491765 ) ) ;
#47280 = DIRECTION ( 'NONE',  ( -0.000000000000000000, 1.000000000000000000, -0.000000000000000000 ) ) ;
#47281 = DIRECTION ( 'NONE',  ( 0.000000000000000000, 0.000000000000000000, 1.000000000000000000 ) ) ;
#47282 = CARTESIAN_POINT ( 'NONE',  ( 150.4550062612853480, 52.39582885725847916, -67.76395233042956079 ) ) ;
#47283 = CARTESIAN_POINT ( 'NONE',  ( 20.36314374176838982, 6.689939636827348046, -22.13797671587966320 ) ) ;
#47284 = CARTESIAN_POINT ( 'NONE',  ( -155.7433525314458791, 69.65452735858369238, -38.13774150188479695 ) ) ;
#47285 = ORIENTED_EDGE ( 'NONE', *, *, #51131, .F. ) ;
#47286 = ORIENTED_EDGE ( 'NONE', *, *, #46065, .T. ) ;
#47287 = CARTESIAN_POINT ( 'NONE',  ( 0.7145311798163209716, 4.618802153517001408, -8.000000000000000000 ) ) ;
#47288 = CARTESIAN_POINT ( 'NONE',  ( -85.10909119100207931, 25.97025675005451717, -46.48749614101045324 ) ) ;
#47289 = CARTESIAN_POINT ( 'NONE',  ( 162.1014732644455023, 61.34312237409763213, 69.67267474247222481 ) ) ;
#47290 = CARTESIAN_POINT ( 'NONE',  ( -154.0716379918897019, 69.49957566103795159, 5.406051683299049060 ) ) ;
#47291 = CARTESIAN_POINT ( 'NONE',  ( -53.09243206623446554, 24.18057240364262128, 27.58472369387556355 ) ) ;
#47292 = CARTESIAN_POINT ( 'NONE',  ( 5.799999999999999822, 0.000000000000000000, 0.000000000000000000 ) ) ;
#47293 = CARTESIAN_POINT ( 'NONE',  ( 61.28323125814100081, 21.66484633135460669, 40.00000000000003553 ) ) ;
#47294 = ORIENTED_EDGE ( 'NONE', *, *, #39111, .F. ) ;
#47295 = VERTEX_POINT ( 'NONE', #23967 ) ;
#47296 = ORIENTED_EDGE ( 'NONE', *, *, #30895, .T. ) ;
#47297 = ADVANCED_FACE ( 'NONE', ( #54918 ), #6743, .T. ) ;
#47298 = CARTESIAN_POINT ( 'NONE',  ( -85.91089317961399274, 25.21459833389208782, 62.75547607985773624 ) ) ;
#47299 = PLANE ( 'NONE',  #48985 ) ;
#47300 = VECTOR ( 'NONE', #55911, 1000.000000000000000 ) ;
#47301 = CARTESIAN_POINT ( 'NONE',  ( -34.74563762132953570, 11.17960945723136668, -62.92554498051175216 ) ) ;
#47302 = CARTESIAN_POINT ( 'NONE',  ( 60.82895951008336510, 30.68107831874607072, 43.58025477438756923 ) ) ;
#47303 = CARTESIAN_POINT ( 'NONE',  ( 32.09567473596477782, 7.571373529017938253, 65.97000810165883422 ) ) ;
#47304 = CARTESIAN_POINT ( 'NONE',  ( 13.84937401517046673, 6.446378549072246500, -8.925169506644754946 ) ) ;
#47305 = AXIS2_PLACEMENT_3D ( 'NONE', #12050, #17679, #54949 ) ;
#47306 = DIRECTION ( 'NONE',  ( -1.000000000000000000, 0.000000000000000000, 0.000000000000000000 ) ) ;
#47307 = CARTESIAN_POINT ( 'NONE',  ( 181.5072453427590347, 79.03352099595187497, 56.15314469597510083 ) ) ;
#47308 = CARTESIAN_POINT ( 'NONE',  ( 5.355005115540897975, 6.145890662064649845, -0.08224679563971175333 ) ) ;
#47309 = CARTESIAN_POINT ( 'NONE',  ( 396.6937511374966334, 500.0000000000000000, -91.64566090791306863 ) ) ;
#47310 = CARTESIAN_POINT ( 'NONE',  ( -0.4996266546846072631, 6.524616273922395848, -95.00000000000133582 ) ) ;
#47311 = EDGE_CURVE ( 'NONE', #22570, #21034, #50359, .T. ) ;
#47312 = CARTESIAN_POINT ( 'NONE',  ( 17.73567516211396011, 7.577454475141601975, -23.43370752981164884 ) ) ;
#47313 = CARTESIAN_POINT ( 'NONE',  ( 198.4017331595408962, 98.09114638179335088, 59.46790870869396883 ) ) ;
#47314 = VECTOR ( 'NONE', #62950, 1000.000000000000000 ) ;
#47315 = VECTOR ( 'NONE', #60638, 1000.000000000000000 ) ;
#47316 = EDGE_CURVE ( 'NONE', #64960, #17852, #55984, .T. ) ;
#47317 = EDGE_CURVE ( 'NONE', #5465, #8520, #39450, .T. ) ;
#47318 = VERTEX_POINT ( 'NONE', #39120 ) ;
#47319 = CARTESIAN_POINT ( 'NONE',  ( 0.000000000000000000, 0.000000000000000000, 0.000000000000000000 ) ) ;
#47320 = APPLICATION_PROTOCOL_DEFINITION ( 'draft international standard', 'automotive_design', 1998, #51204 ) ;
#47321 = CARTESIAN_POINT ( 'NONE',  ( 174.1364721914477229, 71.85829564941444403, 33.96918356720905763 ) ) ;
#47322 = CARTESIAN_POINT ( 'NONE',  ( 31.11269837220809364, 20.55634918610396866, 85.00100000000000477 ) ) ;
#47323 = CARTESIAN_POINT ( 'NONE',  ( -103.8932886509197004, 34.74144483217663293, -49.84274311153227188 ) ) ;
#47324 = CARTESIAN_POINT ( 'NONE',  ( 184.3879440808139805, 83.47316703125157744, -36.98841972577437787 ) ) ;
#47325 = ORIENTED_EDGE ( 'NONE', *, *, #69568, .F. ) ;
#47326 = ORIENTED_EDGE ( 'NONE', *, *, #23109, .T. ) ;
#47327 = CARTESIAN_POINT ( 'NONE',  ( -27.48703802937314933, 8.975952825337591534, -9.593638160064255516 ) ) ;
#47328 = CARTESIAN_POINT ( 'NONE',  ( 203.1414537950835779, 105.9225671689748367, 17.21051589850434382 ) ) ;
#47329 = ORIENTED_EDGE ( 'NONE', *, *, #43084, .T. ) ;
#47330 = CARTESIAN_POINT ( 'NONE',  ( 0.000000000000000000, -36.09918303830819752, 30.00000000000000000 ) ) ;
#47331 = EDGE_LOOP ( 'NONE', ( #14006, #26076 ) ) ;
#47332 = CARTESIAN_POINT ( 'NONE',  ( 114.6659427952414632, 32.10199811723105512, 70.03145237251035837 ) ) ;
#47333 = FACE_OUTER_BOUND ( 'NONE', #54957, .T. ) ;
#47334 = CARTESIAN_POINT ( 'NONE',  ( 111.9975424824652634, 172.0000000000000284, 354.1673509436691347 ) ) ;
#47335 = EDGE_CURVE ( 'NONE', #30237, #14714, #2175, .T. ) ;
#47336 = CARTESIAN_POINT ( 'NONE',  ( -95.63568360745007624, 29.53168204475776548, 34.53108459816321130 ) ) ;
#47337 = CARTESIAN_POINT ( 'NONE',  ( -72.62976060914745347, 18.74780984163036024, 170.0000000000000000 ) ) ;
#47339 = ORIENTED_EDGE ( 'NONE', *, *, #54944, .T. ) ;
#47338 = DIRECTION ( 'NONE',  ( -0.000000000000000000, 0.000000000000000000, -1.000000000000000000 ) ) ;
#47340 = EDGE_CURVE ( 'NONE', #15785, #59242, #55624, .T. ) ;
#47341 = B_SPLINE_CURVE_WITH_KNOTS ( 'NONE', 3,
 ( #52793, #26081, #47511, #14821, #10922, #63372, #63717, #36295, #5311, #20443, #57749, #15861, #36982, #68970, #10235, #31699, #64393, #21477, #21154, #37308, #53133, #15181, #58763, #26771, #52464, #42598, #53823, #4962, #10577, #47180, #26427, #47868, #37656, #32045, #48197, #9909, #59109, #25408, #46839, #36643, #68311, #9560, #31025, #4287, #25749, #41909 ),
 .UNSPECIFIED., .F., .F.,
 ( 4, 2, 2, 2, 2, 2, 2, 2, 2, 2, 2, 2, 2, 2, 2, 2, 2, 2, 2, 2, 2, 2, 4 ),
 ( 6.938893903907228378E-18, 0.001572224531395625307, 0.003144449062791243674, 0.004716673594186861392, 0.006288898125582480410, 0.007861122656978098561, 0.009433347188373715844, 0.01021945945407154617, 0.01100557171976937303, 0.01179168398546720162, 0.01257779625116503194, 0.01415002078256068739, 0.01493613304825850557, 0.01572224531395632549, 0.01650835757965414888, 0.01729446984535196533, 0.01886669437674765026, 0.01965280664244548059, 0.02043891890814331438, 0.02201114343953897504, 0.02358336797093463916, 0.02436948023663243132, 0.02515559250233022348 ),
 .UNSPECIFIED. ) ;
#47342 = DIRECTION ( 'NONE',  ( -1.000000000000000000, 0.000000000000000000, 0.000000000000000000 ) ) ;
#47343 = ORIENTED_EDGE ( 'NONE', *, *, #47311, .F. ) ;
#47344 = ORIENTED_EDGE ( 'NONE', *, *, #2551, .F. ) ;
#47345 = CARTESIAN_POINT ( 'NONE',  ( -124.3331814159187303, 45.47486189329070783, -22.90848852574204031 ) ) ;
#47346 = DIRECTION ( 'NONE',  ( -0.000000000000000000, 1.000000000000000000, -0.000000000000000000 ) ) ;
#47347 = CARTESIAN_POINT ( 'NONE',  ( -179.8996803435689174, 95.00451760716448746, -12.14598228191335849 ) ) ;
#47349 = ORIENTED_EDGE ( 'NONE', *, *, #43014, .T. ) ;
#47348 = CARTESIAN_POINT ( 'NONE',  ( -148.6409722988649946, 63.44808865916659357, -34.85989714948443918 ) ) ;
#47350 = CARTESIAN_POINT ( 'NONE',  ( 58.47885130911549112, 12.69429933094348328, 4.475850833756106262 ) ) ;
#47351 = VECTOR ( 'NONE', #50713, 1000.000000000000000 ) ;
#47352 = DIRECTION ( 'NONE',  ( 0.000000000000000000, 0.000000000000000000, 1.000000000000000000 ) ) ;
#47353 = ORIENTED_EDGE ( 'NONE', *, *, #28010, .T. ) ;
#47354 = B_SPLINE_CURVE_WITH_KNOTS ( 'NONE', 3,
 ( #52395, #35532, #56986, #8097, #30255, #61569, #4212, #46768, #51704, #24981, #56281, #46413, #62613, #45735, #35873, #57329, #9141, #20044, #67213, #41497, #62948, #18661, #13384, #25677, #13720, #47108, #40112, #52720, #48457, #37586, #54088, #21079, #32322, #69252, #64320, #48127, #5236, #26355, #63299, #10504, #26695, #20725, #68899, #42180, #5575, #41842 ),
 .UNSPECIFIED., .F., .F.,
 ( 4, 2, 2, 2, 2, 2, 2, 2, 2, 2, 2, 2, 2, 2, 2, 2, 2, 2, 2, 2, 2, 2, 4 ),
 ( 0.02989107162308292723, 0.03170280136394034581, 0.03351453110479776093, 0.03532626084565517605, 0.03713799058651259116, 0.03894972032737000628, 0.03985558519779868608, 0.04076145006822736588, 0.04166731493865603875, 0.04257317980908471855, 0.04347904467951339835, 0.04438490954994207816, 0.04529077442037075796, 0.04619663929079943776, 0.04710250416122811756, 0.04800836903165679737, 0.04891423390208547717, 0.04982009877251415697, 0.05163182851337153045, 0.05344355825422891781, 0.05525528799508629130, 0.05706701773594367866, 0.05887874747680105214 ),
 .UNSPECIFIED. ) ;
#47355 = CARTESIAN_POINT ( 'NONE',  ( -57.42615654242919021, 15.33060010148602892, -8.753093045165913466 ) ) ;
#47356 = VECTOR ( 'NONE', #48161, 1000.000000000000000 ) ;
#47357 = CARTESIAN_POINT ( 'NONE',  ( -128.3448054685827913, 49.34430406923178225, -76.35012269041114052 ) ) ;
#47358 = LINE ( 'NONE', #20634, #63983 ) ;
#47359 = CARTESIAN_POINT ( 'NONE',  ( -55.89173002820263036, 16.72186783039639124, 27.58472315868180402 ) ) ;
#47360 = CARTESIAN_POINT ( 'NONE',  ( -97.88309373898363219, 30.60238467438962928, -75.45378525617154253 ) ) ;
#47361 = VERTEX_POINT ( 'NONE', #44016 ) ;
#47362 = EDGE_LOOP ( 'NONE', ( #25920, #14659, #19740, #5255 ) ) ;
#47363 = CARTESIAN_POINT ( 'NONE',  ( 187.5325688887158151, 85.37769363979911930, -66.70143880898807254 ) ) ;
#47364 = VECTOR ( 'NONE', #67195, 1000.000000000000000 ) ;
#47365 = CARTESIAN_POINT ( 'NONE',  ( -36.11269837220812207, -31.11269837220801193, 0.000000000000000000 ) ) ;
#47366 = FACE_BOUND ( 'NONE', #36527, .T. ) ;
#47367 = PRODUCT_RELATED_PRODUCT_CATEGORY ( 'part', '', ( #59083 ) ) ;
#47368 = CARTESIAN_POINT ( 'NONE',  ( 104.3759779378692372, 27.35691041569132409, -65.56839599289385490 ) ) ;
#47369 = CARTESIAN_POINT ( 'NONE',  ( -67.03031041878467988, 33.66749151869449008, 170.0000000000000000 ) ) ;
#47370 = CARTESIAN_POINT ( 'NONE',  ( 79.14129363775930415, 17.00055658855363205, 36.71904541452036597 ) ) ;
#47371 = CARTESIAN_POINT ( 'NONE',  ( 0.3173508448886513400, 5.375634714784618851, -6.689127551062007626 ) ) ;
#47372 = CARTESIAN_POINT ( 'NONE',  ( -118.4709174626548673, 42.97515378817186615, 39.22611101928199417 ) ) ;
#47373 = CARTESIAN_POINT ( 'NONE',  ( -169.8791831685530553, 83.59058982490282119, -62.27878394338570445 ) ) ;
#47375 = ORIENTED_EDGE ( 'NONE', *, *, #19527, .F. ) ;
#47374 = ADVANCED_FACE ( 'NONE', ( #12372 ), #49998, .F. ) ;
#47376 = CARTESIAN_POINT ( 'NONE',  ( -107.0751323097254613, 35.28386110859231906, -21.45789132277915456 ) ) ;
#47377 = VERTEX_POINT ( 'NONE', #23630 ) ;
#47378 = CARTESIAN_POINT ( 'NONE',  ( -34.06864996337443330, 10.03773626259442331, 17.90007924047801779 ) ) ;
#47379 = EDGE_CURVE ( 'NONE', #11718, #18311, #45067, .T. ) ;
#47380 = CARTESIAN_POINT ( 'NONE',  ( 79.19119222799088220, 18.06817527909835164, 65.05072483751119705 ) ) ;
#47381 = DIRECTION ( 'NONE',  ( 0.000000000000000000, 0.000000000000000000, -1.000000000000000000 ) ) ;
#47382 = CARTESIAN_POINT ( 'NONE',  ( 55.04622734272535212, -19.32405960966675451, 27.58472369380034550 ) ) ;
#47383 = FACE_OUTER_BOUND ( 'NONE', #41823, .T. ) ;
#47384 = LINE ( 'NONE', #14697, #52934 ) ;
#47385 = CARTESIAN_POINT ( 'NONE',  ( 36.09137906183515554, 8.001963043161770983, -76.69864084344654032 ) ) ;
#47386 = DIRECTION ( 'NONE',  ( -1.000000000000000000, -0.000000000000000000, -0.000000000000000000 ) ) ;
#47387 = CARTESIAN_POINT ( 'NONE',  ( -36.38071096718369546, 11.47804921491337815, -10.30964823013966303 ) ) ;
#47388 = ORIENTED_EDGE ( 'NONE', *, *, #10997, .T. ) ;
#47389 = PLANE ( 'NONE',  #30859 ) ;
#47390 = ORIENTED_EDGE ( 'NONE', *, *, #66408, .F. ) ;
#47391 = CARTESIAN_POINT ( 'NONE',  ( 57.41085175769453741, 12.46982565415947697, 59.16780719303546476 ) ) ;
#47392 = SURFACE_STYLE_USAGE ( .BOTH. , #36512 ) ;
#47393 = CARTESIAN_POINT ( 'NONE',  ( -29.75049355503753645, 9.320234381800291956, 3.560369807396146502 ) ) ;
#47394 = FACE_OUTER_BOUND ( 'NONE', #27717, .T. ) ;
#47395 = CARTESIAN_POINT ( 'NONE',  ( 0.000000000000000000, 0.000000000000000000, 41.38025477438755928 ) ) ;
#47396 = DIRECTION ( 'NONE',  ( 1.000000000000000000, 0.000000000000000000, 0.000000000000000000 ) ) ;
#47397 = CARTESIAN_POINT ( 'NONE',  ( 153.4509883044095773, 55.84811350575044031, -49.96048919769913255 ) ) ;
#47398 = EDGE_CURVE ( 'NONE', #27081, #37153, #50698, .T. ) ;
#47399 = EDGE_CURVE ( 'NONE', #59711, #59702, #51142, .T. ) ;
#47400 = ORIENTED_EDGE ( 'NONE', *, *, #66970, .T. ) ;
#47401 = AXIS2_PLACEMENT_3D ( 'NONE', #69564, #31952, #63955 ) ;
#47402 = DIRECTION ( 'NONE',  ( 0.9820818503191347526, 1.059916043821828977E-14, -0.1884548733085578409 ) ) ;
#47403 = LINE ( 'NONE', #11158, #27327 ) ;
#47404 = CARTESIAN_POINT ( 'NONE',  ( 176.6156959113759513, 75.60152827082542615, -10.83810559835997900 ) ) ;
#47405 = CARTESIAN_POINT ( 'NONE',  ( -109.7686203588201295, 37.90089348911613598, 65.35533321413022634 ) ) ;
#47406 = DIRECTION ( 'NONE',  ( 0.000000000000000000, 0.000000000000000000, 1.000000000000000000 ) ) ;
#47407 = ORIENTED_EDGE ( 'NONE', *, *, #22526, .T. ) ;
#47408 = CARTESIAN_POINT ( 'NONE',  ( -78.66644367742109978, 23.39876645725288284, 3.573650549209446137 ) ) ;
#47409 = VECTOR ( 'NONE', #33086, 1000.000000000000000 ) ;
#47410 = B_SPLINE_CURVE_WITH_KNOTS ( 'NONE', 3,
 ( #40619, #60692, #12868, #23425, #45206, #39249, #39590, #7928, #23763, #34323, #1602, #65992, #18137, #55408, #61042, #35008, #33968, #29726, #40285, #35355, #2312, #51190, #62071, #39932, #17793, #13892, #50835, #12510, #66349, #61390, #1968, #7234, #8632, #55771, #45907, #7593, #61728, #67375, #28691, #50144, #29381, #56452, #13554, #19165, #23066 ),
 .UNSPECIFIED., .F., .F.,
 ( 4, 2, 2, 2, 2, 2, 2, 2, 2, 2, 2, 1, 2, 2, 2, 2, 2, 2, 2, 2, 2, 2, 4 ),
 ( 1.430489624538199204E-17, 0.001502898956853382460, 0.002254348435280062631, 0.003005797913706743235, 0.004508696870560142608, 0.005260146348986859642, 0.006011595827413576676, 0.007514494784267024621, 0.009017393741120474301, 0.01052029269797392051, 0.01127174217640065229, 0.01202319165482738407, 0.01277464113325411238, 0.01352609061168084242, 0.01502898956853430251, 0.01578043904696103256, 0.01653188852538776260, 0.01803478748224122269, 0.01953768643909467931, 0.02028913591752141629, 0.02104058539594814981, 0.02254348435280158561, 0.02404638330965502488 ),
 .UNSPECIFIED. ) ;
#47411 = CARTESIAN_POINT ( 'NONE',  ( -1.314022807222071432, 6.554273999800675377, -12.31960447689811389 ) ) ;
#47412 = CARTESIAN_POINT ( 'NONE',  ( 198.7129816317745963, 100.1061386900356069, -12.45321170628048080 ) ) ;
#47413 = VECTOR ( 'NONE', #45687, 1000.000000000000000 ) ;
#47414 = CARTESIAN_POINT ( 'NONE',  ( -152.9869010856123452, 67.18780492383567093, 85.26019206469960920 ) ) ;
#47415 = CARTESIAN_POINT ( 'NONE',  ( 22.25657943806483274, 6.793941046373902282, 94.99999999999866418 ) ) ;
#47416 = ORIENTED_EDGE ( 'NONE', *, *, #58138, .T. ) ;
#47417 = CARTESIAN_POINT ( 'NONE',  ( 15.55634918610411610, 46.66904755831205875, 85.00100000000000477 ) ) ;
#47418 = CARTESIAN_POINT ( 'NONE',  ( 69.68177367721197868, -20.52767805628085895, 41.38025477438755928 ) ) ;
#47419 = CARTESIAN_POINT ( 'NONE',  ( 185.7267155939802024, 84.90388481853123892, 30.91358943140728499 ) ) ;
#47420 = CARTESIAN_POINT ( 'NONE',  ( 154.4617654203035499, 56.60942201271839025, 30.02488550039760895 ) ) ;
#47421 = DIRECTION ( 'NONE',  ( 1.000000000000000000, -0.000000000000000000, -0.000000000000000000 ) ) ;
#47422 = CIRCLE ( 'NONE', #9273, 5.000000000000000888 ) ;
#47423 = ORIENTED_EDGE ( 'NONE', *, *, #64707, .F. ) ;
#47424 = DIRECTION ( 'NONE',  ( -0.000000000000000000, -0.000000000000000000, -1.000000000000000000 ) ) ;
#47425 = ORIENTED_EDGE ( 'NONE', *, *, #57514, .F. ) ;
#47426 = CARTESIAN_POINT ( 'NONE',  ( -73.81689110552359523, 20.53332132481500594, -21.49728268473057113 ) ) ;
#47427 = CARTESIAN_POINT ( 'NONE',  ( 16.78635691501517613, 6.000000000000000000, -14.43565316649550034 ) ) ;
#47428 = CARTESIAN_POINT ( 'NONE',  ( -61.75956139478098095, 16.58288496614412466, 34.45118629696971624 ) ) ;
#47429 = B_SPLINE_CURVE_WITH_KNOTS ( 'NONE', 3,
 ( #61302, #29631, #34593, #50405, #44781, #45115, #29986, #33882, #23337, #66258, #24372, #56720, #23671, #55320, #2222, #66945, #18048, #7141, #39504, #18738, #61982, #45816, #2563, #56364, #3259, #56029, #12772, #60951, #67295, #24719, #34234, #13126, #46152, #40531, #13800, #61646, #55675, #7841, #35261, #19079 ),
 .UNSPECIFIED., .F., .F.,
 ( 4, 2, 2, 2, 2, 2, 2, 2, 2, 2, 2, 2, 2, 2, 2, 2, 2, 2, 2, 4 ),
 ( 0.02454308262169000582, 0.02608670964102882336, 0.02685852315069824775, 0.02763033666036767214, 0.02917396367970651744, 0.02994577718937594529, 0.03071759069904536968, 0.03226121771838418029, 0.03303303122805360120, 0.03380484473772302212, 0.03534847175706185701, 0.03689209877640069885, 0.03843572579573954068, 0.03997935281507837557, 0.04152297983441721740, 0.04306660685375605924, 0.04461023387309490107, 0.04615386089243374290, 0.04769748791177259167, 0.04924111493111144044 ),
 .UNSPECIFIED. ) ;
#47431 = ORIENTED_EDGE ( 'NONE', *, *, #12788, .F. ) ;
#47430 = DIRECTION ( 'NONE',  ( -1.000000000000000000, -0.000000000000000000, -0.000000000000000000 ) ) ;
#47432 = CARTESIAN_POINT ( 'NONE',  ( -176.3896317155480062, 90.84057090619019448, 31.55718514125764074 ) ) ;
#47433 = DIRECTION ( 'NONE',  ( -0.000000000000000000, -0.000000000000000000, -1.000000000000000000 ) ) ;
#47434 = CARTESIAN_POINT ( 'NONE',  ( 116.8917656767876565, 33.20682060519246903, -39.94289992015058743 ) ) ;
#47435 = VERTEX_POINT ( 'NONE', #22576 ) ;
#47436 = CARTESIAN_POINT ( 'NONE',  ( -13.24252603915519444, -63.63674649211960599, 40.00000000000003553 ) ) ;
#47437 = PLANE ( 'NONE',  #54511 ) ;
#47438 = CARTESIAN_POINT ( 'NONE',  ( 141.0645618855930934, 45.95036951196541963, 61.71528580804383068 ) ) ;
#47439 = DIRECTION ( 'NONE',  ( 0.000000000000000000, 0.000000000000000000, 1.000000000000000000 ) ) ;
#47440 = DIRECTION ( 'NONE',  ( 0.000000000000000000, 0.000000000000000000, -1.000000000000000000 ) ) ;
#47441 = DIRECTION ( 'NONE',  ( -0.000000000000000000, -1.000000000000000000, -0.000000000000000000 ) ) ;
#47442 = ORIENTED_EDGE ( 'NONE', *, *, #56064, .F. ) ;
#47443 = DIRECTION ( 'NONE',  ( 1.000000000000000000, 0.000000000000000000, 0.000000000000000000 ) ) ;
#47444 = ORIENTED_EDGE ( 'NONE', *, *, #3642, .T. ) ;
#47445 = AXIS2_PLACEMENT_3D ( 'NONE', #62678, #14483, #59447 ) ;
#47446 = CARTESIAN_POINT ( 'NONE',  ( 156.5993887774280324, 58.24868799840903932, -24.23210818043918025 ) ) ;
#47447 = EDGE_CURVE ( 'NONE', #16032, #20172, #5315, .T. ) ;
#47448 = CARTESIAN_POINT ( 'NONE',  ( 55.61348889667009132, -50.24791103897046440, 41.38025477438755928 ) ) ;
#47449 = CARTESIAN_POINT ( 'NONE',  ( 110.2429982417149574, 29.99119854320843714, 44.61121420573733332 ) ) ;
#47450 = AXIS2_PLACEMENT_3D ( 'NONE', #21086, #10860, #58692 ) ;
#47451 = CARTESIAN_POINT ( 'NONE',  ( -149.5074843970971301, 64.17983161892345834, -76.65738112195568021 ) ) ;
#47452 = CARTESIAN_POINT ( 'NONE',  ( 69.70008851143845163, 14.32304089804287806, 94.41978594955163828 ) ) ;
#47453 = CARTESIAN_POINT ( 'NONE',  ( 183.1873354889582686, 82.20882912211249050, 2.752098851290597725 ) ) ;
#47454 = CARTESIAN_POINT ( 'NONE',  ( 16.62148331457517969, -18.83783649008704586, 3.061616997868437868E-16 ) ) ;
#47455 = EDGE_CURVE ( 'NONE', #49554, #65052, #27808, .T. ) ;
#47457 = PLANE ( 'NONE',  #62445 ) ;
#47456 = AXIS2_PLACEMENT_3D ( 'NONE', #37535, #16435, #36511 ) ;
#47458 = ORIENTED_EDGE ( 'NONE', *, *, #21899, .T. ) ;
#47459 = CYLINDRICAL_SURFACE ( 'NONE', #17228, 7.500000000000020428 ) ;
#47461 = VERTEX_POINT ( 'NONE', #40834 ) ;
#47460 = ADVANCED_FACE ( 'NONE', ( #55274 ), #18001, .F. ) ;
#47462 = CYLINDRICAL_SURFACE ( 'NONE', #45304, 7.500000000000013323 ) ;
#47463 = CARTESIAN_POINT ( 'NONE',  ( 59.72526569420001152, 11.93313563009889222, -63.30790693026741422 ) ) ;
#47464 = PLANE ( 'NONE',  #60844 ) ;
#47465 = FACE_OUTER_BOUND ( 'NONE', #46417, .T. ) ;
#47466 = EDGE_CURVE ( 'NONE', #30492, #34240, #31818, .T. ) ;
#47467 = CARTESIAN_POINT ( 'NONE',  ( -1.515478260543418498, 6.562165592639543021, 87.23764935852220503 ) ) ;
#47468 = VECTOR ( 'NONE', #38914, 1000.000000000000000 ) ;
#47469 = DIRECTION ( 'NONE',  ( 0.000000000000000000, 0.000000000000000000, -1.000000000000000000 ) ) ;
#47470 = ORIENTED_EDGE ( 'NONE', *, *, #19439, .T. ) ;
#47471 = DIRECTION ( 'NONE',  ( -1.000000000000000000, 0.000000000000000000, 0.000000000000000000 ) ) ;
#47472 = CARTESIAN_POINT ( 'NONE',  ( -452.6627218934862071, 370.0000000000064233, -141.4497041420121661 ) ) ;
#47473 = ORIENTED_EDGE ( 'NONE', *, *, #28029, .F. ) ;
#47474 = ORIENTED_EDGE ( 'NONE', *, *, #45926, .F. ) ;
#47475 = CARTESIAN_POINT ( 'NONE',  ( -30.46358361599563480, 10.45190018822943756, -62.20962308564316601 ) ) ;
#47476 = CARTESIAN_POINT ( 'NONE',  ( 59.72526569420001863, 11.93313563009889222, -36.46335633980373814 ) ) ;
#47477 = CARTESIAN_POINT ( 'NONE',  ( 19.71799482800335923, -15.56722426018171035, 3.061616997868437868E-16 ) ) ;
#47478 = FACE_OUTER_BOUND ( 'NONE', #3264, .T. ) ;
#47479 = DIRECTION ( 'NONE',  ( -0.000000000000000000, -0.000000000000000000, 1.000000000000000000 ) ) ;
#47480 = EDGE_CURVE ( 'NONE', #51871, #53693, #46895, .T. ) ;
#47481 = ORIENTED_EDGE ( 'NONE', *, *, #68780, .T. ) ;
#47482 = CARTESIAN_POINT ( 'NONE',  ( -125.8938041572051105, 47.69968343338781835, 45.61994787315711619 ) ) ;
#47483 = VERTEX_POINT ( 'NONE', #20078 ) ;
#47484 = CARTESIAN_POINT ( 'NONE',  ( 211.8476521439973794, 116.6941316755176956, 12.15074821135860894 ) ) ;
#47485 = DIRECTION ( 'NONE',  ( -0.000000000000000000, -0.000000000000000000, -1.000000000000000000 ) ) ;
#47486 =( NAMED_UNIT ( * ) PLANE_ANGLE_UNIT ( ) SI_UNIT ( $, .RADIAN. ) );
#47487 = DIRECTION ( 'NONE',  ( -0.000000000000000000, -0.000000000000000000, -1.000000000000000000 ) ) ;
#47488 = STYLED_ITEM ( 'NONE', ( #33043 ), #40824 ) ;
#47489 = ORIENTED_EDGE ( 'NONE', *, *, #14226, .F. ) ;
#47490 = ORIENTED_EDGE ( 'NONE', *, *, #42397, .F. ) ;
#47491 = CARTESIAN_POINT ( 'NONE',  ( 113.3053295232375319, -21.67655155662104249, 3.765949955696211937 ) ) ;
#47492 = CARTESIAN_POINT ( 'NONE',  ( -133.2885345616805068, 52.79649921787450495, 90.38452661033592506 ) ) ;
#47493 = VECTOR ( 'NONE', #2503, 1000.000000000000000 ) ;
#47494 = CARTESIAN_POINT ( 'NONE',  ( 38.42095780754792145, 9.297684251045549075, -62.51249201856361282 ) ) ;
#47495 = LINE ( 'NONE', #58402, #7462 ) ;
#47496 = CARTESIAN_POINT ( 'NONE',  ( 65.41496713438829147, 13.24164235279043922, 44.43526210712943936 ) ) ;
#47497 = CARTESIAN_POINT ( 'NONE',  ( 13.20823635526162931, 7.437507787974027451, 84.13046171212820923 ) ) ;
#47498 = CIRCLE ( 'NONE', #64377, 5.000000000000004441 ) ;
#47499 = EDGE_LOOP ( 'NONE', ( #59102, #67882, #23661, #13261 ) ) ;
#47500 = LINE ( 'NONE', #4606, #37060 ) ;
#47501 = DIRECTION ( 'NONE',  ( -0.000000000000000000, -1.000000000000000000, -0.000000000000000000 ) ) ;
#47502 = EDGE_LOOP ( 'NONE', ( #30467, #60034, #69143 ) ) ;
#47503 = AXIS2_PLACEMENT_3D ( 'NONE', #19568, #24852, #45953 ) ;
#47504 = CARTESIAN_POINT ( 'NONE',  ( -85.91089317961400695, 25.21459833389208072, 9.066374898930352089 ) ) ;
#47505 = ORIENTED_EDGE ( 'NONE', *, *, #2945, .T. ) ;
#47506 = VECTOR ( 'NONE', #41968, 1000.000000000000000 ) ;
#47507 = ORIENTED_EDGE ( 'NONE', *, *, #38854, .F. ) ;
#47508 = VERTEX_POINT ( 'NONE', #68604 ) ;
#47509 = CARTESIAN_POINT ( 'NONE',  ( -118.4106078162223383, 42.93830006159886636, 11.84514837596003822 ) ) ;
#47510 = CARTESIAN_POINT ( 'NONE',  ( -180.3158531669106424, 95.51092859788506928, 63.02641839755398934 ) ) ;
#47511 = CARTESIAN_POINT ( 'NONE',  ( 132.9485794245231887, 40.87843215479638559, 71.31345729829673985 ) ) ;
#47512 = EDGE_LOOP ( 'NONE', ( #8101, #18120, #15669, #68417, #60968, #22518 ) ) ;
#47513 = EDGE_CURVE ( 'NONE', #36977, #29802, #45799, .T. ) ;
#47514 = CARTESIAN_POINT ( 'NONE',  ( -35.41676323786686709, 10.27805710077606172, 85.03917892935545808 ) ) ;
#47515 = CARTESIAN_POINT ( 'NONE',  ( 153.8366942494330658, 54.87992279068315327, 43.47454990642605566 ) ) ;
#47516 = CARTESIAN_POINT ( 'NONE',  ( -26.00000000000002132, 0.000000000000000000, 55.00000000000001421 ) ) ;
#47517 = B_SPLINE_CURVE_WITH_KNOTS ( 'NONE', 3,
 ( #66902, #29249, #19034, #23969, #66554, #14106, #34544, #51053, #56672, #8842, #46108, #24674, #40487, #45421, #29941, #18697, #51406, #67579, #39453, #34191, #2863, #35215, #2518, #13757, #45069, #24331, #67251, #3218, #35567, #61259, #30292, #19378, #40152, #40835, #7455, #28911, #2176, #18340, #50360, #13080 ),
 .UNSPECIFIED., .F., .F.,
 ( 4, 2, 2, 2, 2, 2, 2, 2, 2, 2, 2, 2, 2, 2, 2, 2, 2, 2, 2, 4 ),
 ( 0.02472759712254455136, 0.02626001169882808198, 0.02779242627511161259, 0.02932484085139513974, 0.03009104813953688423, 0.03085725542767862525, 0.03238967000396209689, 0.03315587729210384138, 0.03392208458024558587, 0.03545449915652906098, 0.03698691373281253608, 0.03851932830909601813, 0.04005174288537949323, 0.04158415746166296834, 0.04311657203794644344, 0.04464898661422991855, 0.04541519390237165610, 0.04618140119051339365, 0.04771381576679689651, 0.04924623034308039243 ),
 .UNSPECIFIED. ) ;
#47518 = CARTESIAN_POINT ( 'NONE',  ( 102.7425154123292828, 25.56407025871219574, -43.66414440344461667 ) ) ;
#47519 = CARTESIAN_POINT ( 'NONE',  ( 0.000000000000000000, 0.000000000000000000, 40.00000000000003553 ) ) ;
#47520 = CARTESIAN_POINT ( 'NONE',  ( -142.3260422482981085, 59.60034523324940636, -66.92270134455016262 ) ) ;
#47521 = ORIENTED_EDGE ( 'NONE', *, *, #31275, .T. ) ;
#47522 = LINE ( 'NONE', #9920, #36521 ) ;
#47523 = CARTESIAN_POINT ( 'NONE',  ( -86.15466590221105037, 26.40813842494318209, -68.96785203774670947 ) ) ;
#47524 = CARTESIAN_POINT ( 'NONE',  ( 174.9099402067543565, 73.96774984027643995, 14.23027204521179279 ) ) ;
#47525 = LINE ( 'NONE', #46161, #9875 ) ;
#47526 = CARTESIAN_POINT ( 'NONE',  ( -80.32755469740936860, 24.04130076192507204, 18.39130622474332100 ) ) ;
#47527 = LINE ( 'NONE', #19431, #24743 ) ;
#47528 = CARTESIAN_POINT ( 'NONE',  ( 37.76166711006369070, 8.201557253608928733, -89.47894714693738649 ) ) ;
#47529 = DIRECTION ( 'NONE',  ( -0.000000000000000000, -0.000000000000000000, -1.000000000000000000 ) ) ;
#47530 = EDGE_CURVE ( 'NONE', #20487, #59656, #12752, .T. ) ;
#47531 = CARTESIAN_POINT ( 'NONE',  ( 70.11766033381772445, 14.43277633974326690, 8.007630405225276249 ) ) ;
#47532 = CARTESIAN_POINT ( 'NONE',  ( 158.3595886390531575, 58.34525996025799799, 2.604644620584485093 ) ) ;
#47533 = CARTESIAN_POINT ( 'NONE',  ( 42.02161712141799654, -26.09918303830819042, 30.00000000000000000 ) ) ;
#47534 = ORIENTED_EDGE ( 'NONE', *, *, #32799, .T. ) ;
#47535 = AXIS2_PLACEMENT_3D ( 'NONE', #64109, #37716, #15920 ) ;
#47536 = ITEM_DEFINED_TRANSFORMATION ( 'NONE', 'NONE', #15237,  #66832 ) ;
#47537 = CARTESIAN_POINT ( 'NONE',  ( -10.27459178052906097, 50.63337688185094976, 26.66469104408689006 ) ) ;
#47538 = ORIENTED_EDGE ( 'NONE', *, *, #46190, .F. ) ;
#47539 = DIRECTION ( 'NONE',  ( 0.000000000000000000, 0.000000000000000000, 1.000000000000000000 ) ) ;
#47540 = VERTEX_POINT ( 'NONE', #25712 ) ;
#47541 = CARTESIAN_POINT ( 'NONE',  ( 21.43750346857337874, 7.754771113113079650, -64.90611682194166576 ) ) ;
#47542 = VECTOR ( 'NONE', #66105, 1000.000000000000000 ) ;
#47543 = CARTESIAN_POINT ( 'NONE',  ( -29.87147652227455552, -74.98256102853682137, 133.5802547743875550 ) ) ;
#47544 = CARTESIAN_POINT ( 'NONE',  ( 24.34685647903079442, -70.88683439560421107, 41.38025477438755928 ) ) ;
#47545 = EDGE_CURVE ( 'NONE', #60060, #68173, #18366, .T. ) ;
#47546 = CARTESIAN_POINT ( 'NONE',  ( 65.62848231372475993, 13.29388722724788963, -23.41044504611049248 ) ) ;
#47547 = DIRECTION ( 'NONE',  ( 0.000000000000000000, -0.000000000000000000, -1.000000000000000000 ) ) ;
#47548 = CARTESIAN_POINT ( 'NONE',  ( 33.76124497394583557, 7.742545529019357886, -38.15270983885158529 ) ) ;
#47549 = VECTOR ( 'NONE', #23793, 1000.000000000000000 ) ;
#47550 = CARTESIAN_POINT ( 'NONE',  ( -48.41612563322100016, -170.0000000000000000, 94.99999999999866418 ) ) ;
#47551 = CARTESIAN_POINT ( 'NONE',  ( 13.56909401489541800, -65.06753427964257241, 133.5802547743875550 ) ) ;
#47552 = CARTESIAN_POINT ( 'NONE',  ( 74.95140232871122521, 0.000000000000000000, 41.38025477438755928 ) ) ;
#47553 = VERTEX_POINT ( 'NONE', #67578 ) ;
#47554 = VECTOR ( 'NONE', #54794, 999.9999999999998863 ) ;
#47555 = ORIENTED_EDGE ( 'NONE', *, *, #63993, .F. ) ;
#47556 = VECTOR ( 'NONE', #44309, 1000.000000000000000 ) ;
#47557 = CARTESIAN_POINT ( 'NONE',  ( 0.000000000000000000, 0.000000000000000000, 41.38025477438755928 ) ) ;
#47558 = CARTESIAN_POINT ( 'NONE',  ( 264.4165763529819628, 225.8585178651493948, 108.9999999999999858 ) ) ;
#47559 = AXIS2_PLACEMENT_3D ( 'NONE', #15595, #63787, #32116 ) ;
#47560 = CARTESIAN_POINT ( 'NONE',  ( 290.0000000000000568, 0.000000000000000000, -19.99999999999997868 ) ) ;
#47561 = EDGE_CURVE ( 'NONE', #36732, #31926, #15472, .T. ) ;
#47562 = VECTOR ( 'NONE', #19905, 999.9999999999998863 ) ;
#47563 = EDGE_CURVE ( 'NONE', #35686, #61651, #53443, .T. ) ;
#47564 = CARTESIAN_POINT ( 'NONE',  ( 63.01563776193090405, 13.70579113808096672, -89.40979201309708913 ) ) ;
#47565 = DIRECTION ( 'NONE',  ( 0.000000000000000000, 0.000000000000000000, 1.000000000000000000 ) ) ;
#47566 = CARTESIAN_POINT ( 'NONE',  ( 182.7745872728868051, 81.77554423487161728, -9.523131544683039351 ) ) ;
#47567 = CARTESIAN_POINT ( 'NONE',  ( 181.0840389613909736, 78.60582251573003987, -78.06960825634331513 ) ) ;
#47568 = FACE_OUTER_BOUND ( 'NONE', #43427, .T. ) ;
#47569 = CARTESIAN_POINT ( 'NONE',  ( 88.53517449242357884, 20.08005703101044759, -9.219238925436826548 ) ) ;
#47570 = CYLINDRICAL_SURFACE ( 'NONE', #11753, 5.000000000000004441 ) ;
#47571 = CARTESIAN_POINT ( 'NONE',  ( 60.40479419793796012, -24.00543350795314979, 170.0000000000000000 ) ) ;
#47572 = CARTESIAN_POINT ( 'NONE',  ( 163.7379901688713630, 64.00402364591251114, 67.88120199201151195 ) ) ;
#47573 = APPLICATION_CONTEXT ( 'automotive_design' ) ;
#47574 = ORIENTED_EDGE ( 'NONE', *, *, #15554, .T. ) ;
#47575 = FACE_OUTER_BOUND ( 'NONE', #50985, .T. ) ;
#47576 = LINE ( 'NONE', #31422, #65347 ) ;
#47577 = CARTESIAN_POINT ( 'NONE',  ( 133.8566784816069344, -170.0000000000000000, 56.35489142945903751 ) ) ;
#47578 = DIRECTION ( 'NONE',  ( 0.000000000000000000, 0.000000000000000000, 1.000000000000000000 ) ) ;
#47579 = CARTESIAN_POINT ( 'NONE',  ( 149.9838583332408462, 52.05699766415860097, 9.536419267673462485 ) ) ;
#47580 = CARTESIAN_POINT ( 'NONE',  ( 230.9999999999999432, 190.0000000000000000, -2.000000000000000000 ) ) ;
#47581 = ORIENTED_EDGE ( 'NONE', *, *, #20789, .F. ) ;
#47582 = CARTESIAN_POINT ( 'NONE',  ( 149.5059104800819796, -64.94516058774519252, -90.98255102680806772 ) ) ;
#47583 = DIRECTION ( 'NONE',  ( -0.000000000000000000, 1.000000000000000000, -0.000000000000000000 ) ) ;
#47584 = ORIENTED_EDGE ( 'NONE', *, *, #45185, .T. ) ;
#47585 = VERTEX_POINT ( 'NONE', #12201 ) ;
#47586 = CIRCLE ( 'NONE', #50983, 5.000000000000000888 ) ;
#47587 = CARTESIAN_POINT ( 'NONE',  ( 31.97180862241589949, 8.570158524060584426, 89.88509897528000181 ) ) ;
#47588 = LINE ( 'NONE', #30749, #35522 ) ;
#47589 = CARTESIAN_POINT ( 'NONE',  ( 31.89651141207536256, 56.63578868294628421, 170.0000000000000000 ) ) ;
#47590 = ORIENTED_EDGE ( 'NONE', *, *, #25293, .T. ) ;
#47591 = CYLINDRICAL_SURFACE ( 'NONE', #30055, 7.500000000000020428 ) ;
#47592 = CARTESIAN_POINT ( 'NONE',  ( -102.2801239173131052, 33.91021738430207222, 72.36362509687883460 ) ) ;
#47593 = AXIS2_PLACEMENT_3D ( 'NONE', #37524, #65310, #54384 ) ;
#47594 = CARTESIAN_POINT ( 'NONE',  ( -0.7076388175553621762, 7.538734751903869657, 8.356667854065962686 ) ) ;
#47595 = CARTESIAN_POINT ( 'NONE',  ( 173.6024011093111028, 72.73634049052009232, -44.32818560226256466 ) ) ;
#47596 = CARTESIAN_POINT ( 'NONE',  ( -154.7826623253030220, 70.14150242829521176, -74.49430738417227360 ) ) ;
#47597 = CIRCLE ( 'NONE', #67871, 5.000000000000004441 ) ;
#47598 = CYLINDRICAL_SURFACE ( 'NONE', #30917, 19.99999999999998934 ) ;
#47599 = ADVANCED_FACE ( 'NONE', ( #26393 ), #44556, .F. ) ;
#47600 = VECTOR ( 'NONE', #29074, 1000.000000000000114 ) ;
#47601 = ORIENTED_EDGE ( 'NONE', *, *, #51926, .F. ) ;
#47602 = CIRCLE ( 'NONE', #2698, 74.95140232871122521 ) ;
#47604 = EDGE_CURVE ( 'NONE', #59849, #51881, #8283, .T. ) ;
#47603 = CARTESIAN_POINT ( 'NONE',  ( 106.6322547488295385, 28.34756922280617530, -23.16909260820694882 ) ) ;
#47605 = AXIS2_PLACEMENT_3D ( 'NONE', #65346, #38969, #5890 ) ;
#47606 = CARTESIAN_POINT ( 'NONE',  ( 26.69682282325795697, -59.27986298182186431, 170.0000000000000000 ) ) ;
#47607 = CYLINDRICAL_SURFACE ( 'NONE', #12737, 7.500000000000013323 ) ;
#47608 = CARTESIAN_POINT ( 'NONE',  ( -65.36598343705435354, 0.000000000000000000, 41.38025477438755928 ) ) ;
#47609 = LINE ( 'NONE', #16644, #58955 ) ;
#47611 = ORIENTED_EDGE ( 'NONE', *, *, #57243, .F. ) ;
#47610 = DIRECTION ( 'NONE',  ( -0.08963930890342655666, -0.9959742939952397345, 2.500042656554808861E-16 ) ) ;
#47612 = ORIENTED_EDGE ( 'NONE', *, *, #5955, .F. ) ;
#47613 = VECTOR ( 'NONE', #34194, 1000.000000000000000 ) ;
#47614 = ORIENTED_EDGE ( 'NONE', *, *, #50356, .F. ) ;
#47615 = CARTESIAN_POINT ( 'NONE',  ( 117.3145357257065484, 33.41973663092564095, -67.71684323464012323 ) ) ;
#47616 = DIRECTION ( 'NONE',  ( 1.850169831522831466E-16, -1.000000000000000000, -1.110223024625156294E-16 ) ) ;
#47617 = CARTESIAN_POINT ( 'NONE',  ( 199.3671895066314619, 99.30947926630331324, -75.97069292755713832 ) ) ;
#47618 = EDGE_CURVE ( 'NONE', #8388, #10885, #55094, .T. ) ;
#47619 = CARTESIAN_POINT ( 'NONE',  ( -24.02131556907225018, 34.12171082077519202, 13.79046412364926688 ) ) ;
#47620 = ADVANCED_FACE ( 'NONE', ( #15827 ), #26048, .F. ) ;
#47621 = CARTESIAN_POINT ( 'NONE',  ( -15.13464256769236016, 8.488509377255644139, -14.37503968884516858 ) ) ;
#47622 = CARTESIAN_POINT ( 'NONE',  ( 153.4268936273268764, 54.57409659828384463, -76.78973794846126566 ) ) ;
#47623 = CARTESIAN_POINT ( 'NONE',  ( -417.6627218934913230, 399.9999999999997726, 113.5502958579881891 ) ) ;
#47624 = DIRECTION ( 'NONE',  ( 1.000000000000000000, 0.000000000000000000, 0.000000000000000000 ) ) ;
#47625 = ORIENTED_EDGE ( 'NONE', *, *, #5149, .T. ) ;
#47626 = ORIENTED_EDGE ( 'NONE', *, *, #58189, .T. ) ;
#47627 = EDGE_CURVE ( 'NONE', #22457, #15914, #68935, .T. ) ;
#47628 = CARTESIAN_POINT ( 'NONE',  ( 70.46579300139245561, 15.56614468937218909, -15.37766843719409593 ) ) ;
#47629 = CARTESIAN_POINT ( 'NONE',  ( -81.23268307104841313, 24.39742801172156916, -49.66676133314191333 ) ) ;
#47630 = CARTESIAN_POINT ( 'NONE',  ( 102.7985695539029791, 25.58774450393820388, 91.77657224901672350 ) ) ;
#47631 = ADVANCED_FACE ( 'NONE', ( #4924 ), #37270, .T. ) ;
#47632 = CARTESIAN_POINT ( 'NONE',  ( -152.9008427825211243, 68.45483453645057637, 4.684046598983249154 ) ) ;
#47633 = EDGE_CURVE ( 'NONE', #4404, #24527, #10538, .T. ) ;
#47634 = LINE ( 'NONE', #58204, #56203 ) ;
#47635 = CARTESIAN_POINT ( 'NONE',  ( 22.89234820949993576, 6.832052815347870123, 35.09748061321546686 ) ) ;
#47636 = CARTESIAN_POINT ( 'NONE',  ( -189.4202820252412494, 108.5506294086428625, -93.67079659341260367 ) ) ;
#47637 = ORIENTED_EDGE ( 'NONE', *, *, #12559, .F. ) ;
#47638 = EDGE_LOOP ( 'NONE', ( #12130, #5394, #478, #3117, #31640, #63206, #4330, #5305, #38622, #28855, #38800, #57626, #65914, #20363, #21753, #13556, #4645, #32088, #5145, #2632, #43999, #69256, #8942 ) ) ;
#47639 = ORIENTED_EDGE ( 'NONE', *, *, #40094, .T. ) ;
#47640 = DIRECTION ( 'NONE',  ( -0.9839295885986321100, 0.1785568947986229116, 0.000000000000000000 ) ) ;
#47641 = CARTESIAN_POINT ( 'NONE',  ( 91.73702110022665579, 22.29915270480343992, -91.50358301110458115 ) ) ;
#47642 = CARTESIAN_POINT ( 'NONE',  ( 108.3281565346183015, 28.00578413698477931, -89.84965755605794868 ) ) ;
#47643 = EDGE_CURVE ( 'NONE', #50410, #9782, #7601, .T. ) ;
#47644 = VECTOR ( 'NONE', #7008, 1000.000000000000000 ) ;
#47645 = CARTESIAN_POINT ( 'NONE',  ( -36.89224332184166144, 11.57404295377976311, -74.81660943836889999 ) ) ;
#47646 = ADVANCED_FACE ( 'NONE', ( #36945 ), #31661, .F. ) ;
#47647 = CARTESIAN_POINT ( 'NONE',  ( 202.7540649946183464, 105.3989460363904840, 56.29713274085410291 ) ) ;
#47648 = EDGE_CURVE ( 'NONE', #49666, #64350, #53609, .T. ) ;
#47649 = ORIENTED_EDGE ( 'NONE', *, *, #40986, .F. ) ;
#47650 = EDGE_CURVE ( 'NONE', #43631, #8643, #54770, .T. ) ;
#47651 = AXIS2_PLACEMENT_3D ( 'NONE', #10588, #5327, #26783 ) ;
#47652 = CARTESIAN_POINT ( 'NONE',  ( 34.45817031441433897, 7.817703378455679086, 58.59672298083805231 ) ) ;
#47653 = CARTESIAN_POINT ( 'NONE',  ( 9.058156535714475766, 6.378495712187264743, -19.49345657520668240 ) ) ;
#47654 = CARTESIAN_POINT ( 'NONE',  ( 18.88468164817599160, 7.626722602998420086, 3.834753717211726087 ) ) ;
#47655 = CARTESIAN_POINT ( 'NONE',  ( 187.9007786055418308, 85.78077355327278042, 66.79259192409129753 ) ) ;
#47656 = PLANE ( 'NONE',  #19655 ) ;
#47657 = CARTESIAN_POINT ( 'NONE',  ( -86.06016868996611890, 25.27707703029502184, -41.33193578213184338 ) ) ;
#47658 = DIRECTION ( 'NONE',  ( 1.000000000000000000, 1.387778780781446169E-16, 0.000000000000000000 ) ) ;
#47659 = DIRECTION ( 'NONE',  ( 0.000000000000000000, 0.000000000000000000, -1.000000000000000000 ) ) ;
#47660 = CARTESIAN_POINT ( 'NONE',  ( 12.91653430408660519, 7.431946598423013306, 3.728854190381519551 ) ) ;
#47661 = AXIS2_PLACEMENT_3D ( 'NONE', #15608, #36725, #38349 ) ;
#47662 = EDGE_LOOP ( 'NONE', ( #26056, #39023, #39960, #26245 ) ) ;
#47663 = CARTESIAN_POINT ( 'NONE',  ( 181.0840389613909736, 78.60582251573002566, 17.46404351504774510 ) ) ;
#47664 = PRODUCT_CONTEXT ( 'NONE', #66008, 'mechanical' ) ;
#47665 = CARTESIAN_POINT ( 'NONE',  ( 177.5945652320814361, 75.14951358071817822, 43.45125508251556568 ) ) ;
#47666 = CARTESIAN_POINT ( 'NONE',  ( -35.66505502203998645, -56.29927565066983419, 34.48241823996503541 ) ) ;
#47667 = CARTESIAN_POINT ( 'NONE',  ( -104.1393288135078024, 34.86912007524090029, -35.23351094377062509 ) ) ;
#47668 = DIRECTION ( 'NONE',  ( 0.000000000000000000, -1.000000000000000000, 0.000000000000000000 ) ) ;
#47669 = VERTEX_POINT ( 'NONE', #33666 ) ;
#47670 = ORIENTED_EDGE ( 'NONE', *, *, #20789, .T. ) ;
#47671 = CARTESIAN_POINT ( 'NONE',  ( -24.07146903340143851, 8.497560047608724076, -14.50675576945464051 ) ) ;
#47672 = CARTESIAN_POINT ( 'NONE',  ( 174.1712199980251796, 71.89075529249559793, 87.58217343572140123 ) ) ;
#47673 = ORIENTED_EDGE ( 'NONE', *, *, #52779, .T. ) ;
#47674 = CARTESIAN_POINT ( 'NONE',  ( 111.1868021579656869, 29.32055685204858619, 71.41117935951764650 ) ) ;
#47675 = ORIENTED_EDGE ( 'NONE', *, *, #45524, .F. ) ;
#47676 = CARTESIAN_POINT ( 'NONE',  ( 113.8626313173126050, 31.71036178495293711, 70.54171001663286233 ) ) ;
#47677 = CARTESIAN_POINT ( 'NONE',  ( 133.8566784816069344, 41.42467568809808398, 29.51034083899533300 ) ) ;
#47678 = FACE_OUTER_BOUND ( 'NONE', #31520, .T. ) ;
#47679 = CARTESIAN_POINT ( 'NONE',  ( 309.8720357909272707, 0.000000000000000000, 256.6193948016162381 ) ) ;
#47680 = CARTESIAN_POINT ( 'NONE',  ( -36.11269837220812207, -31.11269837220801193, 2.000000000000000000 ) ) ;
#47682 = VERTEX_POINT ( 'NONE', #58722 ) ;
#47681 = CARTESIAN_POINT ( 'NONE',  ( -64.18058723658641895, -10.37664328995269791, 3.061616997868437868E-16 ) ) ;
#47683 = DIRECTION ( 'NONE',  ( -1.000000000000000000, 0.000000000000000000, 0.000000000000000000 ) ) ;
#47684 = VERTEX_POINT ( 'NONE', #28018 ) ;
#47685 = ORIENTED_EDGE ( 'NONE', *, *, #11568, .T. ) ;
#47687 = EDGE_CURVE ( 'NONE', #4856, #58000, #64016, .T. ) ;
#47686 = CARTESIAN_POINT ( 'NONE',  ( -119.2982054035570911, 42.30181775808004829, -19.14876710156486794 ) ) ;
#47688 = VECTOR ( 'NONE', #11191, 1000.000000000000000 ) ;
#47689 = CARTESIAN_POINT ( 'NONE',  ( 311.9975424824652350, 170.0000000000000284, 256.6193948016162381 ) ) ;
#47690 = CARTESIAN_POINT ( 'NONE',  ( -180.2244609727085276, 95.39945930389644957, -17.79149012421619247 ) ) ;
#47691 = CARTESIAN_POINT ( 'NONE',  ( 133.8566784816069060, 41.42467568809810530, 56.35489142945903751 ) ) ;
#47693 = ORIENTED_EDGE ( 'NONE', *, *, #28231, .F. ) ;
#47692 = LINE ( 'NONE', #60342, #20858 ) ;
#47694 = DIRECTION ( 'NONE',  ( -0.7071067811865475727, 0.000000000000000000, -0.7071067811865474617 ) ) ;
#47695 = VERTEX_POINT ( 'NONE', #15493 ) ;
#47696 = B_SPLINE_CURVE_WITH_KNOTS ( 'NONE', 3,
 ( #33860, #23654, #67278, #7486, #50722, #18371 ),
 .UNSPECIFIED., .F., .F.,
 ( 4, 2, 4 ),
 ( 0.03218934490037906465, 0.06469832469447792112, 0.09720730448857675676 ),
 .UNSPECIFIED. ) ;
#47697 = CARTESIAN_POINT ( 'NONE',  ( -61.51762070241279190, 16.51067482779403761, -12.06156012046973736 ) ) ;
#47698 = AXIS2_PLACEMENT_3D ( 'NONE', #43496, #38227, #33321 ) ;
#47699 = EDGE_CURVE ( 'NONE', #3371, #36808, #54746, .T. ) ;
#47700 = EDGE_CURVE ( 'NONE', #12944, #66081, #9971, .T. ) ;
#47701 = VECTOR ( 'NONE', #63537, 1000.000000000000227 ) ;
#47702 = ADVANCED_FACE ( 'NONE', ( #2686 ), #7275, .T. ) ;
#47703 = CARTESIAN_POINT ( 'NONE',  ( 70.65683382808231272, -25.18281821780013274, 170.0000000000000000 ) ) ;
#47704 = CARTESIAN_POINT ( 'NONE',  ( 59.86221654654867308, 11.96331997874669284, -90.10186521222453848 ) ) ;
#47705 = AXIS2_PLACEMENT_3D ( 'NONE', #26000, #31962, #53389 ) ;
#47706 = CARTESIAN_POINT ( 'NONE',  ( -95.88718821240200896, 29.65015105908827309, 7.244506905266613117 ) ) ;
#47707 = CARTESIAN_POINT ( 'NONE',  ( -97.85576954355164503, 30.58918648956191788, -63.28394810425090355 ) ) ;
#47708 = ORIENTED_EDGE ( 'NONE', *, *, #49704, .F. ) ;
#47709 = ORIENTED_EDGE ( 'NONE', *, *, #39308, .T. ) ;
#47710 = EDGE_CURVE ( 'NONE', #20984, #66775, #24834, .T. ) ;
#47711 = CARTESIAN_POINT ( 'NONE',  ( 184.3994103300443044, 82.02159554764423888, -63.82720643750994327 ) ) ;
#47712 = CARTESIAN_POINT ( 'NONE',  ( -26.83517958587572494, -59.60356471962950309, 41.38025477438755928 ) ) ;
#47713 = FACE_OUTER_BOUND ( 'NONE', #46663, .T. ) ;
#47714 = EDGE_CURVE ( 'NONE', #37653, #805, #32558, .T. ) ;
#47715 = CARTESIAN_POINT ( 'NONE',  ( 105.7953515382195917, 27.97683113100023178, -64.20869765785622008 ) ) ;
#47716 = CARTESIAN_POINT ( 'NONE',  ( -71.26746920569853216, 20.70422440535243069, 36.66531925523995028 ) ) ;
#47717 = CARTESIAN_POINT ( 'NONE',  ( -74.20136529587824725, 21.74007521413448885, -63.42900937661281802 ) ) ;
#47718 = CARTESIAN_POINT ( 'NONE',  ( 67.55199883153194662, 14.80832170058782182, -49.21298022547202322 ) ) ;
#47719 = CARTESIAN_POINT ( 'NONE',  ( -125.6703656163501392, 47.55170550253210848, 30.61994787315705935 ) ) ;
#47720 = CARTESIAN_POINT ( 'NONE',  ( 212.1962110267000128, 117.2292732107321456, 63.17560925674016659 ) ) ;
#47721 = ORIENTED_EDGE ( 'NONE', *, *, #6848, .F. ) ;
#47722 = CARTESIAN_POINT ( 'NONE',  ( -36.61438981621043354, -5.226566692248933776, 4.385610183789545147 ) ) ;
#47723 = EDGE_LOOP ( 'NONE', ( #6414, #7216, #46475, #29176 ) ) ;
#47724 = CARTESIAN_POINT ( 'NONE',  ( -32.41982179707237322, 9.753975577087190985, 3.420357701285721141 ) ) ;
#47725 = CARTESIAN_POINT ( 'NONE',  ( -149.5074843970971301, -170.0000000000000000, 38.22082123989905966 ) ) ;
#47726 = CARTESIAN_POINT ( 'NONE',  ( 93.87650740736111743, 23.09802612281733758, 62.06025712787139526 ) ) ;
#47727 = CARTESIAN_POINT ( 'NONE',  ( 150.4550062612853480, 52.39582885725847206, -14.07485114950216065 ) ) ;
#47728 = CARTESIAN_POINT ( 'NONE',  ( 53.32245423372616244, -37.19594572654634845, 170.0000000000000000 ) ) ;
#47729 = DIRECTION ( 'NONE',  ( 1.000000000000000000, -0.000000000000000000, 0.000000000000000000 ) ) ;
#47730 = CARTESIAN_POINT ( 'NONE',  ( 36.31593203568480988, 8.028139509847028066, -76.80444249456844830 ) ) ;
#47731 = CARTESIAN_POINT ( 'NONE',  ( 63.01563776193091826, -170.0000000000000000, 56.65751152968497451 ) ) ;
#47732 = CARTESIAN_POINT ( 'NONE',  ( -32.40928421737412890, 10.77259363352673560, -23.42573354065221025 ) ) ;
#47733 = ADVANCED_FACE ( 'NONE', ( #63500, #9341, #69456, #20579, #36776, #37107 ), #14283, .T. ) ;
#47734 = VERTEX_POINT ( 'NONE', #58548 ) ;
#47735 = CARTESIAN_POINT ( 'NONE',  ( -125.0779128240347973, 47.16111191621167364, -88.63580480530789885 ) ) ;
#47736 = ORIENTED_EDGE ( 'NONE', *, *, #34883, .F. ) ;
#47737 = PLANE ( 'NONE',  #1425 ) ;
#47738 = CARTESIAN_POINT ( 'NONE',  ( 15.78827728214693416, 7.507518794609589818, -77.36349468914950478 ) ) ;
#47740 = ADVANCED_FACE ( 'NONE', ( #58219 ), #4412, .T. ) ;
#47739 = CARTESIAN_POINT ( 'NONE',  ( -189.9638655956220248, 108.0957249433520815, 8.346787301602333287 ) ) ;
#47741 = FACE_OUTER_BOUND ( 'NONE', #42032, .T. ) ;
#47742 = CARTESIAN_POINT ( 'NONE',  ( -1.728570918131773881, 6.570609986804655023, 33.24078084807834443 ) ) ;
#47743 = CARTESIAN_POINT ( 'NONE',  ( 55.65793654284612302, 50.28674377798304107, 170.0000000000000000 ) ) ;
#47744 = CARTESIAN_POINT ( 'NONE',  ( 157.4703587214989113, 58.92748579479261650, -51.12418429913766005 ) ) ;
#47745 = VECTOR ( 'NONE', #53486, 1000.000000000000000 ) ;
#47746 = ORIENTED_EDGE ( 'NONE', *, *, #18535, .F. ) ;
#47747 = VECTOR ( 'NONE', #25763, 1000.000000000000000 ) ;
#47748 = CARTESIAN_POINT ( 'NONE',  ( 620.5071894358227382, 928.5915846175159913, 622.5068267248769871 ) ) ;
#47749 = CARTESIAN_POINT ( 'NONE',  ( -189.8071159312683847, 107.8771087123620021, -18.14639082933156189 ) ) ;
#47750 = CARTESIAN_POINT ( 'NONE',  ( 442.3372781065085064, 390.0000000000001137, -141.4497041420117398 ) ) ;
#47751 = CARTESIAN_POINT ( 'NONE',  ( -102.2801239173131052, 33.91021738430207222, 57.36362509687880618 ) ) ;
#47752 = CONTEXT_DEPENDENT_SHAPE_REPRESENTATION ( #4455, #62578 ) ;
#47753 = CARTESIAN_POINT ( 'NONE',  ( 0.2727178028659107412, 2.726369936601795653E-15, -21.02500000000000213 ) ) ;
#47754 = VERTEX_POINT ( 'NONE', #25877 ) ;
#47756 = CARTESIAN_POINT ( 'NONE',  ( 133.8566784816069344, -170.0000000000000000, -89.71241211332301191 ) ) ;
#47755 = CIRCLE ( 'NONE', #37657, 500.0000000000000000 ) ;
#47757 = CIRCLE ( 'NONE', #7361, 8.000000000000000000 ) ;
#47758 = B_SPLINE_CURVE_WITH_KNOTS ( 'NONE', 3,
 ( #8750, #19633, #41785, #61838 ),
 .UNSPECIFIED., .F., .F.,
 ( 4, 4 ),
 ( 9.900409499241261188E-07, 0.05658314289920116785 ),
 .UNSPECIFIED. ) ;
#47759 = CARTESIAN_POINT ( 'NONE',  ( 94.06703982324148683, 22.09435144471461498, 65.05402493561722110 ) ) ;
#47760 = B_SPLINE_CURVE_WITH_KNOTS ( 'NONE', 3,
 ( #44021, #781, #28559, #44741, #27854, #44376, #60212, #49645, #54928, #49297, #7805, #2184, #1130, #11672, #66220, #29256, #50003, #18007, #43673, #22233, #60908, #22581, #65863, #23636, #1473, #12730, #45074, #66558, #17660, #17298, #55280, #18347, #6749, #39809, #14110, #50705, #8144, #40157, #67255, #46457 ),
 .UNSPECIFIED., .F., .F.,
 ( 4, 2, 2, 2, 2, 2, 2, 2, 2, 2, 2, 2, 2, 2, 2, 2, 2, 2, 2, 4 ),
 ( 0.02472759712254455136, 0.02626001169882808198, 0.02779242627511160912, 0.02932484085139513974, 0.03009104813953688423, 0.03085725542767862872, 0.03238967000396208301, 0.03315587729210382750, 0.03392208458024557199, 0.03545449915652905404, 0.03698691373281252914, 0.03851932830909600425, 0.04005174288537947935, 0.04158415746166295446, 0.04311657203794642956, 0.04464898661422990467, 0.04541519390237164222, 0.04618140119051337977, 0.04771381576679689651, 0.04924623034308040631 ),
 .UNSPECIFIED. ) ;
#47761 =( GEOMETRIC_REPRESENTATION_CONTEXT ( 3 ) GLOBAL_UNCERTAINTY_ASSIGNED_CONTEXT ( ( #57108 ) ) GLOBAL_UNIT_ASSIGNED_CONTEXT ( ( #63074, #68362, #19826 ) ) REPRESENTATION_CONTEXT ( 'NONE', 'WORKASPACE' ) );
#47762 = CARTESIAN_POINT ( 'NONE',  ( 203.9203998321607685, 106.9845510704142129, -9.511358609132138042 ) ) ;
#47763 = VECTOR ( 'NONE', #28951, 1000.000000000000000 ) ;
#47764 = CARTESIAN_POINT ( 'NONE',  ( 78.57571471437144339, 6.000000000000000000, -20.00000000000000000 ) ) ;
#47765 = AXIS2_PLACEMENT_3D ( 'NONE', #13561, #60352, #3011 ) ;
#47766 = CARTESIAN_POINT ( 'NONE',  ( -1.118033988749894458, 0.000000000000000000, 0.000000000000000000 ) ) ;
#47767 = EDGE_LOOP ( 'NONE', ( #45985, #15964, #47123, #34133, #23210 ) ) ;
#47768 = CARTESIAN_POINT ( 'NONE',  ( 0.1306530452038140722, -5.952467836904157927, 5.690023276062402324 ) ) ;
#47769 = DIRECTION ( 'NONE',  ( 0.000000000000000000, 1.224646799147344826E-16, 1.000000000000000000 ) ) ;
#47770 = CARTESIAN_POINT ( 'NONE',  ( 161.7031777507227446, 62.31724004902784486, 16.27331598182586703 ) ) ;
#47771 = CARTESIAN_POINT ( 'NONE',  ( -99.10904156412040322, 32.31949011661294691, 44.83230361419195731 ) ) ;
#47772 = VERTEX_POINT ( 'NONE', #57878 ) ;
#47773 = CARTESIAN_POINT ( 'NONE',  ( 174.2538192999569731, 73.34752463892027663, 60.54307137167467090 ) ) ;
#47774 = ORIENTED_EDGE ( 'NONE', *, *, #40424, .F. ) ;
#47776 = EDGE_CURVE ( 'NONE', #59523, #33643, #12380, .T. ) ;
#47775 = DIRECTION ( 'NONE',  ( 1.000000000000000000, -0.000000000000000000, -0.000000000000000000 ) ) ;
#47777 = CARTESIAN_POINT ( 'NONE',  ( 67.92995549349549833, 13.86623459444476225, -75.75181126496241291 ) ) ;
#47778 = CARTESIAN_POINT ( 'NONE',  ( -59.56523643198714524, 15.93788386494078502, 43.81298497852716167 ) ) ;
#47779 = B_SPLINE_CURVE_WITH_KNOTS ( 'NONE', 3,
 ( #49934, #7390, #34124, #24266, #55924, #13699, #13020, #62224, #44674, #35504, #2455, #35151, #50631, #45712, #14045, #56606, #50989, #18283, #7737, #8073, #51343, #66149, #56965, #34481, #34819, #24614, #8430, #66842, #46048, #29189, #40088, #2804, #23909, #61871, #18630, #29881, #3158, #13362, #67189, #8785, #61543, #56256, #29522 ),
 .UNSPECIFIED., .F., .F.,
 ( 4, 2, 2, 2, 2, 2, 2, 2, 2, 2, 2, 2, 1, 2, 2, 2, 2, 2, 2, 2, 2, 4 ),
 ( 0.02371951416048009159, 0.02520633211177543409, 0.02594974108742308799, 0.02669315006307074190, 0.02817996801436604623, 0.02966678596566135057, 0.03041019494130899753, 0.03115360391695664102, 0.03264042186825193148, 0.03412723981954722541, 0.03561405777084253321, 0.03635746674649016630, 0.03710087572213779938, 0.03784428469778543941, 0.03858769367343307249, 0.04007451162472835948, 0.04156132957602363953, 0.04304814752731893346, 0.04379155650296658042, 0.04453496547861424126, 0.04602178342990954213, 0.04750860138120484993 ),
 .UNSPECIFIED. ) ;
#47781 = VERTEX_POINT ( 'NONE', #54662 ) ;
#47780 = CARTESIAN_POINT ( 'NONE',  ( 157.0316110297314083, 58.58403635656379294, 17.56491688178972055 ) ) ;
#47782 = CARTESIAN_POINT ( 'NONE',  ( 157.4703587214989113, 58.92748579479261650, -51.12418429913766005 ) ) ;
#47783 = PLANE ( 'NONE',  #39555 ) ;
#47784 = CARTESIAN_POINT ( 'NONE',  ( 111.1829448509513014, 30.43012797723691065, -35.96691630598188993 ) ) ;
#47785 = ORIENTED_EDGE ( 'NONE', *, *, #6461, .F. ) ;
#47786 = DIRECTION ( 'NONE',  ( -0.000000000000000000, -1.000000000000000000, -0.000000000000000000 ) ) ;
#47787 = EDGE_CURVE ( 'NONE', #9014, #7875, #37441, .T. ) ;
#47788 = VECTOR ( 'NONE', #18486, 1000.000000000000000 ) ;
#47789 = CARTESIAN_POINT ( 'NONE',  ( 141.3707934840545022, 46.15056991286794386, 63.82522392161691016 ) ) ;
#47790 = CARTESIAN_POINT ( 'NONE',  ( -175.1895962157337010, 90.99110972060688596, 31.10022776195569705 ) ) ;
#47791 = CARTESIAN_POINT ( 'NONE',  ( -36.37371824399145481, 10.45334302951138561, -75.33134930568731136 ) ) ;
#47792 = EDGE_CURVE ( 'NONE', #43717, #50848, #32186, .T. ) ;
#47793 = CARTESIAN_POINT ( 'NONE',  ( 188.2076037774874919, 86.11782719225436722, -19.24392630350066469 ) ) ;
#47794 = ORIENTED_EDGE ( 'NONE', *, *, #13502, .T. ) ;
#47796 = EDGE_CURVE ( 'NONE', #27271, #68798, #7653, .T. ) ;
#47795 = CARTESIAN_POINT ( 'NONE',  ( 45.76553115525427273, 10.34124506813254918, 6.592493761944549391 ) ) ;
#47797 = ORIENTED_EDGE ( 'NONE', *, *, #36619, .T. ) ;
#47798 = ORIENTED_EDGE ( 'NONE', *, *, #55044, .T. ) ;
#47799 = CARTESIAN_POINT ( 'NONE',  ( -21.03405120204975276, 13.73704776265648775, 3.061616997868437868E-16 ) ) ;
#47800 = EDGE_CURVE ( 'NONE', #34186, #64281, #4276, .T. ) ;
#47801 = CARTESIAN_POINT ( 'NONE',  ( 207.4566510040494904, 111.9649643341356438, -23.95860942766702806 ) ) ;
#47802 = AXIS2_PLACEMENT_3D ( 'NONE', #47395, #52347, #41107 ) ;
#47803 = AXIS2_PLACEMENT_3D ( 'NONE', #55376, #7564, #34650 ) ;
#47804 = CARTESIAN_POINT ( 'NONE',  ( 6.400000000000000355, -9.237604307034033013, -1.753283555911559014E-16 ) ) ;
#47805 = LINE ( 'NONE', #5582, #41188 ) ;
#47806 = CARTESIAN_POINT ( 'NONE',  ( -109.7047744410585608, 36.71529196001675643, 92.81931154901670311 ) ) ;
#47807 =( GEOMETRIC_REPRESENTATION_CONTEXT ( 3 ) GLOBAL_UNCERTAINTY_ASSIGNED_CONTEXT ( ( #4337 ) ) GLOBAL_UNIT_ASSIGNED_CONTEXT ( ( #21203, #80, #64450 ) ) REPRESENTATION_CONTEXT ( 'NONE', 'WORKASPACE' ) );
#47808 = CARTESIAN_POINT ( 'NONE',  ( 0.000000000000000000, -0.1068809833119260672, -91.05865558859387932 ) ) ;
#47809 = DIRECTION ( 'NONE',  ( 0.000000000000000000, 1.000000000000000000, 0.000000000000000000 ) ) ;
#47810 = DIRECTION ( 'NONE',  ( 0.000000000000000000, 0.000000000000000000, 1.000000000000000000 ) ) ;
#47811 = ORIENTED_EDGE ( 'NONE', *, *, #18928, .T. ) ;
#47812 = CARTESIAN_POINT ( 'NONE',  ( -97.90661117598844498, 31.73207306186866816, -90.10694785018394271 ) ) ;
#47813 = ORIENTED_EDGE ( 'NONE', *, *, #55020, .T. ) ;
#47814 = CARTESIAN_POINT ( 'NONE',  ( -76.78104518372333587, 22.68568622761703324, 57.48804312598085176 ) ) ;
#47815 = CYLINDRICAL_SURFACE ( 'NONE', #44184, 60.00000000000000000 ) ;
#47816 = CARTESIAN_POINT ( 'NONE',  ( 61.09275639403233527, 12.23448398202909893, -77.33071701894527905 ) ) ;
#47817 = CARTESIAN_POINT ( 'NONE',  ( -78.66644367742109978, 22.32174330031319442, 3.573650549209446137 ) ) ;
#47818 = FACE_OUTER_BOUND ( 'NONE', #36008, .T. ) ;
#47819 = CARTESIAN_POINT ( 'NONE',  ( 86.62931800182293784, 19.42108912189599579, 71.55663816294304524 ) ) ;
#47820 = CARTESIAN_POINT ( 'NONE',  ( 164.9700808964341547, 65.04346068891115351, -70.17999518051283303 ) ) ;
#47821 = VERTEX_POINT ( 'NONE', #42725 ) ;
#47822 = CARTESIAN_POINT ( 'NONE',  ( -71.22878586122430988, 19.62649588091169406, 65.76083851737067221 ) ) ;
#47823 = DIRECTION ( 'NONE',  ( 0.000000000000000000, 0.7071067811865474617, 0.7071067811865474617 ) ) ;
#47824 = VERTEX_POINT ( 'NONE', #32870 ) ;
#47825 = EDGE_CURVE ( 'NONE', #6663, #11578, #38139, .T. ) ;
#47826 = ORIENTED_EDGE ( 'NONE', *, *, #68753, .F. ) ;
#47827 = CARTESIAN_POINT ( 'NONE',  ( -8.000000000000000000, -1.555946510856143883, -0.06708870216335346970 ) ) ;
#47828 = CARTESIAN_POINT ( 'NONE',  ( 61.10129719786244351, 12.23677173834305165, -35.96503823067305206 ) ) ;
#47829 = CARTESIAN_POINT ( 'NONE',  ( 51.00231698266622260, -42.89951341137784624, 34.48241824007785539 ) ) ;
#47830 = CARTESIAN_POINT ( 'NONE',  ( 6.400000000000000355, -4.618802153517011178, 8.000000000000000000 ) ) ;
#47831 = DIRECTION ( 'NONE',  ( 0.000000000000000000, -1.000000000000000000, 0.000000000000000000 ) ) ;
#47832 = ORIENTED_EDGE ( 'NONE', *, *, #63330, .T. ) ;
#47833 = ORIENTED_EDGE ( 'NONE', *, *, #56596, .F. ) ;
#47834 = CARTESIAN_POINT ( 'NONE',  ( -131.2955621888335429, 51.38237199780174080, 32.89462560528686907 ) ) ;
#47835 = ORIENTED_EDGE ( 'NONE', *, *, #13517, .F. ) ;
#47836 = CARTESIAN_POINT ( 'NONE',  ( 37.46876540261052924, 9.179568636624027889, -23.52597108042403207 ) ) ;
#47837 = CARTESIAN_POINT ( 'NONE',  ( 188.1848725084043110, 87.59259440284084519, -95.00000000000133582 ) ) ;
#47838 = CARTESIAN_POINT ( 'NONE',  ( 207.4867844023104624, 110.2451255333963616, 43.68190180099020381 ) ) ;
#47839 = CARTESIAN_POINT ( 'NONE',  ( 0.000000000000000000, 0.000000000000000000, 43.58025477438756212 ) ) ;
#47840 = DIRECTION ( 'NONE',  ( -0.000000000000000000, -0.000000000000000000, -1.000000000000000000 ) ) ;
#47841 = AXIS2_PLACEMENT_3D ( 'NONE', #11030, #26528, #64853 ) ;
#47842 = VERTEX_POINT ( 'NONE', #33232 ) ;
#47843 = VERTEX_POINT ( 'NONE', #44102 ) ;
#47844 = CARTESIAN_POINT ( 'NONE',  ( 159.6593397521790223, 59.37286298965126718, -23.96695613349937304 ) ) ;
#47845 = DIRECTION ( 'NONE',  ( 0.000000000000000000, 0.000000000000000000, 1.000000000000000000 ) ) ;
#47846 = AXIS2_PLACEMENT_3D ( 'NONE', #61507, #39703, #44972 ) ;
#47847 = CARTESIAN_POINT ( 'NONE',  ( -165.9122696334864600, 79.44688201528256855, -17.45773735543971128 ) ) ;
#47848 = DIRECTION ( 'NONE',  ( -1.000000000000000000, 0.000000000000000000, 0.000000000000000000 ) ) ;
#47849 = DIRECTION ( 'NONE',  ( 0.000000000000000000, 0.000000000000000000, 1.000000000000000000 ) ) ;
#47850 = CARTESIAN_POINT ( 'NONE',  ( -190.3074740493607351, 108.5764897054613414, -72.83801848297902382 ) ) ;
#47851 = CIRCLE ( 'NONE', #22049, 10.00000000000000000 ) ;
#47852 = VECTOR ( 'NONE', #32467, 1000.000000000000114 ) ;
#47853 = ORIENTED_EDGE ( 'NONE', *, *, #62728, .F. ) ;
#47854 = AXIS2_PLACEMENT_3D ( 'NONE', #48420, #22760, #60398 ) ;
#47855 = CARTESIAN_POINT ( 'NONE',  ( -125.8938041572051389, -170.0000000000000000, 72.46449846362081360 ) ) ;
#47856 = AXIS2_PLACEMENT_3D ( 'NONE', #40200, #29633, #67629 ) ;
#47857 = CARTESIAN_POINT ( 'NONE',  ( -99.10260179032840711, 31.19580119595417855, 71.66143382347762270 ) ) ;
#47858 = EDGE_CURVE ( 'NONE', #56268, #30529, #58897, .T. ) ;
#47859 = ORIENTED_EDGE ( 'NONE', *, *, #66822, .T. ) ;
#47860 = CARTESIAN_POINT ( 'NONE',  ( -173.1211646369891355, -170.0000000000000000, -15.36740657428631351 ) ) ;
#47861 = ORIENTED_EDGE ( 'NONE', *, *, #38744, .F. ) ;
#47862 = AXIS2_PLACEMENT_3D ( 'NONE', #6905, #54737, #13491 ) ;
#47863 = EDGE_CURVE ( 'NONE', #58815, #41480, #64180, .T. ) ;
#47864 = EDGE_CURVE ( 'NONE', #66948, #53100, #10712, .T. ) ;
#47865 = ORIENTED_EDGE ( 'NONE', *, *, #33555, .T. ) ;
#47866 = CARTESIAN_POINT ( 'NONE',  ( -120.5002574492098972, 44.22930148497321312, 16.49287155969762253 ) ) ;
#47867 = CARTESIAN_POINT ( 'NONE',  ( -180.3153482337535536, 95.51031295027647161, 67.30752748117252793 ) ) ;
#47868 = CARTESIAN_POINT ( 'NONE',  ( 128.0568017572569204, 38.03085713813912605, 59.07289773574036218 ) ) ;
#47869 = VERTEX_POINT ( 'NONE', #21962 ) ;
#47870 = CARTESIAN_POINT ( 'NONE',  ( 60.82895951008428170, -30.68107831874537084, 170.0000000000000000 ) ) ;
#47871 = DIRECTION ( 'NONE',  ( -0.000000000000000000, 1.000000000000000000, -0.000000000000000000 ) ) ;
#47872 = CYLINDRICAL_SURFACE ( 'NONE', #47114, 65.00000000000000000 ) ;
#47873 = EDGE_CURVE ( 'NONE', #42825, #46238, #32339, .T. ) ;
#47874 = CARTESIAN_POINT ( 'NONE',  ( -102.2801239173131052, 33.91021738430207932, 30.51907450641510522 ) ) ;
#47875 = CARTESIAN_POINT ( 'NONE',  ( -31.43908319763710679, 9.591432048623758533, 45.21645440618919309 ) ) ;
#47877 = EDGE_CURVE ( 'NONE', #56862, #1104, #7546, .T. ) ;
#47876 = DIRECTION ( 'NONE',  ( -1.000000000000000000, 0.000000000000000000, 0.000000000000000000 ) ) ;
#47878 = ORIENTED_EDGE ( 'NONE', *, *, #59156, .F. ) ;
#47879 = FACE_BOUND ( 'NONE', #21423, .T. ) ;
#47880 = LINE ( 'NONE', #10589, #3933 ) ;
#47881 = CARTESIAN_POINT ( 'NONE',  ( -1.734723475976807094E-15, 9.237604307034022355, -8.785468820183664818 ) ) ;
#47882 = CARTESIAN_POINT ( 'NONE',  ( 117.3188760168912523, 32.29536350891957142, -94.58846656126689822 ) ) ;
#47883 = CARTESIAN_POINT ( 'NONE',  ( -119.1605144823340510, 43.39823405392971267, -45.72746398012520785 ) ) ;
#47884 = CARTESIAN_POINT ( 'NONE',  ( 26.12852347772543737, 70.00000000000000000, 77.58025477438755502 ) ) ;
#47885 = DIRECTION ( 'NONE',  ( 1.000000000000000000, 4.565061778886334783E-18, 0.000000000000000000 ) ) ;
#47886 = CARTESIAN_POINT ( 'NONE',  ( -154.2585856850055279, 68.31650218414623055, 5.568140700381407626 ) ) ;
#47887 = CARTESIAN_POINT ( 'NONE',  ( -118.5151419614604720, 43.00218563933586324, -67.88871905889871528 ) ) ;
#47888 = DIRECTION ( 'NONE',  ( 0.9510565162951544194, -0.3090169943749447312, 0.000000000000000000 ) ) ;
#47889 = CARTESIAN_POINT ( 'NONE',  ( -81.24432217070638274, 24.40203426192927338, 71.80983157096119385 ) ) ;
#47890 = CARTESIAN_POINT ( 'NONE',  ( 90.51709546286271291, 21.85407654229979357, -22.89523223895175974 ) ) ;
#47891 = EDGE_LOOP ( 'NONE', ( #63573, #25417, #20567, #17203 ) ) ;
#47892 = AXIS2_PLACEMENT_3D ( 'NONE', #31222, #21002, #11127 ) ;
#47893 = VERTEX_POINT ( 'NONE', #61347 ) ;
#47894 = DIRECTION ( 'NONE',  ( 0.000000000000000000, 0.000000000000000000, 1.000000000000000000 ) ) ;
#47895 = ORIENTED_EDGE ( 'NONE', *, *, #65597, .F. ) ;
#47896 = CARTESIAN_POINT ( 'NONE',  ( -196.7348448768811409, -170.0000000000000000, -42.11108379800802481 ) ) ;
#47897 = CIRCLE ( 'NONE', #54624, 21.50000000000000000 ) ;
#47898 = CARTESIAN_POINT ( 'NONE',  ( 0.000000000000000000, 0.000000000000000000, -10.00000000000000000 ) ) ;
#47899 = CARTESIAN_POINT ( 'NONE',  ( -19.15041326417105338, -47.98507813326755667, 26.66469066592269144 ) ) ;
#47900 = DIRECTION ( 'NONE',  ( 0.000000000000000000, 0.000000000000000000, 1.000000000000000000 ) ) ;
#47901 = CIRCLE ( 'NONE', #68165, 5.000000000000170530 ) ;
#47902 = CARTESIAN_POINT ( 'NONE',  ( -51.13576748034041941, 14.70354244225167584, -75.96136548085722495 ) ) ;
#47903 = ORIENTED_EDGE ( 'NONE', *, *, #67800, .F. ) ;
#47904 = CARTESIAN_POINT ( 'NONE',  ( 417.3372781065085633, 394.9999999999999432, 83.55029585798834546 ) ) ;
#47905 = CARTESIAN_POINT ( 'NONE',  ( -122.8202784017355356, 45.69728649588467562, -8.723847309115170034 ) ) ;
#47906 = ORIENTED_EDGE ( 'NONE', *, *, #70, .T. ) ;
#47907 = ORIENTED_EDGE ( 'NONE', *, *, #23350, .F. ) ;
#47908 = CARTESIAN_POINT ( 'NONE',  ( 69.08240197259638649, 14.16210831900843381, -47.63718284325325669 ) ) ;
#47909 = CARTESIAN_POINT ( 'NONE',  ( 173.7502847382833693, 72.87471067097989419, 92.08090874032060924 ) ) ;
#47910 = VECTOR ( 'NONE', #34502, 999.9999999999998863 ) ;
#47911 = CARTESIAN_POINT ( 'NONE',  ( 36.30976181811464443, 12.29214648180296088, 13.32819397642331971 ) ) ;
#47912 = DIRECTION ( 'NONE',  ( -1.000000000000000000, 0.000000000000000000, -0.000000000000000000 ) ) ;
#47913 = PLANE ( 'NONE',  #26303 ) ;
#47914 = CARTESIAN_POINT ( 'NONE',  ( 284.9668435325538667, 21.99239968880144502, -0.6609596067687139032 ) ) ;
#47915 = CARTESIAN_POINT ( 'NONE',  ( -15.26524495591509201, 7.490231452641286758, 63.48037225783858872 ) ) ;
#47916 = CARTESIAN_POINT ( 'NONE',  ( -83.12901536265222546, 24.07178615860086524, -9.738105063539622464 ) ) ;
#47917 = CARTESIAN_POINT ( 'NONE',  ( 0.000000000000000000, 50.00000000000000000, 0.000000000000000000 ) ) ;
#47918 = FACE_OUTER_BOUND ( 'NONE', #66324, .T. ) ;
#47919 = CARTESIAN_POINT ( 'NONE',  ( -55.05276343752910151, -170.0000000000000000, -42.71632399845987749 ) ) ;
#47920 = CARTESIAN_POINT ( 'NONE',  ( 109.9975424824652777, 172.0000000000000284, 418.0000000000000000 ) ) ;
#47921 = CARTESIAN_POINT ( 'NONE',  ( 164.4760519199596160, 64.62478832434433684, 66.48423307707000163 ) ) ;
#47922 = ORIENTED_EDGE ( 'NONE', *, *, #54705, .F. ) ;
#47923 = CARTESIAN_POINT ( 'NONE',  ( 0.000000000000000000, 23.07878402833891229, 5.000000000000000000 ) ) ;
#47924 = CARTESIAN_POINT ( 'NONE',  ( 89.88147981065576175, 21.62466191578946351, -36.54612782466419674 ) ) ;
#47925 = CARTESIAN_POINT ( 'NONE',  ( 152.1153500913667642, 54.85403770686895086, 69.01100629273766174 ) ) ;
#47926 = LINE ( 'NONE', #39138, #39992 ) ;
#47927 = CARTESIAN_POINT ( 'NONE',  ( 150.2076397309211870, 52.21780102759854003, 8.173336009946826408 ) ) ;
#47928 = CARTESIAN_POINT ( 'NONE',  ( -14.97009123890826032, 8.472783959029182910, 89.00005877110403674 ) ) ;
#47929 = VERTEX_POINT ( 'NONE', #39543 ) ;
#47930 = CARTESIAN_POINT ( 'NONE',  ( -56.72814287166057312, 15.13700122306437557, 71.97630986414527854 ) ) ;
#47931 = ADVANCED_FACE ( 'NONE', ( #55365 ), #66637, .F. ) ;
#47932 = ORIENTED_EDGE ( 'NONE', *, *, #26828, .T. ) ;
#47933 = VECTOR ( 'NONE', #28016, 1000.000000000000000 ) ;
#47934 = ORIENTED_EDGE ( 'NONE', *, *, #2303, .F. ) ;
#47935 = CARTESIAN_POINT ( 'NONE',  ( 46.77033063468804386, 10.50186244217540654, 92.54074439162803856 ) ) ;
#47936 = LINE ( 'NONE', #59182, #54579 ) ;
#47937 = EDGE_CURVE ( 'NONE', #16719, #18334, #4038, .T. ) ;
#47938 = CARTESIAN_POINT ( 'NONE',  ( 139.6272612117789720, 46.21653985347571592, -92.40408479050303470 ) ) ;
#47939 = ORIENTED_EDGE ( 'NONE', *, *, #56875, .F. ) ;
#47940 = AXIS2_PLACEMENT_3D ( 'NONE', #33328, #21707, #1650 ) ;
#47941 = CARTESIAN_POINT ( 'NONE',  ( -58.10608953386397957, 15.52134062643865242, -76.41550596808153273 ) ) ;
#47942 = CARTESIAN_POINT ( 'NONE',  ( -90.99999999999998579, 0.000000000000000000, -2.818925648462311528E-14 ) ) ;
#47943 = EDGE_CURVE ( 'NONE', #40688, #11023, #67210, .T. ) ;
#47944 = CARTESIAN_POINT ( 'NONE',  ( -7.825402957745081878, 7.899365992529268965, 3.271030448983517580 ) ) ;
#47945 = DIRECTION ( 'NONE',  ( 0.000000000000000000, 0.000000000000000000, 1.000000000000000000 ) ) ;
#47946 = VECTOR ( 'NONE', #15004, 1000.000000000000000 ) ;
#47947 = CARTESIAN_POINT ( 'NONE',  ( 164.4953970817402933, 63.32598771815145255, 87.94741031797519781 ) ) ;
#47948 = CARTESIAN_POINT ( 'NONE',  ( 87.10668362745096260, 19.58396519288863757, 29.71208757247931231 ) ) ;
#47949 = VECTOR ( 'NONE', #18244, 1000.000000000000000 ) ;
#47950 = EDGE_LOOP ( 'NONE', ( #62150, #68428, #23888, #63467 ) ) ;
#47951 = CARTESIAN_POINT ( 'NONE',  ( 32.68347998332510684, -12.52158680757303344, 30.00000000000000000 ) ) ;
#47952 = AXIS2_PLACEMENT_3D ( 'NONE', #22018, #205, #49429 ) ;
#47953 = CARTESIAN_POINT ( 'NONE',  ( -66.97713359923356791, 33.64188291208976977, 41.38025477438755928 ) ) ;
#47955 = EDGE_CURVE ( 'NONE', #22681, #59605, #60410, .T. ) ;
#47954 = CARTESIAN_POINT ( 'NONE',  ( -28.13527276074848871, 10.08983026464525068, 30.97886788483921805 ) ) ;
#47956 = CARTESIAN_POINT ( 'NONE',  ( 197.1975259970232059, 98.19639476549653523, 37.03425924184826101 ) ) ;
#47957 = DIRECTION ( 'NONE',  ( 1.000000000000000000, 0.000000000000000000, 0.000000000000000000 ) ) ;
#47959 = ORIENTED_EDGE ( 'NONE', *, *, #25887, .F. ) ;
#47958 = DIRECTION ( 'NONE',  ( -0.7071067811865475727, 0.000000000000000000, -0.7071067811865475727 ) ) ;
#47960 = ORIENTED_EDGE ( 'NONE', *, *, #12819, .F. ) ;
#47961 = VERTEX_POINT ( 'NONE', #7186 ) ;
#47962 = B_SPLINE_CURVE_WITH_KNOTS ( 'NONE', 3,
 ( #57605, #19265, #30874, #68168, #40718, #35101 ),
 .UNSPECIFIED., .F., .F.,
 ( 4, 2, 4 ),
 ( 1.095770181093909371E-06, 0.03239442681617710207, 0.06478775786217311206 ),
 .UNSPECIFIED. ) ;
#47963 = CARTESIAN_POINT ( 'NONE',  ( -452.6627218934859798, 400.0000000000064801, -111.4497041420121661 ) ) ;
#47964 = CYLINDRICAL_SURFACE ( 'NONE', #15442, 20.00000000000000000 ) ;
#47965 = CYLINDRICAL_SURFACE ( 'NONE', #61319, 7.500000000000020428 ) ;
#47966 = CARTESIAN_POINT ( 'NONE',  ( -15.55634918610405748, -10.55634918610400597, 0.000000000000000000 ) ) ;
#47967 = CARTESIAN_POINT ( 'NONE',  ( -11.57950265606958062, 8.174070387114799274, -9.576061325039194827 ) ) ;
#47968 = CARTESIAN_POINT ( 'NONE',  ( 157.0336341255056993, 57.31169401067820957, -77.96873488960137877 ) ) ;
#47969 = DIRECTION ( 'NONE',  ( 0.000000000000000000, 0.000000000000000000, 1.000000000000000000 ) ) ;
#47970 = CARTESIAN_POINT ( 'NONE',  ( -155.1355020251929773, 69.10372769512069624, -47.29556375445353211 ) ) ;
#47971 = VERTEX_POINT ( 'NONE', #28644 ) ;
#47972 = ORIENTED_EDGE ( 'NONE', *, *, #56469, .T. ) ;
#47973 = CARTESIAN_POINT ( 'NONE',  ( 0.000000000000000000, 0.000000000000000000, 41.38025477438755928 ) ) ;
#47974 = CARTESIAN_POINT ( 'NONE',  ( -79.14638003838382474, 23.58242782405879012, -35.11545063171788428 ) ) ;
#47975 = CARTESIAN_POINT ( 'NONE',  ( 103.1602294306414933, 25.74091644446069083, 88.30902535134187303 ) ) ;
#47976 = CARTESIAN_POINT ( 'NONE',  ( 113.4402889550712530, 31.50582881646777622, -9.776826010279577872 ) ) ;
#47978 = CARTESIAN_POINT ( 'NONE',  ( -18.15845058245960075, 17.18344181019522310, 0.000000000000000000 ) ) ;
#47977 = AXIS2_PLACEMENT_3D ( 'NONE', #39135, #12741, #55638 ) ;
#47979 = CARTESIAN_POINT ( 'NONE',  ( 20.36314374176837916, 6.689939636827347158, 31.55112446504767476 ) ) ;
#47980 = CARTESIAN_POINT ( 'NONE',  ( -156.3413281584584809, 71.56573911209629557, 94.99999999999866418 ) ) ;
#47981 = EDGE_LOOP ( 'NONE', ( #20230, #26866 ) ) ;
#47982 = ORIENTED_EDGE ( 'NONE', *, *, #50509, .F. ) ;
#47983 = ORIENTED_EDGE ( 'NONE', *, *, #67817, .F. ) ;
#47984 = AXIS2_PLACEMENT_3D ( 'NONE', #59664, #55440, #39623 ) ;
#47985 = CARTESIAN_POINT ( 'NONE',  ( -156.8773151811562627, 72.06122063279302381, -14.04873829481672054 ) ) ;
#47986 = CARTESIAN_POINT ( 'NONE',  ( 32.15284246740100116, 8.588257691344876932, -41.18047241676685388 ) ) ;
#47987 = AXIS2_PLACEMENT_3D ( 'NONE', #27415, #48853, #1748 ) ;
#47988 = CARTESIAN_POINT ( 'NONE',  ( -35.38560449531986052, 10.27249159032101922, 58.17866205316500583 ) ) ;
#47989 = CYLINDRICAL_SURFACE ( 'NONE', #42985, 7.500000000000013323 ) ;
#47990 = ORIENTED_EDGE ( 'NONE', *, *, #31843, .T. ) ;
#47991 = VECTOR ( 'NONE', #40277, 1000.000000000000227 ) ;
#47992 = CARTESIAN_POINT ( 'NONE',  ( 186.7642514597452816, 86.02880938169741398, 68.55708177098027534 ) ) ;
#47993 = CARTESIAN_POINT ( 'NONE',  ( -156.8764584803562343, 70.69066846313526753, 63.64140852508641188 ) ) ;
#47994 = EDGE_CURVE ( 'NONE', #17392, #18081, #23385, .T. ) ;
#47995 = VECTOR ( 'NONE', #54878, 1000.000000000000000 ) ;
#47996 = CARTESIAN_POINT ( 'NONE',  ( 17.73567516211396367, 7.577454475141601975, 3.410843060652023251 ) ) ;
#47997 = CARTESIAN_POINT ( 'NONE',  ( 185.1802655733641529, 82.84606286178497214, 69.95176336533883443 ) ) ;
#47998 = CARTESIAN_POINT ( 'NONE',  ( 6.400000000000000355, 9.237604307034018802, 1.301042606982603546E-15 ) ) ;
#47999 = CARTESIAN_POINT ( 'NONE',  ( -81.90266786693715062, 23.58030232261292980, -35.83251721507301824 ) ) ;
#48000 = CARTESIAN_POINT ( 'NONE',  ( 18.89064107370900913, 6.619789970027367687, 71.19189653376322724 ) ) ;
#48001 = CARTESIAN_POINT ( 'NONE',  ( 41.66904755831210849, 4.999999999999909406, 0.000000000000000000 ) ) ;
#48002 = CARTESIAN_POINT ( 'NONE',  ( 203.1511228994173450, 104.2426341584999534, 56.16747440225678645 ) ) ;
#48003 = ADVANCED_FACE ( 'NONE', ( #19824 ), #47228, .T. ) ;
#48004 = AXIS2_PLACEMENT_3D ( 'NONE', #25421, #35962, #9231 ) ;
#48005 = EDGE_LOOP ( 'NONE', ( #41645, #38010 ) ) ;
#48006 = DIRECTION ( 'NONE',  ( -1.000000000000000000, 0.000000000000000000, 0.000000000000000000 ) ) ;
#48007 = APPLICATION_PROTOCOL_DEFINITION ( 'draft international standard', 'automotive_design', 1998, #47573 ) ;
#48008 = CARTESIAN_POINT ( 'NONE',  ( 176.0745160362857860, 73.68684431790052258, 42.39531241251699356 ) ) ;
#48009 = CARTESIAN_POINT ( 'NONE',  ( -131.3154845336012784, 50.16828105866952825, -47.61854828779179627 ) ) ;
#48010 = CARTESIAN_POINT ( 'NONE',  ( -109.3386876948163433, 37.66246927061207117, -45.09996864586627652 ) ) ;
#48011 = CARTESIAN_POINT ( 'NONE',  ( 55.57634120535664124, 12.09544293553732786, -69.08107002945564545 ) ) ;
#48012 = VERTEX_POINT ( 'NONE', #68360 ) ;
#48013 = EDGE_LOOP ( 'NONE', ( #47082, #50560, #14517, #23370 ) ) ;
#48014 = EDGE_CURVE ( 'NONE', #31561, #12851, #25633, .T. ) ;
#48015 = CARTESIAN_POINT ( 'NONE',  ( -25.80058235236790054, 8.733375263008319678, -11.00299486492387757 ) ) ;
#48016 = CARTESIAN_POINT ( 'NONE',  ( 174.2486163051500512, 71.96303772754802708, 87.40529692077977586 ) ) ;
#48017 = EDGE_CURVE ( 'NONE', #18311, #67396, #45141, .T. ) ;
#48018 = EDGE_LOOP ( 'NONE', ( #24815, #57741, #21665, #49941 ) ) ;
#48019 = CARTESIAN_POINT ( 'NONE',  ( 117.7411475730015553, 32.50808475802732289, 63.41313343984494821 ) ) ;
#48020 = EDGE_LOOP ( 'NONE', ( #56530, #30770, #39152, #66687 ) ) ;
#48021 = DIRECTION ( 'NONE',  ( 1.000000000000000000, 0.000000000000000000, 0.000000000000000000 ) ) ;
#48022 = LINE ( 'NONE', #42750, #59792 ) ;
#48023 = LINE ( 'NONE', #30838, #6136 ) ;
#48024 = EDGE_CURVE ( 'NONE', #16, #26782, #6528, .T. ) ;
#48025 = ADVANCED_FACE ( 'NONE', ( #30725 ), #25459, .F. ) ;
#48026 = CARTESIAN_POINT ( 'NONE',  ( -97.47339919287391297, 30.40512551257287299, 43.79714771676525942 ) ) ;
#48027 = CARTESIAN_POINT ( 'NONE',  ( 93.09528872995971938, 21.72934119836186184, -39.48931322913085751 ) ) ;
#48028 = DIRECTION ( 'NONE',  ( -0.000000000000000000, -0.000000000000000000, -1.000000000000000000 ) ) ;
#48029 = ORIENTED_EDGE ( 'NONE', *, *, #43442, .F. ) ;
#48030 = ORIENTED_EDGE ( 'NONE', *, *, #35256, .F. ) ;
#48031 = VECTOR ( 'NONE', #43060, 1000.000000000000000 ) ;
#48032 = CARTESIAN_POINT ( 'NONE',  ( -118.4063383664800000, 41.75753822095644097, -15.05876597828681440 ) ) ;
#48033 = FACE_BOUND ( 'NONE', #44568, .T. ) ;
#48034 = ADVANCED_FACE ( 'NONE', ( #63072 ), #68019, .T. ) ;
#48035 = CARTESIAN_POINT ( 'NONE',  ( -180.6209440844958465, 95.88392769199010957, -15.04742671162544632 ) ) ;
#48036 = VECTOR ( 'NONE', #23121, 1000.000000000000000 ) ;
#48037 = DIRECTION ( 'NONE',  ( 0.000000000000000000, -0.09748146057682104126, -0.9952373409613456401 ) ) ;
#48039 = ORIENTED_EDGE ( 'NONE', *, *, #48557, .F. ) ;
#48038 = CARTESIAN_POINT ( 'NONE',  ( -147.7860806339125190, 62.73248524776227697, -49.62554806688481079 ) ) ;
#48040 = LINE ( 'NONE', #63891, #46549 ) ;
#48041 = EDGE_CURVE ( 'NONE', #31287, #28747, #14876, .T. ) ;
#48042 = ADVANCED_FACE ( 'NONE', ( #58142 ), #20498, .F. ) ;
#48043 = AXIS2_PLACEMENT_3D ( 'NONE', #40528, #29627, #12420 ) ;
#48044 = VERTEX_POINT ( 'NONE', #9960 ) ;
#48045 = FACE_OUTER_BOUND ( 'NONE', #39757, .T. ) ;
#48046 = CARTESIAN_POINT ( 'NONE',  ( -61.39252081892698953, 16.47343302442958901, -19.88650151685294531 ) ) ;
#48047 = CARTESIAN_POINT ( 'NONE',  ( 79.38020582286195292, 17.07365509555548400, -18.46566652421186561 ) ) ;
#48048 = VECTOR ( 'NONE', #44166, 1000.000000000000000 ) ;
#48049 = CARTESIAN_POINT ( 'NONE',  ( -133.0921934900200085, 52.65587531157186874, -67.13582062954424146 ) ) ;
#48050 = PLANE ( 'NONE',  #37028 ) ;
#48051 = CARTESIAN_POINT ( 'NONE',  ( -97.88309373898358956, 30.60238467438963283, 5.079866515219528367 ) ) ;
#48052 = CARTESIAN_POINT ( 'NONE',  ( -96.45845418068303445, 29.92035703021965176, -74.11387427670096884 ) ) ;
#48053 = VERTEX_POINT ( 'NONE', #25110 ) ;
#48054 = B_SPLINE_CURVE_WITH_KNOTS ( 'NONE', 3,
 ( #11894, #32323, #11532, #32663, #53751, #26356, #54089, #31974, #64674, #22105, #65022, #27724, #5237, #69253, #53403, #52388, #16817, #16132, #21408, #42852, #64321, #37587, #38278, #59034, #33010, #10856, #5576, #59723, #50578, #34421, #44951, #60438, #2745, #28420, #66782, #2058, #34061, #18571 ),
 .UNSPECIFIED., .F., .F.,
 ( 4, 2, 2, 2, 2, 2, 2, 2, 2, 2, 2, 2, 2, 2, 2, 2, 2, 2, 4 ),
 ( 0.02546424207107600771, 0.02703543426729205709, 0.02782103036540011995, 0.02860662646350817934, 0.03017781865972437444, 0.03174901085594056954, 0.03332020305215676464, 0.03489139524837295975, 0.03646258744458915485, 0.03724818354269723159, 0.03803377964080531526, 0.03881937573891339199, 0.03960497183702146873, 0.04117616403323766383, 0.04274735622945385893, 0.04431854842567005404, 0.04588974062188624914, 0.04746093281810244424, 0.05060331721053485526 ),
 .UNSPECIFIED. ) ;
#48055 = EDGE_LOOP ( 'NONE', ( #22106, #66156, #68047, #54684 ) ) ;
#48056 = DIRECTION ( 'NONE',  ( -0.000000000000000000, 1.000000000000000000, -0.000000000000000000 ) ) ;
#48057 = CARTESIAN_POINT ( 'NONE',  ( 9.823983574062872037, 6.382904402091122087, 32.94129060586310231 ) ) ;
#48058 = CARTESIAN_POINT ( 'NONE',  ( -783.0172411895269988, -622.0000000000060254, 10.00000000000000000 ) ) ;
#48059 = LINE ( 'NONE', #37864, #38526 ) ;
#48060 = PLANE ( 'NONE',  #47892 ) ;
#48061 = CARTESIAN_POINT ( 'NONE',  ( -71.97171223898807568, 20.94894057408425780, 41.33603137547984829 ) ) ;
#48062 = CARTESIAN_POINT ( 'NONE',  ( 84.27368848767925158, 18.63026910897603727, 30.07530638778384358 ) ) ;
#48063 = LINE ( 'NONE', #37515, #58373 ) ;
#48064 = CARTESIAN_POINT ( 'NONE',  ( 39.88975917505626967, 9.487965272711662124, -50.61981746542780058 ) ) ;
#48065 = CARTESIAN_POINT ( 'NONE',  ( 50.98853755884145755, 388.0000000000065370, -123.9497041420120382 ) ) ;
#48066 = ORIENTED_EDGE ( 'NONE', *, *, #13125, .T. ) ;
#48067 = PLANE ( 'NONE',  #14194 ) ;
#48068 = ORIENTED_EDGE ( 'NONE', *, *, #29527, .T. ) ;
#48069 = CARTESIAN_POINT ( 'NONE',  ( -8.807541152391515027, 6.956521193351525412, -35.46664261147883934 ) ) ;
#48070 = LINE ( 'NONE', #54740, #15023 ) ;
#48071 = CARTESIAN_POINT ( 'NONE',  ( -85.85116202048752143, 25.18960254254224296, -94.10664488620292900 ) ) ;
#48072 = LINE ( 'NONE', #10109, #41043 ) ;
#48073 = LINE ( 'NONE', #27664, #62479 ) ;
#48074 = CARTESIAN_POINT ( 'NONE',  ( 32.46582168790593670, 7.608418697099893713, -67.07998740085851352 ) ) ;
#48075 = CARTESIAN_POINT ( 'NONE',  ( -100.4440683050664518, 32.98184228837416043, -62.07263191239334077 ) ) ;
#48076 = CARTESIAN_POINT ( 'NONE',  ( 112.9086998128567672, 31.25010873462638727, -90.09042788728231699 ) ) ;
#48077 = EDGE_LOOP ( 'NONE', ( #63994, #9424 ) ) ;
#48078 = CARTESIAN_POINT ( 'NONE',  ( 39.51413990058172487, 70.00000000000000000, 2.347205688660291667 ) ) ;
#48080 = VERTEX_POINT ( 'NONE', #57796 ) ;
#48079 = EDGE_CURVE ( 'NONE', #26166, #7837, #62737, .T. ) ;
#48081 = CARTESIAN_POINT ( 'NONE',  ( 57.57684776206768618, 12.50442334002049272, 58.98747899309388742 ) ) ;
#48082 = DIRECTION ( 'NONE',  ( -0.000000000000000000, -0.000000000000000000, -1.000000000000000000 ) ) ;
#48083 = CARTESIAN_POINT ( 'NONE',  ( -31.11269837220804035, 20.55634918610408945, 2.000000000000001776 ) ) ;
#48084 = DIRECTION ( 'NONE',  ( -0.000000000000000000, 1.000000000000000000, -0.000000000000000000 ) ) ;
#48085 = CARTESIAN_POINT ( 'NONE',  ( -4.070918861171928249, 6.675509947362632701, 44.11282707256027180 ) ) ;
#48086 = CARTESIAN_POINT ( 'NONE',  ( -95.86612279493104438, 29.64021615886204941, -11.77456874465409520 ) ) ;
#48087 = CARTESIAN_POINT ( 'NONE',  ( 93.32575898730515007, 22.89018551198909535, 87.50692670039568100 ) ) ;
#48088 = ADVANCED_FACE ( 'NONE', ( #19467 ), #52172, .F. ) ;
#48089 =( REPRESENTATION_RELATIONSHIP ('NONE','NONE', #46031, #36174 ) REPRESENTATION_RELATIONSHIP_WITH_TRANSFORMATION ( #3396 )SHAPE_REPRESENTATION_RELATIONSHIP( ) );
#48090 = EDGE_LOOP ( 'NONE', ( #40471, #61306, #47046, #30772 ) ) ;
#48091 = DIRECTION ( 'NONE',  ( 0.000000000000000000, -1.000000000000000000, 0.000000000000000000 ) ) ;
#48092 = CARTESIAN_POINT ( 'NONE',  ( 133.8566784816069344, -170.0000000000000000, -97.21241211332302612 ) ) ;
#48093 = CARTESIAN_POINT ( 'NONE',  ( 447.3372781065083359, 400.0000000000044338, 83.55029585798381220 ) ) ;
#48094 = CARTESIAN_POINT ( 'NONE',  ( -108.0902552660050588, 36.97681740369923631, 60.09494272580671748 ) ) ;
#48095 = CONTEXT_DEPENDENT_SHAPE_REPRESENTATION ( #7654, #18732 ) ;
#48096 = CARTESIAN_POINT ( 'NONE',  ( -133.0921934900200085, 52.65587531157188295, -40.29127003908051563 ) ) ;
#48097 = VERTEX_POINT ( 'NONE', #46541 ) ;
#48098 = DIRECTION ( 'NONE',  ( 9.729521452151193035E-15, -5.551115123116034723E-17, 1.000000000000000000 ) ) ;
#48099 = CARTESIAN_POINT ( 'NONE',  ( 93.70675391435744928, 21.95852801827564349, 61.56192124033761104 ) ) ;
#48100 = EDGE_CURVE ( 'NONE', #63790, #36305, #15583, .T. ) ;
#48101 = CARTESIAN_POINT ( 'NONE',  ( -148.2650023942115922, 63.13271795942794284, 84.50851806093228902 ) ) ;
#48102 = EDGE_CURVE ( 'NONE', #34356, #5113, #51009, .T. ) ;
#48103 = CARTESIAN_POINT ( 'NONE',  ( 1.224646799147353256E-15, 70.00000000000000000, 10.00000000000000000 ) ) ;
#48104 = EDGE_CURVE ( 'NONE', #62594, #38367, #64447, .T. ) ;
#48105 = ORIENTED_EDGE ( 'NONE', *, *, #37538, .T. ) ;
#48106 = FACE_OUTER_BOUND ( 'NONE', #42607, .T. ) ;
#48107 = CARTESIAN_POINT ( 'NONE',  ( 80.73462811483979351, 18.54763808182593721, 5.703558285329590305 ) ) ;
#48108 = CARTESIAN_POINT ( 'NONE',  ( 157.4703587214989113, 58.92748579479258808, 2.564916881789689462 ) ) ;
#48109 = CARTESIAN_POINT ( 'NONE',  ( 188.9999999999999432, -2.000000000000000000, 0.000000000000000000 ) ) ;
#48110 = VERTEX_POINT ( 'NONE', #28200 ) ;
#48111 = CARTESIAN_POINT ( 'NONE',  ( 15.55634918610409656, 36.11269837220803680, 2.000000000000001776 ) ) ;
#48112 = EDGE_LOOP ( 'NONE', ( #15091, #10117, #46315, #69240 ) ) ;
#48113 = CARTESIAN_POINT ( 'NONE',  ( -108.1144194775597214, 35.84457139767598477, -47.25378443719495891 ) ) ;
#48114 = CARTESIAN_POINT ( 'NONE',  ( 65.40032188136230218, 13.23841673691966925, -77.18017510422534144 ) ) ;
#48115 = CARTESIAN_POINT ( 'NONE',  ( 149.4165763529819344, -26.99999999999998224, 129.0000000000000000 ) ) ;
#48117 = EDGE_LOOP ( 'NONE', ( #24969, #42994 ) ) ;
#48116 = CARTESIAN_POINT ( 'NONE',  ( 157.4703587214989398, 58.92748579479258808, 17.56491688178971700 ) ) ;
#48118 = FACE_BOUND ( 'NONE', #31656, .T. ) ;
#48119 = CARTESIAN_POINT ( 'NONE',  ( 0.000000000000000000, 0.000000000000000000, 0.000000000000000000 ) ) ;
#48120 = ADVANCED_FACE ( 'NONE', ( #56329 ), #16610, .T. ) ;
#48121 = EDGE_CURVE ( 'NONE', #1594, #62220, #12032, .T. ) ;
#48122 = CARTESIAN_POINT ( 'NONE',  ( 116.6436511186860798, 33.08230081168870385, -39.50517661178831474 ) ) ;
#48123 = ORIENTED_EDGE ( 'NONE', *, *, #56304, .F. ) ;
#48124 = ADVANCED_FACE ( 'NONE', ( #55630 ), #18703, .F. ) ;
#48125 = LINE ( 'NONE', #62944, #29954 ) ;
#48126 = DIRECTION ( 'NONE',  ( -1.000000000000000000, 0.000000000000000000, -0.000000000000000000 ) ) ;
#48127 = CARTESIAN_POINT ( 'NONE',  ( -167.6386155194958292, 81.22597462185134987, 43.46491529870461790 ) ) ;
#48128 = CARTESIAN_POINT ( 'NONE',  ( -34.51918258780364823, 10.11719938103012240, -76.50446516501558847 ) ) ;
#48129 = EDGE_LOOP ( 'NONE', ( #34568, #14567, #50181, #29344 ) ) ;
#48130 = AXIS2_PLACEMENT_3D ( 'NONE', #32979, #12574, #18198 ) ;
#48131 = CARTESIAN_POINT ( 'NONE',  ( 46.51377856795991761, 10.46037936279323688, 13.00077528625720369 ) ) ;
#48132 = VERTEX_POINT ( 'NONE', #40158 ) ;
#48133 = ORIENTED_EDGE ( 'NONE', *, *, #58327, .F. ) ;
#48134 = DIRECTION ( 'NONE',  ( 1.000000000000000000, 0.000000000000000000, 0.000000000000000000 ) ) ;
#48135 = VECTOR ( 'NONE', #17169, 1000.000000000000000 ) ;
#48136 = CARTESIAN_POINT ( 'NONE',  ( -106.6711220790662651, 36.20923238211247508, 5.089478997775757740 ) ) ;
#48137 = DIRECTION ( 'NONE',  ( 1.000000000000000000, 0.000000000000000000, -0.000000000000000000 ) ) ;
#48138 = CARTESIAN_POINT ( 'NONE',  ( -155.1355020251929773, 69.10372769512071045, -74.14011434491720820 ) ) ;
#48139 = CARTESIAN_POINT ( 'NONE',  ( 67.35224030275335849, 13.72040503854036331, 84.87408482119735709 ) ) ;
#48140 = CYLINDRICAL_SURFACE ( 'NONE', #41521, 7.500000000000020428 ) ;
#48141 = CARTESIAN_POINT ( 'NONE',  ( -131.7724154034330581, 50.48821165954354484, 69.62870055094876420 ) ) ;
#48142 = CARTESIAN_POINT ( 'NONE',  ( 63.01563776193091826, 12.67277567978498176, 29.81296093922127710 ) ) ;
#48143 = ORIENTED_EDGE ( 'NONE', *, *, #18028, .T. ) ;
#48144 = LINE ( 'NONE', #27042, #41996 ) ;
#48145 = VERTEX_POINT ( 'NONE', #60909 ) ;
#48146 = CARTESIAN_POINT ( 'NONE',  ( -75.43495400358860081, 22.18831810339352728, 57.99029328673930195 ) ) ;
#48147 = CARTESIAN_POINT ( 'NONE',  ( 185.5415406465189676, 83.23025870924408309, 30.75849858761065292 ) ) ;
#48148 = CARTESIAN_POINT ( 'NONE',  ( 59.29597493004737885, 11.84030339376943886, -63.53442171863188292 ) ) ;
#48149 = CARTESIAN_POINT ( 'NONE',  ( -72.20490592113146988, 19.96451062593607872, 14.91352488762884931 ) ) ;
#48150 = CARTESIAN_POINT ( 'NONE',  ( -119.2949674747224975, 43.48097822533565449, 68.56738607616526338 ) ) ;
#48151 = DIRECTION ( 'NONE',  ( 0.000000000000000000, 0.000000000000000000, 1.000000000000000000 ) ) ;
#48152 = CARTESIAN_POINT ( 'NONE',  ( 197.4024603413583350, 96.84614858128594506, 88.60102860378297862 ) ) ;
#48153 = CARTESIAN_POINT ( 'NONE',  ( 15.78827728214693416, -170.0000000000000000, -35.51894409868578606 ) ) ;
#48154 = ORIENTED_EDGE ( 'NONE', *, *, #38422, .T. ) ;
#48155 = DIRECTION ( 'NONE',  ( 1.000000000000000000, 0.000000000000000000, 0.000000000000000000 ) ) ;
#48156 = PLANE ( 'NONE',  #48703 ) ;
#48157 = VERTEX_POINT ( 'NONE', #28560 ) ;
#48158 = ORIENTED_EDGE ( 'NONE', *, *, #41069, .T. ) ;
#48159 = CARTESIAN_POINT ( 'NONE',  ( -23.93895920923072396, 9.495000752338453864, -69.90383058804481209 ) ) ;
#48160 = CARTESIAN_POINT ( 'NONE',  ( 217.9999999999999716, 128.6235316737731296, 94.99999999999866418 ) ) ;
#48161 = DIRECTION ( 'NONE',  ( 0.000000000000000000, -1.000000000000000000, 0.000000000000000000 ) ) ;
#48162 = ADVANCED_FACE ( 'NONE', ( #50369 ), #50005, .T. ) ;
#48163 = PLANE ( 'NONE',  #24086 ) ;
#48164 = ORIENTED_EDGE ( 'NONE', *, *, #38350, .T. ) ;
#48165 = ORIENTED_EDGE ( 'NONE', *, *, #3842, .F. ) ;
#48166 = DIRECTION ( 'NONE',  ( -0.000000000000000000, 1.000000000000000000, -0.000000000000000000 ) ) ;
#48167 = ORIENTED_EDGE ( 'NONE', *, *, #60038, .F. ) ;
#48168 = LINE ( 'NONE', #53450, #54816 ) ;
#48169 = CARTESIAN_POINT ( 'NONE',  ( 447.3372781065085064, 365.0000000000043769, 113.5502958579838122 ) ) ;
#48170 = CARTESIAN_POINT ( 'NONE',  ( 204.6977192012829789, 106.3443248447423457, 44.20772073876944575 ) ) ;
#48171 = CARTESIAN_POINT ( 'NONE',  ( -66.25334388784037287, 7.217961348991855708, 34.48241795236665297 ) ) ;
#48172 = EDGE_CURVE ( 'NONE', #39145, #47003, #35136, .T. ) ;
#48173 = PLANE ( 'NONE',  #11407 ) ;
#48174 = EDGE_CURVE ( 'NONE', #1784, #45368, #63820, .T. ) ;
#48175 = DIRECTION ( 'NONE',  ( -0.3090169943749447312, -0.9510565162951544194, 0.000000000000000000 ) ) ;
#48176 = ORIENTED_EDGE ( 'NONE', *, *, #7720, .T. ) ;
#48177 = VECTOR ( 'NONE', #36022, 1000.000000000000000 ) ;
#48178 = EDGE_CURVE ( 'NONE', #22146, #56862, #54340, .T. ) ;
#48179 = ORIENTED_EDGE ( 'NONE', *, *, #34822, .F. ) ;
#48180 = CARTESIAN_POINT ( 'NONE',  ( 0.000000000000000000, 0.000000000000000000, -9.500000000000000000 ) ) ;
#48181 = CARTESIAN_POINT ( 'NONE',  ( 442.3372781065086201, 0.000000000000000000, 103.5502958579881749 ) ) ;
#48182 = CARTESIAN_POINT ( 'NONE',  ( 35.44311777160620380, 8.940232499250161169, -63.58956774339669238 ) ) ;
#48183 = CARTESIAN_POINT ( 'NONE',  ( -6.000000000000000000, 23.07878402833891229, 9.999999999999998224 ) ) ;
#48184 = LINE ( 'NONE', #42910, #5982 ) ;
#48185 = CARTESIAN_POINT ( 'NONE',  ( -190.4968431727839402, 108.8425311198515004, -73.13328961415110996 ) ) ;
#48186 = VECTOR ( 'NONE', #975, 1000.000000000000000 ) ;
#48187 = ORIENTED_EDGE ( 'NONE', *, *, #24944, .F. ) ;
#48188 = CARTESIAN_POINT ( 'NONE',  ( -96.45845418068304866, 29.92035703021964466, 60.10887867561745423 ) ) ;
#48189 = ORIENTED_EDGE ( 'NONE', *, *, #42321, .T. ) ;
#48190 = B_SPLINE_CURVE_WITH_KNOTS ( 'NONE', 3,
 ( #60505, #61205, #38708, #18640, #11972, #12670, #66159, #40101, #33442, #55932, #7749, #45017, #65440, #54868, #43964, #2125, #23239, #60151 ),
 .UNSPECIFIED., .F., .F.,
 ( 4, 2, 2, 2, 2, 2, 2, 2, 4 ),
 ( 0.01054411675784286233, 0.01184819941084477336, 0.01315228206384668266, 0.01445636471684859370, 0.01576044736985050473, 0.01706453002285241577, 0.01836861267585432334, 0.01967269532885623437, 0.02097677798185814541 ),
 .UNSPECIFIED. ) ;
#48191 = CARTESIAN_POINT ( 'NONE',  ( -73.63346300764935393, 20.46798018699518096, 32.35235876508207298 ) ) ;
#48192 = ORIENTED_EDGE ( 'NONE', *, *, #4674, .F. ) ;
#48193 = VERTEX_POINT ( 'NONE', #59767 ) ;
#48194 = CARTESIAN_POINT ( 'NONE',  ( -118.6302575928420424, 43.07263081214308897, 13.16250469874441009 ) ) ;
#48195 = VECTOR ( 'NONE', #21159, 1000.000000000000000 ) ;
#48196 = LINE ( 'NONE', #41565, #39397 ) ;
#48197 = CARTESIAN_POINT ( 'NONE',  ( 129.1137093889807943, 38.63348691920619871, 58.04000564037256282 ) ) ;
#48198 = VERTEX_POINT ( 'NONE', #59079 ) ;
#48199 = EDGE_CURVE ( 'NONE', #51166, #61254, #6316, .T. ) ;
#48200 = DIRECTION ( 'NONE',  ( -0.000000000000000000, -0.000000000000000000, -1.000000000000000000 ) ) ;
#48201 = CARTESIAN_POINT ( 'NONE',  ( 155.2910738464913436, 55.97560547655806573, 29.71883570028862920 ) ) ;
#48202 = CARTESIAN_POINT ( 'NONE',  ( 8.000000000000003553, -4.618802153517020948, -8.785468820183664818 ) ) ;
#48203 = CARTESIAN_POINT ( 'NONE',  ( 414.4083459183741525, 394.9999999999999432, 80.62136366985377833 ) ) ;
#48204 = PLANE ( 'NONE',  #34588 ) ;
#48205 = FACE_OUTER_BOUND ( 'NONE', #15140, .T. ) ;
#48206 = CARTESIAN_POINT ( 'NONE',  ( -24.94151142167916646, 8.614613465433006212, 33.93833259409825587 ) ) ;
#48207 = CARTESIAN_POINT ( 'NONE',  ( -142.5087559769084748, 59.74468185400778708, -66.40863924655131711 ) ) ;
#48208 = ORIENTED_EDGE ( 'NONE', *, *, #54705, .T. ) ;
#48209 = CIRCLE ( 'NONE', #54959, 25.12245591505646303 ) ;
#48210 = CARTESIAN_POINT ( 'NONE',  ( 450.2085304802404266, 190.0000000000000000, -250.0000000000000000 ) ) ;
#48211 = FACE_OUTER_BOUND ( 'NONE', #9435, .T. ) ;
#48212 = CARTESIAN_POINT ( 'NONE',  ( -180.3161328724957855, 97.10341277064807741, 67.30497477601284118 ) ) ;
#48213 = LINE ( 'NONE', #6369, #30469 ) ;
#48214 = PLANE ( 'NONE',  #55918 ) ;
#48215 = CARTESIAN_POINT ( 'NONE',  ( -81.23268307104841313, 24.39742801172156206, 4.022339847785443290 ) ) ;
#48216 = PLANE ( 'NONE',  #6746 ) ;
#48217 = CARTESIAN_POINT ( 'NONE',  ( 111.3030933484817382, 21.46146164524274980, 4.838392277045666212 ) ) ;
#48218 = CARTESIAN_POINT ( 'NONE',  ( -71.36003922708370339, 19.67168905366865772, -94.55123213910407287 ) ) ;
#48219 = DIRECTION ( 'NONE',  ( 0.000000000000000000, 0.000000000000000000, 1.000000000000000000 ) ) ;
#48220 = CARTESIAN_POINT ( 'NONE',  ( 160.9069879467681119, 60.37290772564306707, 3.382471444115906500 ) ) ;
#48221 = CARTESIAN_POINT ( 'NONE',  ( 45.90675866695829654, 10.36357315963267922, -93.06977314594286099 ) ) ;
#48222 = ORIENTED_EDGE ( 'NONE', *, *, #16274, .F. ) ;
#48223 = CARTESIAN_POINT ( 'NONE',  ( -38.68632430131779643, 11.91908191268693074, 12.81834785221818684 ) ) ;
#48224 = ORIENTED_EDGE ( 'NONE', *, *, #61362, .F. ) ;
#48225 = CARTESIAN_POINT ( 'NONE',  ( -58.00979178563811445, -29.32343869649178814, 40.00000000000003553 ) ) ;
#48226 = ORIENTED_EDGE ( 'NONE', *, *, #62495, .T. ) ;
#48227 = AXIS2_PLACEMENT_3D ( 'NONE', #35348, #62066, #56807 ) ;
#48228 = CARTESIAN_POINT ( 'NONE',  ( 19.54452863209719027, 7.657034792877146501, -63.35344965661052186 ) ) ;
#48229 = CARTESIAN_POINT ( 'NONE',  ( 117.6076489466057780, 33.56811790321052058, 89.33957235143014941 ) ) ;
#48230 = LINE ( 'NONE', #22562, #49045 ) ;
#48231 = CARTESIAN_POINT ( 'NONE',  ( 67.56108154898467433, 13.77276756375644595, -10.39039143759568518 ) ) ;
#48233 = CARTESIAN_POINT ( 'NONE',  ( 138.5943620234099001, 45.55242290395134575, -49.35784197316183253 ) ) ;
#48232 = AXIS2_PLACEMENT_3D ( 'NONE', #18801, #50806, #51843 ) ;
#48234 = CARTESIAN_POINT ( 'NONE',  ( -54.56685407443680447, 15.59259313022788085, -62.06087458892354647 ) ) ;
#48235 = LINE ( 'NONE', #5682, #35326 ) ;
#48236 = CARTESIAN_POINT ( 'NONE',  ( -15.47041015649658391, 73.39774458108210808, 170.0000000000000000 ) ) ;
#48237 = EDGE_LOOP ( 'NONE', ( #8354, #709, #38616, #5695 ) ) ;
#48238 = ORIENTED_EDGE ( 'NONE', *, *, #37626, .F. ) ;
#48239 = ADVANCED_FACE ( 'NONE', ( #27071 ), #10548, .F. ) ;
#48240 = DIRECTION ( 'NONE',  ( 0.000000000000000000, 0.02271222823333339177, -0.9997420440737084801 ) ) ;
#48241 = FILL_AREA_STYLE_COLOUR ( '', #38332 ) ;
#48242 = ADVANCED_FACE ( 'NONE', ( #54491 ), #54136, .T. ) ;
#48243 = CARTESIAN_POINT ( 'NONE',  ( 129.8870388671970204, 40.24164088984107934, -90.83676810778949573 ) ) ;
#48244 = CIRCLE ( 'NONE', #26929, 66.50000000000000000 ) ;
#48245 = CARTESIAN_POINT ( 'NONE',  ( 46.66904755831212981, 15.55634918610394379, 85.00100000000000477 ) ) ;
#48246 = ORIENTED_EDGE ( 'NONE', *, *, #34088, .T. ) ;
#48247 = CARTESIAN_POINT ( 'NONE',  ( 91.11019107624152014, 22.06959540317786761, 16.38678607536089160 ) ) ;
#48248 = CARTESIAN_POINT ( 'NONE',  ( 188.4920037102893957, 87.93425473911918289, -15.67097523847415808 ) ) ;
#48249 = CARTESIAN_POINT ( 'NONE',  ( 206.2957331585308793, 110.2946564621822745, 2.490034632839250417 ) ) ;
#48250 = DIRECTION ( 'NONE',  ( 0.8584487936018655452, 0.5128992774059070170, 0.000000000000000000 ) ) ;
#48251 = CARTESIAN_POINT ( 'NONE',  ( 41.81982603358024875, 8.735900550613189708, -9.159026031209867469 ) ) ;
#48252 = CARTESIAN_POINT ( 'NONE',  ( 208.9507214515059843, 112.3605999017434982, -23.17500676389725456 ) ) ;
#48253 = CARTESIAN_POINT ( 'NONE',  ( 0.000000000000000000, 0.000000000000000000, 0.000000000000000000 ) ) ;
#48254 = CARTESIAN_POINT ( 'NONE',  ( 164.8444104055694766, 64.93678790243659193, 62.35759023313505622 ) ) ;
#48255 = SHAPE_REPRESENTATION ( 'stand', ( #66832 ), #30915 ) ;
#48256 = EDGE_CURVE ( 'NONE', #11896, #55210, #61566, .T. ) ;
#48257 = VERTEX_POINT ( 'NONE', #32023 ) ;
#48258 = EDGE_CURVE ( 'NONE', #11698, #65661, #48168, .T. ) ;
#48259 = CARTESIAN_POINT ( 'NONE',  ( 130.7260570116704059, 40.73146260246712558, 16.99693353642962990 ) ) ;
#48260 = CARTESIAN_POINT ( 'NONE',  ( 89.20981392318256553, 21.38519354635262815, -36.27533723528620158 ) ) ;
#48261 = CARTESIAN_POINT ( 'NONE',  ( 155.7167524447090727, 57.56687707799954268, 71.05957392723330202 ) ) ;
#48262 = CARTESIAN_POINT ( 'NONE',  ( -34.79003333406912901, 38.19633060033950755, 26.66469104408690427 ) ) ;
#48263 = DIRECTION ( 'NONE',  ( -0.8160245890732938934, -0.5780171883497599028, 0.000000000000000000 ) ) ;
#48264 = VECTOR ( 'NONE', #1098, 1000.000000000000114 ) ;
#48265 = CARTESIAN_POINT ( 'NONE',  ( -3.022581224654154131, 7.632926133645733024, 85.53503376044743334 ) ) ;
#48266 = VERTEX_POINT ( 'NONE', #1049 ) ;
#48267 = CARTESIAN_POINT ( 'NONE',  ( 63.01563776193090405, 12.67277567978497643, 17.96841034875761878 ) ) ;
#48268 = CARTESIAN_POINT ( 'NONE',  ( 0.000000000000000000, 6.928203230275506108, 4.000000000000007105 ) ) ;
#48269 = VERTEX_POINT ( 'NONE', #4934 ) ;
#48270 = VERTEX_POINT ( 'NONE', #10897 ) ;
#48271 = CARTESIAN_POINT ( 'NONE',  ( 32.39877097090366931, 8.612975291426320013, 93.80784019633749438 ) ) ;
#48272 = DIRECTION ( 'NONE',  ( 0.000000000000000000, 0.000000000000000000, 1.000000000000000000 ) ) ;
#48273 = CARTESIAN_POINT ( 'NONE',  ( 105.8022841538864185, 26.88074187880708976, 31.04807806109887025 ) ) ;
#48274 = VERTEX_POINT ( 'NONE', #21126 ) ;
#48275 = CARTESIAN_POINT ( 'NONE',  ( -58.76006735892197241, 15.70681061434692261, -76.08508450424285741 ) ) ;
#48276 = CARTESIAN_POINT ( 'NONE',  ( 38.90894112122322213, 8.345444037631242651, -8.775266874964067654 ) ) ;
#48277 = DIRECTION ( 'NONE',  ( 0.000000000000000000, 0.000000000000000000, -1.000000000000000000 ) ) ;
#48278 = CONICAL_SURFACE ( 'NONE', #57309, 2.999999999999981792, 0.7853981633974482790 ) ;
#48279 = CARTESIAN_POINT ( 'NONE',  ( 164.8121648350735882, 63.59223683144968220, 89.02090917915565171 ) ) ;
#48280 = CARTESIAN_POINT ( 'NONE',  ( 93.70675391435746349, 21.95852801827565060, 34.71737064987392074 ) ) ;
#48281 = VERTEX_POINT ( 'NONE', #21793 ) ;
#48282 = CARTESIAN_POINT ( 'NONE',  ( 105.7953515382196059, 27.97683113100022467, -10.51959647692886080 ) ) ;
#48283 = DIRECTION ( 'NONE',  ( -1.000000000000000000, -0.000000000000000000, -0.000000000000000000 ) ) ;
#48284 = CARTESIAN_POINT ( 'NONE',  ( 9.689943677145727463, 7.388265075009367244, 33.14200807007561167 ) ) ;
#48285 = CARTESIAN_POINT ( 'NONE',  ( 65.02380462922316440, 13.14718491827419555, -89.67200624934488928 ) ) ;
#48286 = CARTESIAN_POINT ( 'NONE',  ( -85.50249391410862643, 26.13441511443011578, 94.70962812146305509 ) ) ;
#48288 = ORIENTED_EDGE ( 'NONE', *, *, #37323, .T. ) ;
#48287 = CARTESIAN_POINT ( 'NONE',  ( 11.51073125898252947, 31.38130312474459416, 6.893343212288933763 ) ) ;
#48289 = EDGE_LOOP ( 'NONE', ( #46676, #37920, #23515, #52610 ) ) ;
#48290 = EDGE_LOOP ( 'NONE', ( #47685, #54321, #17592, #10834 ) ) ;
#48291 = CARTESIAN_POINT ( 'NONE',  ( -7.825402957745085430, 6.891034867348157178, -8.573520141480125645 ) ) ;
#48292 = CARTESIAN_POINT ( 'NONE',  ( -166.7617689806962460, 81.76611317639944332, 88.02160040033108146 ) ) ;
#48293 = LINE ( 'NONE', #21580, #25550 ) ;
#48294 = CARTESIAN_POINT ( 'NONE',  ( -190.6985136298601731, 109.1272424661242582, -95.00000000000133582 ) ) ;
#48295 = CARTESIAN_POINT ( 'NONE',  ( -37.93379515072631847, 11.77251734620211288, 60.77801631423660211 ) ) ;
#48296 = FACE_OUTER_BOUND ( 'NONE', #48290, .T. ) ;
#48297 = CARTESIAN_POINT ( 'NONE',  ( 150.7926588734436280, 52.63999027731883729, -67.04403352340344213 ) ) ;
#48298 = CARTESIAN_POINT ( 'NONE',  ( 17.74393407086870056, 6.570779001277778697, -8.916980308073734207 ) ) ;
#48299 = ORIENTED_EDGE ( 'NONE', *, *, #33846, .F. ) ;
#48300 = CARTESIAN_POINT ( 'NONE',  ( -156.9406434201983700, 70.74968524571475825, -41.16293729598802287 ) ) ;
#48301 = ORIENTED_EDGE ( 'NONE', *, *, #47633, .F. ) ;
#48302 = ORIENTED_EDGE ( 'NONE', *, *, #40114, .T. ) ;
#48303 = CARTESIAN_POINT ( 'NONE',  ( 68.63585058221468671, 15.08566240483131438, -21.36693067117767697 ) ) ;
#48304 = CARTESIAN_POINT ( 'NONE',  ( -82.32006615997346444, 24.83050031643765720, -49.18324661891568184 ) ) ;
#48305 = CYLINDRICAL_SURFACE ( 'NONE', #40093, 7.500000000000020428 ) ;
#48306 = AXIS2_PLACEMENT_3D ( 'NONE', #143, #16329, #43398 ) ;
#48307 = CARTESIAN_POINT ( 'NONE',  ( -151.6648563624119106, 67.36546864992756412, 4.179678963093405919 ) ) ;
#48308 = EDGE_CURVE ( 'NONE', #22151, #58159, #32368, .T. ) ;
#48309 = CARTESIAN_POINT ( 'NONE',  ( 183.1910712700537545, 80.76073941711165105, -36.51428264922770950 ) ) ;
#48310 = DIRECTION ( 'NONE',  ( 4.852411958229186445E-18, -1.576644219464734062E-18, -1.000000000000000000 ) ) ;
#48311 = CARTESIAN_POINT ( 'NONE',  ( -155.7884408287038696, 71.05759622589089020, 87.79867964050457374 ) ) ;
#48312 = ORIENTED_EDGE ( 'NONE', *, *, #33270, .T. ) ;
#48313 = EDGE_LOOP ( 'NONE', ( #14645, #41911 ) ) ;
#48314 = ADVANCED_FACE ( 'NONE', ( #6337 ), #37983, .T. ) ;
#48315 = ORIENTED_EDGE ( 'NONE', *, *, #62281, .F. ) ;
#48316 = CARTESIAN_POINT ( 'NONE',  ( -156.0204364459164879, 71.27041535366186054, -11.74006770552829870 ) ) ;
#48317 = EDGE_CURVE ( 'NONE', #57391, #38316, #64027, .T. ) ;
#48318 = CARTESIAN_POINT ( 'NONE',  ( 31.90170717962885405, 8.563261373066637816, -42.87966478670944781 ) ) ;
#48319 = EDGE_CURVE ( 'NONE', #14354, #47669, #26401, .T. ) ;
#48320 = CARTESIAN_POINT ( 'NONE',  ( -34.74312654625184393, 10.15703162223800504, 57.82354398925224359 ) ) ;
#48321 = CARTESIAN_POINT ( 'NONE',  ( 197.4121679705847328, 98.46451029407251099, 61.76465183233728595 ) ) ;
#48322 = ORIENTED_EDGE ( 'NONE', *, *, #37954, .F. ) ;
#48323 = CARTESIAN_POINT ( 'NONE',  ( 184.0001683447904099, 83.06228184427189376, 56.72983684963124773 ) ) ;
#48324 = CARTESIAN_POINT ( 'NONE',  ( -153.7005182577090068, 67.81869626254727734, 71.30039421697708235 ) ) ;
#48325 = CARTESIAN_POINT ( 'NONE',  ( 23.03546163277113124, 7.848986635155161373, 12.61657727460462830 ) ) ;
#48326 = CARTESIAN_POINT ( 'NONE',  ( 107.0471828278921009, 27.43080724084234845, 17.06850905904248350 ) ) ;
#48327 = DIRECTION ( 'NONE',  ( -0.000000000000000000, -0.000000000000000000, -1.000000000000000000 ) ) ;
#48328 = CARTESIAN_POINT ( 'NONE',  ( -86.10361028793435878, 25.29528064050659708, -43.61713178642852284 ) ) ;
#48329 = CARTESIAN_POINT ( 'NONE',  ( 18.66025561752211104, 6.609375019058820300, 57.41805809103978930 ) ) ;
#48330 = FACE_OUTER_BOUND ( 'NONE', #146, .T. ) ;
#48331 = CARTESIAN_POINT ( 'NONE',  ( 8.480442907658519047, 6.376693431076494889, -68.15865659835031920 ) ) ;
#48332 = EDGE_CURVE ( 'NONE', #49487, #56693, #31252, .T. ) ;
#48333 = ORIENTED_EDGE ( 'NONE', *, *, #68219, .T. ) ;
#48334 = CARTESIAN_POINT ( 'NONE',  ( -1.666933348992582609, 64.97862212458815634, 170.0000000000000000 ) ) ;
#48335 = ITEM_DEFINED_TRANSFORMATION ( 'NONE', 'NONE', #7412,  #66832 ) ;
#48336 = CIRCLE ( 'NONE', #35982, 20.00000000000001066 ) ;
#48337 = CARTESIAN_POINT ( 'NONE',  ( 175.3815143714021190, 73.02838262206999786, 41.68673370242148479 ) ) ;
#48338 = CARTESIAN_POINT ( 'NONE',  ( -55.05276343752910151, -170.0000000000000000, 45.31732777293115788 ) ) ;
#48339 = CARTESIAN_POINT ( 'NONE',  ( 46.84183314611288296, 9.494161546644496852, -68.98510195083733265 ) ) ;
#48340 = CARTESIAN_POINT ( 'NONE',  ( 55.51528220483958620, 12.08323518953685216, -69.82681857395122904 ) ) ;
#48341 = ORIENTED_EDGE ( 'NONE', *, *, #53726, .F. ) ;
#48342 = VECTOR ( 'NONE', #37557, 1000.000000000000000 ) ;
#48343 = ORIENTED_EDGE ( 'NONE', *, *, #34114, .T. ) ;
#48344 = CARTESIAN_POINT ( 'NONE',  ( 25.00000000000763478, -65.13282190615278466, -9.999999999999998224 ) ) ;
#48345 = CARTESIAN_POINT ( 'NONE',  ( 173.8016025329976344, 71.54639721357104065, 88.69313603028011528 ) ) ;
#48346 = ORIENTED_EDGE ( 'NONE', *, *, #27286, .T. ) ;
#48347 = AXIS2_PLACEMENT_3D ( 'NONE', #39405, #49948, #12674 ) ;
#48348 = ORIENTED_EDGE ( 'NONE', *, *, #23531, .F. ) ;
#48349 = CARTESIAN_POINT ( 'NONE',  ( 114.6632852039171411, 30.98120524556724931, 57.89195650209787658 ) ) ;
#48350 = VERTEX_POINT ( 'NONE', #16528 ) ;
#48351 = LINE ( 'NONE', #31521, #900 ) ;
#48352 = CARTESIAN_POINT ( 'NONE',  ( -58.00979178563811445, -29.32343869649178814, 40.00000000000003553 ) ) ;
#48353 = CARTESIAN_POINT ( 'NONE',  ( 135.0005116824453637, 43.29964618809727028, 56.43905545767402998 ) ) ;
#48354 = LINE ( 'NONE', #37134, #10557 ) ;
#48355 = AXIS2_PLACEMENT_3D ( 'NONE', #54745, #43836, #64971 ) ;
#48356 = B_SPLINE_CURVE_WITH_KNOTS ( 'NONE', 3,
 ( #8821, #24653, #46783, #51029, #41169, #67908, #46088, #30271, #52065, #62964, #19357, #29565, #68254, #13398, #67557, #8116, #20059, #2843, #3878, #14439, #24310, #3526, #40813, #25349, #34860, #56297, #9502, #41511, #40467, #29920, #46429, #45751, #67231, #14770, #30964, #19016, #51720, #62267, #61911, #35193, #56648, #19707, #36236, #52410 ),
 .UNSPECIFIED., .F., .F.,
 ( 4, 2, 2, 2, 2, 2, 2, 2, 2, 2, 2, 2, 2, 2, 2, 2, 2, 2, 2, 2, 2, 4 ),
 ( 0.000000000000000000, 0.003518733725596301810, 0.004398417156995386261, 0.005278100588394469411, 0.007037467451192689488, 0.007917150882591761363, 0.008796834313990834972, 0.01055620117678902209, 0.01231556803958721094, 0.01319525147098630537, 0.01407493490238540153, 0.01495461833378449422, 0.01583430176518358865, 0.01671398519658268134, 0.01759366862798177750, 0.01935303549077994900, 0.02111240235357811704, 0.02199208578497717850, 0.02287176921637623650, 0.02463113607917438025, 0.02639050294197252747, 0.02814986980477067122 ),
 .UNSPECIFIED. ) ;
#48357 = LINE ( 'NONE', #47679, #60711 ) ;
#48358 = CARTESIAN_POINT ( 'NONE',  ( 5.850262805259840881, 188.0000000000000000, -1.724042536399415404 ) ) ;
#48359 = CARTESIAN_POINT ( 'NONE',  ( -179.9997297618090784, 95.12611598520665268, 94.99999999999866418 ) ) ;
#48360 = EDGE_LOOP ( 'NONE', ( #57361, #49180 ) ) ;
#48361 = ORIENTED_EDGE ( 'NONE', *, *, #59719, .F. ) ;
#48362 = DIRECTION ( 'NONE',  ( 0.000000000000000000, 0.000000000000000000, 1.000000000000000000 ) ) ;
#48363 = CARTESIAN_POINT ( 'NONE',  ( -52.69240448066584293, -53.30312580971443026, 41.38025477438755928 ) ) ;
#48364 = CARTESIAN_POINT ( 'NONE',  ( -143.2587158300142107, 60.34092810886538416, -38.15695033877188536 ) ) ;
#48365 =( GEOMETRIC_REPRESENTATION_CONTEXT ( 3 ) GLOBAL_UNCERTAINTY_ASSIGNED_CONTEXT ( ( #14197 ) ) GLOBAL_UNIT_ASSIGNED_CONTEXT ( ( #36592, #31645, #30623 ) ) REPRESENTATION_CONTEXT ( 'NONE', 'WORKASPACE' ) );
#48366 = CARTESIAN_POINT ( 'NONE',  ( -165.7140086129056158, 80.68381997492571145, -70.27195394581150367 ) ) ;
#48368 = EDGE_LOOP ( 'NONE', ( #53203, #64773, #20295, #16268, #14812, #13028, #19438, #43547, #47353, #30835 ) ) ;
#48367 = CARTESIAN_POINT ( 'NONE',  ( -142.8450945664715164, 58.72815783657288335, -38.85811206571208487 ) ) ;
#48369 = CARTESIAN_POINT ( 'NONE',  ( -24.98026281234600887, 0.9932118737287082277, 0.000000000000000000 ) ) ;
#48370 = ORIENTED_EDGE ( 'NONE', *, *, #40498, .F. ) ;
#48372 = EDGE_CURVE ( 'NONE', #27916, #11578, #3248, .T. ) ;
#48371 = CARTESIAN_POINT ( 'NONE',  ( -190.6985136298601731, 109.1272424661242582, 94.99999999999866418 ) ) ;
#48373 = CARTESIAN_POINT ( 'NONE',  ( 429.8372781065087906, 388.0000000000066507, -133.9497041420121377 ) ) ;
#48374 = CARTESIAN_POINT ( 'NONE',  ( 135.4423125506059193, 42.39015362494583883, -24.01277294691661268 ) ) ;
#48375 = CARTESIAN_POINT ( 'NONE',  ( 88.98408042523108463, 20.23787745328938215, -77.29091413920239972 ) ) ;
#48376 = DIRECTION ( 'NONE',  ( -0.000000000000000000, -0.000000000000000000, -1.000000000000000000 ) ) ;
#48377 = CARTESIAN_POINT ( 'NONE',  ( -99.31850058233797540, 31.30166762705810513, 18.06902438764207020 ) ) ;
#48378 = DIRECTION ( 'NONE',  ( -0.000000000000000000, 1.000000000000000000, -0.000000000000000000 ) ) ;
#48379 = VERTEX_POINT ( 'NONE', #7379 ) ;
#48380 = ORIENTED_EDGE ( 'NONE', *, *, #61150, .F. ) ;
#48381 = VECTOR ( 'NONE', #37609, 1000.000000000000000 ) ;
#48382 = CARTESIAN_POINT ( 'NONE',  ( 188.5837490358996433, 86.53279111916960176, -70.88036999316274489 ) ) ;
#48383 = CARTESIAN_POINT ( 'NONE',  ( 69.68177367721199289, -20.52767805628082698, 170.0000000000000000 ) ) ;
#48384 = CARTESIAN_POINT ( 'NONE',  ( 0.000000000000000000, 0.000000000000000000, 40.00000000000003553 ) ) ;
#48385 = CARTESIAN_POINT ( 'NONE',  ( 26.99999999999999645, -27.00000000000000355, 12.00000000000000000 ) ) ;
#48386 = CARTESIAN_POINT ( 'NONE',  ( 103.1534365798307959, 26.83148826706845469, -67.76694820224788884 ) ) ;
#48387 = CIRCLE ( 'NONE', #33823, 74.95140232871122521 ) ;
#48388 = CARTESIAN_POINT ( 'NONE',  ( 84.74140601443112075, 18.78541996275573212, 44.47455478255000116 ) ) ;
#48389 = CARTESIAN_POINT ( 'NONE',  ( 66.07923263163411320, 14.44036440558002354, -50.07076703234795190 ) ) ;
#48390 = CARTESIAN_POINT ( 'NONE',  ( -119.2804658695888236, 43.47213805166353495, 34.57302842571210277 ) ) ;
#48391 = CARTESIAN_POINT ( 'NONE',  ( 212.1931396682533091, 117.2245435827728954, 63.86598910989989264 ) ) ;
#48392 = PRODUCT_DEFINITION_SHAPE ( 'NONE', 'NONE',  #23342 ) ;
#48393 = ORIENTED_EDGE ( 'NONE', *, *, #55587, .F. ) ;
#48394 = CARTESIAN_POINT ( 'NONE',  ( -55.05276343752910151, -170.0000000000000000, -15.87177340799618364 ) ) ;
#48395 = EDGE_CURVE ( 'NONE', #32729, #23927, #66827, .T. ) ;
#48396 = ORIENTED_EDGE ( 'NONE', *, *, #5050, .F. ) ;
#48397 = VECTOR ( 'NONE', #60427, 1000.000000000000000 ) ;
#48398 = VECTOR ( 'NONE', #12111, 1000.000000000000000 ) ;
#48399 = CARTESIAN_POINT ( 'NONE',  ( 0.000000000000000000, 0.000000000000000000, 0.000000000000000000 ) ) ;
#48400 = CARTESIAN_POINT ( 'NONE',  ( -81.67541167344860753, 23.49044848824860665, 84.73050038251950866 ) ) ;
#48401 = CARTESIAN_POINT ( 'NONE',  ( 93.32228019177713918, 22.88890999585038699, 60.66295313681071377 ) ) ;
#48402 = DIRECTION ( 'NONE',  ( -1.644874880248581709E-16, -1.882710788443314728E-16, 1.000000000000000000 ) ) ;
#48403 = DIRECTION ( 'NONE',  ( -0.8118923937861950435, -0.5838071093367415143, 0.000000000000000000 ) ) ;
#48404 = CARTESIAN_POINT ( 'NONE',  ( -94.83794676023110526, 30.26879337035744655, -68.29633011496009942 ) ) ;
#48405 = ADVANCED_FACE ( 'NONE', ( #39379 ), #17574, .F. ) ;
#48406 = CARTESIAN_POINT ( 'NONE',  ( 116.1038088070373675, 32.81248144313010329, -92.41388108080619190 ) ) ;
#48407 = VERTEX_POINT ( 'NONE', #60482 ) ;
#48408 = CARTESIAN_POINT ( 'NONE',  ( -61.36325649057843634, 43.03793052543095854, 41.38025477438755928 ) ) ;
#48409 = CARTESIAN_POINT ( 'NONE',  ( -439.4229916354183842, 394.9999999999998295, -128.9497041420121093 ) ) ;
#48410 = ORIENTED_EDGE ( 'NONE', *, *, #48803, .T. ) ;
#48411 = CARTESIAN_POINT ( 'NONE',  ( 62.53356220515463093, 13.59349015304565178, 56.65751152968498161 ) ) ;
#48412 = SURFACE_SIDE_STYLE ('',( #6925 ) ) ;
#48413 = CARTESIAN_POINT ( 'NONE',  ( -7.825402957745081878, 7.899365992529268965, 3.271030448983517580 ) ) ;
#48414 = LINE ( 'NONE', #48765, #32301 ) ;
#48415 = CARTESIAN_POINT ( 'NONE',  ( -6.851003965218994018, 6.829052369041588300, 30.16287756619037452 ) ) ;
#48416 = CARTESIAN_POINT ( 'NONE',  ( -31.43908319763709969, 10.61114334766715928, 72.06100499665289760 ) ) ;
#48417 = CARTESIAN_POINT ( 'NONE',  ( 79.13548761208615190, 18.05107300752372623, 90.44251185706802687 ) ) ;
#48418 = EDGE_CURVE ( 'NONE', #16361, #68856, #50976, .T. ) ;
#48419 = VERTEX_POINT ( 'NONE', #60129 ) ;
#48420 = CARTESIAN_POINT ( 'NONE',  ( 571.0906130828565210, 908.9915846175127854, 803.5068267248682332 ) ) ;
#48421 = CARTESIAN_POINT ( 'NONE',  ( -154.0833774771448645, 69.51012195447351871, 71.02675010485698692 ) ) ;
#48423 = ADVANCED_FACE ( 'NONE', ( #8060 ), #13010, .F. ) ;
#48422 = LINE ( 'NONE', #49476, #37658 ) ;
#48424 = EDGE_CURVE ( 'NONE', #55222, #11778, #34110, .T. ) ;
#48425 = CARTESIAN_POINT ( 'NONE',  ( -104.5916564445179802, 35.10571011602406344, 72.01391628937817302 ) ) ;
#48426 = CARTESIAN_POINT ( 'NONE',  ( -133.1640943168118554, 52.70734926280007215, -40.55218783485771894 ) ) ;
#48427 = EDGE_LOOP ( 'NONE', ( #39508, #56610, #16990, #13893 ) ) ;
#48428 = DIRECTION ( 'NONE',  ( 0.000000000000000000, 0.000000000000000000, 1.000000000000000000 ) ) ;
#48429 = CARTESIAN_POINT ( 'NONE',  ( -2.190131154568196958, 6.589492063460818727, -21.02878240156981349 ) ) ;
#48430 = CARTESIAN_POINT ( 'NONE',  ( -155.0443000888154472, 69.02121705336244872, 86.81356557659563578 ) ) ;
#48431 = CARTESIAN_POINT ( 'NONE',  ( 140.1999945597798956, 45.38880890490930398, 33.00061941519715702 ) ) ;
#48432 = VERTEX_POINT ( 'NONE', #50286 ) ;
#48433 = CARTESIAN_POINT ( 'NONE',  ( 70.34686579112866411, -18.11777090454118877, 0.000000000000000000 ) ) ;
#48434 = CARTESIAN_POINT ( 'NONE',  ( 80.71682498289320051, 18.54204664833079264, 15.00838200872322759 ) ) ;
#48435 = CARTESIAN_POINT ( 'NONE',  ( 157.9121974517528315, 59.27335488206247760, 2.564916881789687242 ) ) ;
#48436 = CARTESIAN_POINT ( 'NONE',  ( -31.73109720166984715, 21.50890660541002219, 13.32819299319723072 ) ) ;
#48437 = VECTOR ( 'NONE', #54315, 1000.000000000000000 ) ;
#48438 = AXIS2_PLACEMENT_3D ( 'NONE', #19499, #57148, #51525 ) ;
#48439 = VERTEX_POINT ( 'NONE', #2108 ) ;
#48440 = PLANE ( 'NONE',  #67686 ) ;
#48441 = B_SPLINE_CURVE_WITH_KNOTS ( 'NONE', 3,
 ( #27421, #23560, #38684, #60133, #11947, #50289, #66140, #702, #44997, #39730, #33764, #22156, #17577, #49923, #1753, #2111, #27775, #33420, #17929, #6672, #60829, #39042, #43600, #60486, #32709, #55201, #28476, #62577, #35845, #34471, #68204, #41119, #35494, #24943, #3150, #18968, #14394, #45349, #56955, #62216, #40416, #67507, #56597, #55913, #45701, #61186, #29180, #67860, #23902, #57297, #8777, #46381, #2794, #19656, #9110, #19305, #61863, #30562, #50624, #2445, #52013, #46733, #3828, #20012 ),
 .UNSPECIFIED., .F., .F.,
 ( 4, 2, 2, 2, 2, 2, 2, 2, 2, 2, 2, 2, 2, 2, 2, 2, 2, 2, 2, 2, 2, 2, 2, 2, 2, 2, 2, 2, 2, 2, 2, 4 ),
 ( 0.000000000000000000, 0.002176927744816822309, 0.003265391617225233897, 0.004353855489633644618, 0.004898087425837850846, 0.005442319362042056206, 0.006530783234450467795, 0.007619247106858878515, 0.008707710979267289236, 0.009796174851675701692, 0.01088463872408411241, 0.01197310259649252313, 0.01306156646890093559, 0.01415003034130934631, 0.01523849421371775703, 0.01632695808612616775, 0.01741542195853457847, 0.01959234970335132012, 0.02068081357575972043, 0.02176927744816812074, 0.02285774132057652105, 0.02394620519298491790, 0.02612313293780171158, 0.02666736487400589786, 0.02721159681021008414, 0.02830006068261845323, 0.02938852455502682232, 0.03047698842743518793, 0.03156545229984356049, 0.03265391617225192611, 0.03374238004466029867, 0.03483084391706866428 ),
 .UNSPECIFIED. ) ;
#48442 = CIRCLE ( 'NONE', #18166, 24.99999999999985434 ) ;
#48443 = ORIENTED_EDGE ( 'NONE', *, *, #3813, .F. ) ;
#48444 = CARTESIAN_POINT ( 'NONE',  ( -109.3432140528234697, 36.51591785955880454, -39.94014320226850856 ) ) ;
#48445 = CARTESIAN_POINT ( 'NONE',  ( -7.825402957745087207, -170.0000000000000000, 91.30468222037457338 ) ) ;
#48447 = ORIENTED_EDGE ( 'NONE', *, *, #52622, .F. ) ;
#48446 = DIRECTION ( 'NONE',  ( -1.000000000000000000, -0.000000000000000000, -0.000000000000000000 ) ) ;
#48448 = CARTESIAN_POINT ( 'NONE',  ( 164.4728833318992258, 63.30716077995678148, 39.60918866813992878 ) ) ;
#48449 = AXIS2_PLACEMENT_3D ( 'NONE', #58038, #31317, #53083 ) ;
#48450 = DIRECTION ( 'NONE',  ( 1.000000000000000000, 0.000000000000000000, 0.000000000000000000 ) ) ;
#48451 = DIRECTION ( 'NONE',  ( -1.000000000000000000, 0.000000000000000000, 0.000000000000000000 ) ) ;
#48452 = ORIENTED_EDGE ( 'NONE', *, *, #68814, .T. ) ;
#48453 = EDGE_CURVE ( 'NONE', #54841, #35686, #39728, .T. ) ;
#48454 = FACE_OUTER_BOUND ( 'NONE', #46565, .T. ) ;
#48455 = EDGE_CURVE ( 'NONE', #5030, #36947, #55910, .T. ) ;
#48456 = FACE_OUTER_BOUND ( 'NONE', #2981, .T. ) ;
#48457 = CARTESIAN_POINT ( 'NONE',  ( -165.9986675144416211, 79.53506019208359135, 40.68902089630642394 ) ) ;
#48458 = CARTESIAN_POINT ( 'NONE',  ( -33.84080342750782933, 9.997552308299095358, -76.78360896099182753 ) ) ;
#48459 = ORIENTED_EDGE ( 'NONE', *, *, #58656, .T. ) ;
#48460 = ORIENTED_EDGE ( 'NONE', *, *, #4704, .F. ) ;
#48461 = ORIENTED_EDGE ( 'NONE', *, *, #26581, .F. ) ;
#48462 =( LENGTH_UNIT ( ) NAMED_UNIT ( * ) SI_UNIT ( .MILLI., .METRE. ) );
#48463 = CARTESIAN_POINT ( 'NONE',  ( -47.55517274199435462, 12.79855951204728370, 91.88478847849279418 ) ) ;
#48464 = CARTESIAN_POINT ( 'NONE',  ( 444.9999999999999432, -35.00000000000000000, 380.0000000000000000 ) ) ;
#48465 = CARTESIAN_POINT ( 'NONE',  ( -153.6931187576189473, 67.81270084382356345, -75.38512700933921451 ) ) ;
#48466 = B_SPLINE_CURVE_WITH_KNOTS ( 'NONE', 3,
 ( #47751, #37551, #32286, #9449, #31586, #31941, #58648, #47072, #21373, #69553, #41803, #53026, #4853, #69214, #48094, #21038, #9798, #42817, #63945, #4512, #42488, #36876, #63262, #37202, #5203, #10471, #47405, #42142, #26657, #16094, #64286, #62918, #59000, #68536, #10819, #53718, #36181, #5540, #26994, #48425, #256, #30909, #63606, #14718 ),
 .UNSPECIFIED., .F., .F.,
 ( 4, 2, 2, 2, 2, 2, 2, 2, 2, 2, 2, 2, 2, 2, 2, 2, 2, 2, 2, 2, 2, 4 ),
 ( 0.02477387709520259204, 0.02633314402883780297, 0.02711277749565540671, 0.02789241096247300697, 0.02945167789610821096, 0.03023131136292582510, 0.03101094482974343924, 0.03257021176337864671, 0.03334984523019624003, 0.03412947869701383335, 0.03568874563064902000, 0.03646837909746659945, 0.03724801256428417195, 0.03802764603110174446, 0.03880727949791931697, 0.04036654643155445504, 0.04192581336518959312, 0.04348508029882473813, 0.04504434723245986927, 0.04660361416609501428, 0.04816288109973015236, 0.04972214803336529043 ),
 .UNSPECIFIED. ) ;
#48467 = CARTESIAN_POINT ( 'NONE',  ( -107.4812999401992073, 35.50239240081075565, 86.29593079873286854 ) ) ;
#48468 = DIRECTION ( 'NONE',  ( 0.000000000000000000, -6.405132834375902056E-16, 1.000000000000000000 ) ) ;
#48469 = EDGE_CURVE ( 'NONE', #25366, #18610, #38681, .T. ) ;
#48470 = CARTESIAN_POINT ( 'NONE',  ( 7.762887554996211747E-14, 51.66904755831208718, 85.00100000000000477 ) ) ;
#48471 = CARTESIAN_POINT ( 'NONE',  ( 8.113421703707349053, 0.000000000000000000, 5.845715376051984435 ) ) ;
#48472 = ADVANCED_FACE ( 'NONE', ( #68539 ), #24941, .T. ) ;
#48473 = ORIENTED_EDGE ( 'NONE', *, *, #66109, .T. ) ;
#48474 = CYLINDRICAL_SURFACE ( 'NONE', #34129, 5.000000000000000888 ) ;
#48475 = ORIENTED_EDGE ( 'NONE', *, *, #16884, .T. ) ;
#48476 = CARTESIAN_POINT ( 'NONE',  ( -20.63749999999999574, 0.000000000000000000, -25.00000000000000711 ) ) ;
#48477 = APPLICATION_CONTEXT ( 'automotive_design' ) ;
#48478 = CARTESIAN_POINT ( 'NONE',  ( 206.7099580236349823, 109.1417833474364727, -63.43384006045138790 ) ) ;
#48479 = EDGE_CURVE ( 'NONE', #31182, #45146, #63265, .T. ) ;
#48480 = DIRECTION ( 'NONE',  ( -1.000000000000000000, 0.000000000000000000, 0.000000000000000000 ) ) ;
#48481 = LINE ( 'NONE', #316, #14432 ) ;
#48482 = CARTESIAN_POINT ( 'NONE',  ( -125.8938041572051389, 47.69968343338781125, 72.46449846362081360 ) ) ;
#48483 = CARTESIAN_POINT ( 'NONE',  ( 16.77480716385437631, 7.540753720029939267, 30.06375086438559308 ) ) ;
#48484 = EDGE_CURVE ( 'NONE', #43433, #49905, #11033, .T. ) ;
#48485 = CARTESIAN_POINT ( 'NONE',  ( -46.66904755831210139, 6.635317295611287136E-14, 85.00100000000000477 ) ) ;
#48486 = CARTESIAN_POINT ( 'NONE',  ( 0.000000000000000000, 0.000000000000000000, 113.5502958579881749 ) ) ;
#48487 = ORIENTED_EDGE ( 'NONE', *, *, #35664, .T. ) ;
#48488 = VECTOR ( 'NONE', #33712, 1000.000000000000000 ) ;
#48489 = CARTESIAN_POINT ( 'NONE',  ( 6.400000000000000355, 6.613092715395708453E-16, 5.400000000000001243 ) ) ;
#48490 = CARTESIAN_POINT ( 'NONE',  ( -75.31295361348102801, 9.223176757708264319E-15, 0.000000000000000000 ) ) ;
#48491 = EDGE_LOOP ( 'NONE', ( #28719, #9981, #66679, #26567 ) ) ;
#48492 = EDGE_LOOP ( 'NONE', ( #64288, #49585, #11931, #66924, #46520, #42841 ) ) ;
#48493 = CARTESIAN_POINT ( 'NONE',  ( -79.62258606008208517, 22.68765733708494636, 30.46417967397961490 ) ) ;
#48494 = LINE ( 'NONE', #330, #61277 ) ;
#48495 = CARTESIAN_POINT ( 'NONE',  ( 63.01563776193091826, 12.67277567978498531, -50.72069083216976537 ) ) ;
#48496 = CIRCLE ( 'NONE', #57529, 60.00000000000000000 ) ;
#48497 = AXIS2_PLACEMENT_3D ( 'NONE', #25713, #10195, #15495 ) ;
#48498 = CARTESIAN_POINT ( 'NONE',  ( -30.47069031368415537, 9.433993659086574723, 57.10770550136132329 ) ) ;
#48499 = FACE_OUTER_BOUND ( 'NONE', #1381, .T. ) ;
#48500 = EDGE_CURVE ( 'NONE', #51645, #46238, #29870, .T. ) ;
#48501 = VECTOR ( 'NONE', #11186, 1000.000000000000000 ) ;
#48502 = ORIENTED_EDGE ( 'NONE', *, *, #34324, .T. ) ;
#48503 = CLOSED_SHELL ( 'NONE', ( #33295, #10017, #20995, #45121, #24561, #61684 ) ) ;
#48504 = EDGE_LOOP ( 'NONE', ( #13009, #9800 ) ) ;
#48505 = EDGE_CURVE ( 'NONE', #168, #38167, #45700, .T. ) ;
#48506 = EDGE_CURVE ( 'NONE', #59279, #44163, #40912, .T. ) ;
#48507 = CARTESIAN_POINT ( 'NONE',  ( 8.904582680623983393, 23.36040254969773144, 0.000000000000000000 ) ) ;
#48508 = VERTEX_POINT ( 'NONE', #47075 ) ;
#48509 = CARTESIAN_POINT ( 'NONE',  ( 437.3372781065085633, 400.0000000000000568, -136.4497041420118251 ) ) ;
#48510 = CARTESIAN_POINT ( 'NONE',  ( -147.1538409485623333, 63.51600817366542628, 31.09618653746209560 ) ) ;
#48511 = CARTESIAN_POINT ( 'NONE',  ( 55.90910788310616653, 11.13585330978403931, 66.60498196571883511 ) ) ;
#48512 = DIRECTION ( 'NONE',  ( 0.000000000000000000, -0.000000000000000000, 1.000000000000000000 ) ) ;
#48513 = CARTESIAN_POINT ( 'NONE',  ( 70.34686579112866411, -18.11777090454118877, 170.0000000000000000 ) ) ;
#48514 = CARTESIAN_POINT ( 'NONE',  ( 15.55634918610409656, 36.11269837220803680, 2.000000000000001776 ) ) ;
#48515 = PLANE ( 'NONE',  #907 ) ;
#48516 = ORIENTED_EDGE ( 'NONE', *, *, #49797, .F. ) ;
#48517 = VERTEX_POINT ( 'NONE', #63609 ) ;
#48518 = FACE_OUTER_BOUND ( 'NONE', #9887, .T. ) ;
#48519 = DIRECTION ( 'NONE',  ( -0.000000000000000000, 0.8660254037844381525, 0.5000000000000008882 ) ) ;
#48520 = DIRECTION ( 'NONE',  ( 0.000000000000000000, -0.000000000000000000, -1.000000000000000000 ) ) ;
#48521 = DIRECTION ( 'NONE',  ( -0.000000000000000000, 1.000000000000000000, -0.000000000000000000 ) ) ;
#48522 = CARTESIAN_POINT ( 'NONE',  ( 67.55134213333074911, 13.77030723107741217, 31.31968777660861036 ) ) ;
#48523 = CARTESIAN_POINT ( 'NONE',  ( 20.62738791527532101, 7.711277635208470649, 85.46445541659694811 ) ) ;
#48524 = ORIENTED_EDGE ( 'NONE', *, *, #35664, .F. ) ;
#48525 = CARTESIAN_POINT ( 'NONE',  ( 79.14242532928585661, 17.00090225993928783, 10.87724778048851881 ) ) ;
#48526 = ORIENTED_EDGE ( 'NONE', *, *, #8502, .T. ) ;
#48527 = CARTESIAN_POINT ( 'NONE',  ( -76.78936026062119424, 21.61552955137052479, 30.65294656790032946 ) ) ;
#48528 = VERTEX_POINT ( 'NONE', #37905 ) ;
#48529 = CIRCLE ( 'NONE', #18246, 25.00000000000000711 ) ;
#48530 = ORIENTED_EDGE ( 'NONE', *, *, #25030, .T. ) ;
#48531 = CARTESIAN_POINT ( 'NONE',  ( -142.2626321327577728, 58.26997216742665842, -71.11658358797649271 ) ) ;
#48532 = CARTESIAN_POINT ( 'NONE',  ( -49.77357484059193382, 41.82599373102802787, 170.0000000000000000 ) ) ;
#48533 = CYLINDRICAL_SURFACE ( 'NONE', #203, 200.0000000000000000 ) ;
#48534 = VECTOR ( 'NONE', #28076, 1000.000000000000114 ) ;
#48535 = ORIENTED_EDGE ( 'NONE', *, *, #51461, .T. ) ;
#48536 = LINE ( 'NONE', #59801, #45769 ) ;
#48537 = VECTOR ( 'NONE', #16119, 1000.000000000000000 ) ;
#48538 = CARTESIAN_POINT ( 'NONE',  ( -444.3832201885272184, 394.6953840236894280, 96.77545299096836118 ) ) ;
#48539 = EDGE_CURVE ( 'NONE', #21176, #16065, #64289, .T. ) ;
#48540 = CARTESIAN_POINT ( 'NONE',  ( 152.3102623290679958, 53.74757787434990774, 42.35763419393935436 ) ) ;
#48541 = CARTESIAN_POINT ( 'NONE',  ( 68.94948716683069279, 15.16699441119057745, 32.69983809954490539 ) ) ;
#48542 = DIRECTION ( 'NONE',  ( -0.000000000000000000, -0.000000000000000000, -1.000000000000000000 ) ) ;
#48543 = CARTESIAN_POINT ( 'NONE',  ( -442.6627218934912662, 394.9999999999998295, 91.05029585798840230 ) ) ;
#48544 = DIRECTION ( 'NONE',  ( 0.000000000000000000, -1.000000000000000000, 0.000000000000000000 ) ) ;
#48545 = DIRECTION ( 'NONE',  ( -0.000000000000000000, -0.000000000000000000, 1.000000000000000000 ) ) ;
#48546 = CARTESIAN_POINT ( 'NONE',  ( -145.3246383987845149, 62.00818849034187252, -75.38709678301769657 ) ) ;
#48547 = ORIENTED_EDGE ( 'NONE', *, *, #24071, .F. ) ;
#48548 = VECTOR ( 'NONE', #9385, 1000.000000000000114 ) ;
#48549 = FACE_BOUND ( 'NONE', #22255, .T. ) ;
#48550 = CARTESIAN_POINT ( 'NONE',  ( -3.252497086158839590, 6.636017118947989957, -75.72773057492425153 ) ) ;
#48551 = PRESENTATION_STYLE_ASSIGNMENT (( #53498 ) ) ;
#48552 = CARTESIAN_POINT ( 'NONE',  ( -146.7404675333698378, 63.17262273741977907, -8.493795772565299274 ) ) ;
#48553 = CARTESIAN_POINT ( 'NONE',  ( -123.0348077379026677, 45.83489305753316501, -35.47620429563009026 ) ) ;
#48554 = CARTESIAN_POINT ( 'NONE',  ( -84.53753601793930272, 25.73343139558516768, 6.379961366978447401 ) ) ;
#48555 = DIRECTION ( 'NONE',  ( 9.729521028634720986E-15, -5.551115123125782702E-17, 1.000000000000000000 ) ) ;
#48556 = LINE ( 'NONE', #27469, #12342 ) ;
#48557 = EDGE_CURVE ( 'NONE', #52201, #34184, #37206, .T. ) ;
#48558 = FACE_OUTER_BOUND ( 'NONE', #55837, .T. ) ;
#48559 = DIRECTION ( 'NONE',  ( 0.000000000000000000, 0.000000000000000000, 1.000000000000000000 ) ) ;
#48560 = CARTESIAN_POINT ( 'NONE',  ( 157.9130201331580565, 57.99550255803048060, 2.564916881789690351 ) ) ;
#48561 = CARTESIAN_POINT ( 'NONE',  ( 92.52113039222226121, 22.58921125235803018, -11.81011023875010935 ) ) ;
#48562 = ORIENTED_EDGE ( 'NONE', *, *, #23576, .T. ) ;
#48563 = CARTESIAN_POINT ( 'NONE',  ( -31.93169728792083362, 10.69234447276977562, 18.37190381572552056 ) ) ;
#48564 = ORIENTED_EDGE ( 'NONE', *, *, #4218, .T. ) ;
#48565 = CARTESIAN_POINT ( 'NONE',  ( -33.97701964160389565, -17.74986561234010551, 13.32819299319722894 ) ) ;
#48566 = EDGE_LOOP ( 'NONE', ( #41574, #3357, #27792, #47489 ) ) ;
#48567 = EDGE_CURVE ( 'NONE', #60670, #68142, #25673, .T. ) ;
#48568 = CARTESIAN_POINT ( 'NONE',  ( 84.26390409839191875, 19.68678207880321551, -63.03273511366791126 ) ) ;
#48569 = CARTESIAN_POINT ( 'NONE',  ( 116.3939302320144691, 32.95725513882212709, 86.49556688537334992 ) ) ;
#48570 = CARTESIAN_POINT ( 'NONE',  ( -142.3187766126155225, 59.59460822661996815, 62.85579774729529845 ) ) ;
#48571 = CARTESIAN_POINT ( 'NONE',  ( 64.94794467308302899, 13.12874966082104322, -9.112897588248744185 ) ) ;
#48572 = CARTESIAN_POINT ( 'NONE',  ( -28.13128612339709278, 10.08889185338653327, -36.06824119723449229 ) ) ;
#48573 = DIRECTION ( 'NONE',  ( -1.000000000000000000, 0.000000000000000000, 0.000000000000000000 ) ) ;
#48574 = CARTESIAN_POINT ( 'NONE',  ( -72.70872533823838069, 21.20779489546082885, -91.74330869458320592 ) ) ;
#48575 = CARTESIAN_POINT ( 'NONE',  ( -137.3060924980642596, 138.4631249211268482, 0.000000000000000000 ) ) ;
#48576 = ORIENTED_EDGE ( 'NONE', *, *, #7236, .T. ) ;
#48577 = ORIENTED_EDGE ( 'NONE', *, *, #47618, .F. ) ;
#48578 = CARTESIAN_POINT ( 'NONE',  ( 36.98541457540710553, 9.120571655722411464, 71.37510936658638627 ) ) ;
#48579 = CARTESIAN_POINT ( 'NONE',  ( -166.7136514167008556, 81.71618216218796249, 61.25921454291933088 ) ) ;
#48580 = CARTESIAN_POINT ( 'NONE',  ( 68.07999999999999829, -26.09918303830819397, 30.00000000000000000 ) ) ;
#48581 = PRODUCT_DEFINITION_CONTEXT ( 'detailed design', #9390, 'design' ) ;
#48582 = AXIS2_PLACEMENT_3D ( 'NONE', #10227, #35595, #3574 ) ;
#48583 = CARTESIAN_POINT ( 'NONE',  ( 70.26840926437850499, 15.51363403943109631, -95.00000000000133582 ) ) ;
#48584 = EDGE_LOOP ( 'NONE', ( #31629, #32562, #8356, #8986, #52400, #3414, #50965, #64259 ) ) ;
#48585 = EDGE_CURVE ( 'NONE', #8745, #31701, #10474, .T. ) ;
#48586 = CARTESIAN_POINT ( 'NONE',  ( 3.678442866637813759E-12, -65.13282190615278466, -5.000000000000000000 ) ) ;
#48587 = CARTESIAN_POINT ( 'NONE',  ( 185.7267155939801739, 84.90388481853123892, -22.77551174952004942 ) ) ;
#48588 = CARTESIAN_POINT ( 'NONE',  ( 211.3757499519975909, 117.8130818709823444, 13.28818959658699939 ) ) ;
#48589 = AXIS2_PLACEMENT_3D ( 'NONE', #40635, #63142, #51887 ) ;
#48590 = CARTESIAN_POINT ( 'NONE',  ( 307.2575771313985342, 0.000000000000000000, 256.6193948016162381 ) ) ;
#48591 = CARTESIAN_POINT ( 'NONE',  ( 41.09671232177016265, 8.635892912882342287, -23.58539976383162795 ) ) ;
#48592 = DIRECTION ( 'NONE',  ( -0.000000000000000000, -0.000000000000000000, 1.000000000000000000 ) ) ;
#48593 = DIRECTION ( 'NONE',  ( 1.000000000000000000, 0.000000000000000000, 0.000000000000000000 ) ) ;
#48594 = ADVANCED_FACE ( 'NONE', ( #53723 ), #43167, .T. ) ;
#48595 = CARTESIAN_POINT ( 'NONE',  ( 163.5944442552010401, 63.88381951184479846, 68.09088869929966847 ) ) ;
#48596 = AXIS2_PLACEMENT_3D ( 'NONE', #5190, #15057, #57965 ) ;
#48597 = VECTOR ( 'NONE', #1554, 1000.000000000000000 ) ;
#48598 = ORIENTED_EDGE ( 'NONE', *, *, #13881, .T. ) ;
#48599 = CARTESIAN_POINT ( 'NONE',  ( 130.3035708464390439, 40.48418876551456691, 16.78814384215078448 ) ) ;
#48600 = CARTESIAN_POINT ( 'NONE',  ( 8.820885042877430138, 74.43053605947413587, 41.38025477438755928 ) ) ;
#48601 = CIRCLE ( 'NONE', #14941, 8.000000000000000000 ) ;
#48602 = CARTESIAN_POINT ( 'NONE',  ( -47.79955240516187587, 13.88975739862079628, 62.68960868740774828 ) ) ;
#48603 = CARTESIAN_POINT ( 'NONE',  ( -5.000000000000026645, -15.55634918610403616, 0.000000000000000000 ) ) ;
#48604 = DIRECTION ( 'NONE',  ( 1.000000000000000000, -0.000000000000000000, 0.000000000000000000 ) ) ;
#48605 = CARTESIAN_POINT ( 'NONE',  ( -5.275096591305005411, 7.745869104888358336, 84.24396437760638889 ) ) ;
#48606 = ORIENTED_EDGE ( 'NONE', *, *, #55107, .F. ) ;
#48607 = CARTESIAN_POINT ( 'NONE',  ( 59.08638499266955790, 11.79550614876702141, 4.075424172557957192 ) ) ;
#48608 = CARTESIAN_POINT ( 'NONE',  ( -61.39252081892698953, 16.47343302442958546, 60.64715025453807584 ) ) ;
#48609 = ORIENTED_EDGE ( 'NONE', *, *, #8920, .F. ) ;
#48610 = ORIENTED_EDGE ( 'NONE', *, *, #2837, .T. ) ;
#48611 = CARTESIAN_POINT ( 'NONE',  ( 31.89306456119750521, 8.562405279423517257, 90.54126529181490923 ) ) ;
#48612 = CARTESIAN_POINT ( 'NONE',  ( -1.068536314442417146, 51.65427688837380060, 26.66469104408687230 ) ) ;
#48613 = CARTESIAN_POINT ( 'NONE',  ( 88.98064924903391670, 21.30386569031176691, -63.04019652766769610 ) ) ;
#48614 = ORIENTED_EDGE ( 'NONE', *, *, #62427, .T. ) ;
#48615 = CARTESIAN_POINT ( 'NONE',  ( -59.94781924509480575, 16.04872117907065032, -63.87327874414468454 ) ) ;
#48616 = CARTESIAN_POINT ( 'NONE',  ( 37.70762885381311236, 8.195134395012276585, -8.965104318115102444 ) ) ;
#48617 = CARTESIAN_POINT ( 'NONE',  ( 175.8947993867357127, 74.90689716047910451, -49.16091051003656531 ) ) ;
#48618 = CARTESIAN_POINT ( 'NONE',  ( -151.2428028786328014, 66.99705074331123456, -76.46685696349274508 ) ) ;
#48619 = CARTESIAN_POINT ( 'NONE',  ( 64.16679220703369424, 10.37413986118183828, 170.0000000000000000 ) ) ;
#48620 = EDGE_CURVE ( 'NONE', #55364, #12081, #21377, .T. ) ;
#48621 = ORIENTED_EDGE ( 'NONE', *, *, #19463, .T. ) ;
#48622 = CARTESIAN_POINT ( 'NONE',  ( -47.55256438668344288, 13.83151366677316219, -42.95852722453810202 ) ) ;
#48623 = EDGE_CURVE ( 'NONE', #25048, #8863, #23418, .T. ) ;
#48624 = VECTOR ( 'NONE', #31081, 1000.000000000000000 ) ;
#48625 = LINE ( 'NONE', #42683, #2224 ) ;
#48626 = CARTESIAN_POINT ( 'NONE',  ( 12.68603346975294599, 7.427591953486039955, 44.34740265932830994 ) ) ;
#48627 = CARTESIAN_POINT ( 'NONE',  ( 204.6977192012829505, 108.0580384837234931, -78.17048162308530834 ) ) ;
#48628 = CARTESIAN_POINT ( 'NONE',  ( 55.00000000000000000, 16.00000000000000000, -5.803681084894614095 ) ) ;
#48629 = CARTESIAN_POINT ( 'NONE',  ( -83.98097503028121480, 25.50453459670680800, 86.30605427587425993 ) ) ;
#48631 = ORIENTED_EDGE ( 'NONE', *, *, #39402, .F. ) ;
#48630 = DIRECTION ( 'NONE',  ( -0.000000000000000000, 1.000000000000000000, -0.000000000000000000 ) ) ;
#48632 = ORIENTED_EDGE ( 'NONE', *, *, #15575, .F. ) ;
#48633 = VECTOR ( 'NONE', #47894, 1000.000000000000000 ) ;
#48634 = EDGE_LOOP ( 'NONE', ( #34699, #52794, #26441, #3279 ) ) ;
#48635 = CARTESIAN_POINT ( 'NONE',  ( -9.771516655894552983, 7.025139475821121415, -23.33315609593830686 ) ) ;
#48636 = CARTESIAN_POINT ( 'NONE',  ( -49.43915770973590895, 13.24768844696974845, 42.81511741946465577 ) ) ;
#48637 = LINE ( 'NONE', #65198, #19918 ) ;
#48638 = CARTESIAN_POINT ( 'NONE',  ( 211.9978709542735373, 172.0000000000000284, 276.7363262511108815 ) ) ;
#48639 = VECTOR ( 'NONE', #65478, 1000.000000000000000 ) ;
#48640 = EDGE_CURVE ( 'NONE', #3417, #43209, #32630, .T. ) ;
#48641 = CARTESIAN_POINT ( 'NONE',  ( -35.38962320578852427, 11.29584325137384937, 70.94093902761839843 ) ) ;
#48642 = CARTESIAN_POINT ( 'NONE',  ( -15.07235766390729026, 8.482541916553470784, -18.02097754923428852 ) ) ;
#48643 = DIRECTION ( 'NONE',  ( 0.000000000000000000, 0.000000000000000000, -1.000000000000000000 ) ) ;
#48644 = CARTESIAN_POINT ( 'NONE',  ( 23.28785143291466397, 6.856621069835718174, -16.67558055457178057 ) ) ;
#48645 = ORIENTED_EDGE ( 'NONE', *, *, #14894, .T. ) ;
#48646 = VECTOR ( 'NONE', #45164, 1000.000000000000000 ) ;
#48647 = DIRECTION ( 'NONE',  ( 0.000000000000000000, 1.000000000000000000, -0.000000000000000000 ) ) ;
#48648 = ORIENTED_EDGE ( 'NONE', *, *, #33742, .F. ) ;
#48649 = EDGE_CURVE ( 'NONE', #66845, #17049, #64642, .T. ) ;
#48650 = ORIENTED_EDGE ( 'NONE', *, *, #48453, .F. ) ;
#48651 = ADVANCED_FACE ( 'NONE', ( #15760 ), #36880, .T. ) ;
#48652 = CARTESIAN_POINT ( 'NONE',  ( -22.50000000000000355, -17.50000000000000000, 0.000000000000000000 ) ) ;
#48653 = CARTESIAN_POINT ( 'NONE',  ( 0.4964154566688004921, -8.859816792613663949, 0.6543471694412422712 ) ) ;
#48654 = AXIS2_PLACEMENT_3D ( 'NONE', #46530, #56751, #41268 ) ;
#48655 = LINE ( 'NONE', #16325, #43589 ) ;
#48656 = CARTESIAN_POINT ( 'NONE',  ( -157.0069571479806996, 72.18154199622281908, 11.07571264450559312 ) ) ;
#48657 = CARTESIAN_POINT ( 'NONE',  ( -107.7743374187917595, 35.66028478413599601, 16.30335207078181980 ) ) ;
#48658 = CARTESIAN_POINT ( 'NONE',  ( 17.74393407086870056, 6.570779001277778697, 44.77212087285361974 ) ) ;
#48659 = CARTESIAN_POINT ( 'NONE',  ( -157.0040855759218630, 72.17887538959165283, 92.33198874388405386 ) ) ;
#48660 = ORIENTED_EDGE ( 'NONE', *, *, #32710, .F. ) ;
#48661 = ORIENTED_EDGE ( 'NONE', *, *, #38442, .F. ) ;
#48662 = ORIENTED_EDGE ( 'NONE', *, *, #61615, .F. ) ;
#48663 =( BOUNDED_CURVE ( )  B_SPLINE_CURVE ( 3, ( #28506, #49950, #32735, #48884 ),
 .UNSPECIFIED., .F., .F. ) 
 B_SPLINE_CURVE_WITH_KNOTS ( ( 4, 4 ),
 ( 1.570796326794911879, 3.141592653589817985 ),
 .UNSPECIFIED. ) 
 CURVE ( )  GEOMETRIC_REPRESENTATION_ITEM ( )  RATIONAL_B_SPLINE_CURVE ( ( 1.000000000000000000, 0.8047378541243627170, 0.8047378541243627170, 1.000000000000000000 ) ) 
 REPRESENTATION_ITEM ( '' )  );
#48664 = CARTESIAN_POINT ( 'NONE',  ( -8.320652113663527416, 6.923290556636832349, 18.27103044898354867 ) ) ;
#48665 = CARTESIAN_POINT ( 'NONE',  ( 88.21281915446409982, 21.03303114364613435, -89.66901925827936282 ) ) ;
#48666 = CARTESIAN_POINT ( 'NONE',  ( -38.26497993382596263, 10.81185389040528122, 67.67827709005032943 ) ) ;
#48667 = DIRECTION ( 'NONE',  ( 1.020422603260505347E-14, -1.000000000000000000, -5.551115123125782702E-17 ) ) ;
#48668 = ORIENTED_EDGE ( 'NONE', *, *, #56242, .T. ) ;
#48669 = CARTESIAN_POINT ( 'NONE',  ( 184.3966782763551748, 83.48172388049827930, 56.90975353678252446 ) ) ;
#48670 = CARTESIAN_POINT ( 'NONE',  ( -156.9252506979473196, 70.73559306219777909, 63.92116529121810942 ) ) ;
#48671 = CARTESIAN_POINT ( 'NONE',  ( -7.825402957745081878, 7.899365992529270741, -50.41807073194384259 ) ) ;
#48672 = CARTESIAN_POINT ( 'NONE',  ( 3.306546357697853733E-15, 35.00000000000000000, 27.00000000000000000 ) ) ;
#48673 = CARTESIAN_POINT ( 'NONE',  ( 23.93060502292685499, -7.646171227524485303, 3.061616997868437868E-16 ) ) ;
#48674 = PLANE ( 'NONE',  #46524 ) ;
#48676 = EDGE_CURVE ( 'NONE', #67501, #10586, #69557, .T. ) ;
#48675 = DIRECTION ( 'NONE',  ( -1.000000000000000000, 0.000000000000000000, 0.000000000000000000 ) ) ;
#48677 = CYLINDRICAL_SURFACE ( 'NONE', #50079, 5.000000000000004441 ) ;
#48678 = DIRECTION ( 'NONE',  ( -0.8160245890732938934, -0.5780171883497599028, 0.000000000000000000 ) ) ;
#48679 = AXIS2_PLACEMENT_3D ( 'NONE', #813, #65895, #39154 ) ;
#48680 = ORIENTED_EDGE ( 'NONE', *, *, #17155, .F. ) ;
#48682 = PLANE ( 'NONE',  #54009 ) ;
#48681 = PRESENTATION_LAYER_ASSIGNMENT (  '', '', ( #36372 ) ) ;
#48683 = CARTESIAN_POINT ( 'NONE',  ( 177.7889574972182345, 75.33777460203562271, 30.05619048107344327 ) ) ;
#48684 = CARTESIAN_POINT ( 'NONE',  ( -127.6992109187851980, 47.69334801994794049, -49.70753535056091721 ) ) ;
#48685 = DIRECTION ( 'NONE',  ( 1.000000000000000000, 1.232595164407830672E-32, -5.551115123125781716E-16 ) ) ;
#48686 = CARTESIAN_POINT ( 'NONE',  ( 55.99998955208977947, 12.18058389017404686, -67.40205469635807844 ) ) ;
#48687 = ORIENTED_EDGE ( 'NONE', *, *, #35697, .T. ) ;
#48688 = VECTOR ( 'NONE', #45853, 1000.000000000000000 ) ;
#48689 = ORIENTED_EDGE ( 'NONE', *, *, #16244, .F. ) ;
#48690 = VECTOR ( 'NONE', #59399, 1000.000000000000000 ) ;
#48691 = CARTESIAN_POINT ( 'NONE',  ( -125.8938041572051105, 46.49392987655493670, -88.60280507916129977 ) ) ;
#48692 = VECTOR ( 'NONE', #37456, 1000.000000000000000 ) ;
#48693 = CARTESIAN_POINT ( 'NONE',  ( 198.2581645178918848, 99.52881771501677122, 13.71845634271636172 ) ) ;
#48694 = ORIENTED_EDGE ( 'NONE', *, *, #40056, .T. ) ;
#48695 = VERTEX_POINT ( 'NONE', #47408 ) ;
#48696 = DIRECTION ( 'NONE',  ( -0.000000000000000000, 1.000000000000000000, -0.000000000000000000 ) ) ;
#48697 = DIRECTION ( 'NONE',  ( -0.000000000000000000, -0.000000000000000000, -1.000000000000000000 ) ) ;
#48698 = ORIENTED_EDGE ( 'NONE', *, *, #36122, .F. ) ;
#48699 = CARTESIAN_POINT ( 'NONE',  ( 0.000000000000000000, 192.0000000000000000, 380.0000000000000000 ) ) ;
#48700 = CARTESIAN_POINT ( 'NONE',  ( 104.3786071038062033, 27.35811053916146562, -92.41772670280587931 ) ) ;
#48701 = CARTESIAN_POINT ( 'NONE',  ( 137.4031600461561027, 44.79620770172218869, 57.24220012813282210 ) ) ;
#48702 = DIRECTION ( 'NONE',  ( -0.000000000000000000, 1.000000000000000000, -0.000000000000000000 ) ) ;
#48703 = AXIS2_PLACEMENT_3D ( 'NONE', #47472, #26727, #69284 ) ;
#48705 = EDGE_CURVE ( 'NONE', #27359, #24527, #15419, .T. ) ;
#48704 = DIRECTION ( 'NONE',  ( 0.000000000000000000, 0.000000000000000000, -1.000000000000000000 ) ) ;
#48706 = CARTESIAN_POINT ( 'NONE',  ( 93.92910382125421620, 22.04227458821877761, -41.58192722603683222 ) ) ;
#48707 = ADVANCED_FACE ( 'NONE', ( #32289 ), #5543, .F. ) ;
#48708 = DIRECTION ( 'NONE',  ( -0.8160245890732938934, -0.5780171883497599028, 0.000000000000000000 ) ) ;
#48709 = EDGE_CURVE ( 'NONE', #55220, #5511, #260, .T. ) ;
#48710 = ORIENTED_EDGE ( 'NONE', *, *, #66879, .F. ) ;
#48711 = ORIENTED_EDGE ( 'NONE', *, *, #5193, .T. ) ;
#48712 = CARTESIAN_POINT ( 'NONE',  ( 8.000000000000000000, -1.555946510856143661, -0.06708870216335349745 ) ) ;
#48713 = EDGE_CURVE ( 'NONE', #3372, #17473, #5880, .T. ) ;
#48714 = LINE ( 'NONE', #6530, #35861 ) ;
#48715 = CARTESIAN_POINT ( 'NONE',  ( -15.55634918610405748, -10.55634918610400597, 0.000000000000000000 ) ) ;
#48716 = CARTESIAN_POINT ( 'NONE',  ( -165.6215009671260248, 80.58889799860442338, -68.74239935707777249 ) ) ;
#48718 = VERTEX_POINT ( 'NONE', #25978 ) ;
#48717 = CARTESIAN_POINT ( 'NONE',  ( -142.1381007084227122, 58.17237452544241449, -43.73358479738932658 ) ) ;
#48719 = DIRECTION ( 'NONE',  ( -0.000000000000000000, 1.000000000000000000, -0.000000000000000000 ) ) ;
#48720 = EDGE_CURVE ( 'NONE', #60730, #42757, #48778, .T. ) ;
#48721 = EDGE_LOOP ( 'NONE', ( #33984, #41954 ) ) ;
#48722 = CARTESIAN_POINT ( 'NONE',  ( -133.1093894320205777, 51.43221067881453479, 36.00316402828616447 ) ) ;
#48723 = CARTESIAN_POINT ( 'NONE',  ( -125.8938041572051389, -170.0000000000000000, 11.27539728269340280 ) ) ;
#48724 = CARTESIAN_POINT ( 'NONE',  ( 48.11816970607299027, -43.69944786993949748, 40.00000000000003553 ) ) ;
#48725 = CARTESIAN_POINT ( 'NONE',  ( 82.95057496836386690, 18.19812356106674400, -9.923320146636031680 ) ) ;
#48726 = CARTESIAN_POINT ( 'NONE',  ( 87.58098510096631628, 19.74745174099415479, -77.62095623220717755 ) ) ;
#48728 = CARTESIAN_POINT ( 'NONE',  ( 11.30618213853385967, 74.15344055032308290, 133.5802547743875550 ) ) ;
#48727 = CIRCLE ( 'NONE', #26327, 65.00000000000000000 ) ;
#48729 = CARTESIAN_POINT ( 'NONE',  ( -99.10260179032846395, 31.19580119595417500, 17.97233264255025986 ) ) ;
#48730 = CARTESIAN_POINT ( 'NONE',  ( -95.50384525802326152, 29.46973564057718420, -66.13451531431674368 ) ) ;
#48731 = ORIENTED_EDGE ( 'NONE', *, *, #55592, .F. ) ;
#48732 = EDGE_CURVE ( 'NONE', #68905, #13402, #31291, .T. ) ;
#48733 = ORIENTED_EDGE ( 'NONE', *, *, #2101, .T. ) ;
#48734 = EDGE_CURVE ( 'NONE', #8790, #66330, #4857, .T. ) ;
#48735 = AXIS2_PLACEMENT_3D ( 'NONE', #36766, #58211, #57186 ) ;
#48736 = CARTESIAN_POINT ( 'NONE',  ( 46.41758729921142645, 9.425975226414237795, 34.75085537779860800 ) ) ;
#48737 = FACE_OUTER_BOUND ( 'NONE', #23996, .T. ) ;
#48738 = CARTESIAN_POINT ( 'NONE',  ( 0.000000000000000000, 0.000000000000000000, 41.38025477438755928 ) ) ;
#48739 = DIRECTION ( 'NONE',  ( -1.000000000000000000, 0.000000000000000000, 0.000000000000000000 ) ) ;
#48740 = VECTOR ( 'NONE', #63336, 1000.000000000000000 ) ;
#48741 = B_SPLINE_CURVE_WITH_KNOTS ( 'NONE', 3,
 ( #2150, #49972, #12348, #7068 ),
 .UNSPECIFIED., .F., .F.,
 ( 4, 4 ),
 ( 0.1259919275528358917, 0.1829744153748748825 ),
 .UNSPECIFIED. ) ;
#48742 = CARTESIAN_POINT ( 'NONE',  ( -53.31111153860302210, 37.18770477615724701, 170.0000000000000000 ) ) ;
#48743 = CARTESIAN_POINT ( 'NONE',  ( -76.79042791651912125, 22.68960395613480330, -62.19449990835644826 ) ) ;
#48744 = CYLINDRICAL_SURFACE ( 'NONE', #19072, 300.0000000000000000 ) ;
#48745 = VECTOR ( 'NONE', #33401, 1000.000000000000000 ) ;
#48746 = CARTESIAN_POINT ( 'NONE',  ( 46.12582897016702077, 10.39833982076224572, -39.78811412968926220 ) ) ;
#48747 = PLANE ( 'NONE',  #55409 ) ;
#48748 = ORIENTED_EDGE ( 'NONE', *, *, #12613, .F. ) ;
#48750 = CARTESIAN_POINT ( 'NONE',  ( -29.51272929882556539, 10.30144624948896670, 18.12442451181507508 ) ) ;
#48749 = AXIS2_PLACEMENT_3D ( 'NONE', #25654, #25309, #24959 ) ;
#48751 = VERTEX_POINT ( 'NONE', #17484 ) ;
#48752 = CARTESIAN_POINT ( 'NONE',  ( -11.78792974237933677, 7.181513757308656487, -49.29051053082125833 ) ) ;
#48753 = VECTOR ( 'NONE', #50992, 1000.000000000000227 ) ;
#48754 = FACE_OUTER_BOUND ( 'NONE', #50313, .T. ) ;
#48755 = CARTESIAN_POINT ( 'NONE',  ( 15.78827728214693416, 6.500811158483328356, -8.674393508222097537 ) ) ;
#48756 = CARTESIAN_POINT ( 'NONE',  ( 152.1190604254709910, 53.60705199010330801, -22.04039180145268162 ) ) ;
#48757 = CARTESIAN_POINT ( 'NONE',  ( 37.45439421541016145, 9.177432671831375899, 17.82874747546184580 ) ) ;
#48758 = DIRECTION ( 'NONE',  ( -0.000000000000000000, -0.000000000000000000, 1.000000000000000000 ) ) ;
#48759 = CARTESIAN_POINT ( 'NONE',  ( -24.39249304643438521, 60.24953346690454481, 40.00000000000003553 ) ) ;
#48760 = CARTESIAN_POINT ( 'NONE',  ( 209.9451731426637480, 113.8261094108102753, 85.02890187354657314 ) ) ;
#48761 = DIRECTION ( 'NONE',  ( 0.000000000000000000, 0.000000000000000000, -1.000000000000000000 ) ) ;
#48762 = ORIENTED_EDGE ( 'NONE', *, *, #6454, .T. ) ;
#48763 = LINE ( 'NONE', #16770, #65451 ) ;
#48764 = CYLINDRICAL_SURFACE ( 'NONE', #28643, 7.500000000000013323 ) ;
#48765 = CARTESIAN_POINT ( 'NONE',  ( 0.000000000000000000, 29.79383981485516841, -24.99999999999999645 ) ) ;
#48766 = CARTESIAN_POINT ( 'NONE',  ( -7.825402957745087207, 6.891034867348158954, 45.11558103944722120 ) ) ;
#48767 = DIRECTION ( 'NONE',  ( -0.6910626489868580968, -0.7227948638273978821, 0.000000000000000000 ) ) ;
#48768 = CARTESIAN_POINT ( 'NONE',  ( 86.98327316344760618, 20.60587179896667465, 83.40257220075987732 ) ) ;
#48769 = B_SPLINE_CURVE_WITH_KNOTS ( 'NONE', 3,
 ( #57197, #56492, #13253, #46279, #40660, #3046 ),
 .UNSPECIFIED., .F., .F.,
 ( 4, 2, 4 ),
 ( 0.03218933327099851582, 0.06469831623231186990, 0.09720729919362522398 ),
 .UNSPECIFIED. ) ;
#48770 = EDGE_LOOP ( 'NONE', ( #66582, #24277 ) ) ;
#48771 = DIRECTION ( 'NONE',  ( 9.978129433818594407E-15, -1.000000000000000000, -3.941291737419305719E-15 ) ) ;
#48772 = CARTESIAN_POINT ( 'NONE',  ( -151.6797345123119101, 67.37848486615948218, 72.25752099154021835 ) ) ;
#48773 = CYLINDRICAL_SURFACE ( 'NONE', #55647, 4.999999999999990230 ) ;
#48774 = CARTESIAN_POINT ( 'NONE',  ( -167.6524579626394882, 82.69702609844095775, -47.35039770195071895 ) ) ;
#48775 = CONTEXT_DEPENDENT_SHAPE_REPRESENTATION ( #43975, #18162 ) ;
#48776 = CARTESIAN_POINT ( 'NONE',  ( -132.0870433264403516, 51.94057326482884207, -38.17611669845395284 ) ) ;
#48777 = ORIENTED_EDGE ( 'NONE', *, *, #42506, .T. ) ;
#48778 = LINE ( 'NONE', #64993, #67260 ) ;
#48779 = DIRECTION ( 'NONE',  ( -1.000000000000000000, 0.000000000000000000, 0.000000000000000000 ) ) ;
#48780 = CARTESIAN_POINT ( 'NONE',  ( 198.8752826725510943, 100.3130050945022873, -21.71571402821468766 ) ) ;
#48781 = CARTESIAN_POINT ( 'NONE',  ( -150.1435789396691121, 64.71993001749778784, 84.41785612803083438 ) ) ;
#48782 = VECTOR ( 'NONE', #5985, 1000.000000000000114 ) ;
#48783 = CYLINDRICAL_SURFACE ( 'NONE', #961, 7.500000000000020428 ) ;
#48784 = EDGE_LOOP ( 'NONE', ( #7747, #39531, #50225, #18731 ) ) ;
#48785 = CARTESIAN_POINT ( 'NONE',  ( 0.000000000000000000, 0.000000000000000000, -8.000000000000000000 ) ) ;
#48786 = CARTESIAN_POINT ( 'NONE',  ( 79.37778929114109872, 18.12554302172301135, 12.34647733481867604 ) ) ;
#48787 = CARTESIAN_POINT ( 'NONE',  ( -149.9471644042847345, 65.87751327280743396, 30.73052297110500319 ) ) ;
#48788 = AXIS2_PLACEMENT_3D ( 'NONE', #47919, #69026, #26136 ) ;
#48789 = EDGE_LOOP ( 'NONE', ( #56183, #16798, #13423, #41260, #10244 ) ) ;
#48790 = VECTOR ( 'NONE', #66386, 1000.000000000000114 ) ;
#48791 = DIRECTION ( 'NONE',  ( 0.000000000000000000, 0.000000000000000000, 1.000000000000000000 ) ) ;
#48792 = CIRCLE ( 'NONE', #57819, 74.95140232871122521 ) ;
#48793 = EDGE_CURVE ( 'NONE', #4017, #51087, #34026, .T. ) ;
#48794 = VERTEX_POINT ( 'NONE', #34385 ) ;
#48795 = EDGE_LOOP ( 'NONE', ( #36715, #51401, #35649, #68217 ) ) ;
#48796 = B_SPLINE_CURVE_WITH_KNOTS ( 'NONE', 3,
 ( #51023, #60869, #45040, #12694, #66871, #34160, #18670, #55596, #40461, #61905, #24648, #40122, #61579, #13392, #13729, #35188, #67551, #36575, #10512, #46423, #26019, #35883, #24991, #4898, #21087, #19697, #68580, #31303, #57686, #57339, #42532, #20381, #52059, #58024, #15463, #52730, #9496, #4220, #15116, #47801, #25340, #36917, #20052, #41163 ),
 .UNSPECIFIED., .F., .F.,
 ( 4, 2, 2, 2, 2, 2, 2, 2, 2, 2, 2, 2, 2, 2, 2, 2, 2, 2, 2, 2, 2, 4 ),
 ( 1.398578778534940505E-17, 0.004120577325733468244, 0.006180865988600218845, 0.008241154651466969447, 0.01030144331433372092, 0.01133158764576706369, 0.01236173197720040300, 0.01339187630863374404, 0.01442202064006708681, 0.01545216497150042785, 0.01648230930293376889, 0.01699738146865044375, 0.01751245363436711167, 0.01854259796580047526, 0.01957274229723383191, 0.02060288662866719550, 0.02266317529153392962, 0.02472346395440066374, 0.02678375261726739440, 0.02781389694870080309, 0.02884404128013421179, 0.03296461860586794718 ),
 .UNSPECIFIED. ) ;
#48797 = CARTESIAN_POINT ( 'NONE',  ( -118.6666422341620688, 41.91578446950640569, -94.04183589441188929 ) ) ;
#48798 = AXIS2_PLACEMENT_3D ( 'NONE', #52543, #25829, #47255 ) ;
#48799 = DIRECTION ( 'NONE',  ( 0.000000000000000000, 0.000000000000000000, 1.000000000000000000 ) ) ;
#48801 = VERTEX_POINT ( 'NONE', #22766 ) ;
#48800 = CARTESIAN_POINT ( 'NONE',  ( 151.6178224291901131, 54.48737267587418387, 14.76196231147637050 ) ) ;
#48802 = CARTESIAN_POINT ( 'NONE',  ( 164.9559213734324601, 63.71338633026439879, 37.45297374046533889 ) ) ;
#48803 = EDGE_CURVE ( 'NONE', #62926, #47295, #23482, .T. ) ;
#48804 = DIRECTION ( 'NONE',  ( -0.000000000000000000, -0.000000000000000000, 1.000000000000000000 ) ) ;
#48805 = DIRECTION ( 'NONE',  ( 0.000000000000000000, 1.000000000000000000, 0.000000000000000000 ) ) ;
#48806 = ORIENTED_EDGE ( 'NONE', *, *, #2918, .T. ) ;
#48807 = DIRECTION ( 'NONE',  ( 0.000000000000000000, 0.000000000000000000, -1.000000000000000000 ) ) ;
#48808 = B_SPLINE_CURVE_WITH_KNOTS ( 'NONE', 3,
 ( #16500, #5257, #28091, #63998, #11918, #32680, #26717, #54105, #33029, #54820, #48147, #5930, #22473, #21770, #15810, #48829, #43214, #49535, #21101, #27742, #64339, #16151, #49183, #59057, #67152, #65749, #8392, #33736, #50951, #28808, #17545, #1366, #44629, #2763, #18941, #13325, #6993, #66454, #39354, #34782, #8035, #12623, #2418, #7352 ),
 .UNSPECIFIED., .F., .F.,
 ( 4, 2, 2, 2, 2, 2, 2, 2, 2, 2, 2, 2, 2, 2, 2, 2, 2, 2, 2, 2, 2, 4 ),
 ( 0.02814986980477066428, 0.02995274102020803464, 0.03085417662792673543, 0.03175561223564543623, 0.03355848345108280312, 0.03536135466652017695, 0.03716422588195755772, 0.03896709709739493155, 0.03986853270511362540, 0.04076996831283231926, 0.04167140392055100617, 0.04257283952826969309, 0.04347427513598838000, 0.04437571074370706692, 0.04527714635142575383, 0.04617858195914444075, 0.04798145317458180070, 0.04978432439001916759, 0.05158719560545653449, 0.05339006682089389444, 0.05519293803633125439, 0.05699580925176862128 ),
 .UNSPECIFIED. ) ;
#48809 = CARTESIAN_POINT ( 'NONE',  ( -37.79823708645146496, 10.72197716414928692, -19.95651543701835351 ) ) ;
#48810 = CARTESIAN_POINT ( 'NONE',  ( -180.4651598106648294, 97.28730001475651079, 39.87329604086140478 ) ) ;
#48811 = CARTESIAN_POINT ( 'NONE',  ( -38.26497993382596974, 10.81185389040525280, -66.54447586226808653 ) ) ;
#48812 = EDGE_CURVE ( 'NONE', #64523, #67945, #43859, .T. ) ;
#48813 = EDGE_LOOP ( 'NONE', ( #6563, #9136, #63794, #38128 ) ) ;
#48814 = VERTEX_POINT ( 'NONE', #66404 ) ;
#48815 = ORIENTED_EDGE ( 'NONE', *, *, #63368, .T. ) ;
#48816 = FACE_OUTER_BOUND ( 'NONE', #44273, .T. ) ;
#48817 = PLANE ( 'NONE',  #44758 ) ;
#48818 = DIRECTION ( 'NONE',  ( 0.000000000000000000, 0.000000000000000000, 1.000000000000000000 ) ) ;
#48819 = LINE ( 'NONE', #68911, #4495 ) ;
#48820 = CARTESIAN_POINT ( 'NONE',  ( 23.17627457812186620, -71.32923872213625316, 43.58025477438756212 ) ) ;
#48821 = DIRECTION ( 'NONE',  ( -0.000000000000000000, -0.000000000000000000, -1.000000000000000000 ) ) ;
#48822 = CARTESIAN_POINT ( 'NONE',  ( -51.16305185958752588, 14.71032321365092521, 85.08607359302328632 ) ) ;
#48823 = CARTESIAN_POINT ( 'NONE',  ( 79.93126905972553686, 17.24332478304276250, 60.67301135421717362 ) ) ;
#48824 = ORIENTED_EDGE ( 'NONE', *, *, #27455, .F. ) ;
#48825 = CIRCLE ( 'NONE', #18543, 65.00000000000000000 ) ;
#48826 = CARTESIAN_POINT ( 'NONE',  ( 429.8372781065085633, 400.0000000000000568, -128.9497041420118251 ) ) ;
#48827 = VERTEX_POINT ( 'NONE', #60404 ) ;
#48828 =( NAMED_UNIT ( * ) SI_UNIT ( $, .STERADIAN. ) SOLID_ANGLE_UNIT ( ) );
#48829 = CARTESIAN_POINT ( 'NONE',  ( 187.8959968237854241, 85.77553094678181367, 33.65882037824376738 ) ) ;
#48830 = DIRECTION ( 'NONE',  ( -4.270088556250601699E-16, -0.000000000000000000, -1.000000000000000000 ) ) ;
#48831 = CARTESIAN_POINT ( 'NONE',  ( -72.78737098446268305, 20.16853011470087864, 6.389890168941366078 ) ) ;
#48832 = CARTESIAN_POINT ( 'NONE',  ( 10.55634918610403084, -3.079134169858832593E-14, 0.000000000000000000 ) ) ;
#48833 = DIRECTION ( 'NONE',  ( -1.000000000000000000, 0.000000000000000000, 0.000000000000000000 ) ) ;
#48834 = CARTESIAN_POINT ( 'NONE',  ( 201.2497471985136315, 101.7319188750771275, 83.71170961202953720 ) ) ;
#48835 = CARTESIAN_POINT ( 'NONE',  ( 0.000000000000000000, 0.000000000000000000, 41.38025477438755928 ) ) ;
#48837 = DIRECTION ( 'NONE',  ( -0.000000000000000000, -0.000000000000000000, -1.000000000000000000 ) ) ;
#48836 = CIRCLE ( 'NONE', #58945, 300.0000000000000000 ) ;
#48838 = VECTOR ( 'NONE', #11494, 1000.000000000000000 ) ;
#48839 = EDGE_LOOP ( 'NONE', ( #15771, #63015, #62559, #65490 ) ) ;
#48840 = FACE_OUTER_BOUND ( 'NONE', #53803, .T. ) ;
#48841 = PLANE ( 'NONE',  #13894 ) ;
#48842 = VERTEX_POINT ( 'NONE', #38961 ) ;
#48843 = ORIENTED_EDGE ( 'NONE', *, *, #33051, .F. ) ;
#48844 = CARTESIAN_POINT ( 'NONE',  ( -86.17927978631389863, 25.32700573188344251, 37.93022061236076325 ) ) ;
#48845 = VECTOR ( 'NONE', #11095, 1000.000000000000000 ) ;
#48846 = CARTESIAN_POINT ( 'NONE',  ( -29.51272929882557250, 10.30144624948894361, -62.40922725957596384 ) ) ;
#48847 = CARTESIAN_POINT ( 'NONE',  ( 46.51377856795993182, 10.46037936279324754, 39.84532587672087089 ) ) ;
#48848 = CARTESIAN_POINT ( 'NONE',  ( -102.2801239173131194, -170.0000000000000000, -76.85912785543962400 ) ) ;
#48849 = AXIS2_PLACEMENT_3D ( 'NONE', #9702, #25199, #4418 ) ;
#48850 = FACE_OUTER_BOUND ( 'NONE', #4917, .T. ) ;
#48851 = ORIENTED_EDGE ( 'NONE', *, *, #42413, .F. ) ;
#48852 = ORIENTED_EDGE ( 'NONE', *, *, #45618, .F. ) ;
#48853 = DIRECTION ( 'NONE',  ( -0.000000000000000000, -6.405132834375902056E-16, 1.000000000000000000 ) ) ;
#48854 = VERTEX_POINT ( 'NONE', #6234 ) ;
#48855 = DIRECTION ( 'NONE',  ( -1.000000000000000000, -0.000000000000000000, -0.000000000000000000 ) ) ;
#48856 = CARTESIAN_POINT ( 'NONE',  ( 187.8389847489735018, 87.20903357420549185, -94.12450799417122482 ) ) ;
#48857 = DIRECTION ( 'NONE',  ( -1.000000000000000000, 0.000000000000000000, 0.000000000000000000 ) ) ;
#48858 = ADVANCED_FACE ( 'NONE', ( #2025 ), #32975, .T. ) ;
#48859 = DIRECTION ( 'NONE',  ( -4.691548276051970363E-18, 2.005263967813451899E-18, -1.000000000000000000 ) ) ;
#48860 = CARTESIAN_POINT ( 'NONE',  ( -29.34297344870648061, 10.27495334741685618, -89.30201075326299076 ) ) ;
#48861 = FACE_OUTER_BOUND ( 'NONE', #28965, .T. ) ;
#48862 = EDGE_CURVE ( 'NONE', #18218, #27522, #17784, .T. ) ;
#48863 = CARTESIAN_POINT ( 'NONE',  ( 50.97490815085634352, 0.000000000000000000, -9.435653166495500344 ) ) ;
#48864 = ORIENTED_EDGE ( 'NONE', *, *, #28577, .F. ) ;
#48865 = VERTEX_POINT ( 'NONE', #28388 ) ;
#48866 = DIRECTION ( 'NONE',  ( 0.000000000000000000, 0.9989683093773507050, 0.04541273895899305274 ) ) ;
#48867 = DIRECTION ( 'NONE',  ( -0.2660368455666826670, 0.9639628606958513535, 0.000000000000000000 ) ) ;
#48868 = DIRECTION ( 'NONE',  ( -1.387778780781445922E-16, 1.000000000000000000, 0.000000000000000000 ) ) ;
#48869 = CARTESIAN_POINT ( 'NONE',  ( 140.5781926063689014, 45.63383190293702540, -73.70520198257123923 ) ) ;
#48870 = CARTESIAN_POINT ( 'NONE',  ( 8.000000000000007105, 249.8719672152120381, 94.99999999999866418 ) ) ;
#48871 = ORIENTED_EDGE ( 'NONE', *, *, #60440, .F. ) ;
#48872 = EDGE_CURVE ( 'NONE', #55930, #14210, #50209, .T. ) ;
#48873 = CARTESIAN_POINT ( 'NONE',  ( 82.95057496836383848, 18.19812356106674400, 16.92123044382763908 ) ) ;
#48874 = EDGE_LOOP ( 'NONE', ( #61109, #30318, #43420, #58042 ) ) ;
#48875 = ADVANCED_FACE ( 'NONE', ( #47575 ), #56507, .F. ) ;
#48876 = CARTESIAN_POINT ( 'NONE',  ( -75.43953471071000649, 21.11829282998125734, 31.13110847576471230 ) ) ;
#48877 = ORIENTED_EDGE ( 'NONE', *, *, #6259, .F. ) ;
#48878 = AXIS2_PLACEMENT_3D ( 'NONE', #49620, #8732, #12354 ) ;
#48879 = CIRCLE ( 'NONE', #45550, 20.00000000000000000 ) ;
#48880 = VERTEX_POINT ( 'NONE', #20861 ) ;
#48881 = CARTESIAN_POINT ( 'NONE',  ( -125.4463376280758951, 47.40387005565906975, 3.785361193902134769 ) ) ;
#48882 = EDGE_CURVE ( 'NONE', #7248, #7351, #62795, .T. ) ;
#48883 = CARTESIAN_POINT ( 'NONE',  ( 93.92280655489128094, 22.03989931749465470, 8.601539047791877834 ) ) ;
#48884 = CARTESIAN_POINT ( 'NONE',  ( -447.6627218934912094, 389.9999999999997726, 108.5502958579879476 ) ) ;
#48885 = VECTOR ( 'NONE', #13415, 1000.000000000000000 ) ;
#48886 = VECTOR ( 'NONE', #59869, 1000.000000000000000 ) ;
#48887 = EDGE_LOOP ( 'NONE', ( #10132, #38037, #4461, #28586, #23692, #33886, #25160, #477 ) ) ;
#48888 = CARTESIAN_POINT ( 'NONE',  ( 56.74421265833558436, 32.44697398030906044, 41.38025477438755928 ) ) ;
#48889 = AXIS2_PLACEMENT_3D ( 'NONE', #29457, #65719, #12950 ) ;
#48890 = CARTESIAN_POINT ( 'NONE',  ( 151.3309484205704507, 53.03078371058069251, 41.22472127221216454 ) ) ;
#48891 = VECTOR ( 'NONE', #28606, 1000.000000000000000 ) ;
#48892 = CARTESIAN_POINT ( 'NONE',  ( -175.1968289912784371, 90.99944698359490758, -34.99253156508922302 ) ) ;
#48893 = FACE_OUTER_BOUND ( 'NONE', #1032, .T. ) ;
#48894 = DIRECTION ( 'NONE',  ( -1.000000000000000000, 0.000000000000000000, 0.000000000000000000 ) ) ;
#48895 = APPLICATION_CONTEXT ( 'automotive_design' ) ;
#48896 = CARTESIAN_POINT ( 'NONE',  ( 86.62931800182293784, 20.48449268398422163, 71.55663816294304524 ) ) ;
#48897 = ADVANCED_FACE ( 'NONE', ( #26488 ), #50889, .T. ) ;
#48898 = ORIENTED_EDGE ( 'NONE', *, *, #38765, .F. ) ;
#48899 = CARTESIAN_POINT ( 'NONE',  ( 424.8372781065087906, 395.0000000000042064, 91.05029585798442326 ) ) ;
#48900 = CARTESIAN_POINT ( 'NONE',  ( -143.2498117110515921, 60.33382252735061968, -73.29988522007047891 ) ) ;
#48901 = EDGE_LOOP ( 'NONE', ( #25868, #61650, #45494, #28117, #15569, #54819 ) ) ;
#48902 = EDGE_CURVE ( 'NONE', #27213, #46584, #63433, .T. ) ;
#48903 = EDGE_CURVE ( 'NONE', #34186, #39203, #25808, .T. ) ;
#48904 = FACE_BOUND ( 'NONE', #30066, .T. ) ;
#48905 = EDGE_CURVE ( 'NONE', #69498, #51848, #21213, .T. ) ;
#48906 = CARTESIAN_POINT ( 'NONE',  ( -4.504169684898453596, 6.697401007565304099, -63.03359714400242098 ) ) ;
#48907 = CARTESIAN_POINT ( 'NONE',  ( -175.1968289912784655, 90.99944698359492179, 72.38567079676552396 ) ) ;
#48908 = CYLINDRICAL_SURFACE ( 'NONE', #33836, 65.00000000000000000 ) ;
#48909 = CARTESIAN_POINT ( 'NONE',  ( -119.2949674747224975, 43.48097822533564738, -38.81081628568947650 ) ) ;
#48910 = CARTESIAN_POINT ( 'NONE',  ( -79.62207341875658528, 23.76621716825509623, 18.52792914764348353 ) ) ;
#48911 = LINE ( 'NONE', #31716, #16823 ) ;
#48912 = DIRECTION ( 'NONE',  ( 0.000000000000000000, 1.000000000000000000, -0.000000000000000000 ) ) ;
#48913 = CARTESIAN_POINT ( 'NONE',  ( -71.99036027973076557, 19.88994728656304289, -92.87964317901223410 ) ) ;
#48914 = CARTESIAN_POINT ( 'NONE',  ( 70.25990036603479894, 14.47042233282419943, 12.42607342676760496 ) ) ;
#48915 = CARTESIAN_POINT ( 'NONE',  ( 162.1014732644455307, 61.34312237409765345, 15.98357356154483533 ) ) ;
#48916 = CARTESIAN_POINT ( 'NONE',  ( 94.14197848494937659, 23.19876128416620631, -16.46679285838030893 ) ) ;
#48917 = ORIENTED_EDGE ( 'NONE', *, *, #42458, .T. ) ;
#48918 = CARTESIAN_POINT ( 'NONE',  ( -32.41898580403142915, 10.77423026598439471, 18.32383438413782528 ) ) ;
#48919 = ORIENTED_EDGE ( 'NONE', *, *, #16159, .F. ) ;
#48920 = CARTESIAN_POINT ( 'NONE',  ( -61.41100614348687969, 43.07262267896646790, 170.0000000000000000 ) ) ;
#48921 = CARTESIAN_POINT ( 'NONE',  ( 84.72546926745363294, 19.84015517905186599, -62.89578937353809351 ) ) ;
#48922 = CARTESIAN_POINT ( 'NONE',  ( 102.8837474253813014, 26.71671612110911553, 89.31275824274561614 ) ) ;
#48923 = CARTESIAN_POINT ( 'NONE',  ( -144.9417090887490360, 61.69631066549397502, 59.11060452198194781 ) ) ;
#48924 = LINE ( 'NONE', #38392, #55848 ) ;
#48925 = CARTESIAN_POINT ( 'NONE',  ( -24.18270484670773612, 9.527492911955590671, -40.85707012195633325 ) ) ;
#48926 = CARTESIAN_POINT ( 'NONE',  ( -48.70883077256302585, 14.10659259062419046, -73.56901164759405276 ) ) ;
#48927 = DIRECTION ( 'NONE',  ( 0.000000000000000000, 0.000000000000000000, -1.000000000000000000 ) ) ;
#48928 = CARTESIAN_POINT ( 'NONE',  ( -118.7011544766493500, 43.11604763363182968, -13.42784816232486733 ) ) ;
#48929 = EDGE_LOOP ( 'NONE', ( #64148, #4129, #23650, #26307 ) ) ;
#48930 = ORIENTED_EDGE ( 'NONE', *, *, #3834, .T. ) ;
#48931 = CARTESIAN_POINT ( 'NONE',  ( 38.43102714813442589, 9.298961820315048143, 56.80533550196272330 ) ) ;
#48932 = CARTESIAN_POINT ( 'NONE',  ( 176.0745160362857860, 73.68684431790050837, 69.23986300298068386 ) ) ;
#48933 = AXIS2_PLACEMENT_3D ( 'NONE', #39254, #34682, #60698 ) ;
#48934 =( LENGTH_UNIT ( ) NAMED_UNIT ( * ) SI_UNIT ( .MILLI., .METRE. ) );
#48935 = CARTESIAN_POINT ( 'NONE',  ( -166.3231866619663606, 81.31146386205588783, -12.18699256254814500 ) ) ;
#48936 = DIRECTION ( 'NONE',  ( -0.000000000000000000, 1.000000000000000000, -0.000000000000000000 ) ) ;
#48937 = ORIENTED_EDGE ( 'NONE', *, *, #39021, .F. ) ;
#48938 = CARTESIAN_POINT ( 'NONE',  ( 311.9975424824652350, 20.00000000000003197, 256.6193948016162381 ) ) ;
#48939 = AXIS2_PLACEMENT_3D ( 'NONE', #18362, #1487, #66571 ) ;
#48940 = CARTESIAN_POINT ( 'NONE',  ( 187.8973304652193690, 87.27378997243177139, -20.02744225065407946 ) ) ;
#48941 = CARTESIAN_POINT ( 'NONE',  ( 210.6584452238134872, 116.7138338345754249, 5.284484997206956969 ) ) ;
#48942 = CARTESIAN_POINT ( 'NONE',  ( -85.33861794503827980, 26.06603235258742401, -92.87200205917845608 ) ) ;
#48943 = CARTESIAN_POINT ( 'NONE',  ( -102.2801239173131194, -170.0000000000000000, 72.36362509687883460 ) ) ;
#48944 = CARTESIAN_POINT ( 'NONE',  ( -17.50000000000002842, -18.06806526123148160, 378.0000000000000000 ) ) ;
#48945 = CARTESIAN_POINT ( 'NONE',  ( 106.0251321087872896, 21.78917327468806064, -3.050596224313125493 ) ) ;
#48946 = AXIS2_PLACEMENT_3D ( 'NONE', #5537, #69549, #54402 ) ;
#48947 = CARTESIAN_POINT ( 'NONE',  ( -57.65733424639443427, 15.39521790791522982, -35.67890556914403533 ) ) ;
#48948 = AXIS2_PLACEMENT_3D ( 'NONE', #15539, #58429, #53140 ) ;
#48949 = EDGE_CURVE ( 'NONE', #57856, #12108, #42658, .T. ) ;
#48950 = VECTOR ( 'NONE', #28972, 1000.000000000000000 ) ;
#48951 = ORIENTED_EDGE ( 'NONE', *, *, #50004, .T. ) ;
#48952 = CYLINDRICAL_SURFACE ( 'NONE', #8801, 7.500000000000020428 ) ;
#48953 = DIRECTION ( 'NONE',  ( -0.000000000000000000, 1.000000000000000000, -0.000000000000000000 ) ) ;
#48954 = CARTESIAN_POINT ( 'NONE',  ( 86.62931800182293784, -170.0000000000000000, 29.71208757247930521 ) ) ;
#48955 = CARTESIAN_POINT ( 'NONE',  ( 2.694222958124177204E-15, 0.000000000000000000, 22.00000000000000355 ) ) ;
#48956 = CARTESIAN_POINT ( 'NONE',  ( 80.34841469379381351, -170.0000000000000000, 94.99999999999866418 ) ) ;
#48957 = DIRECTION ( 'NONE',  ( 1.000000000000000000, 0.000000000000000000, 3.556183125752454544E-16 ) ) ;
#48958 = B_SPLINE_CURVE_WITH_KNOTS ( 'NONE', 3,
 ( #23946, #2493, #66875, #7069, #40126, #34517, #28527, #54895, #61582, #66187, #49614, #34164, #13058, #50335, #1807, #23261 ),
 .UNSPECIFIED., .F., .F.,
 ( 4, 2, 2, 2, 2, 2, 2, 4 ),
 ( 0.01012072446094006324, 0.01138741587173669988, 0.01265410728253333825, 0.01392079869332997488, 0.01518749010412661152, 0.01645418151492324815, 0.01772087292571988479, 0.02025425574731319622 ),
 .UNSPECIFIED. ) ;
#48959 = ORIENTED_EDGE ( 'NONE', *, *, #61956, .T. ) ;
#48961 = EDGE_CURVE ( 'NONE', #8644, #21982, #5710, .T. ) ;
#48960 = CARTESIAN_POINT ( 'NONE',  ( -737.6000277536880958, -694.2189502691659300, 0.000000000000000000 ) ) ;
#48962 = ADVANCED_FACE ( 'NONE', ( #5708 ), #6415, .T. ) ;
#48963 = DIRECTION ( 'NONE',  ( -0.7071067811865545671, 2.831068712794148784E-15, -0.7071067811865405783 ) ) ;
#48964 = EDGE_LOOP ( 'NONE', ( #62920, #66463, #63961, #2810 ) ) ;
#48965 = EDGE_CURVE ( 'NONE', #50563, #24929, #11330, .T. ) ;
#48966 = ORIENTED_EDGE ( 'NONE', *, *, #28865, .F. ) ;
#48967 = DIRECTION ( 'NONE',  ( -0.6579387259397027066, -0.7530714660036196273, 0.000000000000000000 ) ) ;
#48968 = DIRECTION ( 'NONE',  ( 0.000000000000000000, 0.000000000000000000, 1.000000000000000000 ) ) ;
#48969 = CARTESIAN_POINT ( 'NONE',  ( 110.2429982417149290, 28.88204397445231209, 29.61121420573730489 ) ) ;
#48970 = ORIENTED_EDGE ( 'NONE', *, *, #28421, .T. ) ;
#48971 = ADVANCED_FACE ( 'NONE', ( #27868 ), #27163, .F. ) ;
#48972 = CARTESIAN_POINT ( 'NONE',  ( -56.72814287166055891, 15.13700122306437379, -62.24644308817313743 ) ) ;
#48973 = ORIENTED_EDGE ( 'NONE', *, *, #47021, .T. ) ;
#48974 = DIRECTION ( 'NONE',  ( 0.000000000000000000, 1.000000000000000000, -0.000000000000000000 ) ) ;
#48975 = CARTESIAN_POINT ( 'NONE',  ( 160.9099843287284557, 61.67000084894967671, 30.22885540498834800 ) ) ;
#48976 = CARTESIAN_POINT ( 'NONE',  ( 109.3154830994003390, 29.56170298203816316, 2.809493426657196480 ) ) ;
#48977 = LINE ( 'NONE', #54251, #56421 ) ;
#48978 = DIRECTION ( 'NONE',  ( 0.000000000000000000, 1.000000000000000000, 0.000000000000000000 ) ) ;
#48979 = CARTESIAN_POINT ( 'NONE',  ( -47.61402178322639855, 13.84598486314981614, -43.70512311542479011 ) ) ;
#48980 = AXIS2_PLACEMENT_3D ( 'NONE', #40808, #51025, #30610 ) ;
#48981 = LINE ( 'NONE', #43708, #67359 ) ;
#48982 = CARTESIAN_POINT ( 'NONE',  ( 8.767814708128309320, 7.383611927972574485, 34.86454251663690940 ) ) ;
#48983 = CARTESIAN_POINT ( 'NONE',  ( 69.71320131704045764, 14.32603187575852921, -93.43281573010639818 ) ) ;
#48984 = CARTESIAN_POINT ( 'NONE',  ( 79.12222162355536170, 16.99473220795134054, 90.79787899594637679 ) ) ;
#48985 = AXIS2_PLACEMENT_3D ( 'NONE', #15310, #4743, #52918 ) ;
#48987 = ORIENTED_EDGE ( 'NONE', *, *, #58801, .F. ) ;
#48986 = DIRECTION ( 'NONE',  ( -0.000000000000000000, -0.000000000000000000, -1.000000000000000000 ) ) ;
#48988 = EDGE_LOOP ( 'NONE', ( #42623, #15441, #25195, #62839 ) ) ;
#48989 = EDGE_CURVE ( 'NONE', #8166, #31066, #16613, .T. ) ;
#48990 = EDGE_CURVE ( 'NONE', #27835, #61270, #49307, .T. ) ;
#48991 = ORIENTED_EDGE ( 'NONE', *, *, #64567, .T. ) ;
#48992 = CARTESIAN_POINT ( 'NONE',  ( -12.78015296493258113, 7.264294661536299103, -10.42199259816774060 ) ) ;
#48993 = CARTESIAN_POINT ( 'NONE',  ( -51.34325167237330589, 13.71819364263221530, 44.34027758300791078 ) ) ;
#48994 = DIRECTION ( 'NONE',  ( 0.000000000000000000, 0.000000000000000000, -1.000000000000000000 ) ) ;
#48995 = DIRECTION ( 'NONE',  ( -0.000000000000000000, -0.000000000000000000, -1.000000000000000000 ) ) ;
#48996 = PRODUCT_DEFINITION_FORMATION_WITH_SPECIFIED_SOURCE ( 'ANY', '', #8064, .NOT_KNOWN. ) ;
#48997 = EDGE_CURVE ( 'NONE', #2626, #9719, #22945, .T. ) ;
#48998 = CARTESIAN_POINT ( 'NONE',  ( -60.47589866267036030, 17.25153113855769149, -47.90273905312907488 ) ) ;
#48999 = DIRECTION ( 'NONE',  ( 0.000000000000000000, -1.000000000000000000, 0.000000000000000000 ) ) ;
#49000 = CARTESIAN_POINT ( 'NONE',  ( 15.55634918610406103, 20.55634918610400064, 2.000000000000001776 ) ) ;
#49001 = DIRECTION ( 'NONE',  ( 1.000000000000000000, -1.243449787580175325E-14, 0.000000000000000000 ) ) ;
#49002 = ORIENTED_EDGE ( 'NONE', *, *, #61614, .F. ) ;
#49003 = AXIS2_PLACEMENT_3D ( 'NONE', #18688, #49279, #66544 ) ;
#49004 = DIRECTION ( 'NONE',  ( -0.9510565162951545304, 0.3090169943749447312, 2.500042656554810833E-16 ) ) ;
#49005 = ORIENTED_EDGE ( 'NONE', *, *, #44479, .F. ) ;
#49006 = EDGE_LOOP ( 'NONE', ( #56761, #31516, #10212, #39153 ) ) ;
#49007 = CARTESIAN_POINT ( 'NONE',  ( -39.55079474733624068, -51.59997227571039957, 43.58025477438756923 ) ) ;
#49008 = CARTESIAN_POINT ( 'NONE',  ( -60.67627457812130132, 44.08389392193514311, 0.000000000000000000 ) ) ;
#49009 = CARTESIAN_POINT ( 'NONE',  ( -26.69138721373299106, 9.876636144558636587, 85.59062689267271651 ) ) ;
#49010 = CARTESIAN_POINT ( 'NONE',  ( -96.78198318406110445, 30.07417864442862410, -47.63888010278168395 ) ) ;
#49011 = CARTESIAN_POINT ( 'NONE',  ( -109.7078892845591582, 36.71702188566221281, 12.24582890309084071 ) ) ;
#49012 = CARTESIAN_POINT ( 'NONE',  ( 21.73827885904430346, 6.764046335627707407, 32.94214015723378708 ) ) ;
#49013 = CARTESIAN_POINT ( 'NONE',  ( 134.3135005523731991, 42.87884033955812413, -24.16835682549730535 ) ) ;
#49014 = ORIENTED_EDGE ( 'NONE', *, *, #5096, .T. ) ;
#49015 = ORIENTED_EDGE ( 'NONE', *, *, #68529, .F. ) ;
#49016 = ORIENTED_EDGE ( 'NONE', *, *, #33835, .F. ) ;
#49017 = DIRECTION ( 'NONE',  ( 0.1342332658176667304, -0.9909497617679331460, 0.000000000000000000 ) ) ;
#49018 = DIRECTION ( 'NONE',  ( -0.7071067811865475727, 0.000000000000000000, 0.7071067811865475727 ) ) ;
#49019 = CARTESIAN_POINT ( 'NONE',  ( 31.90247004928965069, 8.563336936370820496, -43.62320764982623444 ) ) ;
#49020 = B_SPLINE_CURVE_WITH_KNOTS ( 'NONE', 3,
 ( #6068, #27530, #1774, #44681, #7399, #28857, #2124, #23577, #66500, #69412, #25316, #45721, #67197, #9127, #29197, #29530, #46056, #13369, #3496, #29888, #52030, #62935, #68222, #18639, #14408, #24966, #24621, #56266, #51000, #2811, #51689, #46397, #20030, #41483, #34492, #35859, #62235, #24274, #67877, #8083, #50643, #7748, #40099, #67527 ),
 .UNSPECIFIED., .F., .F.,
 ( 4, 2, 2, 2, 2, 2, 2, 2, 2, 2, 2, 2, 2, 2, 2, 2, 2, 2, 2, 2, 2, 4 ),
 ( 0.000000000000000000, 0.001487235713946833890, 0.002230853570920231319, 0.002974471427893629616, 0.004461707141840403658, 0.005948942855787178567, 0.007436178569733952609, 0.008179796426707356544, 0.008923414283680760478, 0.01041064999762751457, 0.01189788571157426693, 0.01264150356854762229, 0.01338512142552098112, 0.01487235713946772307, 0.01561597499644110446, 0.01635959285341448410, 0.01784682856736124340, 0.01933406428130800270, 0.02007768213828138235, 0.02082129999525476199, 0.02230853570920153170, 0.02379577142314830140 ),
 .UNSPECIFIED. ) ;
#49021 = CARTESIAN_POINT ( 'NONE',  ( -38.93878980550034896, 10.94326053663842124, 65.05816493757461672 ) ) ;
#49022 = CARTESIAN_POINT ( 'NONE',  ( 204.6977192012829505, 108.0580384837234931, 56.05227132923312183 ) ) ;
#49023 = VERTEX_POINT ( 'NONE', #10990 ) ;
#49024 = CARTESIAN_POINT ( 'NONE',  ( -452.6627218934913230, 1.665334536937734811E-13, 83.55029585798817493 ) ) ;
#49025 = LINE ( 'NONE', #22318, #65239 ) ;
#49026 =( LENGTH_UNIT ( ) NAMED_UNIT ( * ) SI_UNIT ( .MILLI., .METRE. ) );
#49027 = CARTESIAN_POINT ( 'NONE',  ( 278.3842135503132340, -21.48302731199174787, -4.742990268296088274 ) ) ;
#49028 = CARTESIAN_POINT ( 'NONE',  ( 102.7551177910568470, 25.56939188780863503, 9.769129899803088435 ) ) ;
#49029 = CYLINDRICAL_SURFACE ( 'NONE', #16278, 7.500000000000020428 ) ;
#49030 = CARTESIAN_POINT ( 'NONE',  ( -452.6627218934860366, 395.0000000000064801, -136.4497041420121661 ) ) ;
#49031 = DIRECTION ( 'NONE',  ( -0.000000000000000000, -0.000000000000000000, 1.000000000000000000 ) ) ;
#49032 = DIRECTION ( 'NONE',  ( -1.000000000000000000, 0.000000000000000000, 0.000000000000000000 ) ) ;
#49033 = CARTESIAN_POINT ( 'NONE',  ( 13.36262230781614946, 7.441298897118792333, 17.78385849237590222 ) ) ;
#49034 = ADVANCED_FACE ( 'NONE', ( #26831 ), #38070, .F. ) ;
#49035 = ORIENTED_EDGE ( 'NONE', *, *, #68306, .T. ) ;
#49036 = AXIS2_PLACEMENT_3D ( 'NONE', #42474, #62905, #4503 ) ;
#49037 = LINE ( 'NONE', #65599, #57463 ) ;
#49038 = CONTEXT_DEPENDENT_SHAPE_REPRESENTATION ( #6706, #51335 ) ;
#49039 = CARTESIAN_POINT ( 'NONE',  ( 0.000000000000000000, 0.000000000000000000, 85.00000000000000000 ) ) ;
#49040 = CARTESIAN_POINT ( 'NONE',  ( -133.1527834403230202, 51.46311219732124442, -40.50885773641505239 ) ) ;
#49041 = CARTESIAN_POINT ( 'NONE',  ( 39.89571693415783926, 8.473773298340393723, -62.46436805589144114 ) ) ;
#49042 = CARTESIAN_POINT ( 'NONE',  ( 59.30258796551118650, 12.87111270082601067, -76.60025956098559163 ) ) ;
#49043 = EDGE_LOOP ( 'NONE', ( #47249, #14911, #59774, #5892 ) ) ;
#49044 = VECTOR ( 'NONE', #12046, 1000.000000000000000 ) ;
#49045 = VECTOR ( 'NONE', #27482, 1000.000000000000000 ) ;
#49046 = ORIENTED_EDGE ( 'NONE', *, *, #68617, .F. ) ;
#49048 = EDGE_CURVE ( 'NONE', #44112, #17378, #5418, .T. ) ;
#49047 = CARTESIAN_POINT ( 'NONE',  ( -20.00000000000002842, 3.680555555555560243, 0.000000000000000000 ) ) ;
#49049 = DIRECTION ( 'NONE',  ( 0.000000000000000000, 0.000000000000000000, 1.000000000000000000 ) ) ;
#49050 = EDGE_LOOP ( 'NONE', ( #11969, #66313, #33378, #67180 ) ) ;
#49051 = VECTOR ( 'NONE', #43886, 1000.000000000000000 ) ;
#49052 = VERTEX_POINT ( 'NONE', #42987 ) ;
#49053 = CARTESIAN_POINT ( 'NONE',  ( 177.7960900018545374, 75.34533826015463376, -36.98054387538336130 ) ) ;
#49054 = EDGE_CURVE ( 'NONE', #45414, #32511, #22590, .T. ) ;
#49055 = DIRECTION ( 'NONE',  ( 1.000000000000000000, -0.000000000000000000, 0.000000000000000000 ) ) ;
#49056 = EDGE_LOOP ( 'NONE', ( #54805, #69492, #48396, #14787 ) ) ;
#49057 = CARTESIAN_POINT ( 'NONE',  ( 116.0963032583228198, 32.80867113471309438, 59.24019559371290455 ) ) ;
#49058 = ADVANCED_FACE ( 'NONE', ( #16269 ), #17310, .T. ) ;
#49059 = CARTESIAN_POINT ( 'NONE',  ( 134.0849965622594198, 42.73957449886185600, 56.35489142945906593 ) ) ;
#49060 = CARTESIAN_POINT ( 'NONE',  ( -73.63346300764936814, 20.46798018699518096, -48.18129300630896239 ) ) ;
#49061 = EDGE_CURVE ( 'NONE', #64521, #61561, #6052, .T. ) ;
#49062 = CARTESIAN_POINT ( 'NONE',  ( -95.04120270830171080, 29.25306318840326369, 40.04767500533338875 ) ) ;
#49063 = CARTESIAN_POINT ( 'NONE',  ( 89.22118407503259618, 20.32164250407898365, -36.27957951410743220 ) ) ;
#49064 = CARTESIAN_POINT ( 'NONE',  ( -47.55256438668344998, 13.83151366677316396, -16.11397663407440817 ) ) ;
#49065 = VERTEX_POINT ( 'NONE', #59170 ) ;
#49066 = CARTESIAN_POINT ( 'NONE',  ( 8.000000000000007105, 249.8719672152120381, 94.99999999999866418 ) ) ;
#49067 = CARTESIAN_POINT ( 'NONE',  ( -42.02161712141799654, -16.09918303830819397, 30.00000000000000000 ) ) ;
#49068 = CARTESIAN_POINT ( 'NONE',  ( -148.6471085600700235, 64.76880961642447687, -49.77594517346916803 ) ) ;
#49069 = DIRECTION ( 'NONE',  ( -0.7100673072878298520, -0.7041338076821836989, 0.000000000000000000 ) ) ;
#49071 = ORIENTED_EDGE ( 'NONE', *, *, #39661, .T. ) ;
#49070 = CARTESIAN_POINT ( 'NONE',  ( -132.9606448460427828, 51.32627791221455027, 94.40546275677576205 ) ) ;
#49072 = CARTESIAN_POINT ( 'NONE',  ( 60.61895554631706773, 13.15982272268127673, 17.59165741550849660 ) ) ;
#49073 = ORIENTED_EDGE ( 'NONE', *, *, #18989, .T. ) ;
#49074 = CARTESIAN_POINT ( 'NONE',  ( -132.2352756077770835, 50.81350938245623183, 34.10723656463518694 ) ) ;
#49075 = AXIS2_PLACEMENT_3D ( 'NONE', #23304, #56336, #29264 ) ;
#49076 = CARTESIAN_POINT ( 'NONE',  ( 2.999999999999996003, 0.000000000000000000, -20.30000000000000071 ) ) ;
#49077 = DIRECTION ( 'NONE',  ( 1.000000000000000000, 0.000000000000000000, 0.000000000000000000 ) ) ;
#49078 = ADVANCED_FACE ( 'NONE', ( #43683 ), #48952, .F. ) ;
#49079 = DIRECTION ( 'NONE',  ( 1.000000000000000000, 0.000000000000000000, 0.000000000000000000 ) ) ;
#49080 = CARTESIAN_POINT ( 'NONE',  ( 80.72161230109726660, 17.48902961068030848, -21.12390682281932186 ) ) ;
#49081 = VECTOR ( 'NONE', #13407, 1000.000000000000114 ) ;
#49082 = CARTESIAN_POINT ( 'NONE',  ( 93.61951000632930686, 21.92572933971849025, -72.89543003249312392 ) ) ;
#49083 = CARTESIAN_POINT ( 'NONE',  ( -95.52163045714286227, 29.47808868198297105, 7.913069298181163447 ) ) ;
#49084 = LINE ( 'NONE', #33640, #31764 ) ;
#49085 = EDGE_LOOP ( 'NONE', ( #9421, #55300, #22965, #36019 ) ) ;
#49086 = VERTEX_POINT ( 'NONE', #33154 ) ;
#49087 = VECTOR ( 'NONE', #50447, 1000.000000000000000 ) ;
#49088 = CARTESIAN_POINT ( 'NONE',  ( 40.38414441725699788, 8.538832720399534892, 44.86554498887630160 ) ) ;
#49089 = CARTESIAN_POINT ( 'NONE',  ( 0.000000000000000000, 500.0000000000000000, -53.65523180892861177 ) ) ;
#49090 = FACE_OUTER_BOUND ( 'NONE', #40032, .T. ) ;
#49091 = CARTESIAN_POINT ( 'NONE',  ( 445.3372781065086201, 217.8591479523844612, 78.55029585798806124 ) ) ;
#49092 = AXIS2_PLACEMENT_3D ( 'NONE', #69050, #41988, #19494 ) ;
#49093 = DIRECTION ( 'NONE',  ( -1.000000000000000000, 0.000000000000000000, 0.000000000000000000 ) ) ;
#49094 = DIRECTION ( 'NONE',  ( -0.000000000000000000, 1.000000000000000000, -0.000000000000000000 ) ) ;
#49095 = CARTESIAN_POINT ( 'NONE',  ( 41.80372346091801461, 9.750024116765239057, -36.01055466632809754 ) ) ;
#49096 = CARTESIAN_POINT ( 'NONE',  ( 158.3595886390531859, 58.34525996025800509, -77.92900715080654095 ) ) ;
#49097 = VERTEX_POINT ( 'NONE', #49654 ) ;
#49098 = CARTESIAN_POINT ( 'NONE',  ( 169.9999999999999716, -6.319444444444440201, 4.000000000000000000 ) ) ;
#49099 = EDGE_LOOP ( 'NONE', ( #16544, #2161, #42116, #14323 ) ) ;
#49101 = AXIS2_PLACEMENT_3D ( 'NONE', #30086, #25849, #3685 ) ;
#49100 = CARTESIAN_POINT ( 'NONE',  ( -11.57931195747592668, 7.164335452024274353, -36.40669791821974854 ) ) ;
#49102 = FACE_OUTER_BOUND ( 'NONE', #12428, .T. ) ;
#49103 = CARTESIAN_POINT ( 'NONE',  ( -85.53818824935325438, 25.05912739833918934, -93.26644400273796975 ) ) ;
#49104 = CARTESIAN_POINT ( 'NONE',  ( 39.40195752203892710, -170.0000000000000000, -43.11981746542777927 ) ) ;
#49105 = CARTESIAN_POINT ( 'NONE',  ( 32.09610685027467269, 8.582590950734816815, 8.856186440854040498 ) ) ;
#49106 = DIRECTION ( 'NONE',  ( 0.000000000000000000, -1.000000000000000000, 0.000000000000000000 ) ) ;
#49107 = CARTESIAN_POINT ( 'NONE',  ( 115.8406869673190300, 32.68156040898470138, -92.10329871651862277 ) ) ;
#49108 = CARTESIAN_POINT ( 'NONE',  ( -17.90772993695113868, 72.84144224619130625, 170.0000000000000000 ) ) ;
#49109 = CARTESIAN_POINT ( 'NONE',  ( -41.21054144751222026, -41.29403858773821412, 27.58472315868181113 ) ) ;
#49110 = CARTESIAN_POINT ( 'NONE',  ( 313.9975424824652350, 172.0000000000000284, 536.6193948016162949 ) ) ;
#49111 = ORIENTED_EDGE ( 'NONE', *, *, #56193, .F. ) ;
#49112 = DIRECTION ( 'NONE',  ( 1.000000000000000000, -0.000000000000000000, -0.000000000000000000 ) ) ;
#49113 = LINE ( 'NONE', #952, #67918 ) ;
#49114 = CARTESIAN_POINT ( 'NONE',  ( -11.78188048797444942, 8.190559674012726887, 4.394732934608507335 ) ) ;
#49115 = ADVANCED_FACE ( 'NONE', ( #64115 ), #26761, .T. ) ;
#49116 = DIRECTION ( 'NONE',  ( 1.000000000000000000, 0.000000000000000000, 0.000000000000000000 ) ) ;
#49118 = EDGE_CURVE ( 'NONE', #65787, #1572, #58828, .T. ) ;
#49117 = CARTESIAN_POINT ( 'NONE',  ( 41.66904755831208007, -10.55634918610412853, 2.000000000000001776 ) ) ;
#49119 = CARTESIAN_POINT ( 'NONE',  ( -102.7502407665687372, 33.01985383847077316, -61.85912785543960268 ) ) ;
#49120 = CARTESIAN_POINT ( 'NONE',  ( 89.81441025544566514, 21.60030303444519717, 84.07925712847533362 ) ) ;
#49121 = ADVANCED_FACE ( 'NONE', ( #28567 ), #50712, .F. ) ;
#49122 = EDGE_LOOP ( 'NONE', ( #15759, #49930 ) ) ;
#49123 = B_SPLINE_CURVE_WITH_KNOTS ( 'NONE', 3,
 ( #36699, #57117, #57799, #52175, #3995, #8930, #63774, #58146, #15586, #30377, #57455, #9963, #68689, #58473, #41621, #4344, #68364, #9267, #46195, #19470, #62740, #25802, #47231, #67675, #40929, #41966, #52846, #9619, #63427, #26135, #37035, #15234, #51828, #10286, #31416, #3638, #41281, #4668, #46545, #25113, #31752, #47569, #68022, #14544, #69025, #25463 ),
 .UNSPECIFIED., .F., .F.,
 ( 4, 2, 2, 2, 2, 2, 2, 2, 2, 2, 2, 2, 2, 2, 2, 2, 2, 2, 2, 2, 2, 2, 4 ),
 ( 0.02404638330965503529, 0.02555608299537562300, 0.02631093283823591686, 0.02706578268109621072, 0.02857548236681676027, 0.02933033220967704024, 0.03008518205253731675, 0.03159488173825786977, 0.03310458142397841586, 0.03385943126683869236, 0.03461428110969896887, 0.03612398079541951496, 0.03687883063827979147, 0.03763368048114007491, 0.03838853032400035142, 0.03914338016686062793, 0.04065307985258120177, 0.04216277953830176173, 0.04367247922402233556, 0.04518217890974290246, 0.04593702875260316509, 0.04669187859546342773, 0.04820157828118395993 ),
 .UNSPECIFIED. ) ;
#49124 = DIRECTION ( 'NONE',  ( -0.9998063756620102493, -0.01967768242440563753, 8.369256426322581013E-15 ) ) ;
#49125 = DIRECTION ( 'NONE',  ( -1.850169831522831466E-16, 1.000000000000000000, 1.110223024625156294E-16 ) ) ;
#49126 = CARTESIAN_POINT ( 'NONE',  ( -133.3392045760936639, 51.59583146030204404, 10.22114052722352362 ) ) ;
#49127 = CARTESIAN_POINT ( 'NONE',  ( -165.7149569557576001, 80.68479365246973600, -40.99114865466042090 ) ) ;
#49128 = CARTESIAN_POINT ( 'NONE',  ( -179.5391134141993348, 94.56797110730775557, 88.11752450009484505 ) ) ;
#49129 = ORIENTED_EDGE ( 'NONE', *, *, #63614, .F. ) ;
#49130 = CARTESIAN_POINT ( 'NONE',  ( -122.3963566076408398, 44.23346594671849630, -49.06497968827187606 ) ) ;
#49131 = LINE ( 'NONE', #13859, #12793 ) ;
#49132 = CARTESIAN_POINT ( 'NONE',  ( 0.000000000000000000, 0.000000000000000000, -7.000000000000000000 ) ) ;
#49133 = CARTESIAN_POINT ( 'NONE',  ( -4.071369321747694947, 7.682719369516284758, -63.25129218461325564 ) ) ;
#49134 = AXIS2_PLACEMENT_3D ( 'NONE', #17290, #60556, #45420 ) ;
#49135 = EDGE_CURVE ( 'NONE', #6327, #56020, #34895, .T. ) ;
#49136 = DIRECTION ( 'NONE',  ( -0.000000000000000000, -0.000000000000000000, -1.000000000000000000 ) ) ;
#49137 = ORIENTED_EDGE ( 'NONE', *, *, #17137, .F. ) ;
#49138 = CARTESIAN_POINT ( 'NONE',  ( 0.7145311798163248573, -4.618802153517011178, 8.000000000000000000 ) ) ;
#49139 = CARTESIAN_POINT ( 'NONE',  ( 200.4600337307565781, 100.7087439352121123, -37.62052402236275128 ) ) ;
#49140 = VECTOR ( 'NONE', #35404, 999.9999999999998863 ) ;
#49141 = EDGE_CURVE ( 'NONE', #12593, #54974, #13771, .T. ) ;
#49142 = CARTESIAN_POINT ( 'NONE',  ( -94.77890319529976182, 30.24118571794803856, 37.51899750598869332 ) ) ;
#49143 = LINE ( 'NONE', #47855, #19083 ) ;
#49144 = VECTOR ( 'NONE', #51529, 999.9999999999998863 ) ;
#49146 = VERTEX_POINT ( 'NONE', #56003 ) ;
#49145 = DIRECTION ( 'NONE',  ( 0.000000000000000000, -0.000000000000000000, -1.000000000000000000 ) ) ;
#49147 = CARTESIAN_POINT ( 'NONE',  ( 175.0634607207819045, 74.11351956991632051, 68.13290361812578055 ) ) ;
#49148 = ORIENTED_EDGE ( 'NONE', *, *, #2073, .F. ) ;
#49149 = ORIENTED_EDGE ( 'NONE', *, *, #4379, .T. ) ;
#49150 = VECTOR ( 'NONE', #19784, 1000.000000000000000 ) ;
#49151 = CARTESIAN_POINT ( 'NONE',  ( 61.28323125814129213, -21.66484633135379667, 40.00000000000003553 ) ) ;
#49152 = DIRECTION ( 'NONE',  ( -0.000000000000000000, -0.000000000000000000, -1.000000000000000000 ) ) ;
#49154 = ORIENTED_EDGE ( 'NONE', *, *, #32879, .F. ) ;
#49153 = DIRECTION ( 'NONE',  ( 0.5111246509603012411, 0.000000000000000000, 0.8595065975201762187 ) ) ;
#49155 = CARTESIAN_POINT ( 'NONE',  ( 164.6406716478537930, 63.44801348349338355, 34.69351737438754668 ) ) ;
#49156 = CARTESIAN_POINT ( 'NONE',  ( -75.31295361348104223, 0.000000000000000000, -2.499999999999970246 ) ) ;
#49157 = CARTESIAN_POINT ( 'NONE',  ( -77.02112161466365592, 22.77583432622785153, -35.29432619449520558 ) ) ;
#49158 = VERTEX_POINT ( 'NONE', #3231 ) ;
#49159 = DIRECTION ( 'NONE',  ( -0.000000000000000000, 1.000000000000000000, -0.000000000000000000 ) ) ;
#49160 = CARTESIAN_POINT ( 'NONE',  ( -37.79601571721867259, 10.72155118426296383, -11.98514248803286897 ) ) ;
#49161 = CARTESIAN_POINT ( 'NONE',  ( 151.2875339161446107, 52.99901520459633986, -93.04759937140129011 ) ) ;
#49162 = CARTESIAN_POINT ( 'NONE',  ( -37.07602570886410831, 10.58457435034603122, -74.63365721006658760 ) ) ;
#49163 = CARTESIAN_POINT ( 'NONE',  ( 22.89270809252619898, 7.840160460323052583, 66.77530781516593095 ) ) ;
#49164 = VERTEX_POINT ( 'NONE', #17670 ) ;
#49165 = ORIENTED_EDGE ( 'NONE', *, *, #52039, .T. ) ;
#49166 = ORIENTED_EDGE ( 'NONE', *, *, #56528, .F. ) ;
#49167 = DIRECTION ( 'NONE',  ( 0.000000000000000000, 0.000000000000000000, -1.000000000000000000 ) ) ;
#49168 = DIRECTION ( 'NONE',  ( -0.000000000000000000, 1.000000000000000000, -0.000000000000000000 ) ) ;
#49169 = CARTESIAN_POINT ( 'NONE',  ( -4.180838820195678096, -65.23214221112786504, 43.58025477438756212 ) ) ;
#49170 = DIRECTION ( 'NONE',  ( -0.8496664383351307803, 0.000000000000000000, 0.5273205320930463014 ) ) ;
#49171 = DIRECTION ( 'NONE',  ( 0.000000000000000000, 0.000000000000000000, 1.000000000000000000 ) ) ;
#49172 = DIRECTION ( 'NONE',  ( -0.9510565162951499785, -0.3090169943749582204, 0.000000000000000000 ) ) ;
#49173 = CARTESIAN_POINT ( 'NONE',  ( -126.3508039230932809, 46.79479538767116509, 72.46449846362081360 ) ) ;
#49174 = CARTESIAN_POINT ( 'NONE',  ( -61.26024128027892601, 17.48385755755500170, 87.28489753407048113 ) ) ;
#49175 = ADVANCED_BREP_SHAPE_REPRESENTATION ( '', ( #40824, #66832 ), #3998 ) ;
#49176 = CARTESIAN_POINT ( 'NONE',  ( 82.13067365723600233, 17.93447087949266816, 58.03607088492858423 ) ) ;
#49177 = VERTEX_POINT ( 'NONE', #18016 ) ;
#49178 = AXIS2_PLACEMENT_3D ( 'NONE', #58391, #27772, #64717 ) ;
#49179 = DIRECTION ( 'NONE',  ( -0.000000000000000000, -0.000000000000000000, -1.000000000000000000 ) ) ;
#49180 = ORIENTED_EDGE ( 'NONE', *, *, #23983, .T. ) ;
#49181 = CARTESIAN_POINT ( 'NONE',  ( 69.77839676787897361, -27.52340539439948586, 170.0000000000000000 ) ) ;
#49182 = ORIENTED_EDGE ( 'NONE', *, *, #26354, .F. ) ;
#49183 = CARTESIAN_POINT ( 'NONE',  ( 188.5837490358995865, 86.53279111916963018, 36.49783236869197367 ) ) ;
#49184 = B_SPLINE_CURVE_WITH_KNOTS ( 'NONE', 3,
 ( #13715, #3172, #8799, #8447, #56276, #30248, #13041, #24633, #40790, #8091, #51699, #3507, #67888, #19681, #66857, #67206, #50315, #14416, #18996, #35869, #57322, #28866, #2133, #23585, #45025, #18299, #39758, #50652, #2474, #23928, #18652, #40108, #61563, #13380, #34841, #4883 ),
 .UNSPECIFIED., .F., .F.,
 ( 4, 2, 2, 2, 2, 2, 2, 2, 2, 2, 2, 2, 2, 2, 2, 2, 2, 4 ),
 ( 0.000000000000000000, 0.001548367318450147691, 0.003096734636900295382, 0.004645101955350443290, 0.006193469273800590764, 0.007741836592250738239, 0.008516020251475821951, 0.009290203910700905662, 0.01083857122915107309, 0.01238693854760123877, 0.01393530586605140620, 0.01548367318450157362, 0.01703204050295174105, 0.01858040782140191194, 0.02012877513985207936, 0.02167714245830224679, 0.02322550977675241074, 0.02477387709520257816 ),
 .UNSPECIFIED. ) ;
#49185 = DIRECTION ( 'NONE',  ( -1.000000000000000000, 0.000000000000000000, -0.000000000000000000 ) ) ;
#49186 = VECTOR ( 'NONE', #64726, 1000.000000000000227 ) ;
#49187 = LINE ( 'NONE', #22476, #44809 ) ;
#49188 = DIRECTION ( 'NONE',  ( 0.000000000000000000, 0.000000000000000000, -1.000000000000000000 ) ) ;
#49189 = CARTESIAN_POINT ( 'NONE',  ( -50.52927270563903761, 13.51486287463704805, 4.970287360925811804 ) ) ;
#49190 = DIRECTION ( 'NONE',  ( 2.497525279955783991E-16, 1.121639896553914790E-17, 1.000000000000000000 ) ) ;
#49191 = EDGE_CURVE ( 'NONE', #53526, #33759, #8151, .T. ) ;
#49192 = VECTOR ( 'NONE', #12332, 1000.000000000000000 ) ;
#49193 = CARTESIAN_POINT ( 'NONE',  ( 160.9099843287284273, 61.67000084894965539, -77.14934695686636701 ) ) ;
#49194 = ORIENTED_EDGE ( 'NONE', *, *, #27949, .F. ) ;
#49195 = CARTESIAN_POINT ( 'NONE',  ( 0.000000000000000000, 0.000000000000000000, 170.0010000000000048 ) ) ;
#49196 = LINE ( 'NONE', #36080, #11669 ) ;
#49197 = VERTEX_POINT ( 'NONE', #61620 ) ;
#49198 = CARTESIAN_POINT ( 'NONE',  ( -15.76129977463437015, -63.43731725181460490, 43.58025477438756212 ) ) ;
#49199 = DIRECTION ( 'NONE',  ( 0.000000000000000000, 0.000000000000000000, -1.000000000000000000 ) ) ;
#49200 = ORIENTED_EDGE ( 'NONE', *, *, #64471, .T. ) ;
#49201 = CARTESIAN_POINT ( 'NONE',  ( -27.00000000000000355, -27.00000000000000355, 12.00000000000000000 ) ) ;
#49203 = EDGE_CURVE ( 'NONE', #10266, #62075, #4223, .T. ) ;
#49202 = CARTESIAN_POINT ( 'NONE',  ( -24.95029760921699591, 9.631514785009940738, -73.43094535933371958 ) ) ;
#49204 = CARTESIAN_POINT ( 'NONE',  ( 43.14669449386823175, 9.942681284149132992, 43.93040857229122764 ) ) ;
#49205 = CARTESIAN_POINT ( 'NONE',  ( -25.35398647985413234, 8.671412257862233020, 60.16984811174116032 ) ) ;
#49206 = CIRCLE ( 'NONE', #33526, 125.0000000000000000 ) ;
#49207 = CARTESIAN_POINT ( 'NONE',  ( -190.6985136298601731, 109.1272424661242582, 94.99999999999866418 ) ) ;
#49208 = EDGE_CURVE ( 'NONE', #43624, #7362, #61951, .T. ) ;
#49209 = EDGE_LOOP ( 'NONE', ( #62616, #58086, #32298, #52785 ) ) ;
#49210 = EDGE_CURVE ( 'NONE', #11106, #47843, #67265, .T. ) ;
#49211 = ORIENTED_EDGE ( 'NONE', *, *, #52096, .T. ) ;
#49212 = DIRECTION ( 'NONE',  ( -0.000000000000000000, 1.000000000000000000, -0.000000000000000000 ) ) ;
#49213 = VERTEX_POINT ( 'NONE', #55288 ) ;
#49214 = CARTESIAN_POINT ( 'NONE',  ( 36.99999522780156980, 9.122638774496639513, -23.38445250925136065 ) ) ;
#49215 = CARTESIAN_POINT ( 'NONE',  ( 21.38432669262978436, 61.76910524360980759, 43.58025477438756212 ) ) ;
#49216 = CARTESIAN_POINT ( 'NONE',  ( 57.39083379741713742, 11.43779987330584724, 59.17179337101942593 ) ) ;
#49217 = CARTESIAN_POINT ( 'NONE',  ( 427.4999999999999432, -18.06806526123148160, 380.0000000000000000 ) ) ;
#49218 =( LENGTH_UNIT ( ) NAMED_UNIT ( * ) SI_UNIT ( .MILLI., .METRE. ) );
#49219 = CARTESIAN_POINT ( 'NONE',  ( 46.66904755831212981, 20.55634918610394379, 85.00100000000000477 ) ) ;
#49220 = VERTEX_POINT ( 'NONE', #28926 ) ;
#49221 = EDGE_CURVE ( 'NONE', #50826, #22538, #16554, .T. ) ;
#49222 = LINE ( 'NONE', #34119, #41394 ) ;
#49223 = ORIENTED_EDGE ( 'NONE', *, *, #66005, .T. ) ;
#49224 = ORIENTED_EDGE ( 'NONE', *, *, #56684, .F. ) ;
#49225 = DIRECTION ( 'NONE',  ( -0.000000000000000000, -0.000000000000000000, 1.000000000000000000 ) ) ;
#49226 = FACE_OUTER_BOUND ( 'NONE', #47512, .T. ) ;
#49227 = PLANE ( 'NONE',  #41998 ) ;
#49228 = CARTESIAN_POINT ( 'NONE',  ( 141.2366329129481244, 46.06278879703611295, -71.73044966183998383 ) ) ;
#49229 = LINE ( 'NONE', #7739, #50948 ) ;
#49230 = EDGE_LOOP ( 'NONE', ( #38843, #49848, #31332, #59572 ) ) ;
#49231 = CARTESIAN_POINT ( 'NONE',  ( 209.9999999999999716, 0.000000000000000000, 72.99999999999998579 ) ) ;
#49232 = VERTEX_POINT ( 'NONE', #33848 ) ;
#49234 = CARTESIAN_POINT ( 'NONE',  ( -72.20490592113145567, 19.96451062593609294, 41.75807547809249343 ) ) ;
#49233 = AXIS2_PLACEMENT_3D ( 'NONE', #36184, #3479, #68202 ) ;
#49235 = EDGE_LOOP ( 'NONE', ( #65883, #27518, #20187, #34455 ) ) ;
#49236 = DIRECTION ( 'NONE',  ( 0.000000000000000000, -1.000000000000000000, 0.000000000000000000 ) ) ;
#49237 = AXIS2_PLACEMENT_3D ( 'NONE', #17048, #16369, #37828 ) ;
#49238 = ORIENTED_EDGE ( 'NONE', *, *, #59796, .T. ) ;
#49239 = CARTESIAN_POINT ( 'NONE',  ( -145.5261806899006842, 60.87473129144525785, -75.51763515817562222 ) ) ;
#49240 = CARTESIAN_POINT ( 'NONE',  ( 92.19920907511537678, 21.39700525884450144, 5.321486460283676223 ) ) ;
#49241 = B_SPLINE_CURVE_WITH_KNOTS ( 'NONE', 3,
 ( #4562, #15123, #64334, #63992, #31309, #36584 ),
 .UNSPECIFIED., .F., .F.,
 ( 4, 2, 4 ),
 ( 1.095770181088979215E-06, 0.03239442681617710207, 0.06478775786217311206 ),
 .UNSPECIFIED. ) ;
#49242 = AXIS2_PLACEMENT_3D ( 'NONE', #42611, #8887, #51791 ) ;
#49243 = CARTESIAN_POINT ( 'NONE',  ( -737.6000277536880958, -694.2189502691659300, 10.00000000000000000 ) ) ;
#49244 = ORIENTED_EDGE ( 'NONE', *, *, #42856, .T. ) ;
#49245 = CARTESIAN_POINT ( 'NONE',  ( -13.32397999417976564, -63.99361958670536410, 3.125053320693569132E-16 ) ) ;
#49246 = CARTESIAN_POINT ( 'NONE',  ( -444.2280788262714282, 394.7493581867591388, 97.47888161141302987 ) ) ;
#49247 = CARTESIAN_POINT ( 'NONE',  ( 36.77024545412684375, 9.095083943590518416, 30.38650154362253630 ) ) ;
#49248 = CARTESIAN_POINT ( 'NONE',  ( -173.1211646369891355, 88.63826465341151106, -49.71195716475001092 ) ) ;
#49249 = CARTESIAN_POINT ( 'NONE',  ( -132.9409505933031710, 51.31241517713429090, -18.18881852736828364 ) ) ;
#49250 = CARTESIAN_POINT ( 'NONE',  ( 173.3767798452622912, 69.10053625052562154, -11.44951126442670386 ) ) ;
#49251 = DIRECTION ( 'NONE',  ( -0.000000000000000000, -0.000000000000000000, -1.000000000000000000 ) ) ;
#49252 = ORIENTED_EDGE ( 'NONE', *, *, #48734, .T. ) ;
#49253 = LINE ( 'NONE', #44698, #20803 ) ;
#49254 = CARTESIAN_POINT ( 'NONE',  ( 103.8102216002272939, -165.0710086335687379, 0.000000000000000000 ) ) ;
#49255 = ORIENTED_EDGE ( 'NONE', *, *, #63643, .T. ) ;
#49256 = B_SPLINE_CURVE_WITH_KNOTS ( 'NONE', 3,
 ( #65223, #48664, #32177, #44095, #505, #5437, #43746, #38485, #11745, #54656, #6483, #38850, #26890, #64525, #33578, #24058, #17741, #50089, #39535, #39198, #12112, #49719, #19112, #40567, #44817, #45498, #23009, #2259, #18085, #60987, #65943, #29672, #66983, #2950, #44461, #66296, #7179, #60639, #1548, #50438, #18425, #7539, #18775, #24409, #34624 ),
 .UNSPECIFIED., .F., .F.,
 ( 4, 2, 2, 2, 2, 2, 2, 2, 1, 2, 2, 2, 2, 2, 2, 2, 2, 2, 2, 2, 2, 2, 4 ),
 ( 0.000000000000000000, 0.001467747071934219147, 0.002201620607901326552, 0.002935494143868433957, 0.004403241215802653104, 0.005870988287736871383, 0.007338735359671084459, 0.008072608895638188828, 0.008806482431605295799, 0.009540355967572401036, 0.01027422950353950627, 0.01174197657547371675, 0.01247585011144082025, 0.01320972364740792375, 0.01467747071934213769, 0.01541134425530924119, 0.01614521779127634296, 0.01761296486321055343, 0.01908071193514476044, 0.01981458547111187088, 0.02054845900707897785, 0.02201620607901318832, 0.02348395315094740227 ),
 .UNSPECIFIED. ) ;
#49257 = FACE_BOUND ( 'NONE', #53287, .T. ) ;
#49258 = CARTESIAN_POINT ( 'NONE',  ( -2.866724795119718561, 6.618578306599220085, -64.11449573703076510 ) ) ;
#49259 = DIRECTION ( 'NONE',  ( 1.000000000000000000, 0.000000000000000000, 0.000000000000000000 ) ) ;
#49260 = CARTESIAN_POINT ( 'NONE',  ( -145.9181947914994737, 62.49417193455356312, -8.878911523042834375 ) ) ;
#49261 = CARTESIAN_POINT ( 'NONE',  ( -31.43908319763709969, 9.591432048623762086, -62.16174795566551836 ) ) ;
#49262 = EDGE_CURVE ( 'NONE', #51505, #24194, #30035, .T. ) ;
#49263 = DIRECTION ( 'NONE',  ( 0.000000000000000000, 0.000000000000000000, -1.000000000000000000 ) ) ;
#49264 = CARTESIAN_POINT ( 'NONE',  ( 133.8566784816069344, 41.42467568809808398, 2.665790248531674678 ) ) ;
#49265 = CARTESIAN_POINT ( 'NONE',  ( -152.5067928559255392, 66.76529500553621688, 4.487733889797546283 ) ) ;
#49266 = CARTESIAN_POINT ( 'NONE',  ( -124.9970785861867455, 47.10847819093959998, -76.70786858315703682 ) ) ;
#49267 = DIRECTION ( 'NONE',  ( 0.000000000000000000, -0.5000000000000009992, -0.8660254037844380415 ) ) ;
#49268 = CARTESIAN_POINT ( 'NONE',  ( 113.8568724296587646, 30.58972477291341008, 3.677294227703742813 ) ) ;
#49269 = CARTESIAN_POINT ( 'NONE',  ( 89.65730223173018487, 21.54473673261222899, -23.34280881699134369 ) ) ;
#49270 = EDGE_LOOP ( 'NONE', ( #63317, #26151 ) ) ;
#49271 = LINE ( 'NONE', #1105, #48639 ) ;
#49272 = VERTEX_POINT ( 'NONE', #7476 ) ;
#49273 = DIRECTION ( 'NONE',  ( 3.081487911019579554E-32, 1.000000000000000000, 3.469446951953612956E-17 ) ) ;
#49274 = CARTESIAN_POINT ( 'NONE',  ( 82.34401416830213805, 19.05992892018825202, -76.32612924313528424 ) ) ;
#49275 = CARTESIAN_POINT ( 'NONE',  ( 31.89651141207616192, -56.63578868294582946, 40.00000000000003553 ) ) ;
#49276 = CARTESIAN_POINT ( 'NONE',  ( -142.0227972901369071, 59.36121938936275200, 64.50888617194736696 ) ) ;
#49277 = CARTESIAN_POINT ( 'NONE',  ( 0.000000000000000000, 0.000000000000000000, -9.500000000000000000 ) ) ;
#49278 = CARTESIAN_POINT ( 'NONE',  ( -25.07901552294942960, 9.649193085547777216, -38.83467625327824635 ) ) ;
#49279 = DIRECTION ( 'NONE',  ( -0.000000000000000000, 1.000000000000000000, -0.000000000000000000 ) ) ;
#49280 = DIRECTION ( 'NONE',  ( -0.000000000000000000, -1.000000000000000000, -0.000000000000000000 ) ) ;
#49281 = CARTESIAN_POINT ( 'NONE',  ( -125.6703656163502529, 47.55170550253213690, -23.06915330777030704 ) ) ;
#49282 = ORIENTED_EDGE ( 'NONE', *, *, #64875, .F. ) ;
#49283 = ORIENTED_EDGE ( 'NONE', *, *, #46146, .T. ) ;
#49285 = EDGE_CURVE ( 'NONE', #25560, #65701, #36757, .T. ) ;
#49284 = CARTESIAN_POINT ( 'NONE',  ( 181.0840389613909736, 80.03940679743415387, 71.15314469597512925 ) ) ;
#49286 = DIRECTION ( 'NONE',  ( -0.000000000000000000, -0.000000000000000000, 1.000000000000000000 ) ) ;
#49287 = CARTESIAN_POINT ( 'NONE',  ( 39.40195752203892710, 8.409560354027387774, -89.30891864635511013 ) ) ;
#49288 = CARTESIAN_POINT ( 'NONE',  ( -166.3231866619664174, 81.31146386205591625, 68.34665920884295076 ) ) ;
#49289 = CARTESIAN_POINT ( 'NONE',  ( -166.0031475600388831, 80.98114714564765393, -12.98692819457663106 ) ) ;
#49290 = B_SPLINE_CURVE_WITH_KNOTS ( 'NONE', 3,
 ( #9174, #30982, #31657, #47827, #14788, #46802 ),
 .UNSPECIFIED., .F., .F.,
 ( 4, 2, 4 ),
 ( 0.008240550023493531037, 0.01057684187039406240, 0.01291313371729459203 ),
 .UNSPECIFIED. ) ;
#49291 = AXIS2_PLACEMENT_3D ( 'NONE', #45455, #67288, #2555 ) ;
#49292 = VECTOR ( 'NONE', #66933, 1000.000000000000114 ) ;
#49293 = ADVANCED_FACE ( 'NONE', ( #18358 ), #29600, .T. ) ;
#49294 = LINE ( 'NONE', #66217, #37529 ) ;
#49295 = EDGE_LOOP ( 'NONE', ( #47907, #120, #69169, #20101 ) ) ;
#49296 = VECTOR ( 'NONE', #33689, 1000.000000000000000 ) ;
#49297 = CARTESIAN_POINT ( 'NONE',  ( 105.4376736768159049, 27.81988511842609313, -49.18599103925714644 ) ) ;
#49298 = CARTESIAN_POINT ( 'NONE',  ( -15.27748264047829352, 7.491388194171919146, 65.44047530913044852 ) ) ;
#49299 = CARTESIAN_POINT ( 'NONE',  ( -84.54326985437107567, 24.64760594531648863, -11.08512233598886176 ) ) ;
#49300 = DIRECTION ( 'NONE',  ( -1.000000000000000000, 0.000000000000000000, 0.000000000000000000 ) ) ;
#49301 = CARTESIAN_POINT ( 'NONE',  ( 39.89571693415785347, 8.473773298340395499, -8.775266874964071206 ) ) ;
#49302 = CARTESIAN_POINT ( 'NONE',  ( 212.1983751099433846, 117.2326047784727194, -16.84004950763299391 ) ) ;
#49303 = FACE_BOUND ( 'NONE', #49918, .T. ) ;
#49304 = CARTESIAN_POINT ( 'NONE',  ( -62.49130718206700408, 16.80297926264071151, -43.70676811772677439 ) ) ;
#49305 = EDGE_CURVE ( 'NONE', #44841, #67632, #17676, .T. ) ;
#49306 = EDGE_LOOP ( 'NONE', ( #21447, #10578, #17951, #28663 ) ) ;
#49307 = LINE ( 'NONE', #65513, #60456 ) ;
#49308 = CARTESIAN_POINT ( 'NONE',  ( 91.49210130311620048, 22.20929244416437598, -37.60641575626819844 ) ) ;
#49309 = DIRECTION ( 'NONE',  ( 0.000000000000000000, 0.000000000000000000, -1.000000000000000000 ) ) ;
#49310 = CARTESIAN_POINT ( 'NONE',  ( -180.6158171975815776, 97.47361786002632300, 11.15276930330031036 ) ) ;
#49311 = CARTESIAN_POINT ( 'NONE',  ( 212.1669304543882220, 119.0398299474538675, 62.85156645179986157 ) ) ;
#49312 = EDGE_CURVE ( 'NONE', #33778, #22804, #65877, .T. ) ;
#49313 = ADVANCED_FACE ( 'NONE', ( #44752 ), #23988, .F. ) ;
#49314 = LINE ( 'NONE', #44036, #14236 ) ;
#49315 = EDGE_LOOP ( 'NONE', ( #31468, #17581, #62300, #13667 ) ) ;
#49316 = CARTESIAN_POINT ( 'NONE',  ( 55.90910788310616653, 11.13585330978404109, 12.91588078479143498 ) ) ;
#49317 = CARTESIAN_POINT ( 'NONE',  ( -58.96922974609609014, 15.76655591015168056, 58.26108731115323280 ) ) ;
#49318 = EDGE_LOOP ( 'NONE', ( #15524, #62754, #62072, #45835 ) ) ;
#49319 = EDGE_LOOP ( 'NONE', ( #27387, #45300, #15206, #22072 ) ) ;
#49320 = DIRECTION ( 'NONE',  ( -0.000000000000000000, -1.000000000000000000, 0.000000000000000000 ) ) ;
#49321 = CARTESIAN_POINT ( 'NONE',  ( 45.78444578631987127, 59.41672343742573759, 170.0000000000000000 ) ) ;
#49322 = CARTESIAN_POINT ( 'NONE',  ( 86.62931800182293784, 20.48449268398422163, -62.66611478937537782 ) ) ;
#49323 = APPLICATION_CONTEXT ( 'automotive_design' ) ;
#49324 = ORIENTED_EDGE ( 'NONE', *, *, #62827, .T. ) ;
#49325 = ORIENTED_EDGE ( 'NONE', *, *, #20546, .F. ) ;
#49326 = CARTESIAN_POINT ( 'NONE',  ( 38.42020198992003799, 8.283430712587438904, -23.72674118770138563 ) ) ;
#49327 = CARTESIAN_POINT ( 'NONE',  ( 163.5944442552009548, 63.88381951184481267, 41.24633810883595686 ) ) ;
#49328 = CARTESIAN_POINT ( 'NONE',  ( 105.4376736768159191, 27.81988511842610379, 4.503110141670216393 ) ) ;
#49329 = CARTESIAN_POINT ( 'NONE',  ( 63.01563776193091826, 13.70579113808095073, 2.968410348757589468 ) ) ;
#49330 = CARTESIAN_POINT ( 'NONE',  ( 87.11228333101212229, 19.58587579906928156, 44.71208757247933363 ) ) ;
#49331 = CARTESIAN_POINT ( 'NONE',  ( 102.7938674513918471, 26.67851209377773003, -15.56664358664439085 ) ) ;
#49332 = CARTESIAN_POINT ( 'NONE',  ( -47.55316895016326839, 13.83165595246916979, 11.47544540822512360 ) ) ;
#49333 = CARTESIAN_POINT ( 'NONE',  ( 65.35403040894466642, -1.250000000000021982, 6.377659838150137469E-18 ) ) ;
#49334 = CARTESIAN_POINT ( 'NONE',  ( -153.9466444020484062, 69.38783913630635425, -89.95288446847763453 ) ) ;
#49335 = CARTESIAN_POINT ( 'NONE',  ( 0.1230226671131348926, -25.12215469714591976, 3.061616997868437868E-16 ) ) ;
#49336 = AXIS2_PLACEMENT_3D ( 'NONE', #20521, #31102, #25824 ) ;
#49337 = CARTESIAN_POINT ( 'NONE',  ( 93.72383014846688809, 21.96492462047006100, 88.44459928000046034 ) ) ;
#49339 = ORIENTED_EDGE ( 'NONE', *, *, #1852, .F. ) ;
#49338 = DIRECTION ( 'NONE',  ( 0.000000000000000000, 0.000000000000000000, 1.000000000000000000 ) ) ;
#49340 = ORIENTED_EDGE ( 'NONE', *, *, #14536, .F. ) ;
#49341 = EDGE_LOOP ( 'NONE', ( #34273, #4013, #37126, #35330, #67844, #45669 ) ) ;
#49342 = CARTESIAN_POINT ( 'NONE',  ( -15.08468253268399906, 7.472949889606721463, -18.02137581700551294 ) ) ;
#49343 = CARTESIAN_POINT ( 'NONE',  ( -165.7250372467519810, 80.69514495077957861, 93.26859561057739256 ) ) ;
#49344 = CARTESIAN_POINT ( 'NONE',  ( -54.09522495088364735, 14.42642983673692392, -23.32612737743259146 ) ) ;
#49345 = ADVANCED_FACE ( 'NONE', ( #66227 ), #51376, .T. ) ;
#49346 = DIRECTION ( 'NONE',  ( -1.000000000000000000, 0.000000000000000000, 0.000000000000000000 ) ) ;
#49347 = CARTESIAN_POINT ( 'NONE',  ( -36.00304714721387001, 11.40794940913595923, 70.53273267370495603 ) ) ;
#49348 = CARTESIAN_POINT ( 'NONE',  ( 37.34307084251124564, 44.82188538352577467, 27.58472315868181113 ) ) ;
#49349 = CARTESIAN_POINT ( 'NONE',  ( -76.10397364431024414, 21.36211154336729834, -76.51270562591143687 ) ) ;
#49350 = CARTESIAN_POINT ( 'NONE',  ( 8.820885042877430138, 74.43053605947413587, 41.38025477438755928 ) ) ;
#49352 = VERTEX_POINT ( 'NONE', #57728 ) ;
#49351 = EDGE_CURVE ( 'NONE', #58864, #67205, #60573, .T. ) ;
#49353 = CARTESIAN_POINT ( 'NONE',  ( -417.6627218934913230, 179.4906275429376308, 111.5502958579881749 ) ) ;
#49354 = ORIENTED_EDGE ( 'NONE', *, *, #47095, .T. ) ;
#49355 = ORIENTED_EDGE ( 'NONE', *, *, #69516, .F. ) ;
#49356 = CARTESIAN_POINT ( 'NONE',  ( -148.6426892915312692, 64.76241938621078020, 18.87627064943540489 ) ) ;
#49357 = CARTESIAN_POINT ( 'NONE',  ( -56.74702624633194858, 16.18586554270559219, -89.08696668261721641 ) ) ;
#49358 = CARTESIAN_POINT ( 'NONE',  ( -27.47737346315476259, 9.991540138299660256, 85.02917570802463842 ) ) ;
#49359 = VECTOR ( 'NONE', #15017, 1000.000000000000000 ) ;
#49360 = CARTESIAN_POINT ( 'NONE',  ( -96.02415295709707266, 29.71480036090586196, -46.65887338834314590 ) ) ;
#49361 = DIRECTION ( 'NONE',  ( -1.000000000000000000, -6.405132834375901070E-16, -5.170250902511168442E-32 ) ) ;
#49362 = DIRECTION ( 'NONE',  ( 1.000000000000000000, 0.000000000000000000, 0.000000000000000000 ) ) ;
#49363 = CARTESIAN_POINT ( 'NONE',  ( 0.000000000000000000, 0.000000000000000000, 0.000000000000000000 ) ) ;
#49364 = ORIENTED_EDGE ( 'NONE', *, *, #62986, .F. ) ;
#49365 = EDGE_CURVE ( 'NONE', #69128, #68503, #4264, .T. ) ;
#49366 = ORIENTED_EDGE ( 'NONE', *, *, #36875, .F. ) ;
#49367 = EDGE_LOOP ( 'NONE', ( #37295, #31312, #21244, #14392 ) ) ;
#49368 = EDGE_CURVE ( 'NONE', #30571, #47754, #9190, .T. ) ;
#49369 = DIRECTION ( 'NONE',  ( 0.000000000000000000, -0.7071067811865474617, -0.7071067811865474617 ) ) ;
#49370 = PLANE ( 'NONE',  #19549 ) ;
#49371 = DIRECTION ( 'NONE',  ( 0.000000000000000000, 0.000000000000000000, 1.000000000000000000 ) ) ;
#49372 = CARTESIAN_POINT ( 'NONE',  ( 59.72526569420001863, 11.93313563009888689, -9.618805749340053168 ) ) ;
#49373 = EDGE_CURVE ( 'NONE', #68802, #58622, #52100, .T. ) ;
#49374 = UNCERTAINTY_MEASURE_WITH_UNIT (LENGTH_MEASURE( 1.000000000000000082E-05 ), #10284, 'distance_accuracy_value', 'NONE');
#49375 = EDGE_CURVE ( 'NONE', #26839, #6967, #9540, .T. ) ;
#49376 = CARTESIAN_POINT ( 'NONE',  ( -48.33725449172840172, 12.98311179783358682, 34.44141564906372110 ) ) ;
#49377 = VECTOR ( 'NONE', #32933, 1000.000000000000000 ) ;
#49378 = CARTESIAN_POINT ( 'NONE',  ( 197.1979149960398274, 98.19687999752004259, 63.21691722051551920 ) ) ;
#49379 = EDGE_LOOP ( 'NONE', ( #65838, #43730, #62862, #12619 ) ) ;
#49380 = CARTESIAN_POINT ( 'NONE',  ( 186.6075385349484463, 85.85749512876287781, 58.55496012458434762 ) ) ;
#49381 = CARTESIAN_POINT ( 'NONE',  ( -156.6819053601225846, 70.51177710383656461, 67.32408636767608812 ) ) ;
#49382 = CARTESIAN_POINT ( 'NONE',  ( -0.5783162822156596716, 7.534184941292926929, -40.97127712057928051 ) ) ;
#49383 = DIRECTION ( 'NONE',  ( 1.000000000000000000, 0.000000000000000000, -0.000000000000000000 ) ) ;
#49384 = CARTESIAN_POINT ( 'NONE',  ( -165.7138623879809529, 79.24467249981147177, 12.69207250051168856 ) ) ;
#49385 = PLANE ( 'NONE',  #37420 ) ;
#49386 = FACE_BOUND ( 'NONE', #49122, .T. ) ;
#49387 = DIRECTION ( 'NONE',  ( -0.000000000000000000, -0.000000000000000000, -1.000000000000000000 ) ) ;
#49388 = CARTESIAN_POINT ( 'NONE',  ( 9.057575839850585453, 6.378493414438676901, -66.54567355087297642 ) ) ;
#49389 = VECTOR ( 'NONE', #53658, 1000.000000000000000 ) ;
#49390 = B_SPLINE_CURVE_WITH_KNOTS ( 'NONE', 3,
 ( #6859, #22689, #38516, #12145, #11422, #49053, #59963, #43780, #66327, #32893, #33606, #890, #55036, #12489, #11780, #33256, #54691, #33951, #34302, #54331, #55747, #28669, #6515, #28309, #27962, #49407, #39570, #1236, #23046, #44493, #65975, #55384, #1951, #23406, #18116, #61021, #57478, #68044, #35333, #61708, #67697, #25481, #13867, #46567 ),
 .UNSPECIFIED., .F., .F.,
 ( 4, 2, 2, 2, 2, 2, 2, 2, 2, 2, 2, 2, 2, 2, 2, 2, 2, 2, 2, 2, 2, 4 ),
 ( 0.000000000000000000, 0.003518733725596278391, 0.004398417156995355903, 0.005278100588394431247, 0.007037467451192647855, 0.007917150882591742281, 0.008796834313990836707, 0.01055620117678906893, 0.01231556803958730288, 0.01319525147098641986, 0.01407493490238553684, 0.01495461833378465208, 0.01583430176518376906, 0.01671398519658288603, 0.01759366862798200301, 0.01935303549078017105, 0.02111240235357833214, 0.02199208578497738667, 0.02287176921637643426, 0.02463113607917451903, 0.02639050294197260033, 0.02814986980477068509 ),
 .UNSPECIFIED. ) ;
#49391 = ORIENTED_EDGE ( 'NONE', *, *, #26883, .T. ) ;
#49392 = DIRECTION ( 'NONE',  ( 0.000000000000000000, 0.000000000000000000, -1.000000000000000000 ) ) ;
#49393 = DIRECTION ( 'NONE',  ( 1.000000000000000000, 0.000000000000000000, 0.000000000000000000 ) ) ;
#49394 = CARTESIAN_POINT ( 'NONE',  ( -126.7989199172159545, 47.09198523267864545, -49.87294221663437099 ) ) ;
#49395 = EDGE_CURVE ( 'NONE', #57138, #26798, #33400, .T. ) ;
#49396 = PLANE ( 'NONE',  #43571 ) ;
#49397 = EDGE_CURVE ( 'NONE', #27768, #64974, #40991, .T. ) ;
#49398 = CARTESIAN_POINT ( 'NONE',  ( -3.000000000000002665, 0.000000000000000000, 0.000000000000000000 ) ) ;
#49399 = EDGE_CURVE ( 'NONE', #15169, #5346, #63700, .T. ) ;
#49400 = ORIENTED_EDGE ( 'NONE', *, *, #30439, .F. ) ;
#49401 = ORIENTED_EDGE ( 'NONE', *, *, #16102, .T. ) ;
#49402 = EDGE_CURVE ( 'NONE', #60863, #26321, #10213, .T. ) ;
#49403 = CARTESIAN_POINT ( 'NONE',  ( -129.8649418364887538, 49.16412313266191347, -89.72624065702046892 ) ) ;
#49404 = CARTESIAN_POINT ( 'NONE',  ( 187.4809559129425338, 85.32157829635528401, 94.42977490495529480 ) ) ;
#49405 = ORIENTED_EDGE ( 'NONE', *, *, #20253, .F. ) ;
#49406 = ORIENTED_EDGE ( 'NONE', *, *, #52357, .F. ) ;
#49407 = CARTESIAN_POINT ( 'NONE',  ( 173.8575673535406168, 71.59843387604337295, -45.75285605104306086 ) ) ;
#49408 = B_SPLINE_CURVE_WITH_KNOTS ( 'NONE', 3,
 ( #39882, #33923, #56067, #23381, #55006, #44820, #55718, #29330, #60297, #18088, #61343, #55360, #65584, #39540, #60994, #50781, #49376, #7542, #49724, #2602, #65948, #1553, #1206, #17745, #39201, #65552, #11720, #1176, #59551, #39173, #480, #48636, #17346, #123, #27907, #48993, #64502, #21579, #11368, #43380, #33193, #21928, #54266 ),
 .UNSPECIFIED., .F., .F.,
 ( 4, 2, 2, 2, 2, 2, 2, 2, 2, 2, 2, 2, 1, 2, 2, 2, 2, 2, 2, 2, 2, 4 ),
 ( 0.02390068823634510300, 0.02538837671117075492, 0.02613222094858358088, 0.02687606518599640684, 0.02836375366082204141, 0.02985144213564767945, 0.03059528637306050194, 0.03133913061047332443, 0.03282681908529898329, 0.03431450756012464909, 0.03580219603495030795, 0.03654604027236314084, 0.03728988450977597374, 0.03803372874718879970, 0.03877757298460163260, 0.04026526145942728452, 0.04175294993425293644, 0.04324063840907858836, 0.04398448264649141431, 0.04472832688390424027, 0.04621601535872986444, 0.04770370383355548860 ),
 .UNSPECIFIED. ) ;
#49409 = CARTESIAN_POINT ( 'NONE',  ( 110.2429982417149432, 28.88204397445229432, 17.76666361527367499 ) ) ;
#49410 = ORIENTED_EDGE ( 'NONE', *, *, #28764, .F. ) ;
#49411 = LINE ( 'NONE', #50127, #24467 ) ;
#49412 = CARTESIAN_POINT ( 'NONE',  ( 444.9999999999999432, 225.0000000000000000, 2.000000000000000000 ) ) ;
#49413 = CARTESIAN_POINT ( 'NONE',  ( -71.96390573417176029, 19.88067451234327621, -39.21214165021154940 ) ) ;
#49414 = VECTOR ( 'NONE', #20129, 1000.000000000000000 ) ;
#49415 = DIRECTION ( 'NONE',  ( -0.000000000000000000, -0.000000000000000000, -1.000000000000000000 ) ) ;
#49416 = CARTESIAN_POINT ( 'NONE',  ( -29.74902699556085039, 10.33856194202125778, -8.661514771972045779 ) ) ;
#49417 = CARTESIAN_POINT ( 'NONE',  ( -48.23766733091049730, 13.99378332280058679, -12.73082205257937360 ) ) ;
#49418 = ORIENTED_EDGE ( 'NONE', *, *, #55857, .F. ) ;
#49419 = CARTESIAN_POINT ( 'NONE',  ( 114.6632852039170984, 30.98120524556721023, -49.48624585975684198 ) ) ;
#49420 = FACE_BOUND ( 'NONE', #30242, .T. ) ;
#49421 = CARTESIAN_POINT ( 'NONE',  ( -142.0070007485041401, 59.34878529741516928, -42.58233384625039974 ) ) ;
#49422 = DIRECTION ( 'NONE',  ( -0.5407162030609373726, -0.6444004775717707689, -0.5407162030609372616 ) ) ;
#49424 = EDGE_LOOP ( 'NONE', ( #14919, #49495, #15795, #39008, #61462, #59018 ) ) ;
#49423 = CARTESIAN_POINT ( 'NONE',  ( -122.1008507185714080, 44.04671359203690884, 85.33186843359860063 ) ) ;
#49425 = DIRECTION ( 'NONE',  ( -0.000000000000000000, 1.000000000000000000, -0.000000000000000000 ) ) ;
#49426 = VECTOR ( 'NONE', #56476, 1000.000000000000000 ) ;
#49427 = ORIENTED_EDGE ( 'NONE', *, *, #52408, .T. ) ;
#49428 = CYLINDRICAL_SURFACE ( 'NONE', #59292, 7.500000000000013323 ) ;
#49429 = DIRECTION ( 'NONE',  ( -1.000000000000000000, 0.000000000000000000, 0.000000000000000000 ) ) ;
#49430 = CARTESIAN_POINT ( 'NONE',  ( 4.165045035621076863, -64.88046627338039229, 170.0000000000000000 ) ) ;
#49431 = PLANE ( 'NONE',  #15885 ) ;
#49432 = CARTESIAN_POINT ( 'NONE',  ( 84.74140601443112075, 18.78541996275572856, -9.214546398377361669 ) ) ;
#49433 = CARTESIAN_POINT ( 'NONE',  ( 41.80869235728136601, 9.750404582811603049, 3.449047885945065062 ) ) ;
#49434 = CARTESIAN_POINT ( 'NONE',  ( 86.62931800182293784, 19.42108912189596381, -77.66611478937542756 ) ) ;
#49435 = EDGE_CURVE ( 'NONE', #61415, #47218, #67596, .T. ) ;
#49436 = DIRECTION ( 'NONE',  ( 0.000000000000000000, 0.000000000000000000, 1.000000000000000000 ) ) ;
#49437 = CARTESIAN_POINT ( 'NONE',  ( 4.250000000000000000, 0.000000000000000000, -0.5251556536572842271 ) ) ;
#49438 = ORIENTED_EDGE ( 'NONE', *, *, #34823, .T. ) ;
#49439 = ORIENTED_EDGE ( 'NONE', *, *, #60611, .F. ) ;
#49440 = CARTESIAN_POINT ( 'NONE',  ( 45.90128843543705983, 9.343910238294478532, 33.63887583473116649 ) ) ;
#49441 = LINE ( 'NONE', #58961, #63191 ) ;
#49442 = LINE ( 'NONE', #27298, #1999 ) ;
#49443 = DIRECTION ( 'NONE',  ( 1.000000000000000000, 0.000000000000000000, 0.000000000000000000 ) ) ;
#49444 = CARTESIAN_POINT ( 'NONE',  ( 207.8407634284391463, 112.5209879629464069, -37.00314380516740442 ) ) ;
#49445 = CARTESIAN_POINT ( 'NONE',  ( -76.32456871438913026, 22.51591205926309769, -76.60115264913015665 ) ) ;
#49446 = CARTESIAN_POINT ( 'NONE',  ( -105.4556185321791162, 34.42302275449793569, 71.67470424851612165 ) ) ;
#49447 = CARTESIAN_POINT ( 'NONE',  ( -31.43908319763709969, 9.591432048623767415, -50.31719736520186359 ) ) ;
#49448 = LINE ( 'NONE', #1281, #53129 ) ;
#49449 = ADVANCED_FACE ( 'NONE', ( #14121 ), #35584, .F. ) ;
#49450 = VERTEX_POINT ( 'NONE', #32721 ) ;
#49451 = CARTESIAN_POINT ( 'NONE',  ( -24.61094659556678010, 9.585225265507405723, 13.98425489515978271 ) ) ;
#49452 = ORIENTED_EDGE ( 'NONE', *, *, #62333, .T. ) ;
#49453 = CARTESIAN_POINT ( 'NONE',  ( -442.6627218934913799, 394.9999999999998295, -125.1412729879898791 ) ) ;
#49454 = ADVANCED_FACE ( 'NONE', ( #1060 ), #10906, .F. ) ;
#49455 = CARTESIAN_POINT ( 'NONE',  ( -8.000000000000000000, 3.871967595402135753, -9.001061386767540640 ) ) ;
#49456 = DIRECTION ( 'NONE',  ( 0.000000000000000000, -1.000000000000000000, 0.000000000000000000 ) ) ;
#49457 = CARTESIAN_POINT ( 'NONE',  ( -41.50537345350635121, -50.04124777106355282, 41.38025477438755928 ) ) ;
#49458 = EDGE_CURVE ( 'NONE', #17792, #65052, #37289, .T. ) ;
#49459 = CARTESIAN_POINT ( 'NONE',  ( -179.9997297618090784, 96.71425526203211120, 94.99999999999866418 ) ) ;
#49460 = AXIS2_PLACEMENT_3D ( 'NONE', #27652, #66366, #61061 ) ;
#49461 = CARTESIAN_POINT ( 'NONE',  ( 115.2641405259299745, 32.39624275045399315, -91.52542046738727777 ) ) ;
#49462 = DIRECTION ( 'NONE',  ( -1.850169831522831466E-16, 1.000000000000000000, 1.110223024625156294E-16 ) ) ;
#49463 = CARTESIAN_POINT ( 'NONE',  ( 205.4975936689702110, 107.4441653241353691, 82.92102392413544010 ) ) ;
#49464 = DIRECTION ( 'NONE',  ( 0.000000000000000000, 0.9952373409613455291, -0.09748146057682102739 ) ) ;
#49465 = EDGE_LOOP ( 'NONE', ( #24479, #18, #13108, #54156 ) ) ;
#49466 = CARTESIAN_POINT ( 'NONE',  ( 56.28782924480456984, 12.23883190161851608, 67.50924629393880139 ) ) ;
#49467 = CARTESIAN_POINT ( 'NONE',  ( 13.83281508467570831, 7.452090093180183672, -62.60602632425918301 ) ) ;
#49468 = CARTESIAN_POINT ( 'NONE',  ( -78.66644367742111399, -170.0000000000000000, 11.07365054920946079 ) ) ;
#49469 = CARTESIAN_POINT ( 'NONE',  ( 285.0000633975121218, -22.00001440852518897, 0.3259197091964841642 ) ) ;
#49470 = CARTESIAN_POINT ( 'NONE',  ( 29.67531360975017662, -24.26667169483791753, 13.32819299319724671 ) ) ;
#49471 = CARTESIAN_POINT ( 'NONE',  ( 89.21443742848369141, 21.38598633305952390, 83.83068150208889335 ) ) ;
#49472 = ORIENTED_EDGE ( 'NONE', *, *, #11256, .F. ) ;
#49473 = DIRECTION ( 'NONE',  ( 1.000000000000000000, 9.989315170677423714E-15, 9.989315170677463157E-15 ) ) ;
#49474 = VECTOR ( 'NONE', #17376, 1000.000000000000114 ) ;
#49475 = CARTESIAN_POINT ( 'NONE',  ( -12.50000000000000000, -17.50000000000000000, 0.000000000000000000 ) ) ;
#49476 = CARTESIAN_POINT ( 'NONE',  ( 34.43940527065382895, 66.63700071734666608, 170.0000000000000000 ) ) ;
#49477 = ADVANCED_FACE ( 'NONE', ( #37993 ), #32377, .T. ) ;
#49478 = CARTESIAN_POINT ( 'NONE',  ( -4.610955605663495938, 74.80943656680578613, 41.38025477438755928 ) ) ;
#49479 = CARTESIAN_POINT ( 'NONE',  ( -132.2286325684322321, 52.04087929935080581, -38.39048859397041724 ) ) ;
#49480 = ORIENTED_EDGE ( 'NONE', *, *, #58825, .F. ) ;
#49481 = CARTESIAN_POINT ( 'NONE',  ( -119.2682179969168175, 42.28333404791697347, -38.86063178010808628 ) ) ;
#49482 = FACE_OUTER_BOUND ( 'NONE', #57134, .T. ) ;
#49483 = ADVANCED_FACE ( 'NONE', ( #10561 ), #32030, .F. ) ;
#49484 = DIRECTION ( 'NONE',  ( 0.000000000000000000, 0.000000000000000000, -1.000000000000000000 ) ) ;
#49485 = CARTESIAN_POINT ( 'NONE',  ( -142.4136725729621560, 58.38849625135428312, 94.36932141740047086 ) ) ;
#49486 = FACE_OUTER_BOUND ( 'NONE', #9626, .T. ) ;
#49487 = VERTEX_POINT ( 'NONE', #60140 ) ;
#49488 = DIRECTION ( 'NONE',  ( -0.000000000000000000, -0.000000000000000000, -1.000000000000000000 ) ) ;
#49489 = CARTESIAN_POINT ( 'NONE',  ( 197.8436586345020203, 97.39326576892285914, -46.92396185645527140 ) ) ;
#49490 = CARTESIAN_POINT ( 'NONE',  ( 164.6046919270428930, 64.73376589608267295, -95.00000000000133582 ) ) ;
#49491 = CARTESIAN_POINT ( 'NONE',  ( 16.27765348919936983, 6.516472002017809295, -50.51894409868578606 ) ) ;
#49493 = ORIENTED_EDGE ( 'NONE', *, *, #44211, .T. ) ;
#49492 = DIRECTION ( 'NONE',  ( -0.04486483035050447404, -0.9989930665413151445, 0.000000000000000000 ) ) ;
#49494 = DIRECTION ( 'NONE',  ( -1.000000000000000000, 0.000000000000000000, 0.000000000000000000 ) ) ;
#49495 = ORIENTED_EDGE ( 'NONE', *, *, #68136, .T. ) ;
#49496 = ORIENTED_EDGE ( 'NONE', *, *, #27485, .T. ) ;
#49497 = CARTESIAN_POINT ( 'NONE',  ( -120.8703893864066146, 43.27420333016311815, -90.52915191075125279 ) ) ;
#49498 = DIRECTION ( 'NONE',  ( 0.000000000000000000, 0.000000000000000000, 1.000000000000000000 ) ) ;
#49500 = ORIENTED_EDGE ( 'NONE', *, *, #18750, .T. ) ;
#49499 = CARTESIAN_POINT ( 'NONE',  ( -8.320534640989464492, 7.931748412542455995, -62.26262132240751157 ) ) ;
#49501 = CARTESIAN_POINT ( 'NONE',  ( 157.9130201331580565, 57.99550255803046639, 29.40946747225336466 ) ) ;
#49502 = VECTOR ( 'NONE', #27923, 1000.000000000000227 ) ;
#49503 = DIRECTION ( 'NONE',  ( -0.000000000000000000, -0.000000000000000000, 1.000000000000000000 ) ) ;
#49504 = DIRECTION ( 'NONE',  ( 0.000000000000000000, 0.000000000000000000, 1.000000000000000000 ) ) ;
#49505 = PRODUCT_DEFINITION_SHAPE ( 'NONE', 'NONE',  #69616 ) ;
#49506 = ORIENTED_EDGE ( 'NONE', *, *, #21663, .F. ) ;
#49507 = CIRCLE ( 'NONE', #19198, 65.36598343705435354 ) ;
#49508 = CARTESIAN_POINT ( 'NONE',  ( 60.00000000000000000, 7.347880794884118356E-15, -10.00000000000000000 ) ) ;
#49509 = EDGE_CURVE ( 'NONE', #9149, #18081, #28992, .T. ) ;
#49510 = VECTOR ( 'NONE', #40604, 1000.000000000000000 ) ;
#49511 = CARTESIAN_POINT ( 'NONE',  ( -61.29635759142585982, -21.66977272663580578, 43.58025477438756923 ) ) ;
#49512 = ADVANCED_FACE ( 'NONE', ( #27083 ), #11956, .F. ) ;
#49513 = DIRECTION ( 'NONE',  ( -0.000000000000000000, -1.000000000000000000, -0.000000000000000000 ) ) ;
#49514 = CARTESIAN_POINT ( 'NONE',  ( -133.3799602664182657, 52.86209125874982107, 11.80555390119608994 ) ) ;
#49515 = CARTESIAN_POINT ( 'NONE',  ( 18.62350602913453557, 0.000000000000000000, 23.51946052065799364 ) ) ;
#49516 = VERTEX_POINT ( 'NONE', #33430 ) ;
#49517 = B_SPLINE_CURVE_WITH_KNOTS ( 'NONE', 3,
 ( #64635, #21369, #5538, #22067, #53366, #31584 ),
 .UNSPECIFIED., .F., .F.,
 ( 4, 2, 4 ),
 ( 0.008240550023493532772, 0.01057684187039406240, 0.01291313371729459550 ),
 .UNSPECIFIED. ) ;
#49518 = ORIENTED_EDGE ( 'NONE', *, *, #33914, .F. ) ;
#49519 = ORIENTED_EDGE ( 'NONE', *, *, #986, .T. ) ;
#49520 = DIRECTION ( 'NONE',  ( -0.000000000000000000, 1.000000000000000000, -0.000000000000000000 ) ) ;
#49521 = CARTESIAN_POINT ( 'NONE',  ( -190.6985136298601731, 109.1272424661242582, 7.126870892829554549 ) ) ;
#49522 = DIRECTION ( 'NONE',  ( 1.000000000000000000, -0.000000000000000000, 0.000000000000000000 ) ) ;
#49523 = CARTESIAN_POINT ( 'NONE',  ( 209.3223706822284100, 190.0000000000000000, 31.44247402469554942 ) ) ;
#49524 = DIRECTION ( 'NONE',  ( 0.000000000000000000, -0.000000000000000000, -1.000000000000000000 ) ) ;
#49525 = PLANE ( 'NONE',  #37046 ) ;
#49526 = CARTESIAN_POINT ( 'NONE',  ( -130.5740389938243027, 49.65308610043481252, 70.84463781538606497 ) ) ;
#49527 = CARTESIAN_POINT ( 'NONE',  ( -71.27103490383372275, 20.70545763375146109, -14.49721781705724233 ) ) ;
#49528 = EDGE_CURVE ( 'NONE', #66603, #36960, #27786, .T. ) ;
#49529 = CARTESIAN_POINT ( 'NONE',  ( 133.8566784816069628, 41.42467568809806977, 17.66579024853170310 ) ) ;
#49530 = ORIENTED_EDGE ( 'NONE', *, *, #72, .T. ) ;
#49531 = CARTESIAN_POINT ( 'NONE',  ( -173.1211646369891639, 87.12891641440852197, -88.40105834567665966 ) ) ;
#49532 = DIRECTION ( 'NONE',  ( 0.000000000000000000, 0.000000000000000000, 1.000000000000000000 ) ) ;
#49533 = ADVANCED_FACE ( 'NONE', ( #48518 ), #41279, .T. ) ;
#49534 = ORIENTED_EDGE ( 'NONE', *, *, #45979, .T. ) ;
#49535 = CARTESIAN_POINT ( 'NONE',  ( 188.2076037774874635, 86.11782719225436722, 34.44517487742668038 ) ) ;
#49536 = DIRECTION ( 'NONE',  ( 1.000000000000000000, 0.000000000000000000, 0.000000000000000000 ) ) ;
#49537 = ADVANCED_FACE ( 'NONE', ( #59780 ), #11591, .T. ) ;
#49538 = CARTESIAN_POINT ( 'NONE',  ( 10.73115448446713494, 22.57968829347503714, 0.000000000000000000 ) ) ;
#49539 = CARTESIAN_POINT ( 'NONE',  ( -122.3759299995709711, 45.41285412136513600, 58.32378120899723228 ) ) ;
#49540 = LINE ( 'NONE', #61162, #15424 ) ;
#49541 = CARTESIAN_POINT ( 'NONE',  ( 0.7145311798163210826, 4.618802153517001408, -8.000000000000000000 ) ) ;
#49542 = DIRECTION ( 'NONE',  ( -0.000000000000000000, -1.000000000000000000, -0.000000000000000000 ) ) ;
#49543 = EDGE_LOOP ( 'NONE', ( #39288, #30512 ) ) ;
#49544 = DIRECTION ( 'NONE',  ( -1.000000000000000000, -1.334402673828311860E-15, -8.547026380416719758E-31 ) ) ;
#49545 = CARTESIAN_POINT ( 'NONE',  ( -44.00727179482512241, -47.83680621839620528, 40.00000000000003553 ) ) ;
#49546 = ORIENTED_EDGE ( 'NONE', *, *, #3724, .T. ) ;
#49547 = LINE ( 'NONE', #18255, #35381 ) ;
#49548 = PLANE ( 'NONE',  #4973 ) ;
#49549 = ORIENTED_EDGE ( 'NONE', *, *, #35580, .F. ) ;
#49550 = CARTESIAN_POINT ( 'NONE',  ( -81.90266786693713641, 23.58030232261292625, 44.70113455631799582 ) ) ;
#49551 = CARTESIAN_POINT ( 'NONE',  ( -31.43908319763709969, 10.61114334766716638, -77.16174795566554678 ) ) ;
#49552 = CARTESIAN_POINT ( 'NONE',  ( 45.04506994399702080, 10.22854084020123899, 32.44892839504316839 ) ) ;
#49553 = CARTESIAN_POINT ( 'NONE',  ( -20.55634918610400419, 15.55634918610405748, 2.000000000000001776 ) ) ;
#49554 = VERTEX_POINT ( 'NONE', #59436 ) ;
#49555 = VECTOR ( 'NONE', #59257, 999.9999999999998863 ) ;
#49556 = EDGE_LOOP ( 'NONE', ( #51286, #45582, #56430, #20081 ) ) ;
#49557 = CARTESIAN_POINT ( 'NONE',  ( 15.55634918610397399, -31.11269837220809364, 85.00100000000000477 ) ) ;
#49558 = ORIENTED_EDGE ( 'NONE', *, *, #22731, .T. ) ;
#49559 = CARTESIAN_POINT ( 'NONE',  ( 33.46033188299904992, 8.722678254080102889, -20.85871202478321962 ) ) ;
#49560 = LINE ( 'NONE', #7021, #1271 ) ;
#49561 = VECTOR ( 'NONE', #15600, 1000.000000000000000 ) ;
#49562 = DIRECTION ( 'NONE',  ( -1.000000000000000000, 0.000000000000000000, 0.000000000000000000 ) ) ;
#49563 = CARTESIAN_POINT ( 'NONE',  ( -0.3732240621745017140, 7.527003275829102336, 65.43944316759959179 ) ) ;
#49564 = EDGE_CURVE ( 'NONE', #45082, #38945, #25053, .T. ) ;
#49565 = B_SPLINE_CURVE_WITH_KNOTS ( 'NONE', 3,
 ( #26891, #149, #43055, #48665, #32864, #42036, #43405, #16679, #15309, #63843, #47641, #69100, #15650, #37101, #66298, #50778, #7181, #34269 ),
 .UNSPECIFIED., .F., .F.,
 ( 4, 2, 2, 2, 2, 2, 2, 2, 4 ),
 ( 0.01000416104488733443, 0.01126184431380911413, 0.01251952758273089383, 0.01377721085165267527, 0.01503489412057445497, 0.01629257738949623641, 0.01755026065841801611, 0.01880794392733979581, 0.02006562719626157551 ),
 .UNSPECIFIED. ) ;
#49566 = PRODUCT_DEFINITION_SHAPE ( 'NONE', 'NONE',  #69582 ) ;
#49567 = LINE ( 'NONE', #39383, #56053 ) ;
#49568 = CIRCLE ( 'NONE', #55204, 65.00000000000000000 ) ;
#49570 = AXIS2_PLACEMENT_3D ( 'NONE', #9431, #15049, #53004 ) ;
#49569 = FACE_OUTER_BOUND ( 'NONE', #10859, .T. ) ;
#49571 = ORIENTED_EDGE ( 'NONE', *, *, #49975, .F. ) ;
#49572 = CARTESIAN_POINT ( 'NONE',  ( -118.8689810167775960, 42.03922634358559662, -71.89854666037425091 ) ) ;
#49573 = ORIENTED_EDGE ( 'NONE', *, *, #55022, .F. ) ;
#49574 = ORIENTED_EDGE ( 'NONE', *, *, #41912, .T. ) ;
#49575 = FACE_OUTER_BOUND ( 'NONE', #21242, .T. ) ;
#49576 = DIRECTION ( 'NONE',  ( -1.000000000000000000, 0.000000000000000000, 0.000000000000000000 ) ) ;
#49577 = CARTESIAN_POINT ( 'NONE',  ( -15.55634918610396866, 31.11269837220809009, 85.00100000000000477 ) ) ;
#49578 = CARTESIAN_POINT ( 'NONE',  ( -131.8384800362509282, 51.76463137407609594, -91.50743145908269582 ) ) ;
#49579 = DIRECTION ( 'NONE',  ( -0.000000000000000000, 1.000000000000000000, 0.000000000000000000 ) ) ;
#49580 = VECTOR ( 'NONE', #14520, 1000.000000000000000 ) ;
#49581 = VERTEX_POINT ( 'NONE', #711 ) ;
#49582 = DIRECTION ( 'NONE',  ( -0.000000000000000000, 1.000000000000000000, -0.000000000000000000 ) ) ;
#49583 = ORIENTED_EDGE ( 'NONE', *, *, #25723, .F. ) ;
#49584 = CARTESIAN_POINT ( 'NONE',  ( -71.21970990337018748, 19.62334883444993139, 36.89203884133947042 ) ) ;
#49585 = ORIENTED_EDGE ( 'NONE', *, *, #12554, .F. ) ;
#49586 = ORIENTED_EDGE ( 'NONE', *, *, #25374, .T. ) ;
#49587 = CARTESIAN_POINT ( 'NONE',  ( -144.9439644317224349, 60.40328483334190679, -75.11390089952729454 ) ) ;
#49588 = CARTESIAN_POINT ( 'NONE',  ( 91.13361825170456143, 21.00701373666981553, 16.38409351591118934 ) ) ;
#49589 = EDGE_CURVE ( 'NONE', #42920, #1235, #64370, .T. ) ;
#49590 = DIRECTION ( 'NONE',  ( 0.000000000000000000, 0.000000000000000000, 1.000000000000000000 ) ) ;
#49591 = EDGE_LOOP ( 'NONE', ( #11533, #43347 ) ) ;
#49592 = CARTESIAN_POINT ( 'NONE',  ( -442.6627218934918915, 395.0000000000064801, -136.4497041420121661 ) ) ;
#49593 = EDGE_CURVE ( 'NONE', #23015, #63135, #24919, .T. ) ;
#49594 = CARTESIAN_POINT ( 'NONE',  ( 69.20653952489904270, 15.23397960627465686, 86.75553736170155616 ) ) ;
#49595 = CARTESIAN_POINT ( 'NONE',  ( 35.44311777160620380, 8.940232499250166498, 43.78863461845804750 ) ) ;
#49596 = CARTESIAN_POINT ( 'NONE',  ( -177.1514380519393512, 93.28180884530866024, -35.87169415068767364 ) ) ;
#49597 = EDGE_CURVE ( 'NONE', #60279, #68666, #50986, .T. ) ;
#49598 = CARTESIAN_POINT ( 'NONE',  ( -133.3149301983942507, 51.57857650535022742, -14.45055437769056361 ) ) ;
#49599 = CARTESIAN_POINT ( 'NONE',  ( -36.11269837220806522, 5.594483210025202879E-14, 0.000000000000000000 ) ) ;
#49600 = CARTESIAN_POINT ( 'NONE',  ( 129.1381264900934696, 38.64720302602604107, -64.51794085108998900 ) ) ;
#49601 = ORIENTED_EDGE ( 'NONE', *, *, #45079, .T. ) ;
#49602 = CARTESIAN_POINT ( 'NONE',  ( 56.42997683260146857, -32.25922681454192542, 40.00000000000003553 ) ) ;
#49603 = CARTESIAN_POINT ( 'NONE',  ( -149.0764453401867797, 65.13297611514538232, -76.65738112195568021 ) ) ;
#49604 = ORIENTED_EDGE ( 'NONE', *, *, #60568, .T. ) ;
#49605 = ADVANCED_FACE ( 'NONE', ( #66147, #49575 ), #44307, .F. ) ;
#49606 = AXIS2_PLACEMENT_3D ( 'NONE', #12742, #23989, #23644 ) ;
#49607 = CARTESIAN_POINT ( 'NONE',  ( -156.9262190792699414, 72.10659547035874084, -41.17427441558346857 ) ) ;
#49608 = DIRECTION ( 'NONE',  ( 1.000000000000000000, 0.000000000000000000, -1.734723475976805517E-15 ) ) ;
#49609 = CARTESIAN_POINT ( 'NONE',  ( -180.4614954900548582, 97.28277348252829881, 63.59750393255907142 ) ) ;
#49611 = CARTESIAN_POINT ( 'NONE',  ( 4.065758146820642860E-17, 0.3912769056150356972, 8.000000000000001776 ) ) ;
#49610 = AXIS2_PLACEMENT_3D ( 'NONE', #60146, #33437, #54863 ) ;
#49612 = DIRECTION ( 'NONE',  ( 0.000000000000000000, 1.000000000000000000, -0.000000000000000000 ) ) ;
#49613 = DIRECTION ( 'NONE',  ( 0.2225209339563184452, -0.9749279121818226201, 0.000000000000000000 ) ) ;
#49614 = CARTESIAN_POINT ( 'NONE',  ( -13.16282047539117173, 7.297462132103659016, -91.32137775416312309 ) ) ;
#49615 = CARTESIAN_POINT ( 'NONE',  ( -149.9449619562961402, 64.55090813009799433, 3.876270649435375137 ) ) ;
#49616 = CARTESIAN_POINT ( 'NONE',  ( -84.49322488516129681, 0.000000000000000000, 43.58025477438756212 ) ) ;
#49618 = CARTESIAN_POINT ( 'NONE',  ( -15.13464256769235661, 8.488509377255647692, 39.31406149208217471 ) ) ;
#49617 = AXIS2_PLACEMENT_3D ( 'NONE', #41584, #58110, #25770 ) ;
#49619 = CARTESIAN_POINT ( 'NONE',  ( 113.4351684956570381, 30.38657459074491385, 3.463604245180824659 ) ) ;
#49620 = CARTESIAN_POINT ( 'NONE',  ( -442.6627218934913230, 1.665334536937734811E-13, 103.5502958579881749 ) ) ;
#49621 = EDGE_LOOP ( 'NONE', ( #17285, #27886, #18422, #28387 ) ) ;
#49622 = CARTESIAN_POINT ( 'NONE',  ( -38.92718193365331558, 11.96647478777219753, 11.36126298385067201 ) ) ;
#49623 = EDGE_LOOP ( 'NONE', ( #21180, #54997, #8043 ) ) ;
#49624 = CARTESIAN_POINT ( 'NONE',  ( 70.34686579112866411, -18.11777090454118877, 170.0000000000000000 ) ) ;
#49625 = EDGE_CURVE ( 'NONE', #41874, #36015, #15421, .T. ) ;
#49626 = VECTOR ( 'NONE', #45022, 1000.000000000000000 ) ;
#49627 = CARTESIAN_POINT ( 'NONE',  ( 82.14396250120411480, 18.99560174459420736, -76.18202846519534432 ) ) ;
#49628 = CARTESIAN_POINT ( 'NONE',  ( 102.7352309018612573, 26.65364508785401298, 90.71718089035570642 ) ) ;
#49629 = CARTESIAN_POINT ( 'NONE',  ( 6.686525924292799239, -5.377136764700172655, -9.183279549040156198 ) ) ;
#49630 = CARTESIAN_POINT ( 'NONE',  ( -44.29440389294402536, -17.09499999999999886, 4.000000000000000000 ) ) ;
#49631 = CLOSED_SHELL ( 'NONE', ( #5137, #32235, #66203, #64019, #29620, #6804, #7385, #56547, #2389, #56731, #38830, #19322, #29556, #33207, #34294, #45354, #57023, #9565, #6359 ) ) ;
#49632 = CYLINDRICAL_SURFACE ( 'NONE', #4739, 23.50000000000000000 ) ;
#49633 = FACE_OUTER_BOUND ( 'NONE', #24722, .T. ) ;
#49634 = CARTESIAN_POINT ( 'NONE',  ( -71.28077210551055032, 20.70883253687733117, -95.00000000000133582 ) ) ;
#49635 = CARTESIAN_POINT ( 'NONE',  ( -2.747334524841524406, 33.31268902856695746, 6.893342931471464929 ) ) ;
#49636 = VERTEX_POINT ( 'NONE', #18281 ) ;
#49637 = ORIENTED_EDGE ( 'NONE', *, *, #9282, .F. ) ;
#49638 = DIRECTION ( 'NONE',  ( -0.000000000000000000, -0.000000000000000000, 1.000000000000000000 ) ) ;
#49639 = CARTESIAN_POINT ( 'NONE',  ( 178.1903523079566298, 75.72906488635186406, 56.72024832093088520 ) ) ;
#49640 = CARTESIAN_POINT ( 'NONE',  ( 40.22957559924974191, 8.518286412483671910, -89.34336208694358561 ) ) ;
#49641 = SURFACE_STYLE_USAGE ( .BOTH. , #1469 ) ;
#49642 = CARTESIAN_POINT ( 'NONE',  ( -165.7690020878297616, 80.74028011998674970, -16.87889564165705281 ) ) ;
#49643 = CARTESIAN_POINT ( 'NONE',  ( 157.4703587214989398, -170.0000000000000000, -9.279633708673955539 ) ) ;
#49644 = ORIENTED_EDGE ( 'NONE', *, *, #63127, .F. ) ;
#49645 = CARTESIAN_POINT ( 'NONE',  ( 106.0228389049370463, 28.07756796303168656, -49.62712291136129039 ) ) ;
#49646 = CARTESIAN_POINT ( 'NONE',  ( 16.28382582968306735, 7.523443033994205997, -35.51894409868578606 ) ) ;
#49647 = CARTESIAN_POINT ( 'NONE',  ( -79.62258606008205675, 22.68765733708495702, -23.22492150694771240 ) ) ;
#49648 = CARTESIAN_POINT ( 'NONE',  ( 183.2136430849848239, 0.000000000000000000, -9.435653166495541200 ) ) ;
#49649 = DIRECTION ( 'NONE',  ( 1.387778780781445922E-16, -1.000000000000000000, -1.232595164407830946E-32 ) ) ;
#49650 = CARTESIAN_POINT ( 'NONE',  ( 211.7451286015360665, 116.5372661580811524, -14.39814270739270974 ) ) ;
#49651 = FACE_BOUND ( 'NONE', #7365, .T. ) ;
#49652 = CARTESIAN_POINT ( 'NONE',  ( 158.3516718297675823, 59.61984652322052369, 56.29275500237260133 ) ) ;
#49653 = VERTEX_POINT ( 'NONE', #39736 ) ;
#49654 = CARTESIAN_POINT ( 'NONE',  ( 110.2429982417149290, 28.88204397445231209, 2.766663615273646570 ) ) ;
#49655 = CARTESIAN_POINT ( 'NONE',  ( -62.97854483871553555, -16.08424353203763602, 170.0000000000000000 ) ) ;
#49656 = AXIS2_PLACEMENT_3D ( 'NONE', #27347, #6245, #47769 ) ;
#49657 = CARTESIAN_POINT ( 'NONE',  ( -50.52615126106342558, 14.55080735582893858, 58.66218285867929438 ) ) ;
#49658 = CARTESIAN_POINT ( 'NONE',  ( 63.01563776193091826, 13.70579113808095073, -50.72069083216976537 ) ) ;
#49659 = CARTESIAN_POINT ( 'NONE',  ( 210.0122310839191755, 115.7355030290287345, 68.86736864163312077 ) ) ;
#49660 = CARTESIAN_POINT ( 'NONE',  ( 8.000000000000000000, 4.618802153517024500, -8.785468820183664818 ) ) ;
#49661 = VECTOR ( 'NONE', #65808, 1000.000000000000114 ) ;
#49662 = ADVANCED_FACE ( 'NONE', ( #1403 ), #66840, .F. ) ;
#49663 = EDGE_LOOP ( 'NONE', ( #370, #26895, #35001, #15174, #60561 ) ) ;
#49664 = CARTESIAN_POINT ( 'NONE',  ( -65.36598343705435354, 0.000000000000000000, 41.38025477438755928 ) ) ;
#49665 = CARTESIAN_POINT ( 'NONE',  ( -56.02358673658414290, 14.94347049174936970, 57.20932295525945221 ) ) ;
#49666 = VERTEX_POINT ( 'NONE', #13360 ) ;
#49667 = AXIS2_PLACEMENT_3D ( 'NONE', #48115, #42513, #53050 ) ;
#49668 = VERTEX_POINT ( 'NONE', #8071 ) ;
#49669 = CARTESIAN_POINT ( 'NONE',  ( -15.55634918610405748, -10.55634918610400597, 85.00100000000000477 ) ) ;
#49670 = CARTESIAN_POINT ( 'NONE',  ( -61.52761555060401832, 17.56359742150277015, -19.68907097625505997 ) ) ;
#49671 = CARTESIAN_POINT ( 'NONE',  ( 102.8458551240039753, 25.60773946375956811, 35.84670615152459305 ) ) ;
#49672 = ORIENTED_EDGE ( 'NONE', *, *, #58213, .F. ) ;
#49673 = AXIS2_PLACEMENT_3D ( 'NONE', #38974, #64658, #44588 ) ;
#49674 = EDGE_LOOP ( 'NONE', ( #50918, #59895, #67593, #1769 ) ) ;
#49675 = DIRECTION ( 'NONE',  ( 0.000000000000000000, -1.000000000000000000, 0.000000000000000000 ) ) ;
#49676 = CARTESIAN_POINT ( 'NONE',  ( 164.4761273435912017, 64.62485394454746768, 34.17979310171889296 ) ) ;
#49677 = CARTESIAN_POINT ( 'NONE',  ( -155.1359377029286009, 70.46175948311804405, -64.17498559856824158 ) ) ;
#49678 = CARTESIAN_POINT ( 'NONE',  ( 68.94309019697863050, 15.16533147648755531, 15.08993511401731880 ) ) ;
#49679 = FACE_OUTER_BOUND ( 'NONE', #38081, .T. ) ;
#49680 = EDGE_CURVE ( 'NONE', #13609, #64426, #29520, .T. ) ;
#49681 = CARTESIAN_POINT ( 'NONE',  ( -50.14440374537738876, 14.45628984983895116, -37.02434562548277341 ) ) ;
#49682 = CARTESIAN_POINT ( 'NONE',  ( -48.58279704072702287, 14.07632445131079635, 14.77428691758652768 ) ) ;
#49683 = CARTESIAN_POINT ( 'NONE',  ( -127.4644500646575409, 48.74852676951793740, -22.90636119001569071 ) ) ;
#49684 = CARTESIAN_POINT ( 'NONE',  ( 0.000000000000000000, 0.000000000000000000, 0.000000000000000000 ) ) ;
#49685 = DIRECTION ( 'NONE',  ( -1.000000000000000000, -0.000000000000000000, -0.000000000000000000 ) ) ;
#49686 = CARTESIAN_POINT ( 'NONE',  ( -44.29440389294402536, 17.09499999999999886, 4.000000000000000000 ) ) ;
#49688 = EDGE_LOOP ( 'NONE', ( #60281, #43435, #22956, #56218 ) ) ;
#49687 = FACE_OUTER_BOUND ( 'NONE', #47362, .T. ) ;
#49689 = ORIENTED_EDGE ( 'NONE', *, *, #13273, .T. ) ;
#49690 = EDGE_CURVE ( 'NONE', #65175, #52293, #13697, .T. ) ;
#49691 = ORIENTED_EDGE ( 'NONE', *, *, #4703, .F. ) ;
#49692 = CARTESIAN_POINT ( 'NONE',  ( -9.525868120571905351, 7.007646177566257073, -8.764757431761587725 ) ) ;
#49693 = DIRECTION ( 'NONE',  ( -0.000000000000000000, 1.000000000000000000, -0.000000000000000000 ) ) ;
#49694 = CARTESIAN_POINT ( 'NONE',  ( -55.05276343752909440, 14.68156374112637330, -8.371773407996169425 ) ) ;
#49695 = CARTESIAN_POINT ( 'NONE',  ( 104.7147873368644753, 26.40702926859712463, -11.48552898774475572 ) ) ;
#49696 = CARTESIAN_POINT ( 'NONE',  ( -57.89360529881253825, 16.50663720601370699, -35.76264078408507174 ) ) ;
#49697 = CARTESIAN_POINT ( 'NONE',  ( 171.1328495613745417, 69.31314377685163208, 0.000000000000000000 ) ) ;
#49698 = LINE ( 'NONE', #23688, #62329 ) ;
#49699 = CARTESIAN_POINT ( 'NONE',  ( -15.15117926080556465, -170.0000000000000000, -95.00000000000133582 ) ) ;
#49700 = ORIENTED_EDGE ( 'NONE', *, *, #62105, .T. ) ;
#49701 = DIRECTION ( 'NONE',  ( 1.000000000000000000, 0.000000000000000000, 0.000000000000000000 ) ) ;
#49702 = ORIENTED_EDGE ( 'NONE', *, *, #39700, .F. ) ;
#49703 = ORIENTED_EDGE ( 'NONE', *, *, #16414, .T. ) ;
#49704 = EDGE_CURVE ( 'NONE', #58183, #37385, #31269, .T. ) ;
#49705 = DIRECTION ( 'NONE',  ( -0.000000000000000000, -0.000000000000000000, -1.000000000000000000 ) ) ;
#49706 = VECTOR ( 'NONE', #26926, 1000.000000000000114 ) ;
#49707 = CARTESIAN_POINT ( 'NONE',  ( -56.11927569309192876, 16.01314504639333336, -88.97860608119357551 ) ) ;
#49708 = CARTESIAN_POINT ( 'NONE',  ( -23.93408125862919178, 9.494352577851083552, 91.57808385503631143 ) ) ;
#49709 = DIRECTION ( 'NONE',  ( 1.000000000000000000, 0.000000000000000000, 0.000000000000000000 ) ) ;
#49710 = VECTOR ( 'NONE', #35450, 1000.000000000000000 ) ;
#49711 = DIRECTION ( 'NONE',  ( 1.000000000000000000, 0.000000000000000000, -0.000000000000000000 ) ) ;
#49712 = LINE ( 'NONE', #17363, #25862 ) ;
#49713 = LINE ( 'NONE', #1543, #52057 ) ;
#49714 = ORIENTED_EDGE ( 'NONE', *, *, #49368, .F. ) ;
#49715 = VERTEX_POINT ( 'NONE', #62221 ) ;
#49716 = ORIENTED_EDGE ( 'NONE', *, *, #49945, .F. ) ;
#49717 = AXIS2_PLACEMENT_3D ( 'NONE', #42470, #31927, #63931 ) ;
#49718 = CARTESIAN_POINT ( 'NONE',  ( 29.69502258243432635, -57.82046033912835270, 170.0000000000000000 ) ) ;
#49719 = CARTESIAN_POINT ( 'NONE',  ( -15.32520546926283167, 7.495995523981875408, 11.26390656212526586 ) ) ;
#49720 = CARTESIAN_POINT ( 'NONE',  ( 32.14349651933088126, 7.576119504381664704, -71.91552036636386447 ) ) ;
#49721 = VECTOR ( 'NONE', #7682, 1000.000000000000000 ) ;
#49722 = CARTESIAN_POINT ( 'NONE',  ( 62.04664474957769471, 12.44961624115901522, -8.923359081094497824 ) ) ;
#49723 = VECTOR ( 'NONE', #48378, 1000.000000000000000 ) ;
#49724 = CARTESIAN_POINT ( 'NONE',  ( -47.80193682758675067, 12.85650137125658077, 35.83676103695687232 ) ) ;
#49725 = CARTESIAN_POINT ( 'NONE',  ( 26.12852347772543737, 70.00000000000000000, 129.5802547743875550 ) ) ;
#49726 = ORIENTED_EDGE ( 'NONE', *, *, #39723, .T. ) ;
#49727 = CARTESIAN_POINT ( 'NONE',  ( 184.9757174666827382, 84.09845285279332927, 57.23800133820973457 ) ) ;
#49728 = CARTESIAN_POINT ( 'NONE',  ( 177.5945652320814077, 75.14951358071814980, -63.92694727933915999 ) ) ;
#49729 = DIRECTION ( 'NONE',  ( 0.9502963056556088528, 0.3113469631412870142, -2.958228394578794270E-31 ) ) ;
#49730 = CARTESIAN_POINT ( 'NONE',  ( -1.096061481932295578, 7.553048580900441067, -46.23872224921927199 ) ) ;
#49731 = FACE_OUTER_BOUND ( 'NONE', #53930, .T. ) ;
#49732 = CARTESIAN_POINT ( 'NONE',  ( -172.7154982671752634, 86.67743928531943709, 3.977144016177345254 ) ) ;
#49733 = LINE ( 'NONE', #18097, #11551 ) ;
#49734 = FACE_BOUND ( 'NONE', #46615, .T. ) ;
#49735 = DIRECTION ( 'NONE',  ( -0.000000000000000000, -0.000000000000000000, -1.000000000000000000 ) ) ;
#49736 = ORIENTED_EDGE ( 'NONE', *, *, #43957, .T. ) ;
#49737 = FACE_OUTER_BOUND ( 'NONE', #5911, .T. ) ;
#49738 = CARTESIAN_POINT ( 'NONE',  ( -129.3963145237380843, 48.84337839101543466, -62.62225689922211558 ) ) ;
#49739 = LINE ( 'NONE', #56085, #34326 ) ;
#49740 = CARTESIAN_POINT ( 'NONE',  ( 43.14356474118744700, 8.925336319666881124, -76.48306521520852641 ) ) ;
#49741 = LINE ( 'NONE', #39564, #19807 ) ;
#49742 = EDGE_LOOP ( 'NONE', ( #3845, #37992, #7098, #33101, #50408, #21084, #33599, #27562, #14856 ) ) ;
#49743 = EDGE_CURVE ( 'NONE', #15400, #23050, #41123, .T. ) ;
#49744 = EDGE_LOOP ( 'NONE', ( #44354, #44625, #60263, #43468 ) ) ;
#49745 = CARTESIAN_POINT ( 'NONE',  ( 410.0000000000000000, 0.000000000000000000, 380.0000000000000000 ) ) ;
#49746 = CARTESIAN_POINT ( 'NONE',  ( 187.5458047452486312, 85.39230033703691447, 86.67446375648381718 ) ) ;
#49747 = VERTEX_POINT ( 'NONE', #57304 ) ;
#49748 = ADVANCED_FACE ( 'NONE', ( #8428 ), #36193, .F. ) ;
#49749 = ORIENTED_EDGE ( 'NONE', *, *, #52805, .T. ) ;
#49750 = MECHANICAL_DESIGN_GEOMETRIC_PRESENTATION_REPRESENTATION (  '', ( #46399 ), #25081 ) ;
#49751 = LINE ( 'NONE', #66664, #49870 ) ;
#49752 = DIRECTION ( 'NONE',  ( -1.387778780781446169E-16, 1.000000000000000000, 3.469446951953615421E-17 ) ) ;
#49753 = DIRECTION ( 'NONE',  ( -0.08963930890344087854, 0.9959742939952382912, 0.000000000000000000 ) ) ;
#49754 = EDGE_LOOP ( 'NONE', ( #20637, #60237 ) ) ;
#49755 = CARTESIAN_POINT ( 'NONE',  ( 100.0000000000000284, 0.000000000000000000, 0.000000000000000000 ) ) ;
#49756 = DIRECTION ( 'NONE',  ( 6.651034621319562720E-17, 2.409948271074239284E-16, 1.000000000000000000 ) ) ;
#49757 = CARTESIAN_POINT ( 'NONE',  ( -76.77329340382466683, 21.60914066444071935, -35.34250697107755457 ) ) ;
#49758 = AXIS2_PLACEMENT_3D ( 'NONE', #5670, #20475, #20138 ) ;
#49759 = CARTESIAN_POINT ( 'NONE',  ( 2.999999999999992450, 2.574819895207310198E-15, 21.02499999999999858 ) ) ;
#49760 = CARTESIAN_POINT ( 'NONE',  ( 89.88695630745277754, 20.55793566325391453, -36.54904141640419368 ) ) ;
#49761 = CONICAL_SURFACE ( 'NONE', #21648, 65.00000000000000000, 0.7853981633974497223 ) ;
#49762 = CARTESIAN_POINT ( 'NONE',  ( -48.70883077256303295, 14.10659259062419224, -19.87991046666667216 ) ) ;
#49764 = EDGE_CURVE ( 'NONE', #23613, #25857, #35502, .T. ) ;
#49763 = CIRCLE ( 'NONE', #28436, 74.95140232871122521 ) ;
#49765 = ORIENTED_EDGE ( 'NONE', *, *, #12412, .T. ) ;
#49766 = VECTOR ( 'NONE', #61528, 1000.000000000000000 ) ;
#49767 = EDGE_CURVE ( 'NONE', #40273, #57137, #63618, .T. ) ;
#49768 = CARTESIAN_POINT ( 'NONE',  ( -122.7930600691578178, 44.48546375740914272, -8.724487278797921519 ) ) ;
#49769 = AXIS2_PLACEMENT_3D ( 'NONE', #21536, #42982, #26485 ) ;
#49770 = CARTESIAN_POINT ( 'NONE',  ( -76.10382222627279702, 22.43453174720078991, 18.12638239063526413 ) ) ;
#49771 = CARTESIAN_POINT ( 'NONE',  ( -142.3187766126154941, 59.59460822661996815, -44.52240461455945564 ) ) ;
#49772 = EDGE_CURVE ( 'NONE', #34394, #14640, #9114, .T. ) ;
#49773 = CARTESIAN_POINT ( 'NONE',  ( 0.000000000000000000, 35.00000000000000000, 0.000000000000000000 ) ) ;
#49775 = ORIENTED_EDGE ( 'NONE', *, *, #53021, .F. ) ;
#49774 = CARTESIAN_POINT ( 'NONE',  ( -131.7960692854462081, 50.50475183506788568, 87.17087325982676305 ) ) ;
#49776 = DIRECTION ( 'NONE',  ( 0.04486483035050447404, 0.9989930665413151445, 0.000000000000000000 ) ) ;
#49777 = VECTOR ( 'NONE', #43399, 1000.000000000000000 ) ;
#49778 = EDGE_CURVE ( 'NONE', #56227, #5626, #15686, .T. ) ;
#49779 = ORIENTED_EDGE ( 'NONE', *, *, #11317, .T. ) ;
#49780 = FACE_OUTER_BOUND ( 'NONE', #53747, .T. ) ;
#49781 = CARTESIAN_POINT ( 'NONE',  ( 83.37782009939532202, 19.39546426214657515, 43.97496025697474664 ) ) ;
#49782 = LINE ( 'NONE', #3009, #5118 ) ;
#49783 = CARTESIAN_POINT ( 'NONE',  ( 185.5415406465189676, 83.23025870924408309, -22.93060259331669570 ) ) ;
#49784 = CARTESIAN_POINT ( 'NONE',  ( 141.2894128405439460, 46.09731134920846785, -15.64124612904248579 ) ) ;
#49785 = CARTESIAN_POINT ( 'NONE',  ( -49.77357484059130144, -41.82599373102875973, 41.38025477438755928 ) ) ;
#49786 = CARTESIAN_POINT ( 'NONE',  ( 89.22118407503259618, 20.32164250407901207, -63.12413010457111540 ) ) ;
#49787 = CARTESIAN_POINT ( 'NONE',  ( 61.62594073580573450, -21.79346734964915555, 3.125053320693586388E-16 ) ) ;
#49788 = CARTESIAN_POINT ( 'NONE',  ( -156.8685326950935064, 70.68337020863233988, -94.46790515003011990 ) ) ;
#49789 = VERTEX_POINT ( 'NONE', #57991 ) ;
#49790 = VERTEX_POINT ( 'NONE', #24957 ) ;
#49791 = EDGE_CURVE ( 'NONE', #3346, #46713, #46387, .T. ) ;
#49792 = CARTESIAN_POINT ( 'NONE',  ( 44.34263167748004264, 9.103379693481564061, 31.75007173307530550 ) ) ;
#49793 = LINE ( 'NONE', #1620, #21695 ) ;
#49794 = CARTESIAN_POINT ( 'NONE',  ( 6.375108774214766072E-14, 31.11269837220806167, 2.000000000000001776 ) ) ;
#49796 = EDGE_CURVE ( 'NONE', #62951, #23405, #5212, .T. ) ;
#49795 = CARTESIAN_POINT ( 'NONE',  ( -447.6627218934913230, 399.9999999999997726, 103.5502958579881891 ) ) ;
#49797 = EDGE_CURVE ( 'NONE', #34803, #62792, #65000, .T. ) ;
#49798 = EDGE_CURVE ( 'NONE', #23417, #67479, #16107, .T. ) ;
#49799 = CARTESIAN_POINT ( 'NONE',  ( 212.1488570093001726, 119.0116247937291547, -44.69745977012216542 ) ) ;
#49800 = DIRECTION ( 'NONE',  ( -0.000000000000000000, 1.000000000000000000, -0.000000000000000000 ) ) ;
#49801 = DIRECTION ( 'NONE',  ( -0.000000000000000000, 1.000000000000000000, -0.000000000000000000 ) ) ;
#49802 = CARTESIAN_POINT ( 'NONE',  ( -27.70562707895080123, 9.007984652865424380, -49.34063250321889882 ) ) ;
#49803 = LINE ( 'NONE', #28718, #38538 ) ;
#49804 = ORIENTED_EDGE ( 'NONE', *, *, #8894, .T. ) ;
#49805 = CARTESIAN_POINT ( 'NONE',  ( -25.07901552294942604, 9.649193085547802085, 14.85442492764910583 ) ) ;
#49806 = ORIENTED_EDGE ( 'NONE', *, *, #21801, .T. ) ;
#49807 = FACE_OUTER_BOUND ( 'NONE', #4103, .T. ) ;
#49808 = AXIS2_PLACEMENT_3D ( 'NONE', #45430, #23979, #33842 ) ;
#49809 = CARTESIAN_POINT ( 'NONE',  ( -86.13912425708386422, 25.31016616653309725, 90.88912426079336626 ) ) ;
#49810 = CARTESIAN_POINT ( 'NONE',  ( 200.0000000000000000, 0.000000000000000000, -10.00000000000000000 ) ) ;
#49811 = CARTESIAN_POINT ( 'NONE',  ( 126.3554864210862121, 38.22801630372147486, 37.23830996261533954 ) ) ;
#49812 = CARTESIAN_POINT ( 'NONE',  ( -41.65447303895287234, 2.493917956440751649, 13.79046412286063550 ) ) ;
#49813 = DIRECTION ( 'NONE',  ( -1.000000000000000000, 0.000000000000000000, 0.000000000000000000 ) ) ;
#49814 = AXIS2_PLACEMENT_3D ( 'NONE', #12978, #40729, #34084 ) ;
#49815 = CARTESIAN_POINT ( 'NONE',  ( -422.6627218934918915, 395.0000000000064801, -116.4497041420121377 ) ) ;
#49816 = CIRCLE ( 'NONE', #19500, 25.00000000000395772 ) ;
#49817 = DIRECTION ( 'NONE',  ( 1.000000000000000000, 0.000000000000000000, 0.000000000000000000 ) ) ;
#49818 = CARTESIAN_POINT ( 'NONE',  ( 212.1225368307689507, 117.1159163218940478, 91.47960818144875361 ) ) ;
#49819 = VERTEX_POINT ( 'NONE', #32299 ) ;
#49820 = DIRECTION ( 'NONE',  ( 0.000000000000000000, 0.000000000000000000, 1.000000000000000000 ) ) ;
#49821 = CARTESIAN_POINT ( 'NONE',  ( 12.03162622199373466, 7.415834979634797541, -63.36749908192140879 ) ) ;
#49822 = CARTESIAN_POINT ( 'NONE',  ( -8.320534640989469821, 7.931748412542455995, 18.27103044898354511 ) ) ;
#49823 = AXIS2_PLACEMENT_3D ( 'NONE', #284, #27021, #23150 ) ;
#49824 = LINE ( 'NONE', #23110, #34384 ) ;
#49825 = CARTESIAN_POINT ( 'NONE',  ( 45.82394788922801609, 46.11928342727494368, 3.061616997868437868E-16 ) ) ;
#49826 = CARTESIAN_POINT ( 'NONE',  ( -95.69827994653627457, 29.56114141562974140, -92.60069445672345978 ) ) ;
#49827 = AXIS2_PLACEMENT_3D ( 'NONE', #33340, #66053, #59688 ) ;
#49828 = ORIENTED_EDGE ( 'NONE', *, *, #62967, .F. ) ;
#49829 = DIRECTION ( 'NONE',  ( -9.622754328042306404E-15, 3.937372610439379594E-15, -0.9999999999999997780 ) ) ;
#49830 = LINE ( 'NONE', #12921, #30715 ) ;
#49831 = CARTESIAN_POINT ( 'NONE',  ( -37.93983213483219430, 11.77368372188049150, -39.04474621805233880 ) ) ;
#49832 = CARTESIAN_POINT ( 'NONE',  ( -168.1811549361197535, 83.25427431521138999, -47.86022128265202724 ) ) ;
#49833 = CARTESIAN_POINT ( 'NONE',  ( -168.3771781763924196, 81.99782240093493613, 86.17408653350808834 ) ) ;
#49834 = ORIENTED_EDGE ( 'NONE', *, *, #40648, .F. ) ;
#49835 = CARTESIAN_POINT ( 'NONE',  ( -121.5921196778231490, 43.72569502503146310, -48.57545037443222924 ) ) ;
#49836 = FACE_OUTER_BOUND ( 'NONE', #63653, .T. ) ;
#49837 = CARTESIAN_POINT ( 'NONE',  ( 204.6977192012829789, -170.0000000000000000, -24.48138044215792419 ) ) ;
#49838 = CARTESIAN_POINT ( 'NONE',  ( -4.731197926646207641, 7.716745361328039898, -76.59901871495883086 ) ) ;
#49839 = EDGE_CURVE ( 'NONE', #62781, #17818, #26330, .T. ) ;
#49840 =( REPRESENTATION_RELATIONSHIP ('NONE','NONE', #40274, #52783 ) REPRESENTATION_RELATIONSHIP_WITH_TRANSFORMATION ( #69554 )SHAPE_REPRESENTATION_RELATIONSHIP( ) );
#49841 = DIRECTION ( 'NONE',  ( -0.000000000000000000, -0.000000000000000000, 1.000000000000000000 ) ) ;
#49842 = ORIENTED_EDGE ( 'NONE', *, *, #25032, .T. ) ;
#49843 = CARTESIAN_POINT ( 'NONE',  ( -66.00000000000000000, 29.79383981485516486, 29.99999999999999645 ) ) ;
#49844 = CARTESIAN_POINT ( 'NONE',  ( 197.3059626281005592, 96.72682679064189415, -42.51509034027653655 ) ) ;
#49845 = LINE ( 'NONE', #12578, #58856 ) ;
#49846 = CARTESIAN_POINT ( 'NONE',  ( 22.30016284075437127, 6.796348835713780012, -39.26592317429871315 ) ) ;
#49848 = ORIENTED_EDGE ( 'NONE', *, *, #58667, .T. ) ;
#49847 = LINE ( 'NONE', #6951, #46659 ) ;
#49849 = ADVANCED_FACE ( 'NONE', ( #43866 ), #27005, .F. ) ;
#49850 = FACE_OUTER_BOUND ( 'NONE', #65459, .T. ) ;
#49851 = EDGE_CURVE ( 'NONE', #65894, #55546, #34137, .T. ) ;
#49852 = VERTEX_POINT ( 'NONE', #11171 ) ;
#49854 = ORIENTED_EDGE ( 'NONE', *, *, #15653, .F. ) ;
#49853 = EDGE_CURVE ( 'NONE', #20172, #62269, #50953, .T. ) ;
#49855 = CARTESIAN_POINT ( 'NONE',  ( -74.79002408692173276, 20.88280597089420709, -9.345738677820531137 ) ) ;
#49856 = CIRCLE ( 'NONE', #48679, 65.36598343705435354 ) ;
#49857 = CARTESIAN_POINT ( 'NONE',  ( -38.69882630632968556, 11.92152976277064624, -94.57351083330412678 ) ) ;
#49858 = EDGE_CURVE ( 'NONE', #64201, #26921, #64652, .T. ) ;
#49859 = VECTOR ( 'NONE', #46619, 1000.000000000000000 ) ;
#49861 = ORIENTED_EDGE ( 'NONE', *, *, #4841, .F. ) ;
#49860 = DIRECTION ( 'NONE',  ( 0.9839295885986296675, 0.1785568947986370669, 0.000000000000000000 ) ) ;
#49862 = CARTESIAN_POINT ( 'NONE',  ( 164.6499013411308283, 63.45576988183551492, 39.09533417168172065 ) ) ;
#49863 = CARTESIAN_POINT ( 'NONE',  ( 122.2516123306975402, 190.0000000000000000, -21.28179539054375624 ) ) ;
#49864 = ADVANCED_FACE ( 'NONE', ( #63954 ), #37562, .F. ) ;
#49865 = CARTESIAN_POINT ( 'NONE',  ( 157.4703587214989398, -170.0000000000000000, -97.31328548006501933 ) ) ;
#49866 = VECTOR ( 'NONE', #45236, 1000.000000000000000 ) ;
#49867 = ORIENTED_EDGE ( 'NONE', *, *, #42450, .F. ) ;
#49868 = CARTESIAN_POINT ( 'NONE',  ( -144.5610324426709496, 61.38759170201291226, -90.35978530201006720 ) ) ;
#49869 = AXIS2_PLACEMENT_3D ( 'NONE', #48399, #37179, #589 ) ;
#49870 = VECTOR ( 'NONE', #50470, 1000.000000000000000 ) ;
#49871 = CARTESIAN_POINT ( 'NONE',  ( -34.74312654625183683, 10.15703162223799794, -22.71010778213880599 ) ) ;
#49872 = CARTESIAN_POINT ( 'NONE',  ( -173.9617926765113509, 89.58633395456780590, 45.78627089199527944 ) ) ;
#49873 = VECTOR ( 'NONE', #21643, 1000.000000000000000 ) ;
#49874 = CARTESIAN_POINT ( 'NONE',  ( -132.9126122820979106, 52.52752252041128145, 8.618821758353476525 ) ) ;
#49875 = CARTESIAN_POINT ( 'NONE',  ( 22.28700331106866628, 7.803633676228378668, 68.11117160914710666 ) ) ;
#49876 = EDGE_LOOP ( 'NONE', ( #44124, #18956, #20476, #1758 ) ) ;
#49877 = ORIENTED_EDGE ( 'NONE', *, *, #3701, .F. ) ;
#49878 = ORIENTED_EDGE ( 'NONE', *, *, #45589, .T. ) ;
#49879 = VECTOR ( 'NONE', #33140, 1000.000000000000000 ) ;
#49881 = ADVANCED_FACE ( 'NONE', ( #59696 ), #31951, .T. ) ;
#49880 = CARTESIAN_POINT ( 'NONE',  ( 206.0512581537811911, 108.2133605824158025, -90.10690865741280220 ) ) ;
#49882 = EDGE_CURVE ( 'NONE', #45637, #35650, #4863, .T. ) ;
#49883 = CARTESIAN_POINT ( 'NONE',  ( -109.7079446832838983, 37.86719386855315861, 10.10418760775352354 ) ) ;
#49884 = DIRECTION ( 'NONE',  ( -0.000000000000000000, 1.000000000000000000, -0.000000000000000000 ) ) ;
#49885 = CARTESIAN_POINT ( 'NONE',  ( -37.79823708645147207, 10.72197716414928870, -46.80106602748205091 ) ) ;
#49886 = CARTESIAN_POINT ( 'NONE',  ( 0.000000000000000000, 0.000000000000000000, 40.00000000000003553 ) ) ;
#49887 = EDGE_CURVE ( 'NONE', #65236, #30808, #38252, .T. ) ;
#49888 = DIRECTION ( 'NONE',  ( 0.7530714660036099684, 0.6579387259397136978, 0.000000000000000000 ) ) ;
#49889 = CARTESIAN_POINT ( 'NONE',  ( -131.6508182719824163, 50.40277850441008667, 60.13134880733180410 ) ) ;
#49890 = CARTESIAN_POINT ( 'NONE',  ( -75.43495400358862923, 22.18831810339352728, -22.54335848465174408 ) ) ;
#49891 = ORIENTED_EDGE ( 'NONE', *, *, #40894, .T. ) ;
#49892 = CARTESIAN_POINT ( 'NONE',  ( 0.000000000000000000, 0.000000000000000000, 15.00000000000000000 ) ) ;
#49893 = EDGE_LOOP ( 'NONE', ( #804, #4708, #37612, #20729 ) ) ;
#49894 = CARTESIAN_POINT ( 'NONE',  ( 37.00112095025830428, 8.109340230899356072, 44.52341621389895465 ) ) ;
#49895 = CARTESIAN_POINT ( 'NONE',  ( 9.850262805259839993, 192.0000000000000000, -1.724042536399416070 ) ) ;
#49896 = LINE ( 'NONE', #43570, #60152 ) ;
#49897 = LINE ( 'NONE', #29150, #57287 ) ;
#49898 = CARTESIAN_POINT ( 'NONE',  ( 0.000000000000000000, 0.000000000000000000, -5.000000000000000000 ) ) ;
#49899 = LINE ( 'NONE', #8040, #46846 ) ;
#49900 = CARTESIAN_POINT ( 'NONE',  ( 86.62931800182293784, 19.42108912189597092, 29.71208757247930521 ) ) ;
#49901 = CARTESIAN_POINT ( 'NONE',  ( 163.7403496014743780, 64.00600007368873889, -74.59240683662380889 ) ) ;
#49902 = ORIENTED_EDGE ( 'NONE', *, *, #42152, .F. ) ;
#49903 = DIRECTION ( 'NONE',  ( 1.000000000000000000, 0.000000000000000000, 0.000000000000000000 ) ) ;
#49904 = PLANE ( 'NONE',  #53180 ) ;
#49905 = VERTEX_POINT ( 'NONE', #22428 ) ;
#49906 = CARTESIAN_POINT ( 'NONE',  ( 3.319543390096042934, -7.321065037175443990, -9.483111142572223429 ) ) ;
#49907 = PLANE ( 'NONE',  #7094 ) ;
#49908 = DIRECTION ( 'NONE',  ( 0.000000000000000000, 0.000000000000000000, -1.000000000000000000 ) ) ;
#49909 = ORIENTED_EDGE ( 'NONE', *, *, #27399, .F. ) ;
#49910 = DIRECTION ( 'NONE',  ( 0.000000000000000000, -1.000000000000000000, 0.000000000000000000 ) ) ;
#49911 = CARTESIAN_POINT ( 'NONE',  ( -9.525868120571907127, 7.007646177566256185, -62.45385861268897543 ) ) ;
#49912 = CARTESIAN_POINT ( 'NONE',  ( 41.09759788073306908, 9.651672055033841957, 44.72369366750157837 ) ) ;
#49913 = CARTESIAN_POINT ( 'NONE',  ( -28.35330809568272414, 9.105138953156460602, 71.40111999495567829 ) ) ;
#49914 = VECTOR ( 'NONE', #28062, 1000.000000000000000 ) ;
#49915 = ORIENTED_EDGE ( 'NONE', *, *, #33675, .F. ) ;
#49916 = ORIENTED_EDGE ( 'NONE', *, *, #21072, .T. ) ;
#49917 = LINE ( 'NONE', #60823, #35672 ) ;
#49918 = EDGE_LOOP ( 'NONE', ( #24246, #4552 ) ) ;
#49919 = DIRECTION ( 'NONE',  ( 0.000000000000000000, 0.000000000000000000, 1.000000000000000000 ) ) ;
#49920 = CARTESIAN_POINT ( 'NONE',  ( -190.6985136298601731, 109.1272424661242582, 94.99999999999866418 ) ) ;
#49921 = AXIS2_PLACEMENT_3D ( 'NONE', #7714, #1737, #29500 ) ;
#49922 = DIRECTION ( 'NONE',  ( -0.2225209339563184452, 0.9749279121818226201, 0.000000000000000000 ) ) ;
#49923 = CARTESIAN_POINT ( 'NONE',  ( 141.0393956947250729, 47.13639180521968086, 88.51104251071252804 ) ) ;
#49924 = LINE ( 'NONE', #55916, #62782 ) ;
#49925 = AXIS2_PLACEMENT_3D ( 'NONE', #46311, #50908, #36458 ) ;
#49926 = VERTEX_POINT ( 'NONE', #15428 ) ;
#49927 = EDGE_CURVE ( 'NONE', #41538, #67458, #36886, .T. ) ;
#49928 = VECTOR ( 'NONE', #41311, 1000.000000000000000 ) ;
#49929 = CARTESIAN_POINT ( 'NONE',  ( 262.2516123306975260, 190.0000000000000000, -21.28179539054375624 ) ) ;
#49930 = ORIENTED_EDGE ( 'NONE', *, *, #27089, .F. ) ;
#49931 = ORIENTED_EDGE ( 'NONE', *, *, #59760, .T. ) ;
#49932 = CARTESIAN_POINT ( 'NONE',  ( -44.39004539972346208, 1.224646799147353256E-15, -9.999999999999998224 ) ) ;
#49933 = PLANE ( 'NONE',  #11441 ) ;
#49934 = CARTESIAN_POINT ( 'NONE',  ( 63.01563776193091826, 12.67277567978498176, 56.65751152968497451 ) ) ;
#49935 = CARTESIAN_POINT ( 'NONE',  ( -127.5408520446061118, 48.79957756518083301, -88.77401935478938810 ) ) ;
#49936 = CARTESIAN_POINT ( 'NONE',  ( 0.000000000000000000, 0.000000000000000000, 0.000000000000000000 ) ) ;
#49937 = ORIENTED_EDGE ( 'NONE', *, *, #42584, .F. ) ;
#49938 = EDGE_CURVE ( 'NONE', #29458, #53628, #54766, .T. ) ;
#49939 = ORIENTED_EDGE ( 'NONE', *, *, #10089, .T. ) ;
#49940 = CARTESIAN_POINT ( 'NONE',  ( 11.21653854975268949, 6.397128675385705954, 43.48040107386871966 ) ) ;
#49941 = ORIENTED_EDGE ( 'NONE', *, *, #42833, .F. ) ;
#49942 = DIRECTION ( 'NONE',  ( -0.000000000000000000, -0.000000000000000000, 1.000000000000000000 ) ) ;
#49943 = ADVANCED_FACE ( 'NONE', ( #48106 ), #69563, .F. ) ;
#49944 = B_SPLINE_CURVE_WITH_KNOTS ( 'NONE', 3,
 ( #26446, #43289, #54184, #48553, #11283, #37327, #16222, #42273, #27465, #42943, #65117, #59123, #6005, #43639, #48909, #388, #10944, #15544, #5332, #20814, #58435, #32415, #53145, #59818, #4977, #22201, #63736, #47883, #69347, #36995, #42613, #15880, #58778, #32064, #26787, #53840, #67810, #54893, #44342, #66525, #62171, #1095, #40714, #17978, #3437, #33471 ),
 .UNSPECIFIED., .F., .F.,
 ( 4, 2, 2, 2, 2, 2, 2, 2, 2, 2, 2, 2, 2, 2, 2, 2, 2, 2, 2, 2, 2, 2, 4 ),
 ( 6.938893903907228378E-18, 0.003192770216278285802, 0.003990962770347853891, 0.004789155324417422414, 0.006385540432556558593, 0.007183732986626134055, 0.007981925540695709517, 0.009578310648834860441, 0.01037650320290445585, 0.01117469575697405126, 0.01197288831104364668, 0.01277108086511324209, 0.01436746597325243117, 0.01596385108139162373, 0.01676204363546120527, 0.01756023618953079027, 0.01835842874360037527, 0.01915662129766995680, 0.02075300640580914763, 0.02234939151394833845, 0.02394577662208752927, 0.02474396917615712468, 0.02554216173022672010 ),
 .UNSPECIFIED. ) ;
#49945 = EDGE_CURVE ( 'NONE', #54901, #5523, #13942, .T. ) ;
#49946 = VERTEX_POINT ( 'NONE', #7299 ) ;
#49947 = CARTESIAN_POINT ( 'NONE',  ( -143.2471548081022945, 59.04577938365765988, -73.31919755755201606 ) ) ;
#49948 = DIRECTION ( 'NONE',  ( 0.9195277725514544587, -0.3930250316539148359, 2.500042656554809847E-16 ) ) ;
#49949 = EDGE_CURVE ( 'NONE', #17365, #7619, #39999, .T. ) ;
#49950 = CARTESIAN_POINT ( 'NONE',  ( -445.5916540816259044, 394.9999999999998863, 106.4792280461225715 ) ) ;
#49951 = VERTEX_POINT ( 'NONE', #28761 ) ;
#49952 = CARTESIAN_POINT ( 'NONE',  ( 65.00000000000000000, 0.000000000000000000, -0.002000000000002000178 ) ) ;
#49953 = CARTESIAN_POINT ( 'NONE',  ( 63.36355093506870872, 13.78687103992073304, 83.50303152118553385 ) ) ;
#49954 = CARTESIAN_POINT ( 'NONE',  ( 35.66087318222939473, 8.964867769223229033, 30.89476568492769459 ) ) ;
#49955 = CIRCLE ( 'NONE', #11743, 243.4957430088094839 ) ;
#49956 = CARTESIAN_POINT ( 'NONE',  ( 63.01563776193091826, 13.70579113808094895, 29.81296093922127710 ) ) ;
#49957 = CARTESIAN_POINT ( 'NONE',  ( -130.1964689553233256, 49.39217932424205060, -9.408478371563832710 ) ) ;
#49958 = CARTESIAN_POINT ( 'NONE',  ( 157.4703587214989113, 57.65129005721576050, 71.25401806271709404 ) ) ;
#49959 = CARTESIAN_POINT ( 'NONE',  ( 15.78827728214693416, -170.0000000000000000, 64.35925826316893961 ) ) ;
#49960 = ORIENTED_EDGE ( 'NONE', *, *, #15434, .T. ) ;
#49961 = CARTESIAN_POINT ( 'NONE',  ( 0.000000000000000000, 190.0000000000000000, 380.0000000000000000 ) ) ;
#49962 = CARTESIAN_POINT ( 'NONE',  ( -142.9756886485677683, 60.11539876121631210, -72.85257420866612676 ) ) ;
#49963 = VERTEX_POINT ( 'NONE', #49843 ) ;
#49964 = AXIS2_PLACEMENT_3D ( 'NONE', #4950, #37643, #21809 ) ;
#49965 = CARTESIAN_POINT ( 'NONE',  ( -150.3831389294225573, 66.25266777263976792, -49.76475080778571680 ) ) ;
#49966 = CARTESIAN_POINT ( 'NONE',  ( 110.2429982417149574, -170.0000000000000000, -16.57788697519001175 ) ) ;
#49967 = AXIS2_PLACEMENT_3D ( 'NONE', #22720, #38910, #54718 ) ;
#49968 = AXIS2_PLACEMENT_3D ( 'NONE', #38496, #63854, #32526 ) ;
#49969 = CARTESIAN_POINT ( 'NONE',  ( -37.52119286077852678, 11.69341290629620467, 33.32117128371067594 ) ) ;
#49970 = DIRECTION ( 'NONE',  ( -0.000000000000000000, 0.000000000000000000, 1.000000000000000000 ) ) ;
#49971 = DIRECTION ( 'NONE',  ( -0.000000000000000000, -0.000000000000000000, 1.000000000000000000 ) ) ;
#49972 = CARTESIAN_POINT ( 'NONE',  ( 29.67531435111662219, 24.26667234255101135, 13.32819397642333215 ) ) ;
#49973 = LINE ( 'NONE', #33473, #17954 ) ;
#49974 = VECTOR ( 'NONE', #8044, 1000.000000000000000 ) ;
#49975 = EDGE_CURVE ( 'NONE', #24702, #19058, #23829, .T. ) ;
#49976 = CARTESIAN_POINT ( 'NONE',  ( -47.80896875121164413, 12.85816703949531181, -67.60146438707388938 ) ) ;
#49977 = CARTESIAN_POINT ( 'NONE',  ( 204.6977192012829789, 108.0580384837235073, 44.20772073876944575 ) ) ;
#49978 = VECTOR ( 'NONE', #27358, 1000.000000000000114 ) ;
#49979 = CARTESIAN_POINT ( 'NONE',  ( 66.63364047053092065, -1.250000000000021760, 34.48241795236666007 ) ) ;
#49980 = CARTESIAN_POINT ( 'NONE',  ( 116.9200705848630548, 32.09536795999726166, 13.72062155485845381 ) ) ;
#49981 = CARTESIAN_POINT ( 'NONE',  ( 46.44475613279522008, 10.44930307940658309, -94.19703056843508193 ) ) ;
#49982 = ORIENTED_EDGE ( 'NONE', *, *, #4195, .F. ) ;
#49984 = AXIS2_PLACEMENT_3D ( 'NONE', #64145, #474, #47957 ) ;
#49983 = CARTESIAN_POINT ( 'NONE',  ( -101.3502439362134595, 33.43728945125133123, -49.97127150509140847 ) ) ;
#49985 = ORIENTED_EDGE ( 'NONE', *, *, #10558, .T. ) ;
#49986 = LINE ( 'NONE', #60544, #18343 ) ;
#49987 = CARTESIAN_POINT ( 'NONE',  ( 79.37778929114109872, 18.12554302172301846, -68.18717443657236288 ) ) ;
#49988 = LINE ( 'NONE', #29927, #13643 ) ;
#49989 = CARTESIAN_POINT ( 'NONE',  ( 0.000000000000000000, 0.000000000000000000, -2.000000000000000000 ) ) ;
#49990 = DIRECTION ( 'NONE',  ( -0.000000000000000000, 1.000000000000000000, -0.000000000000000000 ) ) ;
#49991 = CARTESIAN_POINT ( 'NONE',  ( -52.13778968636738398, -39.42540649522064911, 41.38025477438755928 ) ) ;
#49992 = FACE_OUTER_BOUND ( 'NONE', #20418, .T. ) ;
#49993 = CARTESIAN_POINT ( 'NONE',  ( -121.1841775822198031, 44.65790002524553159, -21.42663191464236760 ) ) ;
#49994 = EDGE_LOOP ( 'NONE', ( #67696, #23324, #65076, #9910 ) ) ;
#49995 = ORIENTED_EDGE ( 'NONE', *, *, #8767, .T. ) ;
#49996 = PLANE ( 'NONE',  #2886 ) ;
#49997 = CARTESIAN_POINT ( 'NONE',  ( 176.6258282025054029, 74.21441092921632787, 57.61756429977015159 ) ) ;
#49998 = CYLINDRICAL_SURFACE ( 'NONE', #35668, 60.00000000000000000 ) ;
#49999 = CARTESIAN_POINT ( 'NONE',  ( -165.9154624515710452, 80.89088623112733956, 67.26787457162097894 ) ) ;
#50000 = CARTESIAN_POINT ( 'NONE',  ( -165.9121868482146454, 80.88751546905567125, -17.45774927130959142 ) ) ;
#50001 = LINE ( 'NONE', #11670, #13788 ) ;
#50002 = ORIENTED_EDGE ( 'NONE', *, *, #64880, .F. ) ;
#50003 = CARTESIAN_POINT ( 'NONE',  ( 103.4725384926516938, 26.96797537091726937, -46.65885272433202147 ) ) ;
#50004 = EDGE_CURVE ( 'NONE', #19565, #38069, #38607, .T. ) ;
#50005 = PLANE ( 'NONE',  #9899 ) ;
#50006 = CARTESIAN_POINT ( 'NONE',  ( -80.55742067659895156, 23.05042616197511407, -23.04419711036395313 ) ) ;
#50007 = FILL_AREA_STYLE_COLOUR ( '', #46492 ) ;
#50008 = CARTESIAN_POINT ( 'NONE',  ( 208.9781236209185806, 112.4006213943319636, -10.80618506829177505 ) ) ;
#50009 = FACE_BOUND ( 'NONE', #46012, .T. ) ;
#50010 = EDGE_CURVE ( 'NONE', #27646, #35609, #22236, .T. ) ;
#50011 = CARTESIAN_POINT ( 'NONE',  ( 163.1370549780983481, 63.50181104276883559, 58.81513812535254715 ) ) ;
#50012 = EDGE_CURVE ( 'NONE', #59078, #6708, #57048, .T. ) ;
#50013 = VECTOR ( 'NONE', #26434, 1000.000000000000000 ) ;
#50014 = EDGE_CURVE ( 'NONE', #63967, #59875, #50900, .T. ) ;
#50015 = VERTEX_POINT ( 'NONE', #2717 ) ;
#50016 = DIRECTION ( 'NONE',  ( -0.000000000000000000, -0.000000000000000000, -1.000000000000000000 ) ) ;
#50017 = LINE ( 'NONE', #49655, #26036 ) ;
#50018 = CONICAL_SURFACE ( 'NONE', #8459, 2.999999999999981792, 0.7853981633974482790 ) ;
#50019 = B_SPLINE_CURVE_WITH_KNOTS ( 'NONE', 3,
 ( #24422, #45864, #39547, #61001 ),
 .UNSPECIFIED., .F., .F.,
 ( 4, 4 ),
 ( 9.900409499071532726E-07, 0.05658314289920116785 ),
 .UNSPECIFIED. ) ;
#50020 = EDGE_CURVE ( 'NONE', #34701, #39310, #13212, .T. ) ;
#50021 = CARTESIAN_POINT ( 'NONE',  ( -49.13048465129991627, 14.20828170588043626, 69.29014951661490329 ) ) ;
#50022 = CARTESIAN_POINT ( 'NONE',  ( -173.9526029538035914, 89.57590038685106038, 4.011525743166236779 ) ) ;
#50023 = CARTESIAN_POINT ( 'NONE',  ( 207.8407634284391747, 112.5209879629464211, 70.37505855668734966 ) ) ;
#50024 = CARTESIAN_POINT ( 'NONE',  ( 84.97343609940686804, 18.86260005312945864, -62.84732350933633427 ) ) ;
#50025 = VECTOR ( 'NONE', #67248, 1000.000000000000000 ) ;
#50026 = AXIS2_PLACEMENT_3D ( 'NONE', #20684, #52008, #20007 ) ;
#50027 = ORIENTED_EDGE ( 'NONE', *, *, #10389, .T. ) ;
#50028 = CARTESIAN_POINT ( 'NONE',  ( 58.09436971064712907, 11.58462396079456447, 16.14920760772560726 ) ) ;
#50029 = CIRCLE ( 'NONE', #11866, 65.36598343705435354 ) ;
#50030 = CARTESIAN_POINT ( 'NONE',  ( -62.45356936877015386, 16.79156452995241011, 63.42059391416657377 ) ) ;
#50031 = ORIENTED_EDGE ( 'NONE', *, *, #816, .T. ) ;
#50032 = FACE_OUTER_BOUND ( 'NONE', #32160, .T. ) ;
#50033 = ORIENTED_EDGE ( 'NONE', *, *, #67580, .T. ) ;
#50034 = CIRCLE ( 'NONE', #54528, 60.00000000000000000 ) ;
#50035 = CARTESIAN_POINT ( 'NONE',  ( 0.3167204509598373074, -8.479269695850863542, 1.313474075707214084 ) ) ;
#50036 = CARTESIAN_POINT ( 'NONE',  ( 10.55634918610411432, 46.66904755831205875, 0.000000000000000000 ) ) ;
#50037 = DIRECTION ( 'NONE',  ( 1.000000000000000000, 0.000000000000000000, 0.000000000000000000 ) ) ;
#50038 = EDGE_CURVE ( 'NONE', #6692, #27030, #20269, .T. ) ;
#50039 = ORIENTED_EDGE ( 'NONE', *, *, #48812, .F. ) ;
#50040 = EDGE_CURVE ( 'NONE', #43949, #56091, #40344, .T. ) ;
#50041 = EDGE_CURVE ( 'NONE', #7321, #57335, #31630, .T. ) ;
#50042 = ORIENTED_EDGE ( 'NONE', *, *, #55330, .T. ) ;
#50043 = CARTESIAN_POINT ( 'NONE',  ( 44.34689728705970424, 10.12166135033765357, 69.91849532475755780 ) ) ;
#50044 = DIRECTION ( 'NONE',  ( 1.387778780781446169E-16, -1.000000000000000000, -3.469446951953615421E-17 ) ) ;
#50045 = CYLINDRICAL_SURFACE ( 'NONE', #18205, 20.00000000000000000 ) ;
#50046 = CARTESIAN_POINT ( 'NONE',  ( 66.30230369578302430, 14.49551544185122154, 3.722485516513172499 ) ) ;
#50047 = DIRECTION ( 'NONE',  ( 0.000000000000000000, 0.000000000000000000, 1.000000000000000000 ) ) ;
#50048 = VERTEX_POINT ( 'NONE', #4442 ) ;
#50049 = B_SPLINE_CURVE_WITH_KNOTS ( 'NONE', 3,
 ( #65641, #17434, #24476, #45915, #3012, #68077, #40626, #56462, #13901, #14932, #25513, #57851, #41672, #40293, #46951, #67384, #63131, #51547, #8289, #62789, #36399, #46247, #9672, #35017, #31133, #29735, #68414, #51199, #67047, #19173, #56826, #20216, #4390, #3690, #19879, #8640, #62084, #52567, #35364, #25854, #30091, #18838, #3352, #61736, #51878, #24812 ),
 .UNSPECIFIED., .F., .F.,
 ( 4, 2, 2, 2, 2, 2, 2, 2, 2, 2, 2, 2, 2, 2, 2, 2, 2, 2, 2, 2, 2, 2, 4 ),
 ( 0.02420077021543439941, 0.02572112563160192794, 0.02648130333968567313, 0.02724148104776941831, 0.02876183646393687746, 0.02952201417202060876, 0.03028219188010434007, 0.03180254729627183391, 0.03332290271243931734, 0.03408308042052305559, 0.03484325812860678689, 0.03636361354477424951, 0.03712379125285798775, 0.03788396896094171212, 0.03864414666902545037, 0.03940432437710918168, 0.04092467979327663041, 0.04244503520944408609, 0.04396539062561154176, 0.04548574604177899744, 0.04624592374986270793, 0.04700610145794641842, 0.04852645687411387410 ),
 .UNSPECIFIED. ) ;
#50050 = FILL_AREA_STYLE ('',( #2560 ) ) ;
#50051 = CARTESIAN_POINT ( 'NONE',  ( -14.35185884954381308, 7.404296649871966451, 94.99999999999866418 ) ) ;
#50052 = CARTESIAN_POINT ( 'NONE',  ( -128.9843070188472609, 49.78011598923034597, -22.41800723653680905 ) ) ;
#50053 = CARTESIAN_POINT ( 'NONE',  ( -5.767955557622883589E-14, -26.11269837220806522, 85.00100000000000477 ) ) ;
#50054 = PLANE ( 'NONE',  #50697 ) ;
#50055 = CARTESIAN_POINT ( 'NONE',  ( 86.34144820818993082, 19.32281591521217834, 83.39973882909016822 ) ) ;
#50057 = VERTEX_POINT ( 'NONE', #3749 ) ;
#50056 = CARTESIAN_POINT ( 'NONE',  ( 0.4964154566687932202, 8.859816792613651515, -0.6543471694412406059 ) ) ;
#50058 = ORIENTED_EDGE ( 'NONE', *, *, #2276, .F. ) ;
#50059 = ORIENTED_EDGE ( 'NONE', *, *, #26188, .T. ) ;
#50060 = CARTESIAN_POINT ( 'NONE',  ( 46.42281973867198275, 9.426811321855158354, 13.21852725678505536 ) ) ;
#50061 = CARTESIAN_POINT ( 'NONE',  ( -177.9905692847866590, 94.28020182061023036, 86.29945827821053683 ) ) ;
#50062 = CARTESIAN_POINT ( 'NONE',  ( -51.78153763344961646, 13.82841714689605084, -22.63801217197542925 ) ) ;
#50063 = CARTESIAN_POINT ( 'NONE',  ( 109.7774723066848566, 28.66666416591279187, -24.07788697519002596 ) ) ;
#50064 = DIRECTION ( 'NONE',  ( -0.000000000000000000, 1.000000000000000000, -0.000000000000000000 ) ) ;
#50065 = CARTESIAN_POINT ( 'NONE',  ( -60.66101049381765620, 17.30588917955502026, -37.71267411079076481 ) ) ;
#50066 = LINE ( 'NONE', #39859, #7417 ) ;
#50067 = CARTESIAN_POINT ( 'NONE',  ( 0.000000000000000000, 65.13282190615278466, -9.999999999999998224 ) ) ;
#50068 = CARTESIAN_POINT ( 'NONE',  ( -15.27748264047829529, 7.491388194171919146, 38.59592471866675112 ) ) ;
#50069 = ORIENTED_EDGE ( 'NONE', *, *, #25667, .T. ) ;
#50070 = CONICAL_SURFACE ( 'NONE', #46698, 65.00000000000000000, 0.7853981633974497223 ) ;
#50071 = DIRECTION ( 'NONE',  ( -0.000000000000000000, 1.000000000000000000, -0.000000000000000000 ) ) ;
#50072 = ORIENTED_EDGE ( 'NONE', *, *, #12817, .F. ) ;
#50073 = VERTEX_POINT ( 'NONE', #13612 ) ;
#50074 = CARTESIAN_POINT ( 'NONE',  ( -149.5074843970971017, 65.50121172469319220, 18.87627064943540134 ) ) ;
#50075 = CIRCLE ( 'NONE', #5123, 5.000000000000018652 ) ;
#50076 = B_SPLINE_CURVE_WITH_KNOTS ( 'NONE', 3,
 ( #53981, #53645, #64562, #542, #16710, #37474, #47676, #47332, #184, #11087, #5469, #43439, #21640, #43094, #68790, #32550, #64916, #38168, #43783, #61025, #39231, #12493, #55040, #6153, #66668, #49057, #44846, #38520, #60328, #27614, #44129, #18468, #6519, #33955, #39916, #6863 ),
 .UNSPECIFIED., .F., .F.,
 ( 4, 2, 2, 2, 2, 2, 2, 2, 2, 2, 2, 2, 2, 2, 2, 2, 2, 4 ),
 ( 1.551583845779545699E-17, 0.001545474820159036195, 0.003090949640318056777, 0.004636424460477077576, 0.006181899280636097942, 0.007727374100795117440, 0.008500111510874630225, 0.009272848920954141275, 0.01081832374111319807, 0.01236379856127225660, 0.01390927338143131166, 0.01545474820159034937, 0.01700022302174938535, 0.01854569784190842133, 0.02009117266206745731, 0.02163664748222649675, 0.02318212230238552579, 0.02472759712254455136 ),
 .UNSPECIFIED. ) ;
#50077 = CARTESIAN_POINT ( 'NONE',  ( -35.41028269237559556, 11.29952379634140769, 85.03514065792309395 ) ) ;
#50078 = CARTESIAN_POINT ( 'NONE',  ( 114.6797682035589361, 32.10876583290006892, -22.64371918772569003 ) ) ;
#50079 = AXIS2_PLACEMENT_3D ( 'NONE', #21969, #11403, #54309 ) ;
#50080 = AXIS2_PLACEMENT_3D ( 'NONE', #2971, #18450, #8243 ) ;
#50081 = CARTESIAN_POINT ( 'NONE',  ( 209.3223706822284100, 18.00000000000002842, 277.8007638641562380 ) ) ;
#50082 = FACE_OUTER_BOUND ( 'NONE', #43682, .T. ) ;
#50083 = LINE ( 'NONE', #1912, #45324 ) ;
#50084 = ORIENTED_EDGE ( 'NONE', *, *, #3333, .F. ) ;
#50085 = ORIENTED_EDGE ( 'NONE', *, *, #48990, .T. ) ;
#50086 = VECTOR ( 'NONE', #63027, 1000.000000000000000 ) ;
#50087 = ORIENTED_EDGE ( 'NONE', *, *, #24481, .T. ) ;
#50088 = CARTESIAN_POINT ( 'NONE',  ( -35.00000000000002842, 225.0000000000000000, 380.0000000000000000 ) ) ;
#50089 = CARTESIAN_POINT ( 'NONE',  ( -14.92903005859421128, 7.458185427130748835, 13.18945556359724591 ) ) ;
#50090 = CARTESIAN_POINT ( 'NONE',  ( 10.00000000000000178, -31.50328976398030534, -5.000000000000000000 ) ) ;
#50091 = DIRECTION ( 'NONE',  ( -0.9115451497320358198, 0.4112000000000002875, -0.000000000000000000 ) ) ;
#50092 = B_SPLINE_CURVE_WITH_KNOTS ( 'NONE', 3,
 ( #66451, #27384, #23178, #1017, #39697, #38649, #12974, #1715, #23525, #12618, #60453, #22819, #43563, #33388, #1363, #7346, #17895, #38294, #54455, #6286, #44623, #65389, #60793, #55518, #12269, #27737, #54814, #17177, #44261, #48823, #39350, #28086, #6988, #28803, #28441, #49176, #50250, #2072, #22467, #34440, #44966, #65742, #55880, #43907, #60090 ),
 .UNSPECIFIED., .F., .F.,
 ( 4, 2, 2, 2, 2, 2, 2, 2, 2, 2, 2, 1, 2, 2, 2, 2, 2, 2, 2, 2, 2, 2, 4 ),
 ( 1.430489624538199204E-17, 0.001502898956853342561, 0.002254348435280008420, 0.003005797913706674280, 0.004508696870560044596, 0.005260146348986746885, 0.006011595827413450041, 0.007514494784266913599, 0.009017393741120378892, 0.01052029269797384245, 0.01127174217640059158, 0.01202319165482733897, 0.01277464113325408636, 0.01352609061168083202, 0.01502898956853428863, 0.01578043904696102562, 0.01653188852538776260, 0.01803478748224124004, 0.01953768643909471747, 0.02028913591752145099, 0.02104058539594818450, 0.02254348435280161683, 0.02404638330965504917 ),
 .UNSPECIFIED. ) ;
#50093 = UNCERTAINTY_MEASURE_WITH_UNIT (LENGTH_MEASURE( 1.000000000000000082E-05 ), #61431, 'distance_accuracy_value', 'NONE');
#50094 = CARTESIAN_POINT ( 'NONE',  ( -447.6627218934914367, 389.9999999999954525, 108.5502958579925235 ) ) ;
#50095 = CARTESIAN_POINT ( 'NONE',  ( 197.9843579228224542, 99.18296459057401648, 66.90814327346225809 ) ) ;
#50096 = ORIENTED_EDGE ( 'NONE', *, *, #36999, .F. ) ;
#50097 = DIRECTION ( 'NONE',  ( 1.337618101958020291E-16, 0.000000000000000000, -1.000000000000000000 ) ) ;
#50098 = CARTESIAN_POINT ( 'NONE',  ( 197.8588046850312878, 99.02485934465606476, -67.57714079882474323 ) ) ;
#50099 =( NAMED_UNIT ( * ) SI_UNIT ( $, .STERADIAN. ) SOLID_ANGLE_UNIT ( ) );
#50100 = CARTESIAN_POINT ( 'NONE',  ( -0.3732240621745021580, 7.527003275829101447, -41.93875919425514098 ) ) ;
#50101 = CARTESIAN_POINT ( 'NONE',  ( -167.3055661520540696, 80.87982228118417538, -91.14224052605258919 ) ) ;
#50102 = CARTESIAN_POINT ( 'NONE',  ( 2.905661822261151883E-14, 20.55634918610402906, 85.00100000000000477 ) ) ;
#50103 = FACE_BOUND ( 'NONE', #64472, .T. ) ;
#50104 = CARTESIAN_POINT ( 'NONE',  ( -189.3388110241866116, 107.2270502731164612, 90.85541177745594155 ) ) ;
#50105 = EDGE_CURVE ( 'NONE', #41204, #52964, #8969, .T. ) ;
#50106 = B_SPLINE_CURVE_WITH_KNOTS ( 'NONE', 3,
 ( #11165, #974, #32976, #22768 ),
 .UNSPECIFIED., .F., .F.,
 ( 4, 4 ),
 ( 0.1259919275528360583, 0.1829744153748752988 ),
 .UNSPECIFIED. ) ;
#50107 = EDGE_CURVE ( 'NONE', #51413, #8171, #21765, .T. ) ;
#50108 = ORIENTED_EDGE ( 'NONE', *, *, #3314, .F. ) ;
#50109 = DIRECTION ( 'NONE',  ( -1.000000000000000000, 0.000000000000000000, 0.000000000000000000 ) ) ;
#50110 = ADVANCED_FACE ( 'NONE', ( #27261 ), #16371, .F. ) ;
#50111 = CARTESIAN_POINT ( 'NONE',  ( -131.1078488676298832, 50.02394948559179255, -63.86183002538741960 ) ) ;
#50112 = CARTESIAN_POINT ( 'NONE',  ( -105.8683518445188412, 35.77995342500076958, -75.96225039305235782 ) ) ;
#50113 = CARTESIAN_POINT ( 'NONE',  ( 36.85262215550070408, 53.56030941157735015, 41.38025477438755928 ) ) ;
#50114 = CARTESIAN_POINT ( 'NONE',  ( 21.38432669262978436, 61.76910524360980759, 6.377659838150160580E-18 ) ) ;
#50115 = PRODUCT_DEFINITION_SHAPE ( 'NONE', 'NONE',  #69624 ) ;
#50116 = ORIENTED_EDGE ( 'NONE', *, *, #797, .T. ) ;
#50117 = DIRECTION ( 'NONE',  ( -0.8160245890732938934, -0.5780171883497599028, 0.000000000000000000 ) ) ;
#50118 = CARTESIAN_POINT ( 'NONE',  ( 181.8074882258020466, 79.33812234480652137, 83.01091592049938583 ) ) ;
#50119 = ORIENTED_EDGE ( 'NONE', *, *, #48506, .T. ) ;
#50120 = AXIS2_PLACEMENT_3D ( 'NONE', #48294, #65554, #66607 ) ;
#50121 = ORIENTED_EDGE ( 'NONE', *, *, #49704, .T. ) ;
#50122 = FACE_OUTER_BOUND ( 'NONE', #41014, .T. ) ;
#50123 = CARTESIAN_POINT ( 'NONE',  ( 151.1700480242206766, 54.15904440870137648, 40.98678080714243066 ) ) ;
#50124 = LINE ( 'NONE', #27963, #59384 ) ;
#50125 = EDGE_CURVE ( 'NONE', #38976, #6944, #16604, .T. ) ;
#50126 = ORIENTED_EDGE ( 'NONE', *, *, #3905, .F. ) ;
#50127 = CARTESIAN_POINT ( 'NONE',  ( -2.609024107869115977E-14, 3.000000000000030198, -46.99999999999997158 ) ) ;
#50128 = CIRCLE ( 'NONE', #29943, 243.4957430088094839 ) ;
#50129 = CARTESIAN_POINT ( 'NONE',  ( -178.2427210808089342, 93.01567669683338124, 5.992848471648135167 ) ) ;
#50130 = CARTESIAN_POINT ( 'NONE',  ( -75.43953471070999228, 21.11829282998124313, -49.40254329562629465 ) ) ;
#50131 = DIRECTION ( 'NONE',  ( 5.055952397801357946E-18, -6.848752866791659805E-19, -1.000000000000000000 ) ) ;
#50132 = AXIS2_PLACEMENT_3D ( 'NONE', #32203, #6143, #21294 ) ;
#50134 = CARTESIAN_POINT ( 'NONE',  ( -31.43908319763710679, 10.61114334766716283, -8.472646774738153752 ) ) ;
#50133 = VECTOR ( 'NONE', #11343, 1000.000000000000000 ) ;
#50135 = CARTESIAN_POINT ( 'NONE',  ( -48.23389383802710739, 13.99288361739331776, -19.00461935341500208 ) ) ;
#50136 = AXIS2_PLACEMENT_3D ( 'NONE', #18187, #7286, #61443 ) ;
#50137 = ORIENTED_EDGE ( 'NONE', *, *, #22704, .F. ) ;
#50138 = CARTESIAN_POINT ( 'NONE',  ( 9.372831690575286860E-16, 1.117010584002392767E-15, -17.00000000000000000 ) ) ;
#50139 = CARTESIAN_POINT ( 'NONE',  ( -74.18622060908363380, 21.73430079572372975, 5.039450213261992495 ) ) ;
#50140 = LINE ( 'NONE', #3675, #4595 ) ;
#50141 = CARTESIAN_POINT ( 'NONE',  ( 0.000000000000000000, 0.000000000000000000, 170.0000000000000000 ) ) ;
#50143 = ORIENTED_EDGE ( 'NONE', *, *, #2324, .F. ) ;
#50142 = DIRECTION ( 'NONE',  ( -0.000000000000000000, 1.000000000000000000, -0.000000000000000000 ) ) ;
#50144 = CARTESIAN_POINT ( 'NONE',  ( 83.60262962804350195, 18.41036205028015971, -50.18795455408093176 ) ) ;
#50145 = ORIENTED_EDGE ( 'NONE', *, *, #39019, .T. ) ;
#50146 = CARTESIAN_POINT ( 'NONE',  ( -145.5261806899007127, 60.87473129144529338, 58.70511779414287190 ) ) ;
#50147 = CARTESIAN_POINT ( 'NONE',  ( 84.74089592029041285, 19.84571403269344714, 29.94973715047667540 ) ) ;
#50148 = CARTESIAN_POINT ( 'NONE',  ( -78.66644367742109978, 22.32174330031319442, 30.41820113967310490 ) ) ;
#50149 = DIRECTION ( 'NONE',  ( -0.000000000000000000, -0.000000000000000000, 1.000000000000000000 ) ) ;
#50150 = CARTESIAN_POINT ( 'NONE',  ( -119.5576859660651223, 42.46117483543970650, 60.94340854921288297 ) ) ;
#50151 = DIRECTION ( 'NONE',  ( -0.7530714660036099684, -0.6579387259397138088, 0.000000000000000000 ) ) ;
#50152 = CARTESIAN_POINT ( 'NONE',  ( -174.7903139851460139, 90.53182997092832807, -8.043439406538249514 ) ) ;
#50153 = CARTESIAN_POINT ( 'NONE',  ( 46.39999999999999858, 0.000000000000000000, 0.000000000000000000 ) ) ;
#50154 = ORIENTED_EDGE ( 'NONE', *, *, #36771, .F. ) ;
#50155 = ORIENTED_EDGE ( 'NONE', *, *, #12502, .T. ) ;
#50156 = CARTESIAN_POINT ( 'NONE',  ( 45.49006904354233427, 9.279592366778889101, 33.02688758334598873 ) ) ;
#50157 = CARTESIAN_POINT ( 'NONE',  ( 197.3054165770395514, 96.72615186924552688, -18.28925989677753350 ) ) ;
#50158 = CARTESIAN_POINT ( 'NONE',  ( -36.11269837220806522, 5.594483210025202879E-14, 0.000000000000000000 ) ) ;
#50159 = CARTESIAN_POINT ( 'NONE',  ( -11.97857133224687409, 31.20571980842448667, 6.893343212288939093 ) ) ;
#50160 = CARTESIAN_POINT ( 'NONE',  ( 210.9631450001600967, 117.1791136960929833, -47.98552383177344183 ) ) ;
#50161 = EDGE_CURVE ( 'NONE', #23252, #56240, #32896, .T. ) ;
#50162 = CARTESIAN_POINT ( 'NONE',  ( -71.27103490383373696, 20.70545763375144688, -68.18631899798461404 ) ) ;
#50163 = CARTESIAN_POINT ( 'NONE',  ( -104.1342612728951877, 33.73231160250195160, 57.58144852683274451 ) ) ;
#50164 = CARTESIAN_POINT ( 'NONE',  ( -30.94753041835914686, 9.510749728915504519, -35.31719736520183517 ) ) ;
#50165 = CARTESIAN_POINT ( 'NONE',  ( 164.7167608259061637, 63.51199216609074227, -72.42214042571447408 ) ) ;
#50166 = PRODUCT_DEFINITION_SHAPE ( 'NONE', 'NONE',  #69608 ) ;
#50167 = ORIENTED_EDGE ( 'NONE', *, *, #22642, .T. ) ;
#50168 = ORIENTED_EDGE ( 'NONE', *, *, #50642, .F. ) ;
#50169 = VECTOR ( 'NONE', #21760, 1000.000000000000000 ) ;
#50170 = FACE_OUTER_BOUND ( 'NONE', #654, .T. ) ;
#50171 = FACE_OUTER_BOUND ( 'NONE', #11614, .T. ) ;
#50172 = LINE ( 'NONE', #50863, #38575 ) ;
#50173 = CARTESIAN_POINT ( 'NONE',  ( 126.8114659053432263, 38.48351437375815465, 34.38739146146416203 ) ) ;
#50174 = CARTESIAN_POINT ( 'NONE',  ( 109.6700404598697958, -21.42428528562852819, -5.000000000000006217 ) ) ;
#50175 = VECTOR ( 'NONE', #26392, 1000.000000000000000 ) ;
#50176 = CARTESIAN_POINT ( 'NONE',  ( -15.47041015649551809, -73.39774458108233546, 43.58025477438756923 ) ) ;
#50177 = CARTESIAN_POINT ( 'NONE',  ( -97.88021438939448160, 31.71889184683104190, -9.577608110017886034 ) ) ;
#50178 = CIRCLE ( 'NONE', #59145, 65.00000000000000000 ) ;
#50179 = CARTESIAN_POINT ( 'NONE',  ( 58.47885130911550533, 12.69429933094348684, 31.32040142421980278 ) ) ;
#50180 = CARTESIAN_POINT ( 'NONE',  ( 44.99999999999999289, 20.00000000000000355, 2.000000000000015543 ) ) ;
#50181 = ORIENTED_EDGE ( 'NONE', *, *, #3415, .T. ) ;
#50182 = ORIENTED_EDGE ( 'NONE', *, *, #66972, .F. ) ;
#50183 = CARTESIAN_POINT ( 'NONE',  ( 55.77012379229940109, 12.13428856597101024, 66.11046144963563620 ) ) ;
#50184 = CARTESIAN_POINT ( 'NONE',  ( 313.9975424824652350, 18.00000000000002842, 401.6295345748407613 ) ) ;
#50185 = ADVANCED_FACE ( 'NONE', ( #25904, #36802 ), #21993, .F. ) ;
#50186 = CARTESIAN_POINT ( 'NONE',  ( 284.3366674800922169, -21.85806848808613267, 2.509805449638021990 ) ) ;
#50187 = CARTESIAN_POINT ( 'NONE',  ( 203.1420903260746229, 104.2307086582027438, 70.93374687166461001 ) ) ;
#50188 = EDGE_CURVE ( 'NONE', #42236, #55222, #40223, .T. ) ;
#50189 = CARTESIAN_POINT ( 'NONE',  ( -96.89229402469325692, 30.12691466369447468, -90.96714292758291265 ) ) ;
#50190 = VECTOR ( 'NONE', #1344, 1000.000000000000000 ) ;
#50191 = ORIENTED_EDGE ( 'NONE', *, *, #32132, .T. ) ;
#50192 = CARTESIAN_POINT ( 'NONE',  ( 658.0910129007216938, 1005.848388255940336, 749.5068267248711891 ) ) ;
#50193 = EDGE_CURVE ( 'NONE', #54158, #53910, #48351, .T. ) ;
#50194 = CARTESIAN_POINT ( 'NONE',  ( -189.2739965869454011, 107.1373753350176656, -16.14596922345551278 ) ) ;
#50195 = CARTESIAN_POINT ( 'NONE',  ( -38.92718193365330848, 11.96647478777219753, -42.32783819707668016 ) ) ;
#50196 = CARTESIAN_POINT ( 'NONE',  ( -165.6404838346739155, 80.60836113891892296, -41.59413812189578863 ) ) ;
#50197 = ITEM_DEFINED_TRANSFORMATION ( 'NONE', 'NONE', #33267,  #66832 ) ;
#50198 = CARTESIAN_POINT ( 'NONE',  ( -166.7504005514883829, 80.30621656552872878, 88.03983344583103587 ) ) ;
#50199 = VERTEX_POINT ( 'NONE', #10392 ) ;
#50200 = CARTESIAN_POINT ( 'NONE',  ( -118.7011677090247161, 41.93687969120208692, -44.55502681419259403 ) ) ;
#50201 = CARTESIAN_POINT ( 'NONE',  ( -58.20343000000241318, -3.983351041215688504, 27.58472315868180402 ) ) ;
#50202 = CARTESIAN_POINT ( 'NONE',  ( -142.3393481102175429, 58.33014244976923379, -17.69161782318237996 ) ) ;
#50203 = CARTESIAN_POINT ( 'NONE',  ( -2.177337698256110787, 7.595833446947581002, -64.80389893477351393 ) ) ;
#50204 = DIRECTION ( 'NONE',  ( -0.000000000000000000, -0.000000000000000000, 1.000000000000000000 ) ) ;
#50205 = ADVANCED_FACE ( 'NONE', ( #10743 ), #5807, .F. ) ;
#50206 = EDGE_LOOP ( 'NONE', ( #51182, #15438, #11490, #58461 ) ) ;
#50207 = CARTESIAN_POINT ( 'NONE',  ( 161.9743715636469119, 62.54005768132974197, -91.30411002385437769 ) ) ;
#50208 = CARTESIAN_POINT ( 'NONE',  ( 199.7278513351970446, 99.76879341361768638, -38.18984482819509196 ) ) ;
#50209 = B_SPLINE_CURVE_WITH_KNOTS ( 'NONE', 3,
 ( #33687, #45262, #27689, #38600, #60042, #39646, #50548, #55117, #49130, #49835, #60748, #11861, #973, #1661, #33339, #2367, #23125, #7650, #22420, #50200, #44575, #66052, #17847, #29101, #12568, #54408, #61104, #54764, #1314, #55469, #28041, #49481, #7292, #12927, #55830, #66748, #18539, #39991, #61450, #31762, #69030, #67097, #53194, #26143, #5022, #24172 ),
 .UNSPECIFIED., .F., .F.,
 ( 4, 2, 2, 2, 2, 2, 2, 2, 2, 2, 2, 2, 2, 2, 2, 2, 2, 2, 2, 2, 2, 2, 4 ),
 ( 0.02584318557310393699, 0.02743529570732771566, 0.02823135077443958418, 0.02902740584155144923, 0.03061951597577517933, 0.03221162610999891290, 0.03380373624422264300, 0.03459979131133449071, 0.03539584637844634535, 0.03619190144555819305, 0.03698795651267004075, 0.03858006664689374310, 0.03937612171400560468, 0.04017217678111746626, 0.04096823184822932784, 0.04176428691534118942, 0.04335639704956491258, 0.04494850718378863574, 0.04654061731801235891, 0.04813272745223608207, 0.04892878251934794365, 0.04972483758645979829, 0.05131694772068349369 ),
 .UNSPECIFIED. ) ;
#50210 = LINE ( 'NONE', #2036, #20658 ) ;
#50211 = EDGE_CURVE ( 'NONE', #3111, #68404, #50076, .T. ) ;
#50212 = EDGE_CURVE ( 'NONE', #48110, #33531, #45794, .T. ) ;
#50213 = EDGE_CURVE ( 'NONE', #59106, #32147, #67160, .T. ) ;
#50214 = CARTESIAN_POINT ( 'NONE',  ( 22.53041628628730209, 6.810083298012985509, -39.69690971090911802 ) ) ;
#50216 = ORIENTED_EDGE ( 'NONE', *, *, #67855, .F. ) ;
#50215 = CARTESIAN_POINT ( 'NONE',  ( 113.8626313173126334, 31.71036178495294067, 16.85260883570550661 ) ) ;
#50217 = CARTESIAN_POINT ( 'NONE',  ( 62.53328835682437159, 12.56090025569837287, 29.81296093922127710 ) ) ;
#50218 = ORIENTED_EDGE ( 'NONE', *, *, #62047, .F. ) ;
#50219 = ORIENTED_EDGE ( 'NONE', *, *, #18927, .T. ) ;
#50220 = AXIS2_PLACEMENT_3D ( 'NONE', #59406, #680, #54466 ) ;
#50221 = CARTESIAN_POINT ( 'NONE',  ( 177.7964363391244547, 76.75162026635251777, 30.05250232064427252 ) ) ;
#50222 = CARTESIAN_POINT ( 'NONE',  ( -38.26251837371328435, 11.83628080764031409, -93.36397248376952973 ) ) ;
#50223 = VECTOR ( 'NONE', #19291, 999.9999999999998863 ) ;
#50225 = ORIENTED_EDGE ( 'NONE', *, *, #56532, .T. ) ;
#50224 = FACE_OUTER_BOUND ( 'NONE', #16702, .T. ) ;
#50226 = LINE ( 'NONE', #23501, #35314 ) ;
#50227 = CARTESIAN_POINT ( 'NONE',  ( -24.18270484670773968, 9.527492911955594224, 39.67658164943471633 ) ) ;
#50228 = CARTESIAN_POINT ( 'NONE',  ( -73.63128929564828695, 21.53548093502884342, -37.05148811347594773 ) ) ;
#50229 = AXIS2_PLACEMENT_3D ( 'NONE', #47254, #36025, #20879 ) ;
#50230 = ORIENTED_EDGE ( 'NONE', *, *, #42026, .T. ) ;
#50231 = VECTOR ( 'NONE', #12811, 1000.000000000000000 ) ;
#50232 = CARTESIAN_POINT ( 'NONE',  ( 177.6874527215932176, 76.64335277577062300, -90.68412946948107844 ) ) ;
#50233 = AXIS2_PLACEMENT_3D ( 'NONE', #5414, #65553, #22282 ) ;
#50234 = LINE ( 'NONE', #34057, #6116 ) ;
#50235 = CARTESIAN_POINT ( 'NONE',  ( -177.5288247523078553, 93.72924674643513754, 44.40754021158874565 ) ) ;
#50236 = DIRECTION ( 'NONE',  ( -0.000000000000000000, -0.000000000000000000, -1.000000000000000000 ) ) ;
#50237 = CARTESIAN_POINT ( 'NONE',  ( 54.03875030502680943, 0.000000000000000000, 2.000000000000001776 ) ) ;
#50238 = ORIENTED_EDGE ( 'NONE', *, *, #42258, .F. ) ;
#50239 = ORIENTED_EDGE ( 'NONE', *, *, #4379, .F. ) ;
#50240 = ORIENTED_EDGE ( 'NONE', *, *, #5268, .F. ) ;
#50241 = CARTESIAN_POINT ( 'NONE',  ( 63.01563776193091826, -170.0000000000000000, -23.87614024170608218 ) ) ;
#50242 = CARTESIAN_POINT ( 'NONE',  ( 21.27121078971612889, 61.42097029141972087, 133.5802547743875550 ) ) ;
#50243 = CARTESIAN_POINT ( 'NONE',  ( -38.26497993382595553, 10.81185389040525635, -39.69992527180441755 ) ) ;
#50244 = ADVANCED_FACE ( 'NONE', ( #34306 ), #11783, .F. ) ;
#50245 = CARTESIAN_POINT ( 'NONE',  ( -94.87314045600119528, 29.17466428498257969, 90.48494885821429534 ) ) ;
#50246 = CARTESIAN_POINT ( 'NONE',  ( -149.0782809666403637, 63.81577337591401289, 30.72082123989905256 ) ) ;
#50247 = CARTESIAN_POINT ( 'NONE',  ( 0.000000000000000000, 0.000000000000000000, -7.000000000000000000 ) ) ;
#50248 = CARTESIAN_POINT ( 'NONE',  ( -76.32456871438913026, 22.51591205926310124, -22.91205146820279026 ) ) ;
#50249 = ORIENTED_EDGE ( 'NONE', *, *, #66286, .F. ) ;
#50250 = CARTESIAN_POINT ( 'NONE',  ( 82.74007713545063325, 18.13042311233563098, 57.63927396060999797 ) ) ;
#50251 = ORIENTED_EDGE ( 'NONE', *, *, #67425, .T. ) ;
#50252 = EDGE_CURVE ( 'NONE', #7475, #42734, #33612, .T. ) ;
#50253 = CARTESIAN_POINT ( 'NONE',  ( 35.44781468922822398, 7.928097401423699786, 31.03618968133934430 ) ) ;
#50254 = DIRECTION ( 'NONE',  ( -0.000000000000000000, 1.000000000000000000, -0.000000000000000000 ) ) ;
#50255 = ORIENTED_EDGE ( 'NONE', *, *, #54212, .T. ) ;
#50256 = CYLINDRICAL_SURFACE ( 'NONE', #43081, 30.00000000000000000 ) ;
#50257 = CYLINDRICAL_SURFACE ( 'NONE', #57954, 5.000000000000000888 ) ;
#50258 = CARTESIAN_POINT ( 'NONE',  ( 8.390996311772816796, 10.00000000000000000, -17.00000000000000000 ) ) ;
#50259 = DIRECTION ( 'NONE',  ( 1.000000000000000000, 0.000000000000000000, 0.000000000000000000 ) ) ;
#50260 = CARTESIAN_POINT ( 'NONE',  ( -47.80896875121164413, 12.85816703949531536, 12.93218738431712289 ) ) ;
#50261 = PLANE ( 'NONE',  #47225 ) ;
#50262 = CARTESIAN_POINT ( 'NONE',  ( -36.11269837220801548, 31.11269837220812207, 85.00100000000000477 ) ) ;
#50263 = ORIENTED_EDGE ( 'NONE', *, *, #65270, .T. ) ;
#50264 = AXIS2_PLACEMENT_3D ( 'NONE', #60918, #50016, #2192 ) ;
#50265 = DIRECTION ( 'NONE',  ( -0.000000000000000000, 1.000000000000000000, -0.000000000000000000 ) ) ;
#50266 = DIRECTION ( 'NONE',  ( -0.5877852522924802425, 0.8090169943749422332, 0.000000000000000000 ) ) ;
#50267 = VERTEX_POINT ( 'NONE', #17050 ) ;
#50268 = CARTESIAN_POINT ( 'NONE',  ( -64.18058723658640474, -10.37664328995270857, 43.58025477438756923 ) ) ;
#50269 = CARTESIAN_POINT ( 'NONE',  ( 63.01563776193090405, 13.70579113808098271, -35.72069083216973695 ) ) ;
#50270 = FACE_OUTER_BOUND ( 'NONE', #2436, .T. ) ;
#50271 = ORIENTED_EDGE ( 'NONE', *, *, #67745, .F. ) ;
#50272 = EDGE_CURVE ( 'NONE', #60501, #3562, #28985, .T. ) ;
#50273 = CARTESIAN_POINT ( 'NONE',  ( 0.000000000000000000, 0.000000000000000000, 30.00000000000000000 ) ) ;
#50274 = CARTESIAN_POINT ( 'NONE',  ( 152.1153500913667642, 54.85403770686892955, -65.21174665958072580 ) ) ;
#50275 = CARTESIAN_POINT ( 'NONE',  ( -38.26497993382596263, 10.81185389040525635, 40.83372649958661782 ) ) ;
#50276 = EDGE_CURVE ( 'NONE', #14895, #15856, #22345, .T. ) ;
#50277 = VECTOR ( 'NONE', #34543, 1000.000000000000000 ) ;
#50278 = CARTESIAN_POINT ( 'NONE',  ( 141.2894128405439176, 46.09731134920846074, -42.48579671950618319 ) ) ;
#50279 = APPLICATION_CONTEXT ( 'automotive_design' ) ;
#50280 = EDGE_CURVE ( 'NONE', #20254, #32779, #39574, .T. ) ;
#50281 = VECTOR ( 'NONE', #40574, 1000.000000000000000 ) ;
#50282 = VERTEX_POINT ( 'NONE', #28673 ) ;
#50283 = CARTESIAN_POINT ( 'NONE',  ( 41.66904755831208007, -10.55634918610412853, 0.000000000000000000 ) ) ;
#50284 = AXIS2_PLACEMENT_3D ( 'NONE', #29981, #66594, #34589 ) ;
#50285 = VERTEX_POINT ( 'NONE', #27966 ) ;
#50286 = CARTESIAN_POINT ( 'NONE',  ( -17.90772993695113868, 72.84144224619130625, 170.0000000000000000 ) ) ;
#50287 = LINE ( 'NONE', #55198, #41696 ) ;
#50288 = CARTESIAN_POINT ( 'NONE',  ( 10.55634918610397577, -31.11269837220809364, 0.000000000000000000 ) ) ;
#50289 = CARTESIAN_POINT ( 'NONE',  ( 141.2920930135741173, 47.30245445423356898, 91.74529553920554292 ) ) ;
#50290 = AXIS2_PLACEMENT_3D ( 'NONE', #42933, #64400, #54883 ) ;
#50291 = CARTESIAN_POINT ( 'NONE',  ( -29.87147652227456263, 100.0000000000000000, 73.58025477438756923 ) ) ;
#50292 = AXIS2_PLACEMENT_3D ( 'NONE', #41925, #36656, #3954 ) ;
#50293 = CARTESIAN_POINT ( 'NONE',  ( 8.000000000000000000, 0.7809653281576085515, 9.452887691357987840E-16 ) ) ;
#50294 = ORIENTED_EDGE ( 'NONE', *, *, #65858, .T. ) ;
#50295 = CARTESIAN_POINT ( 'NONE',  ( 164.7167608259061922, 63.51199216609071385, -18.73303924478714677 ) ) ;
#50296 = DIRECTION ( 'NONE',  ( -0.000000000000000000, -0.000000000000000000, -1.000000000000000000 ) ) ;
#50297 = CARTESIAN_POINT ( 'NONE',  ( 61.91366885787727625, 28.42865614899003290, 170.0000000000000000 ) ) ;
#50298 = CARTESIAN_POINT ( 'NONE',  ( 141.0804878838241336, 45.96076546397620177, -68.28228989354154521 ) ) ;
#50299 = DIRECTION ( 'NONE',  ( -1.000000000000000000, 0.000000000000000000, 0.000000000000000000 ) ) ;
#50300 = EDGE_CURVE ( 'NONE', #5640, #42425, #49411, .T. ) ;
#50301 = ADVANCED_FACE ( 'NONE', ( #34662 ), #1955, .F. ) ;
#50302 = ORIENTED_EDGE ( 'NONE', *, *, #60618, .T. ) ;
#50303 = EDGE_CURVE ( 'NONE', #4364, #27445, #10980, .T. ) ;
#50304 = CARTESIAN_POINT ( 'NONE',  ( 161.7006237583813970, 62.31514460450500792, -22.98982369199385900 ) ) ;
#50305 = CARTESIAN_POINT ( 'NONE',  ( 13.84937401517046851, 6.446378549072247388, 44.76393167428260256 ) ) ;
#50306 = ORIENTED_EDGE ( 'NONE', *, *, #47260, .F. ) ;
#50307 = CARTESIAN_POINT ( 'NONE',  ( -61.86403937395562025, 16.61416349803656090, -66.41162500208781694 ) ) ;
#50308 = FACE_OUTER_BOUND ( 'NONE', #21868, .T. ) ;
#50309 = ORIENTED_EDGE ( 'NONE', *, *, #53757, .T. ) ;
#50310 = CARTESIAN_POINT ( 'NONE',  ( 163.7379901688713062, 64.00402364591248272, -39.49700036984320661 ) ) ;
#50311 = CARTESIAN_POINT ( 'NONE',  ( 93.63037639125411715, 21.92981100938040484, 13.06913551750571756 ) ) ;
#50312 = CARTESIAN_POINT ( 'NONE',  ( 164.4728833318992542, 63.30716077995680990, -40.92446310325109948 ) ) ;
#50313 = EDGE_LOOP ( 'NONE', ( #9503, #23705, #24097, #18561 ) ) ;
#50314 = AXIS2_PLACEMENT_3D ( 'NONE', #22081, #27346, #31599 ) ;
#50315 = CARTESIAN_POINT ( 'NONE',  ( -95.05323930133207000, 30.36974142673411947, 13.24519497187949391 ) ) ;
#50316 = DIRECTION ( 'NONE',  ( 0.000000000000000000, 0.000000000000000000, -1.000000000000000000 ) ) ;
#50317 = AXIS2_PLACEMENT_3D ( 'NONE', #44823, #50097, #29679 ) ;
#50318 = B_SPLINE_CURVE_WITH_KNOTS ( 'NONE', 3,
 ( #9100, #30548, #30898, #10123 ),
 .UNSPECIFIED., .F., .F.,
 ( 4, 4 ),
 ( 0.1259919275528358362, 0.1829744153748746882 ),
 .UNSPECIFIED. ) ;
#50319 = CARTESIAN_POINT ( 'NONE',  ( 32.90051628396145844, 8.664124555952449569, 33.64247275619753452 ) ) ;
#50320 = CARTESIAN_POINT ( 'NONE',  ( -178.2448732545371115, 94.58403736950705820, -36.71535872372318465 ) ) ;
#50321 = CARTESIAN_POINT ( 'NONE',  ( -179.3508319071551966, 95.92102653685060432, -91.71737262036411664 ) ) ;
#50322 = CARTESIAN_POINT ( 'NONE',  ( 153.2384531768735769, 54.43344429203621360, 69.96338799158385768 ) ) ;
#50323 = CARTESIAN_POINT ( 'NONE',  ( 127.2202105166096402, 37.55913282978156076, -73.87116003439983558 ) ) ;
#50324 = ORIENTED_EDGE ( 'NONE', *, *, #11098, .F. ) ;
#50325 = CARTESIAN_POINT ( 'NONE',  ( 141.0517870458593563, 47.14452711594498879, -68.23502628271137382 ) ) ;
#50326 = AXIS2_PLACEMENT_3D ( 'NONE', #13348, #19300, #8058 ) ;
#50327 = CARTESIAN_POINT ( 'NONE',  ( -11.78188048797445475, 8.190559674012726887, 58.08383411553590037 ) ) ;
#50328 = ORIENTED_EDGE ( 'NONE', *, *, #53282, .T. ) ;
#50329 = CARTESIAN_POINT ( 'NONE',  ( -156.0204364459165163, 71.27041535366187475, -38.58461829599199433 ) ) ;
#50330 = VECTOR ( 'NONE', #56628, 1000.000000000000000 ) ;
#50331 = CARTESIAN_POINT ( 'NONE',  ( -0.2498518736781690786, 33.42485144267424602, 6.893343212288930211 ) ) ;
#50332 = CARTESIAN_POINT ( 'NONE',  ( -38.68632430131781774, 11.91908191268690942, 39.66289844268187892 ) ) ;
#50333 = DIRECTION ( 'NONE',  ( 0.000000000000000000, -1.000000000000000000, 0.000000000000000000 ) ) ;
#50334 = CARTESIAN_POINT ( 'NONE',  ( -2.177337698256109455, 7.595833446947581002, 42.57430342708116910 ) ) ;
#50335 = CARTESIAN_POINT ( 'NONE',  ( -14.65035343718723482, 7.431577370124334614, -93.38227200523709826 ) ) ;
#50336 = DIRECTION ( 'NONE',  ( 0.000000000000000000, 0.000000000000000000, -1.000000000000000000 ) ) ;
#50337 = CARTESIAN_POINT ( 'NONE',  ( -3.862560291631539133, 7.672660553664873540, -22.44576929375073604 ) ) ;
#50338 = CARTESIAN_POINT ( 'NONE',  ( -9.779603649692299783, 8.034615131607074190, 44.87335778418307086 ) ) ;
#50339 = CARTESIAN_POINT ( 'NONE',  ( 113.4493678088378203, 30.39339414805072792, 17.06312677987657622 ) ) ;
#50340 = CARTESIAN_POINT ( 'NONE',  ( -20.55634918610405748, -15.55634918610400774, 0.000000000000000000 ) ) ;
#50341 = EDGE_LOOP ( 'NONE', ( #2538, #57643, #8886, #6253 ) ) ;
#50342 = VECTOR ( 'NONE', #61595, 1000.000000000000000 ) ;
#50343 = ADVANCED_FACE ( 'NONE', ( #18121 ), #38884, .F. ) ;
#50344 = CARTESIAN_POINT ( 'NONE',  ( 0.000000000000000000, 0.000000000000000000, 0.000000000000000000 ) ) ;
#50345 = ORIENTED_EDGE ( 'NONE', *, *, #4327, .T. ) ;
#50346 = CARTESIAN_POINT ( 'NONE',  ( 102.7551177910568327, 25.56939188780866345, -70.76452187158794516 ) ) ;
#50347 = CARTESIAN_POINT ( 'NONE',  ( 45.35621884287174765, 10.27694987765648449, -20.86182146456972930 ) ) ;
#50348 = CARTESIAN_POINT ( 'NONE',  ( 46.50704915687940399, 9.440294391580033917, 66.67262751023041289 ) ) ;
#50349 = DIRECTION ( 'NONE',  ( -1.000000000000000000, 0.000000000000000000, 0.000000000000000000 ) ) ;
#50350 = DIRECTION ( 'NONE',  ( 0.000000000000000000, -1.000000000000000000, 0.000000000000000000 ) ) ;
#50351 = DIRECTION ( 'NONE',  ( -1.000000000000000000, -0.000000000000000000, -0.000000000000000000 ) ) ;
#50352 = CARTESIAN_POINT ( 'NONE',  ( -78.66644367742111399, 22.32174330031318377, 57.26275173013680586 ) ) ;
#50353 = FACE_BOUND ( 'NONE', #8554, .T. ) ;
#50354 = ORIENTED_EDGE ( 'NONE', *, *, #62889, .F. ) ;
#50355 = ORIENTED_EDGE ( 'NONE', *, *, #62408, .F. ) ;
#50356 = EDGE_CURVE ( 'NONE', #47218, #8003, #55940, .T. ) ;
#50357 = CARTESIAN_POINT ( 'NONE',  ( -15.55634918610405748, -15.55634918610400774, 2.000000000000001776 ) ) ;
#50358 = CARTESIAN_POINT ( 'NONE',  ( 175.3815143714021758, 73.02838262207001208, 68.53128429288518930 ) ) ;
#50359 = LINE ( 'NONE', #60204, #1976 ) ;
#50360 = CARTESIAN_POINT ( 'NONE',  ( 109.7732660198864494, 29.77277639096405792, 71.45576479620105204 ) ) ;
#50361 = EDGE_CURVE ( 'NONE', #28307, #49946, #45191, .T. ) ;
#50362 = CARTESIAN_POINT ( 'NONE',  ( -165.6208371326873703, 80.58821715390998008, -15.66524306475966455 ) ) ;
#50363 = EDGE_CURVE ( 'NONE', #192, #19283, #50816, .T. ) ;
#50364 = EDGE_CURVE ( 'NONE', #35065, #38023, #40265, .T. ) ;
#50365 = DIRECTION ( 'NONE',  ( 0.000000000000000000, 0.000000000000000000, 1.000000000000000000 ) ) ;
#50366 = ORIENTED_EDGE ( 'NONE', *, *, #20334, .F. ) ;
#50367 = EDGE_CURVE ( 'NONE', #44993, #50858, #41308, .T. ) ;
#50368 = CARTESIAN_POINT ( 'NONE',  ( 90.51709546286271291, 21.85407654229980423, 3.949318351511905689 ) ) ;
#50369 = FACE_OUTER_BOUND ( 'NONE', #42955, .T. ) ;
#50370 = CARTESIAN_POINT ( 'NONE',  ( 181.0840389613909736, 78.60582251573005408, -51.22505766587963905 ) ) ;
#50371 = CYLINDRICAL_SURFACE ( 'NONE', #21786, 7.500000000000013323 ) ;
#50372 = CARTESIAN_POINT ( 'NONE',  ( 99.99999999999997158, 6.000000000000000000, -25.00000000000000000 ) ) ;
#50373 = FACE_BOUND ( 'NONE', #41239, .T. ) ;
#50374 = VECTOR ( 'NONE', #61862, 1000.000000000000000 ) ;
#50375 = ORIENTED_EDGE ( 'NONE', *, *, #19457, .T. ) ;
#50376 = CIRCLE ( 'NONE', #29045, 200.0000000000000000 ) ;
#50377 = CARTESIAN_POINT ( 'NONE',  ( 1.667562369267789890, -64.99262834925670518, 170.0000000000000000 ) ) ;
#50378 = FACE_OUTER_BOUND ( 'NONE', #43513, .T. ) ;
#50379 = CARTESIAN_POINT ( 'NONE',  ( 15.55634918610403261, 4.999999999999969802, 85.00100000000000477 ) ) ;
#50380 = CARTESIAN_POINT ( 'NONE',  ( -179.2128128997734393, 95.75254520622991095, 7.073590364011439924 ) ) ;
#50381 = DIRECTION ( 'NONE',  ( -1.000000000000000000, 0.000000000000000000, 0.000000000000000000 ) ) ;
#50382 = CARTESIAN_POINT ( 'NONE',  ( 85.67452303415197434, 19.09699411916384904, -62.71192339984101238 ) ) ;
#50383 = MECHANICAL_DESIGN_GEOMETRIC_PRESENTATION_REPRESENTATION (  '', ( #26819 ), #2130 ) ;
#50384 = EDGE_LOOP ( 'NONE', ( #26763, #53555, #65758, #39779 ) ) ;
#50385 = ADVANCED_FACE ( 'NONE', ( #3665 ), #24448, .F. ) ;
#50386 = FACE_OUTER_BOUND ( 'NONE', #50961, .T. ) ;
#50387 = CARTESIAN_POINT ( 'NONE',  ( 199.3764470687682149, 100.9548044849098716, -38.53510737021463228 ) ) ;
#50388 = EDGE_LOOP ( 'NONE', ( #25847, #69079, #29728, #32288 ) ) ;
#50389 = DIRECTION ( 'NONE',  ( -0.000000000000000000, 0.000000000000000000, -1.000000000000000000 ) ) ;
#50390 = VERTEX_POINT ( 'NONE', #13871 ) ;
#50391 = DIRECTION ( 'NONE',  ( -0.000000000000000000, -0.000000000000000000, 1.000000000000000000 ) ) ;
#50392 = CARTESIAN_POINT ( 'NONE',  ( -447.6627218934912662, 369.9999999999998295, 113.5502958579880328 ) ) ;
#50393 = CARTESIAN_POINT ( 'NONE',  ( 94.11595392909974578, 23.18887043179184815, -69.65182159334985101 ) ) ;
#50394 = EDGE_LOOP ( 'NONE', ( #7285, #55495 ) ) ;
#50395 = ORIENTED_EDGE ( 'NONE', *, *, #47480, .T. ) ;
#50396 = CARTESIAN_POINT ( 'NONE',  ( 40.38132770291768736, 9.553709436640062336, 71.71008232015611839 ) ) ;
#50397 = CARTESIAN_POINT ( 'NONE',  ( -173.1211646369891355, 88.63826465341151106, 57.66624519710472185 ) ) ;
#50398 = FACE_OUTER_BOUND ( 'NONE', #39365, .T. ) ;
#50399 = CARTESIAN_POINT ( 'NONE',  ( 447.3372781065085633, 399.9999999999998863, 113.5502958579881891 ) ) ;
#50400 = ORIENTED_EDGE ( 'NONE', *, *, #61538, .F. ) ;
#50401 = CARTESIAN_POINT ( 'NONE',  ( 65.13282190615461786, 1.839221433318906476E-12, 5.000000000000000000 ) ) ;
#50402 = CARTESIAN_POINT ( 'NONE',  ( -51.77431913897918747, 14.86466849149170955, 17.73581465740154428 ) ) ;
#50403 = CARTESIAN_POINT ( 'NONE',  ( -133.2787743207940707, 52.78950725740543248, -14.23327279590464833 ) ) ;
#50404 = CARTESIAN_POINT ( 'NONE',  ( -156.7429055738855936, 71.93655028710443844, -93.96263355926134864 ) ) ;
#50405 = CARTESIAN_POINT ( 'NONE',  ( 111.8699272271189358, 29.64190505307780654, -23.90307673515284037 ) ) ;
#50406 = CARTESIAN_POINT ( 'NONE',  ( 87.31198329270952740, 19.65488789718978069, 83.42517577981676880 ) ) ;
#50408 = ORIENTED_EDGE ( 'NONE', *, *, #30355, .F. ) ;
#50407 = CYLINDRICAL_SURFACE ( 'NONE', #43275, 5.000000000000004441 ) ;
#50409 = ORIENTED_EDGE ( 'NONE', *, *, #65618, .F. ) ;
#50410 = VERTEX_POINT ( 'NONE', #25138 ) ;
#50411 = DIRECTION ( 'NONE',  ( 1.000000000000000000, 0.000000000000000000, -0.000000000000000000 ) ) ;
#50412 = CARTESIAN_POINT ( 'NONE',  ( -4.364688291132434728, -24.74039788130350459, 3.061616997868437868E-16 ) ) ;
#50413 = CARTESIAN_POINT ( 'NONE',  ( -74.99999999999998579, 0.000000000000000000, 25.00000000000007816 ) ) ;
#50414 = CARTESIAN_POINT ( 'NONE',  ( 107.0477776024378898, 27.43148174916616355, -23.36746922899289558 ) ) ;
#50415 = CARTESIAN_POINT ( 'NONE',  ( 140.8935642633566943, 45.83887848292358314, -94.58095331458939370 ) ) ;
#50416 = CARTESIAN_POINT ( 'NONE',  ( 204.7199663062789057, 108.0881780334054838, 82.89220380942870747 ) ) ;
#50417 = EDGE_CURVE ( 'NONE', #16169, #39050, #33449, .T. ) ;
#50418 = DIRECTION ( 'NONE',  ( 0.000000000000000000, 0.000000000000000000, 1.000000000000000000 ) ) ;
#50419 = CARTESIAN_POINT ( 'NONE',  ( -71.56718866013692093, 19.74312628447965068, -66.98874544750654536 ) ) ;
#50420 = CARTESIAN_POINT ( 'NONE',  ( 112.3013380801408658, 400.0000000000066507, -123.9497041420121235 ) ) ;
#50421 = EDGE_LOOP ( 'NONE', ( #52194, #61683, #45995, #25943 ) ) ;
#50422 = ADVANCED_FACE ( 'NONE', ( #35691 ), #8952, .F. ) ;
#50423 = CARTESIAN_POINT ( 'NONE',  ( 15.29305096970402289, 7.491604910111008486, -8.674393508222093985 ) ) ;
#50424 = VERTEX_POINT ( 'NONE', #24098 ) ;
#50425 = VERTEX_POINT ( 'NONE', #45537 ) ;
#50426 = AXIS2_PLACEMENT_3D ( 'NONE', #15682, #37130, #58576 ) ;
#50427 = CARTESIAN_POINT ( 'NONE',  ( 64.94098077424391136, 14.16208887966257457, -23.64097255858331792 ) ) ;
#50428 = CARTESIAN_POINT ( 'NONE',  ( 181.5079096844946491, 80.47139261082469375, -78.06960825634331513 ) ) ;
#50429 = CARTESIAN_POINT ( 'NONE',  ( -165.6397095829521788, 80.60756690931943069, 37.71251476309661399 ) ) ;
#50430 = CARTESIAN_POINT ( 'NONE',  ( 111.1865443042262456, 30.43181341527238715, -24.03313457428269473 ) ) ;
#50431 = VECTOR ( 'NONE', #1316, 1000.000000000000000 ) ;
#50432 = CARTESIAN_POINT ( 'NONE',  ( -108.6909373351217312, 36.15835109565439609, 7.250169111965115931 ) ) ;
#50433 = DIRECTION ( 'NONE',  ( -0.000000000000000000, 1.000000000000000000, -0.000000000000000000 ) ) ;
#50434 = CARTESIAN_POINT ( 'NONE',  ( 139.6326990672751265, 46.22017155708127234, -21.46926057526128417 ) ) ;
#50435 = ORIENTED_EDGE ( 'NONE', *, *, #67045, .T. ) ;
#50436 = ORIENTED_EDGE ( 'NONE', *, *, #38178, .F. ) ;
#50437 = CARTESIAN_POINT ( 'NONE',  ( -7.825402957745087207, -170.0000000000000000, -96.60717191287118055 ) ) ;
#50438 = CARTESIAN_POINT ( 'NONE',  ( -10.91976120871577827, 7.112268444252504374, 3.934707406933564133 ) ) ;
#50439 = CARTESIAN_POINT ( 'NONE',  ( -18.15845058245960075, 17.18344181019522310, 0.000000000000000000 ) ) ;
#50440 = CARTESIAN_POINT ( 'NONE',  ( 56.66438910147189034, 11.28870326331392526, -20.37264592891143522 ) ) ;
#50441 = EDGE_CURVE ( 'NONE', #54841, #16199, #51172, .T. ) ;
#50442 = B_SPLINE_CURVE_WITH_KNOTS ( 'NONE', 3,
 ( #67638, #40893, #62353, #47528, #21171, #10255, #58109, #20465, #41250, #31040, #47198, #4981, #63740, #14507, #52140, #62706, #20817, #41928, #57419, #35965, #4307, #25424, #52484, #14845 ),
 .UNSPECIFIED., .F., .F.,
 ( 4, 2, 2, 2, 2, 2, 2, 2, 2, 2, 2, 4 ),
 ( 0.009967446706431848380, 0.01121006802826941991, 0.01245268935010699143, 0.01307400001102577806, 0.01369531067194456470, 0.01493793199378213796, 0.01555924265470091244, 0.01618055331561968346, 0.01742317463745724979, 0.01804448529837605550, 0.01866579595929486121, 0.01990841728113247958 ),
 .UNSPECIFIED. ) ;
#50443 = EDGE_CURVE ( 'NONE', #7667, #64962, #35711, .T. ) ;
#50444 = CARTESIAN_POINT ( 'NONE',  ( -190.6985136298602015, 109.1272424661243434, 42.87371446347281534 ) ) ;
#50445 = CARTESIAN_POINT ( 'NONE',  ( 198.4059165548112276, 99.71594270191991427, 67.64306774733000793 ) ) ;
#50446 = ORIENTED_EDGE ( 'NONE', *, *, #2551, .T. ) ;
#50447 = DIRECTION ( 'NONE',  ( -0.000000000000000000, 1.000000000000000000, -0.000000000000000000 ) ) ;
#50448 = CARTESIAN_POINT ( 'NONE',  ( -62.41727141396690115, 17.83188754031768042, -68.07784404646591270 ) ) ;
#50449 = CARTESIAN_POINT ( 'NONE',  ( 197.3756653044962945, 98.41886189307120958, -72.30260639311568127 ) ) ;
#50450 = DIRECTION ( 'NONE',  ( -9.860761315262647568E-31, 2.366582715663035416E-30, 1.000000000000000000 ) ) ;
#50451 = CARTESIAN_POINT ( 'NONE',  ( 275.2579562709427705, -21.94247096656777174, -1.618386763725532917 ) ) ;
#50452 = DIRECTION ( 'NONE',  ( 0.000000000000000000, -1.000000000000000000, 0.000000000000000000 ) ) ;
#50453 = CARTESIAN_POINT ( 'NONE',  ( -171.5864836273286755, 85.43596863096360039, -88.54944863603246574 ) ) ;
#50454 = LINE ( 'NONE', #50102, #21710 ) ;
#50455 = FACE_BOUND ( 'NONE', #58663, .T. ) ;
#50456 = CYLINDRICAL_SURFACE ( 'NONE', #57959, 65.00000000000000000 ) ;
#50457 = CARTESIAN_POINT ( 'NONE',  ( -1.083610669212419664, 6.545642299653469109, 67.78290952672001879 ) ) ;
#50458 = ORIENTED_EDGE ( 'NONE', *, *, #24142, .T. ) ;
#50459 = CARTESIAN_POINT ( 'NONE',  ( 275.2647131865113010, 21.94130279673636608, 1.613668875657348512 ) ) ;
#50460 = CARTESIAN_POINT ( 'NONE',  ( 150.0278556977734183, 53.32860603304214209, 64.83238834058245459 ) ) ;
#50461 = CARTESIAN_POINT ( 'NONE',  ( 329.1355598199468204, 0.000000000000000000, -129.5087625010780812 ) ) ;
#50462 = AXIS2_PLACEMENT_3D ( 'NONE', #61138, #54801, #12960 ) ;
#50463 = DIRECTION ( 'NONE',  ( 0.9839295885986321100, -0.1785568947986229116, 0.000000000000000000 ) ) ;
#50464 = CARTESIAN_POINT ( 'NONE',  ( 6.933333333333335347, 8.000000000000000000, 43.13333333333333286 ) ) ;
#50465 = VERTEX_POINT ( 'NONE', #2988 ) ;
#50466 = CARTESIAN_POINT ( 'NONE',  ( -188.6739852773920347, 108.2139733222100517, 9.872393598427303019 ) ) ;
#50467 = CARTESIAN_POINT ( 'NONE',  ( 15.78827728214693416, 6.500811158483284835, 3.170157082241545687 ) ) ;
#50468 = ORIENTED_EDGE ( 'NONE', *, *, #19048, .F. ) ;
#50469 = ORIENTED_EDGE ( 'NONE', *, *, #33995, .T. ) ;
#50470 = DIRECTION ( 'NONE',  ( 0.000000000000000000, 1.000000000000000000, -0.000000000000000000 ) ) ;
#50471 = CARTESIAN_POINT ( 'NONE',  ( 153.2208437558771834, 55.67531116261155688, 43.10704344242034836 ) ) ;
#50472 = DIRECTION ( 'NONE',  ( 1.000000000000000000, 0.000000000000000000, 0.000000000000000000 ) ) ;
#50473 = ORIENTED_EDGE ( 'NONE', *, *, #60280, .F. ) ;
#50474 = DIRECTION ( 'NONE',  ( -1.387778780781445922E-16, 1.000000000000000000, 1.232595164407830946E-32 ) ) ;
#50475 = VECTOR ( 'NONE', #14227, 1000.000000000000000 ) ;
#50476 = CARTESIAN_POINT ( 'NONE',  ( -178.7458319892713803, 93.61502008198023361, 16.44468136262722524 ) ) ;
#50477 = CARTESIAN_POINT ( 'NONE',  ( -3.252497086158848916, 6.636017118948021931, 4.805921196466799827 ) ) ;
#50478 = CARTESIAN_POINT ( 'NONE',  ( 36.61292551086699376, -65.40035471292219427, 41.38025477438755928 ) ) ;
#50479 = AXIS2_PLACEMENT_3D ( 'NONE', #14218, #41979, #58485 ) ;
#50480 = CARTESIAN_POINT ( 'NONE',  ( 38.61145386526410306, 15.82625607536648005, 13.79046412312118086 ) ) ;
#50481 = CARTESIAN_POINT ( 'NONE',  ( -190.6985136298601731, 109.1272424661242582, 33.97142148329322708 ) ) ;
#50482 = ORIENTED_EDGE ( 'NONE', *, *, #31675, .F. ) ;
#50483 = CARTESIAN_POINT ( 'NONE',  ( 114.6890011751076202, 30.99337387307412683, -37.36302526878641572 ) ) ;
#50484 = CARTESIAN_POINT ( 'NONE',  ( 8.000000000000007105, 249.8719672152120381, 94.99999999999866418 ) ) ;
#50485 = CARTESIAN_POINT ( 'NONE',  ( -12.50000000000000000, 207.5000000000000284, 0.000000000000000000 ) ) ;
#50486 = CARTESIAN_POINT ( 'NONE',  ( -169.1122507277982834, 84.24359299875008844, -75.41064519614697303 ) ) ;
#50488 = ORIENTED_EDGE ( 'NONE', *, *, #40094, .F. ) ;
#50487 = CARTESIAN_POINT ( 'NONE',  ( -131.1785597586340941, 50.07314260389248517, 86.47842268959267642 ) ) ;
#50489 = CARTESIAN_POINT ( 'NONE',  ( -27.41072479265578110, -43.79449985997803196, 26.66469066592268433 ) ) ;
#50490 = CIRCLE ( 'NONE', #58354, 2.999999999999999112 ) ;
#50491 = ADVANCED_FACE ( 'NONE', ( #46571 ), #67358, .F. ) ;
#50492 = VERTEX_POINT ( 'NONE', #62762 ) ;
#50493 = CARTESIAN_POINT ( 'NONE',  ( -142.4991775570125299, 58.45550857435405590, 67.79001987503191629 ) ) ;
#50494 = CARTESIAN_POINT ( 'NONE',  ( 82.14396250120408638, 18.99560174459421802, 31.19617389665937779 ) ) ;
#50495 = DIRECTION ( 'NONE',  ( -1.000000000000000000, 0.000000000000000000, 0.000000000000000000 ) ) ;
#50496 = DIRECTION ( 'NONE',  ( -0.000000000000000000, -0.000000000000000000, -1.000000000000000000 ) ) ;
#50497 = ADVANCED_FACE ( 'NONE', ( #67018 ), #36024, .F. ) ;
#50498 = DIRECTION ( 'NONE',  ( -0.000000000000000000, -1.000000000000000000, -0.000000000000000000 ) ) ;
#50499 = LINE ( 'NONE', #59989, #1848 ) ;
#50500 = CARTESIAN_POINT ( 'NONE',  ( -180.2188652555596207, 96.98354576637423463, -17.80801388957663534 ) ) ;
#50501 = ADVANCED_FACE ( 'NONE', ( #40956 ), #19850, .F. ) ;
#50502 = CYLINDRICAL_SURFACE ( 'NONE', #35138, 5.000000000000004441 ) ;
#50503 = EDGE_LOOP ( 'NONE', ( #39124, #24480, #29421, #29435 ) ) ;
#50504 = ORIENTED_EDGE ( 'NONE', *, *, #41055, .T. ) ;
#50505 = EDGE_CURVE ( 'NONE', #11659, #6690, #29363, .T. ) ;
#50506 = CARTESIAN_POINT ( 'NONE',  ( 110.2429982417149290, 28.88204397445231209, 56.45576479620100940 ) ) ;
#50507 = CARTESIAN_POINT ( 'NONE',  ( -5.000000000000000888, 0.000000000000000000, -9.474599999999998801 ) ) ;
#50508 = DIRECTION ( 'NONE',  ( -0.000000000000000000, -0.000000000000000000, -1.000000000000000000 ) ) ;
#50509 = EDGE_CURVE ( 'NONE', #16366, #44589, #66423, .T. ) ;
#50510 = CARTESIAN_POINT ( 'NONE',  ( 63.98009977735161158, 12.89803120691695604, -23.82977458817669358 ) ) ;
#50511 = CARTESIAN_POINT ( 'NONE',  ( -71.86568654225716557, 20.91200104397924875, -72.63218713565318296 ) ) ;
#50512 = CARTESIAN_POINT ( 'NONE',  ( -108.9136445001390143, 36.28030794288190464, 68.37215121731419742 ) ) ;
#50513 = CARTESIAN_POINT ( 'NONE',  ( -23.98903001682803193, 8.486614814224632042, -43.81140712853910202 ) ) ;
#50514 = FACE_OUTER_BOUND ( 'NONE', #56972, .T. ) ;
#50515 = ORIENTED_EDGE ( 'NONE', *, *, #66369, .F. ) ;
#50516 = EDGE_LOOP ( 'NONE', ( #48346, #18229, #49604, #65427 ) ) ;
#50517 = ORIENTED_EDGE ( 'NONE', *, *, #63378, .F. ) ;
#50518 = DIRECTION ( 'NONE',  ( 1.000000000000000000, 0.000000000000000000, -0.000000000000000000 ) ) ;
#50519 = CARTESIAN_POINT ( 'NONE',  ( -71.48316049915626991, 19.71415776932100528, 93.78843686400733759 ) ) ;
#50520 = LINE ( 'NONE', #29076, #8265 ) ;
#50521 = EDGE_CURVE ( 'NONE', #7387, #3371, #68616, .T. ) ;
#50522 = CARTESIAN_POINT ( 'NONE',  ( 128.4157044224113804, 39.39296260757094359, 31.82551368169737316 ) ) ;
#50523 = CARTESIAN_POINT ( 'NONE',  ( -58.20343064176747561, 3.983351098974750482, 27.58472369368492139 ) ) ;
#50524 = CIRCLE ( 'NONE', #28015, 65.00000000000000000 ) ;
#50525 = CARTESIAN_POINT ( 'NONE',  ( 47.73902449249074920, -57.85799893277823713, 170.0000000000000000 ) ) ;
#50526 = CARTESIAN_POINT ( 'NONE',  ( -149.5074843970971017, 64.17983161892348676, 57.56537183036274996 ) ) ;
#50527 = CIRCLE ( 'NONE', #46051, 74.95140232871122521 ) ;
#50528 = CARTESIAN_POINT ( 'NONE',  ( 55.51528220483959331, 12.08323518953685216, 37.55138378790348241 ) ) ;
#50529 = CARTESIAN_POINT ( 'NONE',  ( 38.75182793578637330, 8.325674960048864648, 83.62384145260158164 ) ) ;
#50530 = CARTESIAN_POINT ( 'NONE',  ( 0.000000000000000000, 0.000000000000000000, 0.000000000000000000 ) ) ;
#50531 = ORIENTED_EDGE ( 'NONE', *, *, #21192, .T. ) ;
#50532 = CARTESIAN_POINT ( 'NONE',  ( -0.8055628312658242862, 6.535476276302842003, -45.56989120479929767 ) ) ;
#50533 = FACE_OUTER_BOUND ( 'NONE', #58918, .T. ) ;
#50534 = CARTESIAN_POINT ( 'NONE',  ( -15.32495246574475267, 8.506829480038508251, 10.26907141737711804 ) ) ;
#50535 = CARTESIAN_POINT ( 'NONE',  ( -147.7845268487069745, 62.73119438705056439, 18.68858363414569723 ) ) ;
#50536 = DIRECTION ( 'NONE',  ( 0.000000000000000000, -1.000000000000000000, 0.000000000000000000 ) ) ;
#50537 = CARTESIAN_POINT ( 'NONE',  ( 197.2200752504831485, 96.62072041958364821, 64.21650735878895944 ) ) ;
#50538 = CARTESIAN_POINT ( 'NONE',  ( -95.59001106299177764, 29.51022327712105664, -92.80581223319890682 ) ) ;
#50539 = ORIENTED_EDGE ( 'NONE', *, *, #56060, .F. ) ;
#50540 = DIRECTION ( 'NONE',  ( 0.4127148655274873734, -0.9108602745606090290, -7.657887502499508081E-15 ) ) ;
#50541 = VECTOR ( 'NONE', #9233, 1000.000000000000000 ) ;
#50542 = CARTESIAN_POINT ( 'NONE',  ( 56.56044417847081718, -35.24940704026185045, 34.48241795236666718 ) ) ;
#50543 = DIRECTION ( 'NONE',  ( 0.000000000000000000, 6.123233995736762338E-17, -1.000000000000000000 ) ) ;
#50544 = CARTESIAN_POINT ( 'NONE',  ( -49.77357484059130144, -41.82599373102875973, 43.58025477438756923 ) ) ;
#50545 = ITEM_DEFINED_TRANSFORMATION ( 'NONE', 'NONE', #9668,  #66832 ) ;
#50546 = DIRECTION ( 'NONE',  ( 0.000000000000000000, 1.000000000000000000, 0.000000000000000000 ) ) ;
#50547 = ORIENTED_EDGE ( 'NONE', *, *, #31980, .T. ) ;
#50548 = CARTESIAN_POINT ( 'NONE',  ( -123.4531143159639157, 44.90777521523904880, -49.50914397245080778 ) ) ;
#50549 = CARTESIAN_POINT ( 'NONE',  ( -144.3945994505580757, 59.96115386701887218, -20.96066555231037754 ) ) ;
#50550 = CARTESIAN_POINT ( 'NONE',  ( -6.125624616441579740, 7.794071945221086040, -62.45369946781575266 ) ) ;
#50551 = SHAPE_REPRESENTATION ( 'hex nut gradec_iso_ISO - 4034 - M10 - N', ( #66832 ), #3998 ) ;
#50552 = CARTESIAN_POINT ( 'NONE',  ( 164.9007491581839417, 64.98457710411663868, 91.68427848334972907 ) ) ;
#50553 = ORIENTED_EDGE ( 'NONE', *, *, #35814, .F. ) ;
#50554 = CARTESIAN_POINT ( 'NONE',  ( 158.9247692837400052, 60.07442151987904566, -89.94665146420680912 ) ) ;
#50555 = CARTESIAN_POINT ( 'NONE',  ( 198.3926538463959162, 98.07933330386030946, -39.72515298445662779 ) ) ;
#50556 = CARTESIAN_POINT ( 'NONE',  ( -156.0204364459164594, 71.27041535366186054, 41.94903347539903393 ) ) ;
#50557 = VECTOR ( 'NONE', #52911, 1000.000000000000000 ) ;
#50558 = CARTESIAN_POINT ( 'NONE',  ( 20.74852474914889910, 6.709938988646747760, -37.37222025436115302 ) ) ;
#50560 = ORIENTED_EDGE ( 'NONE', *, *, #38290, .T. ) ;
#50559 = CARTESIAN_POINT ( 'NONE',  ( 117.3145357257065768, 33.41973663092564806, 12.81680853675090503 ) ) ;
#50561 = EDGE_CURVE ( 'NONE', #52688, #9201, #45066, .T. ) ;
#50562 = CARTESIAN_POINT ( 'NONE',  ( 59.95259601283825646, 11.98300577492411634, 30.46261997733679650 ) ) ;
#50563 = VERTEX_POINT ( 'NONE', #28409 ) ;
#50564 = ORIENTED_EDGE ( 'NONE', *, *, #21192, .F. ) ;
#50565 = CARTESIAN_POINT ( 'NONE',  ( 180.2494929075577943, 79.18888319146950039, 44.30859410551142474 ) ) ;
#50566 = CARTESIAN_POINT ( 'NONE',  ( 22.89634831467701304, 6.832298124325686395, -67.45812584797086231 ) ) ;
#50568 = ORIENTED_EDGE ( 'NONE', *, *, #27861, .F. ) ;
#50567 = CARTESIAN_POINT ( 'NONE',  ( -15.13464256769235838, 8.488509377255649468, -68.06414086977258648 ) ) ;
#50569 = CARTESIAN_POINT ( 'NONE',  ( 45.78444578631984285, 59.41672343742577311, 43.58025477438756923 ) ) ;
#50570 = LINE ( 'NONE', #9654, #19502 ) ;
#50571 = AXIS2_PLACEMENT_3D ( 'NONE', #67615, #19415, #40872 ) ;
#50572 = CARTESIAN_POINT ( 'NONE',  ( -74.79539698934961223, 21.95498232236883496, -49.04378561426771910 ) ) ;
#50573 = ORIENTED_EDGE ( 'NONE', *, *, #288, .T. ) ;
#50574 = CARTESIAN_POINT ( 'NONE',  ( 205.5049354810107900, 109.1776577097391225, -78.17048162308532255 ) ) ;
#50575 = EDGE_CURVE ( 'NONE', #36668, #66775, #65251, .T. ) ;
#50576 = LINE ( 'NONE', #29817, #8410 ) ;
#50577 = CARTESIAN_POINT ( 'NONE',  ( 110.7117404013331452, 30.20916032354563185, 29.61121420573731555 ) ) ;
#50578 = CARTESIAN_POINT ( 'NONE',  ( 127.4669243510812890, 38.85312661085429653, 67.81406123581646739 ) ) ;
#50579 = CARTESIAN_POINT ( 'NONE',  ( 20.74561700410411191, 7.717362891868938313, 70.00851792305307697 ) ) ;
#50580 = ORIENTED_EDGE ( 'NONE', *, *, #61214, .T. ) ;
#50581 = ORIENTED_EDGE ( 'NONE', *, *, #40174, .F. ) ;
#50582 = VERTEX_POINT ( 'NONE', #641 ) ;
#50583 = EDGE_CURVE ( 'NONE', #13335, #57503, #12243, .T. ) ;
#50584 = AXIS2_PLACEMENT_3D ( 'NONE', #8649, #29746, #66705 ) ;
#50585 = CARTESIAN_POINT ( 'NONE',  ( 15.78827728214693416, 7.507518794609588042, -23.67439350822212774 ) ) ;
#50586 = PRESENTATION_STYLE_ASSIGNMENT (( #7338 ) ) ;
#50587 = CARTESIAN_POINT ( 'NONE',  ( -37.92542950990691963, 10.74638084523341952, -46.59059523367306355 ) ) ;
#50588 = CARTESIAN_POINT ( 'NONE',  ( 218.0000000000000000, 128.6235316737731296, 94.99999999999866418 ) ) ;
#50589 = DIRECTION ( 'NONE',  ( -0.7818314824680221431, -0.6234898018587432533, 5.102127870520021999E-18 ) ) ;
#50590 = CARTESIAN_POINT ( 'NONE',  ( -132.0958200534848004, 50.71531800824802616, 60.73979307723551102 ) ) ;
#50591 = CARTESIAN_POINT ( 'NONE',  ( -173.1211646369891355, 87.12891641440857882, -76.55650775521370122 ) ) ;
#50592 = ORIENTED_EDGE ( 'NONE', *, *, #65796, .T. ) ;
#50593 = CARTESIAN_POINT ( 'NONE',  ( 149.0250918491436778, 0.000000000000000000, -9.435653166495526989 ) ) ;
#50594 = ORIENTED_EDGE ( 'NONE', *, *, #68084, .T. ) ;
#50595 = CARTESIAN_POINT ( 'NONE',  ( 34.83825437341840114, 7.859462995505743343, 31.44215116196434678 ) ) ;
#50596 = CARTESIAN_POINT ( 'NONE',  ( 86.62931800182293784, 20.48449268398423229, 56.55663816294300261 ) ) ;
#50597 = DIRECTION ( 'NONE',  ( 0.000000000000000000, 0.000000000000000000, 1.000000000000000000 ) ) ;
#50598 = EDGE_CURVE ( 'NONE', #5626, #25055, #38979, .T. ) ;
#50599 = CARTESIAN_POINT ( 'NONE',  ( -17.50000000000000000, 207.5000000000000284, 20.00000000000000000 ) ) ;
#50600 = CARTESIAN_POINT ( 'NONE',  ( -783.0172411895269988, -622.0000000000060254, 10.00000000000000000 ) ) ;
#50601 = CARTESIAN_POINT ( 'NONE',  ( -124.7710763417278201, 46.96042092553521741, 57.54553104023176502 ) ) ;
#50602 = CARTESIAN_POINT ( 'NONE',  ( -10.69547582519244600, 8.103864215011986616, -49.86004041143019805 ) ) ;
#50603 = AXIS2_PLACEMENT_3D ( 'NONE', #63498, #6120, #53947 ) ;
#50604 = EDGE_CURVE ( 'NONE', #6738, #17255, #11180, .T. ) ;
#50605 = CARTESIAN_POINT ( 'NONE',  ( 155.7277429502854034, 56.30804678861341728, -50.93229212615000989 ) ) ;
#50606 = EDGE_LOOP ( 'NONE', ( #60128, #41513, #8136, #45795 ) ) ;
#50607 = LINE ( 'NONE', #2771, #62332 ) ;
#50608 = CARTESIAN_POINT ( 'NONE',  ( -157.0069704378501854, 70.81086990254190994, -14.88609962755286986 ) ) ;
#50609 = VERTEX_POINT ( 'NONE', #59370 ) ;
#50610 = DIRECTION ( 'NONE',  ( -0.000000000000000000, -0.000000000000000000, -1.000000000000000000 ) ) ;
#50611 = DIRECTION ( 'NONE',  ( 0.7818314824680311359, -0.6234898018587318180, 5.102127870520020458E-18 ) ) ;
#50612 = DIRECTION ( 'NONE',  ( 1.000000000000000000, 0.000000000000000000, -0.000000000000000000 ) ) ;
#50613 = VERTEX_POINT ( 'NONE', #7318 ) ;
#50614 = CYLINDRICAL_SURFACE ( 'NONE', #62588, 299.9999999999999432 ) ;
#50615 = CARTESIAN_POINT ( 'NONE',  ( 151.1700480242206197, 54.15904440870131964, -66.39142155471229501 ) ) ;
#50616 = CARTESIAN_POINT ( 'NONE',  ( -38.54881010929334906, 10.86689971295294654, 40.15423812736370479 ) ) ;
#50617 = CARTESIAN_POINT ( 'NONE',  ( 141.2811136745703209, 46.09188267874204570, -44.61855967972866210 ) ) ;
#50618 = ORIENTED_EDGE ( 'NONE', *, *, #58194, .T. ) ;
#50619 =( LENGTH_UNIT ( ) NAMED_UNIT ( * ) SI_UNIT ( .MILLI., .METRE. ) );
#50620 = CARTESIAN_POINT ( 'NONE',  ( -125.4481990864046139, 46.20056605584955634, 30.61994787315706645 ) ) ;
#50621 = ORIENTED_EDGE ( 'NONE', *, *, #22251, .F. ) ;
#50622 = CARTESIAN_POINT ( 'NONE',  ( 37.45439421541014724, 9.177432671831377675, -9.015803115001828516 ) ) ;
#50623 = CARTESIAN_POINT ( 'NONE',  ( 5.799999999999999822, 0.000000000000000000, 8.000000000000000000 ) ) ;
#50624 = CARTESIAN_POINT ( 'NONE',  ( 126.6387625275754374, 38.38663782932677293, 92.76825455630849149 ) ) ;
#50625 = CYLINDRICAL_SURFACE ( 'NONE', #63927, 7.500000000000020428 ) ;
#50626 = CYLINDRICAL_SURFACE ( 'NONE', #53970, 5.000000000000004441 ) ;
#50627 = CARTESIAN_POINT ( 'NONE',  ( -125.0023254877051784, 45.90912477771776423, -76.71887141435124136 ) ) ;
#50628 = ORIENTED_EDGE ( 'NONE', *, *, #61473, .T. ) ;
#50629 = CARTESIAN_POINT ( 'NONE',  ( 164.3577270662354124, 63.21061577643037310, -19.76033467163099644 ) ) ;
#50630 = DIRECTION ( 'NONE',  ( -0.000000000000000000, -0.000000000000000000, -1.000000000000000000 ) ) ;
#50631 = CARTESIAN_POINT ( 'NONE',  ( 68.61679388097593346, 14.04192738700837317, 59.16375057879944421 ) ) ;
#50632 = CARTESIAN_POINT ( 'NONE',  ( 134.7770330630252715, 41.98246829846535633, -62.91025920626427848 ) ) ;
#50633 = CARTESIAN_POINT ( 'NONE',  ( 5.722400986011420443, -32.93231276838069022, 6.893342931642330029 ) ) ;
#50634 = VECTOR ( 'NONE', #40316, 1000.000000000000227 ) ;
#50635 = AXIS2_PLACEMENT_3D ( 'NONE', #4180, #45705, #25648 ) ;
#50636 = ORIENTED_EDGE ( 'NONE', *, *, #64543, .F. ) ;
#50637 = ADVANCED_FACE ( 'NONE', ( #32646 ), #54078, .F. ) ;
#50638 = CARTESIAN_POINT ( 'NONE',  ( -31.43908319763710679, -170.0000000000000000, 45.21645440618919309 ) ) ;
#50639 = AXIS2_PLACEMENT_3D ( 'NONE', #12160, #55404, #11102 ) ;
#50640 = CARTESIAN_POINT ( 'NONE',  ( 209.9999999999999716, -57.00000000000007816, 72.99999999999998579 ) ) ;
#50641 = ORIENTED_EDGE ( 'NONE', *, *, #38769, .F. ) ;
#50642 = EDGE_CURVE ( 'NONE', #15785, #37709, #28059, .T. ) ;
#50643 = CARTESIAN_POINT ( 'NONE',  ( 64.94098077424391136, 14.16208887966257279, 56.89267921280773521 ) ) ;
#50644 = LINE ( 'NONE', #12321, #35332 ) ;
#50645 = ORIENTED_EDGE ( 'NONE', *, *, #15956, .T. ) ;
#50646 = CARTESIAN_POINT ( 'NONE',  ( 164.4760519199595308, 64.62478832434435105, -40.89396928478465298 ) ) ;
#50647 = FACE_OUTER_BOUND ( 'NONE', #44323, .T. ) ;
#50648 = VECTOR ( 'NONE', #31377, 1000.000000000000000 ) ;
#50649 = CARTESIAN_POINT ( 'NONE',  ( 45.57199999999999562, 0.000000000000000000, 0.000000000000000000 ) ) ;
#50650 = FACE_OUTER_BOUND ( 'NONE', #58493, .T. ) ;
#50651 = VERTEX_POINT ( 'NONE', #59709 ) ;
#50652 = CARTESIAN_POINT ( 'NONE',  ( -97.48179118242299523, 31.52606332398820399, 5.389128531495072316 ) ) ;
#50653 = EDGE_CURVE ( 'NONE', #32859, #56923, #28773, .T. ) ;
#50654 = EDGE_CURVE ( 'NONE', #26077, #58934, #22789, .T. ) ;
#50655 = CARTESIAN_POINT ( 'NONE',  ( 69.99712624136184047, 15.44163584096631325, 93.82355723117841251 ) ) ;
#50656 = CARTESIAN_POINT ( 'NONE',  ( 155.7277429502854034, 56.30804678861341017, 29.60135964524100061 ) ) ;
#50657 = CARTESIAN_POINT ( 'NONE',  ( 86.15454111412294935, 20.32174891186169319, -23.97701360844805762 ) ) ;
#50658 = CARTESIAN_POINT ( 'NONE',  ( -132.2352756077771119, 50.81350938245625315, -19.58186461629218655 ) ) ;
#50659 = CARTESIAN_POINT ( 'NONE',  ( -145.6099850599923968, 60.94286946341170363, -89.59051459497440817 ) ) ;
#50660 = DIRECTION ( 'NONE',  ( 0.000000000000000000, -0.000000000000000000, 1.000000000000000000 ) ) ;
#50662 = ORIENTED_EDGE ( 'NONE', *, *, #42060, .T. ) ;
#50661 = ADVANCED_FACE ( 'NONE', ( #38619 ), #54790, .F. ) ;
#50663 = CARTESIAN_POINT ( 'NONE',  ( -94.83091526606384036, 30.26550147229323073, 63.84764049538445363 ) ) ;
#50664 = CARTESIAN_POINT ( 'NONE',  ( -15.07235766390729026, 8.482541916553474337, 62.51267422215675396 ) ) ;
#50665 = ORIENTED_EDGE ( 'NONE', *, *, #55163, .T. ) ;
#50666 = EDGE_CURVE ( 'NONE', #62075, #10266, #5732, .T. ) ;
#50667 = FACE_OUTER_BOUND ( 'NONE', #7127, .T. ) ;
#50668 = DIRECTION ( 'NONE',  ( -0.000000000000000000, -0.000000000000000000, -1.000000000000000000 ) ) ;
#50669 = LINE ( 'NONE', #13393, #8862 ) ;
#50670 = CARTESIAN_POINT ( 'NONE',  ( -1.866625526081663544, 7.583073082893620587, 42.19666861288822446 ) ) ;
#50671 = CARTESIAN_POINT ( 'NONE',  ( 133.8566784816069344, -170.0000000000000000, -16.67876034193198365 ) ) ;
#50672 = DIRECTION ( 'NONE',  ( 1.000000000000000000, -0.000000000000000000, 0.000000000000000000 ) ) ;
#50673 = CARTESIAN_POINT ( 'NONE',  ( -0.9897066053608923886, 7.549089325901772618, -19.16927265933078317 ) ) ;
#50674 = CARTESIAN_POINT ( 'NONE',  ( -8.810383862755511331, 7.965311326754782151, 45.06702628433764346 ) ) ;
#50675 = CARTESIAN_POINT ( 'NONE',  ( -62.45176220516622578, 16.79101814080732424, 12.22500217833821878 ) ) ;
#50676 = VERTEX_POINT ( 'NONE', #27356 ) ;
#50677 = CARTESIAN_POINT ( 'NONE',  ( -96.76336539645315327, 31.18045094643427717, -47.61949373948618813 ) ) ;
#50678 = ORIENTED_EDGE ( 'NONE', *, *, #23089, .T. ) ;
#50679 = LINE ( 'NONE', #35198, #47493 ) ;
#50680 = EDGE_CURVE ( 'NONE', #58183, #53205, #32993, .T. ) ;
#50681 = CARTESIAN_POINT ( 'NONE',  ( 44.34362023773823580, 10.12115849931652711, -21.93874443874187108 ) ) ;
#50682 = CARTESIAN_POINT ( 'NONE',  ( 46.13856685535755986, 9.381502944822521783, 67.59186432702131242 ) ) ;
#50683 = CARTESIAN_POINT ( 'NONE',  ( 7.345652830558766055, -4.996589667937388235, -9.003584543331200507 ) ) ;
#50684 = DIRECTION ( 'NONE',  ( -1.000000000000000000, -0.000000000000000000, -0.000000000000000000 ) ) ;
#50685 = AXIS2_PLACEMENT_3D ( 'NONE', #6138, #37810, #60311 ) ;
#50686 = EDGE_CURVE ( 'NONE', #18800, #36151, #21394, .T. ) ;
#50687 = ADVANCED_FACE ( 'NONE', ( #24547 ), #35434, .F. ) ;
#50688 = EDGE_CURVE ( 'NONE', #32880, #35021, #60904, .T. ) ;
#50689 = DIRECTION ( 'NONE',  ( 1.000000000000000000, 0.000000000000000000, 0.000000000000000000 ) ) ;
#50690 = AXIS2_PLACEMENT_3D ( 'NONE', #26153, #69042, #10305 ) ;
#50691 = LINE ( 'NONE', #24666, #8370 ) ;
#50692 = CARTESIAN_POINT ( 'NONE',  ( -168.7187482717113198, 82.35796501763485367, 59.07591196666088962 ) ) ;
#50693 = VERTEX_POINT ( 'NONE', #30496 ) ;
#50694 = VERTEX_POINT ( 'NONE', #18559 ) ;
#50695 = LINE ( 'NONE', #18693, #8462 ) ;
#50696 = LINE ( 'NONE', #30634, #25485 ) ;
#50698 = LINE ( 'NONE', #66552, #31198 ) ;
#50697 = AXIS2_PLACEMENT_3D ( 'NONE', #12424, #19421, #52799 ) ;
#50699 = VECTOR ( 'NONE', #66295, 1000.000000000000000 ) ;
#50700 = CARTESIAN_POINT ( 'NONE',  ( -417.6627218934913230, 179.4906275429376308, -146.4497041420118819 ) ) ;
#50701 = CARTESIAN_POINT ( 'NONE',  ( 157.4703587214989113, 57.65129005721575339, -24.27963370867398396 ) ) ;
#50702 = PRESENTATION_LAYER_ASSIGNMENT (  '', '', ( #12545 ) ) ;
#50703 = CARTESIAN_POINT ( 'NONE',  ( 58.08938767906776235, 12.61185010801508888, -10.69966040140734620 ) ) ;
#50704 = ORIENTED_EDGE ( 'NONE', *, *, #64790, .F. ) ;
#50705 = CARTESIAN_POINT ( 'NONE',  ( 107.9213359589209063, 28.92595015506875100, -36.27514522574465161 ) ) ;
#50706 = CARTESIAN_POINT ( 'NONE',  ( 21.74799039132243550, 7.772294950329605712, -38.43909590461863957 ) ) ;
#50707 = DIRECTION ( 'NONE',  ( -1.000000000000000000, 0.000000000000000000, -1.734723475976805517E-15 ) ) ;
#50708 = DIRECTION ( 'NONE',  ( -0.000000000000000000, 1.000000000000000000, -0.000000000000000000 ) ) ;
#50709 = CARTESIAN_POINT ( 'NONE',  ( 211.0967808702091588, 115.5516932918877018, -20.90306055675851482 ) ) ;
#50710 = FACE_BOUND ( 'NONE', #42745, .T. ) ;
#50711 = ORIENTED_EDGE ( 'NONE', *, *, #26426, .T. ) ;
#50712 = PLANE ( 'NONE',  #53711 ) ;
#50713 = DIRECTION ( 'NONE',  ( -0.000000000000000000, -0.000000000000000000, -1.000000000000000000 ) ) ;
#50714 = CARTESIAN_POINT ( 'NONE',  ( 32.37980458033285913, 8.611076697115699119, -67.31855367964614345 ) ) ;
#50715 = CARTESIAN_POINT ( 'NONE',  ( -72.62976060914746768, 18.74780984163032826, 43.58025477438756923 ) ) ;
#50716 = CARTESIAN_POINT ( 'NONE',  ( 157.0336341255056141, 57.31169401067818114, 2.564916881789689462 ) ) ;
#50717 = CARTESIAN_POINT ( 'NONE',  ( -200.0000000000000000, 2.449293598294706434E-14, 7.000000000000000000 ) ) ;
#50718 = ORIENTED_EDGE ( 'NONE', *, *, #34056, .T. ) ;
#50719 = DIRECTION ( 'NONE',  ( 0.000000000000000000, 0.000000000000000000, -1.000000000000000000 ) ) ;
#50720 = CARTESIAN_POINT ( 'NONE',  ( 198.2581645178918563, 99.52881771501682806, -39.97064483821105085 ) ) ;
#50721 = ORIENTED_EDGE ( 'NONE', *, *, #10872, .F. ) ;
#50722 = CARTESIAN_POINT ( 'NONE',  ( -64.56490107723145400, 16.52205003563488006, 34.48241823982461085 ) ) ;
#50723 = ORIENTED_EDGE ( 'NONE', *, *, #40967, .F. ) ;
#50724 = EDGE_CURVE ( 'NONE', #48508, #8633, #8001, .T. ) ;
#50725 = CARTESIAN_POINT ( 'NONE',  ( -86.17927978631391284, 25.32700573188346738, -69.44798174949396241 ) ) ;
#50726 = CARTESIAN_POINT ( 'NONE',  ( -62.49137879463568623, 17.85440472148627933, -14.88192700454524520 ) ) ;
#50727 = CARTESIAN_POINT ( 'NONE',  ( 63.00000000000000000, 7.715274834628325378E-15, 170.0000000000000000 ) ) ;
#50728 = ORIENTED_EDGE ( 'NONE', *, *, #14, .T. ) ;
#50729 = AXIS2_PLACEMENT_3D ( 'NONE', #15926, #37372, #38421 ) ;
#50730 = ORIENTED_EDGE ( 'NONE', *, *, #36033, .F. ) ;
#50731 = CARTESIAN_POINT ( 'NONE',  ( 45.04506994399700659, 10.22854084020123899, 59.29347898550686580 ) ) ;
#50732 = LINE ( 'NONE', #34584, #10144 ) ;
#50733 = CARTESIAN_POINT ( 'NONE',  ( 23.09541709302172308, 6.844586979481588784, 8.962678893484639531 ) ) ;
#50734 = VECTOR ( 'NONE', #41045, 1000.000000000000000 ) ;
#50735 = VERTEX_POINT ( 'NONE', #26938 ) ;
#50736 = EDGE_CURVE ( 'NONE', #58514, #25791, #25918, .T. ) ;
#50737 = PRODUCT_DEFINITION_SHAPE ( 'NONE', 'NONE',  #69584 ) ;
#50738 = AXIS2_PLACEMENT_3D ( 'NONE', #27038, #60088, #1361 ) ;
#50739 = CIRCLE ( 'NONE', #21553, 65.00000000000000000 ) ;
#50740 = CARTESIAN_POINT ( 'NONE',  ( -23.73638277007043840, 7.847555861075215411, 0.000000000000000000 ) ) ;
#50741 = CARTESIAN_POINT ( 'NONE',  ( -47.94536219817735656, 13.92422159065987586, 8.527031293414781388 ) ) ;
#50742 = CARTESIAN_POINT ( 'NONE',  ( -132.4776673493542489, 52.21763813822158085, -19.17034394188376112 ) ) ;
#50743 = DIRECTION ( 'NONE',  ( 2.220446049250313081E-16, -0.000000000000000000, 1.000000000000000000 ) ) ;
#50744 = EDGE_CURVE ( 'NONE', #69370, #30206, #21458, .T. ) ;
#50745 = LINE ( 'NONE', #1884, #33168 ) ;
#50747 = ORIENTED_EDGE ( 'NONE', *, *, #3482, .F. ) ;
#50746 = DIRECTION ( 'NONE',  ( -0.000000000000000000, -0.000000000000000000, 1.000000000000000000 ) ) ;
#50748 = ORIENTED_EDGE ( 'NONE', *, *, #53154, .F. ) ;
#50749 = VECTOR ( 'NONE', #50996, 1000.000000000000000 ) ;
#50750 = VERTEX_POINT ( 'NONE', #4457 ) ;
#50751 = CARTESIAN_POINT ( 'NONE',  ( 39.88971011078923823, 8.472992116645418292, 3.069283715499572907 ) ) ;
#50752 = CARTESIAN_POINT ( 'NONE',  ( 429.8372781065087338, 388.0000000000066507, -128.9497041420121093 ) ) ;
#50753 = CARTESIAN_POINT ( 'NONE',  ( -49.14234466229833487, 13.17605306081208560, -20.49537269497533032 ) ) ;
#50754 = CARTESIAN_POINT ( 'NONE',  ( 107.0471828278920583, 27.43080724084233069, -9.776041531421187258 ) ) ;
#50755 = CARTESIAN_POINT ( 'NONE',  ( 203.9276061909314706, 105.2889220654478777, 2.363170148305746565 ) ) ;
#50756 = CARTESIAN_POINT ( 'NONE',  ( 211.5020032503682330, 118.0078774122368515, 87.23615886703346689 ) ) ;
#50757 = CYLINDRICAL_SURFACE ( 'NONE', #36638, 7.500000000000020428 ) ;
#50758 = CARTESIAN_POINT ( 'NONE',  ( -85.64924756730677302, 26.19583280090850153, 62.01450634387265382 ) ) ;
#50759 = CARTESIAN_POINT ( 'NONE',  ( -15.13254930056756464, 7.477527548005403979, 39.32343163489576199 ) ) ;
#50760 = ORIENTED_EDGE ( 'NONE', *, *, #6174, .F. ) ;
#50761 = CARTESIAN_POINT ( 'NONE',  ( 10.83521140779424030, 7.398743030771586682, -21.82737784355149557 ) ) ;
#50762 = ORIENTED_EDGE ( 'NONE', *, *, #8977, .T. ) ;
#50763 = ORIENTED_EDGE ( 'NONE', *, *, #10010, .T. ) ;
#50764 = CARTESIAN_POINT ( 'NONE',  ( -144.9417090887490644, 61.69631066549396792, 5.421503341054570768 ) ) ;
#50765 = FACE_OUTER_BOUND ( 'NONE', #22922, .T. ) ;
#50766 = CARTESIAN_POINT ( 'NONE',  ( -37.11830583849306464, 11.61671896815851390, 86.49628856077504224 ) ) ;
#50767 = DIRECTION ( 'NONE',  ( 0.000000000000000000, -1.000000000000000000, 0.000000000000000000 ) ) ;
#50768 = EDGE_CURVE ( 'NONE', #62204, #68773, #19801, .T. ) ;
#50769 = DIRECTION ( 'NONE',  ( 1.000000000000000000, 0.000000000000000000, 0.000000000000000000 ) ) ;
#50770 = FACE_OUTER_BOUND ( 'NONE', #4610, .T. ) ;
#50771 = EDGE_CURVE ( 'NONE', #988, #40831, #50817, .T. ) ;
#50772 = FACE_OUTER_BOUND ( 'NONE', #6551, .T. ) ;
#50773 = ORIENTED_EDGE ( 'NONE', *, *, #65368, .F. ) ;
#50774 = ORIENTED_EDGE ( 'NONE', *, *, #6435, .F. ) ;
#50775 = DIRECTION ( 'NONE',  ( -0.000000000000000000, -0.000000000000000000, -1.000000000000000000 ) ) ;
#50776 = CARTESIAN_POINT ( 'NONE',  ( -74.52723870109939242, -7.962625360375267469, 41.38025477438755928 ) ) ;
#50777 = CARTESIAN_POINT ( 'NONE',  ( -1.734723475976807094E-15, 9.237604307034022355, -0.7145311798163346273 ) ) ;
#50778 = CARTESIAN_POINT ( 'NONE',  ( 93.59491193977102341, 22.99153521538281453, -94.19891465754322724 ) ) ;
#50779 = UNCERTAINTY_MEASURE_WITH_UNIT (LENGTH_MEASURE( 1.000000000000000082E-05 ), #35744, 'distance_accuracy_value', 'NONE');
#50780 = CONICAL_SURFACE ( 'NONE', #64282, 4.999999999999997335, 0.7853981633974482790 ) ;
#50781 = CARTESIAN_POINT ( 'NONE',  ( -48.57297291660698590, 13.03920345822338334, 34.00833018951762909 ) ) ;
#50782 = CARTESIAN_POINT ( 'NONE',  ( 70.26840926437850499, -170.0000000000000000, -95.00000000000133582 ) ) ;
#50783 = ORIENTED_EDGE ( 'NONE', *, *, #45966, .T. ) ;
#50784 = LINE ( 'NONE', #45156, #58097 ) ;
#50785 = CARTESIAN_POINT ( 'NONE',  ( -56.02289203441036847, 15.98631679403370320, -62.10799750277473663 ) ) ;
#50786 = CARTESIAN_POINT ( 'NONE',  ( 197.2847860006354779, 98.30530166401516112, -71.82171173343019177 ) ) ;
#50787 = CONICAL_SURFACE ( 'NONE', #10352, 65.00000000000000000, 0.7853981633974497223 ) ;
#50788 = B_SPLINE_CURVE_WITH_KNOTS ( 'NONE', 3,
 ( #68561, #26346, #58007, #25320, #53053, #63635, #15781, #21070, #5227, #30588, #9478, #10154, #31967, #15448, #16123, #26004, #52036, #3855, #52382, #63288, #61379, #68886, #57668, #58337, #10496, #9826, #53393, #31284, #30938, #69241, #42516, #4202, #46754, #68226, #36899, #41488, #52711, #4539, #21397, #47432, #31617, #42842, #20716, #64313, #64664, #65013 ),
 .UNSPECIFIED., .F., .F.,
 ( 4, 2, 2, 2, 2, 2, 2, 2, 2, 2, 2, 2, 2, 2, 2, 2, 2, 2, 2, 2, 2, 2, 4 ),
 ( 0.000000000000000000, 0.003736383952885418379, 0.005604575929328127135, 0.007472767905770836758, 0.008406863893992191569, 0.009340959882213546381, 0.01120915185865624039, 0.01214324784687757092, 0.01307734383509889971, 0.01401143982332023023, 0.01494553581154155902, 0.01587963179976289302, 0.01681372778798422354, 0.01774782377620555407, 0.01868191976442688459, 0.01961601575264821859, 0.02055011174086954912, 0.02148420772909087964, 0.02241830371731221017, 0.02428649569375488856, 0.02615468767019756696, 0.02802287964664024883, 0.02989107162308292723 ),
 .UNSPECIFIED. ) ;
#50789 = CARTESIAN_POINT ( 'NONE',  ( 275.0330373230561349, -21.99242646597929252, 0.6602422734858162112 ) ) ;
#50790 = CARTESIAN_POINT ( 'NONE',  ( 102.8458551240039185, 25.60773946375956811, 9.002155561060931177 ) ) ;
#50791 = CARTESIAN_POINT ( 'NONE',  ( -167.6386155194958576, 81.22597462185139250, 16.62036470824096313 ) ) ;
#50792 = CARTESIAN_POINT ( 'NONE',  ( -452.6627218934914367, 399.9999999999998863, -146.4497041420118251 ) ) ;
#50793 = FACE_OUTER_BOUND ( 'NONE', #33416, .T. ) ;
#50794 = CIRCLE ( 'NONE', #26047, 89.99999999999998579 ) ;
#50795 = PRESENTATION_LAYER_ASSIGNMENT (  '', '', ( #63151 ) ) ;
#50796 = AXIS2_PLACEMENT_3D ( 'NONE', #34498, #29893, #3504 ) ;
#50797 = CARTESIAN_POINT ( 'NONE',  ( -7.825402957745087207, 6.891034867348159842, 71.96013162991091860 ) ) ;
#50798 = ORIENTED_EDGE ( 'NONE', *, *, #5461, .T. ) ;
#50799 = CARTESIAN_POINT ( 'NONE',  ( 280.0000000000000000, 21.42428528562853884, -4.999999999999990230 ) ) ;
#50800 = VECTOR ( 'NONE', #56181, 1000.000000000000000 ) ;
#50801 = CARTESIAN_POINT ( 'NONE',  ( 150.9013375937531123, 53.96275732797612079, 67.38256602799636141 ) ) ;
#50802 = DIRECTION ( 'NONE',  ( -0.04486483035051862939, 0.9989930665413143673, 0.000000000000000000 ) ) ;
#50803 = LINE ( 'NONE', #50113, #33461 ) ;
#50804 = DIRECTION ( 'NONE',  ( 0.000000000000000000, 1.000000000000000000, 0.000000000000000000 ) ) ;
#50805 = ORIENTED_EDGE ( 'NONE', *, *, #47545, .F. ) ;
#50806 = DIRECTION ( 'NONE',  ( -1.001915251000354105E-14, 1.000000000000000000, -5.551115123125782702E-17 ) ) ;
#50807 = EDGE_CURVE ( 'NONE', #10912, #51932, #59977, .T. ) ;
#50808 = DIRECTION ( 'NONE',  ( -0.000000000000000000, -0.000000000000000000, 1.000000000000000000 ) ) ;
#50809 = ORIENTED_EDGE ( 'NONE', *, *, #11877, .T. ) ;
#50810 = ORIENTED_EDGE ( 'NONE', *, *, #26764, .F. ) ;
#50811 = EDGE_CURVE ( 'NONE', #22360, #29280, #19209, .T. ) ;
#50812 = CARTESIAN_POINT ( 'NONE',  ( 63.01563776193090405, 12.67277567978497643, 71.65751152968501003 ) ) ;
#50813 = CARTESIAN_POINT ( 'NONE',  ( -180.0179082103088035, 95.14811732286295864, -66.09535773320961027 ) ) ;
#50814 = CARTESIAN_POINT ( 'NONE',  ( -422.6627218934913799, 394.9999999999998295, -116.4497041420117824 ) ) ;
#50815 = ORIENTED_EDGE ( 'NONE', *, *, #68866, .T. ) ;
#50816 = LINE ( 'NONE', #67701, #39068 ) ;
#50817 = B_SPLINE_CURVE_WITH_KNOTS ( 'NONE', 3,
 ( #21313, #47019, #53659, #5484, #14661, #68477, #36123, #36467, #57923, #37842, #38182, #54704, #22357, #32908, #48364, #5818, #32566, #22703, #54346, #33624, #53993, #49421, #6873, #11793, #17417, #49771, #39244, #38533, #64576, #12506, #1251, #60340, #6168, #28325, #27275, #43107, #33964, #27630, #44514, #7230, #44144, #64929, #17788, #49068, #11436, #60688 ),
 .UNSPECIFIED., .F., .F.,
 ( 4, 2, 2, 2, 2, 2, 2, 2, 2, 2, 2, 2, 2, 2, 2, 2, 2, 2, 2, 2, 2, 2, 4 ),
 ( 3.179800655392250756E-17, 0.003373244802897452585, 0.004216556003621778001, 0.005059867204346101682, 0.006746489605794751647, 0.007589800806519077063, 0.008433112007243401612, 0.009276423207967727028, 0.01011973440869205071, 0.01180635681014071195, 0.01349297921158937492, 0.01433629041231369167, 0.01517960161303801361, 0.01686622401448661587, 0.01770953521521088925, 0.01855284641593516609, 0.02023946881738373713, 0.02108278001810798621, 0.02192609121883223183, 0.02361271362028073695, 0.02445602482100496175, 0.02529933602172918655, 0.02698595842317763269 ),
 .UNSPECIFIED. ) ;
#50818 = CARTESIAN_POINT ( 'NONE',  ( -175.9970298498767249, 90.38640259140137800, 4.537318838786393194 ) ) ;
#50819 = CARTESIAN_POINT ( 'NONE',  ( -2.174378755909794236, 6.588636630831475216, 15.72640502805996654 ) ) ;
#50820 = CARTESIAN_POINT ( 'NONE',  ( 58.09877917144280701, 12.61383386832654452, -48.90516037375699909 ) ) ;
#50821 = CARTESIAN_POINT ( 'NONE',  ( -86.10360257264194672, 26.38663017581291115, 38.92037401638386029 ) ) ;
#50822 = CARTESIAN_POINT ( 'NONE',  ( -3.318518101603030512, -7.321656987762886537, -6.254491282525755281E-15 ) ) ;
#50823 = CARTESIAN_POINT ( 'NONE',  ( 139.3067271572849677, 44.81402783181198402, 15.32414253876127930 ) ) ;
#50824 = ADVANCED_BREP_SHAPE_REPRESENTATION ( '', ( #39903, #66832 ), #30915 ) ;
#50825 = ADVANCED_FACE ( 'NONE', ( #1598 ), #65988, .F. ) ;
#50826 = VERTEX_POINT ( 'NONE', #43794 ) ;
#50827 = CARTESIAN_POINT ( 'NONE',  ( 116.6734749296699079, 31.97209464358268605, -39.53049973554296770 ) ) ;
#50828 = CARTESIAN_POINT ( 'NONE',  ( -75.00452312211128003, 22.03104735285382532, 4.523913399809351255 ) ) ;
#50829 = ADVANCED_FACE ( 'NONE', ( #43451 ), #65269, .T. ) ;
#50830 = CARTESIAN_POINT ( 'NONE',  ( 42.71504753277076105, 8.863481902720385719, -36.38681058640105448 ) ) ;
#50831 = EDGE_CURVE ( 'NONE', #60761, #41997, #67649, .T. ) ;
#50832 = DIRECTION ( 'NONE',  ( -4.565061778886334783E-18, 1.000000000000000000, 0.000000000000000000 ) ) ;
#50834 = VERTEX_POINT ( 'NONE', #45902 ) ;
#50833 = CARTESIAN_POINT ( 'NONE',  ( -417.6627218934913230, 219.4906275429376308, -146.4497041420118819 ) ) ;
#50835 = CARTESIAN_POINT ( 'NONE',  ( 79.38020582286198135, 17.07365509555549110, -45.31021711467555235 ) ) ;
#50836 = AXIS2_PLACEMENT_3D ( 'NONE', #10061, #26586, #42416 ) ;
#50837 = ORIENTED_EDGE ( 'NONE', *, *, #30250, .F. ) ;
#50838 = CARTESIAN_POINT ( 'NONE',  ( 0.000000000000000000, 0.000000000000000000, -10.00000000000000000 ) ) ;
#50839 = CARTESIAN_POINT ( 'NONE',  ( 86.62931800182293784, 20.48449268398423229, 44.71208757247933363 ) ) ;
#50840 = CARTESIAN_POINT ( 'NONE',  ( 39.54205320694339321, 51.58901073076764021, 170.0000000000000000 ) ) ;
#50841 = CARTESIAN_POINT ( 'NONE',  ( 141.9165763529819344, -2.000000000000000000, 108.9999999999999858 ) ) ;
#50842 = VECTOR ( 'NONE', #47547, 1000.000000000000000 ) ;
#50843 = CARTESIAN_POINT ( 'NONE',  ( -125.4481990864045855, 46.20056605584957765, 57.46449846362079228 ) ) ;
#50844 = LINE ( 'NONE', #61398, #28642 ) ;
#50845 = CARTESIAN_POINT ( 'NONE',  ( 21.08384185994383841, 7.735488641401683907, -91.38067577833801636 ) ) ;
#50846 = CARTESIAN_POINT ( 'NONE',  ( -47.65155309726505806, 13.85482731128119838, 36.57865308283418670 ) ) ;
#50847 = ORIENTED_EDGE ( 'NONE', *, *, #9397, .F. ) ;
#50848 = VERTEX_POINT ( 'NONE', #34318 ) ;
#50849 = CARTESIAN_POINT ( 'NONE',  ( 104.7147873368645179, 26.40702926859711042, 69.04812278364634892 ) ) ;
#50850 = VECTOR ( 'NONE', #6608, 1000.000000000000000 ) ;
#50851 = FACE_OUTER_BOUND ( 'NONE', #57303, .T. ) ;
#50852 = CARTESIAN_POINT ( 'NONE',  ( -189.2442476610617916, 107.0963225822736433, 65.70228303047002782 ) ) ;
#50853 = DIRECTION ( 'NONE',  ( 1.000000000000000000, 2.465190328815660250E-32, 1.671219923253722421E-63 ) ) ;
#50854 = LINE ( 'NONE', #44538, #61794 ) ;
#50855 = CARTESIAN_POINT ( 'NONE',  ( -26.87327614295023892, 8.886070347947290671, -36.84684950165980410 ) ) ;
#50856 = ADVANCED_FACE ( 'NONE', ( #29377, #2648, #45548, #61724, #13549 ), #7589, .T. ) ;
#50857 = DIRECTION ( 'NONE',  ( 0.000000000000000000, 0.000000000000000000, -1.000000000000000000 ) ) ;
#50858 = VERTEX_POINT ( 'NONE', #19509 ) ;
#50859 = ORIENTED_EDGE ( 'NONE', *, *, #10080, .F. ) ;
#50860 = ORIENTED_EDGE ( 'NONE', *, *, #26231, .T. ) ;
#50861 = CARTESIAN_POINT ( 'NONE',  ( -10.91976120871578537, 7.112268444252506150, -49.75439377399378316 ) ) ;
#50862 = CARTESIAN_POINT ( 'NONE',  ( -72.54743664134970516, 20.08440888238853717, 87.25848529910209095 ) ) ;
#50863 = CARTESIAN_POINT ( 'NONE',  ( -56.44201257846631847, 32.26641783793562013, 0.000000000000000000 ) ) ;
#50864 = DIRECTION ( 'NONE',  ( 1.000000000000000000, 0.000000000000000000, 0.000000000000000000 ) ) ;
#50865 = DIRECTION ( 'NONE',  ( -0.8160245890732938934, -0.5780171883497599028, 0.000000000000000000 ) ) ;
#50866 = CARTESIAN_POINT ( 'NONE',  ( -56.72676045871359207, 16.18052435693490310, 30.50251775650468744 ) ) ;
#50867 = DIRECTION ( 'NONE',  ( 0.000000000000000000, 1.000000000000000000, 0.000000000000000000 ) ) ;
#50868 = CARTESIAN_POINT ( 'NONE',  ( 55.64941047419414843, 12.11006143146460978, 38.78652927538340123 ) ) ;
#50869 = CARTESIAN_POINT ( 'NONE',  ( 31.99225359986736095, 7.561112794910904711, 89.89537387559623483 ) ) ;
#50870 = CARTESIAN_POINT ( 'NONE',  ( 0.000000000000000000, -0.4541622202827808596, -4.636770908075737552 ) ) ;
#50871 = EDGE_LOOP ( 'NONE', ( #6586, #57650, #66906, #6987 ) ) ;
#50872 = CARTESIAN_POINT ( 'NONE',  ( -3.857727530059809062, 6.665032499723453796, -36.54875858820001611 ) ) ;
#50873 = FACE_OUTER_BOUND ( 'NONE', #66507, .T. ) ;
#50874 = CARTESIAN_POINT ( 'NONE',  ( -14.33576511807126153, 8.413127487936186810, 14.52671630318449303 ) ) ;
#50875 = LINE ( 'NONE', #39978, #55549 ) ;
#50876 = CARTESIAN_POINT ( 'NONE',  ( 283.7666631852362116, -21.75169080623575724, -3.304315882619051514 ) ) ;
#50877 = CARTESIAN_POINT ( 'NONE',  ( -109.5025362253418706, 36.60371748273998094, -67.27247425872458564 ) ) ;
#50878 = CARTESIAN_POINT ( 'NONE',  ( 130.7457207912711112, 40.74300766298685517, -23.51872159297877829 ) ) ;
#50879 = VERTEX_POINT ( 'NONE', #50485 ) ;
#50880 = VECTOR ( 'NONE', #34174, 1000.000000000000114 ) ;
#50881 = APPLICATION_PROTOCOL_DEFINITION ( 'draft international standard', 'automotive_design', 1998, #46670 ) ;
#50882 = CARTESIAN_POINT ( 'NONE',  ( 129.1052153257903683, 39.78893484542956571, -37.69982810349421243 ) ) ;
#50883 = CARTESIAN_POINT ( 'NONE',  ( -126.3458714439411068, 46.79154809309480356, 3.775397282693374823 ) ) ;
#50884 = DIRECTION ( 'NONE',  ( -0.000000000000000000, 1.000000000000000000, -0.000000000000000000 ) ) ;
#50885 = EDGE_CURVE ( 'NONE', #15022, #22933, #35004, .T. ) ;
#50886 = CONTEXT_DEPENDENT_SHAPE_REPRESENTATION ( #21590, #38874 ) ;
#50887 = FACE_OUTER_BOUND ( 'NONE', #43224, .T. ) ;
#50888 = ORIENTED_EDGE ( 'NONE', *, *, #39553, .T. ) ;
#50889 = PLANE ( 'NONE',  #39132 ) ;
#50890 = EDGE_CURVE ( 'NONE', #21908, #66303, #13888, .T. ) ;
#50891 = EDGE_CURVE ( 'NONE', #52445, #42554, #23758, .T. ) ;
#50892 = DIRECTION ( 'NONE',  ( -0.000000000000000000, -0.000000000000000000, -1.000000000000000000 ) ) ;
#50893 = EDGE_CURVE ( 'NONE', #8872, #23841, #3001, .T. ) ;
#50894 = AXIS2_PLACEMENT_3D ( 'NONE', #43411, #64889, #60302 ) ;
#50895 = DIRECTION ( 'NONE',  ( -0.000000000000000000, -1.000000000000000000, -0.000000000000000000 ) ) ;
#50896 = EDGE_CURVE ( 'NONE', #2615, #26373, #40969, .T. ) ;
#50897 = AXIS2_PLACEMENT_3D ( 'NONE', #48253, #48593, #38067 ) ;
#50898 = CARTESIAN_POINT ( 'NONE',  ( 150.4653148198808879, 53.64543865262506017, 87.89445436269947720 ) ) ;
#50899 = ORIENTED_EDGE ( 'NONE', *, *, #20631, .F. ) ;
#50900 = LINE ( 'NONE', #12230, #19992 ) ;
#50901 = CARTESIAN_POINT ( 'NONE',  ( 130.3245512970360664, 39.33195360491887271, 43.64341809288409735 ) ) ;
#50902 = B_SPLINE_CURVE_WITH_KNOTS ( 'NONE', 3,
 ( #69109, #31166, #10369, #20244, #4416, #58223 ),
 .UNSPECIFIED., .F., .F.,
 ( 4, 2, 4 ),
 ( 1.095770181115537934E-06, 0.03239442681617711595, 0.06478775786217312593 ),
 .UNSPECIFIED. ) ;
#50903 = EDGE_CURVE ( 'NONE', #47585, #17657, #50140, .T. ) ;
#50904 = CARTESIAN_POINT ( 'NONE',  ( -156.3734885497381129, 71.59531449004283843, 35.19087983619847648 ) ) ;
#50905 = VECTOR ( 'NONE', #4051, 1000.000000000000000 ) ;
#50906 = PLANE ( 'NONE',  #32537 ) ;
#50907 = CARTESIAN_POINT ( 'NONE',  ( 79.38020582286199556, 17.07365509555549110, 8.378884066251806928 ) ) ;
#50909 = ORIENTED_EDGE ( 'NONE', *, *, #47095, .F. ) ;
#50908 = DIRECTION ( 'NONE',  ( 0.000000000000000000, 0.000000000000000000, 1.000000000000000000 ) ) ;
#50910 = CARTESIAN_POINT ( 'NONE',  ( 59.72526569420001152, 11.93313563009888867, 44.07029543158733276 ) ) ;
#50911 = ORIENTED_EDGE ( 'NONE', *, *, #53734, .F. ) ;
#50912 = ORIENTED_EDGE ( 'NONE', *, *, #39579, .T. ) ;
#50913 = CARTESIAN_POINT ( 'NONE',  ( 175.0696098417091378, 74.11936424544845181, 32.32058490622820557 ) ) ;
#50914 = EDGE_CURVE ( 'NONE', #25055, #52276, #29034, .T. ) ;
#50915 = CARTESIAN_POINT ( 'NONE',  ( -31.43908319763710679, 10.61114334766713796, -89.00629854612920155 ) ) ;
#50916 = ADVANCED_FACE ( 'NONE', ( #26171 ), #37402, .F. ) ;
#50918 = ORIENTED_EDGE ( 'NONE', *, *, #63202, .F. ) ;
#50917 = CARTESIAN_POINT ( 'NONE',  ( -15.32584732649904247, 8.506915958926390076, -69.27421579052196421 ) ) ;
#50919 = CARTESIAN_POINT ( 'NONE',  ( -95.00922893699316774, 30.34910376528943132, 89.83886361574879231 ) ) ;
#50920 = CARTESIAN_POINT ( 'NONE',  ( -23.99957301099516727, 9.503061049698466434, 36.73396631618189900 ) ) ;
#50921 = CARTESIAN_POINT ( 'NONE',  ( -71.86568654225716557, 20.91200104397924875, -45.78763654518949267 ) ) ;
#50922 = ORIENTED_EDGE ( 'NONE', *, *, #63361, .F. ) ;
#50923 = B_SPLINE_CURVE_WITH_KNOTS ( 'NONE', 3,
 ( #39517, #1898, #65924, #39860, #6464, #27912, #49349, #12790, #1183, #16997, #44075, #66611, #7522, #18404, #2239, #838, #28973, #65559, #61316, #12090, #59906, #38826, #60275, #6802, #54984, #28254, #17719, #12437, #50419, #33896, #34248, #13479, #67307, #9237, #14849, #14169, #24733, #24389, #45831, #25077, #67991, #51463, #57424, #40897 ),
 .UNSPECIFIED., .F., .F.,
 ( 4, 2, 2, 2, 2, 2, 2, 2, 2, 2, 2, 2, 2, 2, 2, 2, 2, 2, 2, 2, 2, 4 ),
 ( 0.02432640572110343277, 0.02583721026359366707, 0.02659261253483879983, 0.02734801480608393259, 0.02885881934857420852, 0.02961422161981933088, 0.03036962389106444976, 0.03188042843355469447, 0.03339123297604493917, 0.03414663524729004418, 0.03490203751853514919, 0.03641284206102534532, 0.03716824433227044339, 0.03792364660351554145, 0.03943445114600568902, 0.04094525568849584352, 0.04245606023098599802, 0.04396686477347614558, 0.04472226704472121589, 0.04547766931596629314, 0.04698847385845641295, 0.04849927840094653275 ),
 .UNSPECIFIED. ) ;
#50924 = CARTESIAN_POINT ( 'NONE',  ( 210.6584452238134588, 116.7138338345753681, -75.24916677418407573 ) ) ;
#50925 = CARTESIAN_POINT ( 'NONE',  ( 139.7883986595928434, 46.32091287009617986, 32.41387198680679660 ) ) ;
#50926 = CARTESIAN_POINT ( 'NONE',  ( 218.0000000000000000, 126.6235316737731296, 94.99999999999866418 ) ) ;
#50927 = CARTESIAN_POINT ( 'NONE',  ( -127.4644500646574556, 48.74852676951797292, 3.938189400447978716 ) ) ;
#50928 = CARTESIAN_POINT ( 'NONE',  ( 63.01563776193091826, 13.70579113808094718, -77.56524142263344856 ) ) ;
#50930 = ORIENTED_EDGE ( 'NONE', *, *, #15247, .F. ) ;
#50929 = B_SPLINE_CURVE_WITH_KNOTS ( 'NONE', 3,
 ( #5541, #69555, #15758, #64287, #16097, #26996, #21717, #59001, #10820, #43165, #32973, #64639, #54406, #6231, #37903, #27687, #49128, #971, #28386, #24170, #13266, #23818, #18883, #3060, #2023, #45613, #60746, #18192, #44573, #55115, #7982, #7648, #40333, #51246, #61780, #29434, #17481, #49833, #34382, #65692, #44207, #50198, #66050, #8336, #12925, #13603, #6936, #23480, #29780, #12219, #33685, #35060, #1659, #29099, #67095, #66402, #55467, #2365 ),
 .UNSPECIFIED., .F., .F.,
 ( 4, 2, 2, 2, 2, 2, 2, 2, 2, 2, 2, 2, 2, 2, 2, 2, 2, 2, 2, 2, 2, 2, 2, 2, 2, 2, 2, 2, 4 ),
 ( 0.000000000000000000, 0.001128500949314689087, 0.002257001898629378174, 0.003385502847944066827, 0.003949753322601412021, 0.004514003797258757215, 0.005642504746573493574, 0.006771005695888229065, 0.007899506645202964555, 0.009028007594517700046, 0.01128500949314724215, 0.01354201139177678079, 0.01579901329040632116, 0.01805601518903586153, 0.01918451613835061437, 0.02031301708766536721, 0.02257001898629487982, 0.02369851993560962919, 0.02482702088492437509, 0.02708402278355386689, 0.02821252373286863707, 0.02934102468218340726, 0.03046952563149817397, 0.03159802658081294069, 0.03216227705547035354, 0.03272652753012775945, 0.03385502847944261984, 0.03498352942875748023, 0.03611203037807233368 ),
 .UNSPECIFIED. ) ;
#50931 = VERTEX_POINT ( 'NONE', #37069 ) ;
#50932 = ORIENTED_EDGE ( 'NONE', *, *, #37724, .F. ) ;
#50933 = VECTOR ( 'NONE', #10871, 1000.000000000000000 ) ;
#50934 = DIRECTION ( 'NONE',  ( 0.000000000000000000, 0.000000000000000000, -1.000000000000000000 ) ) ;
#50935 = CARTESIAN_POINT ( 'NONE',  ( -7.486743542470078339, 64.58150799671128084, 170.0000000000000000 ) ) ;
#50936 = VECTOR ( 'NONE', #40731, 1000.000000000000000 ) ;
#50937 = CARTESIAN_POINT ( 'NONE',  ( 417.3372781065086201, 399.9999999999998863, 113.5502958579881891 ) ) ;
#50938 = DIRECTION ( 'NONE',  ( 1.000000000000000000, 0.000000000000000000, 0.000000000000000000 ) ) ;
#50939 = DIRECTION ( 'NONE',  ( 1.000000000000000000, 0.000000000000000000, 0.000000000000000000 ) ) ;
#50940 = VECTOR ( 'NONE', #12247, 1000.000000000000000 ) ;
#50941 = CARTESIAN_POINT ( 'NONE',  ( -125.8938041572051105, 46.49392987655492959, 57.46449846362076386 ) ) ;
#50942 = CARTESIAN_POINT ( 'NONE',  ( 280.0000000000000000, 21.42428528562853884, -4.999999999999990230 ) ) ;
#50943 = ORIENTED_EDGE ( 'NONE', *, *, #31366, .T. ) ;
#50945 = DIRECTION ( 'NONE',  ( 0.000000000000000000, 0.000000000000000000, 1.000000000000000000 ) ) ;
#50944 = VECTOR ( 'NONE', #7979, 1000.000000000000114 ) ;
#50946 = ORIENTED_EDGE ( 'NONE', *, *, #6019, .F. ) ;
#50947 = CARTESIAN_POINT ( 'NONE',  ( -94.96454763573188984, 30.32814623986933000, -94.53419202597292781 ) ) ;
#50948 = VECTOR ( 'NONE', #45006, 1000.000000000000227 ) ;
#50949 = CARTESIAN_POINT ( 'NONE',  ( 84.27937148876358719, 19.69225537006224158, 56.93023493300005100 ) ) ;
#50950 = VERTEX_POINT ( 'NONE', #58510 ) ;
#50951 = CARTESIAN_POINT ( 'NONE',  ( 188.2133404574781537, 86.12414067617872604, 39.15481199342811891 ) ) ;
#50952 = DIRECTION ( 'NONE',  ( -0.000000000000000000, -1.000000000000000000, -0.000000000000000000 ) ) ;
#50953 = B_SPLINE_CURVE_WITH_KNOTS ( 'NONE', 3,
 ( #48785, #980, #270, #10481, #630, #42826 ),
 .UNSPECIFIED., .F., .F.,
 ( 4, 2, 4 ),
 ( 0.02753256082175533151, 0.02987018134127081281, 0.03220780186078629065 ),
 .UNSPECIFIED. ) ;
#50954 = CARTESIAN_POINT ( 'NONE',  ( 39.40195752203892710, 8.409560354027389550, 18.06928371549960133 ) ) ;
#50955 = CARTESIAN_POINT ( 'NONE',  ( 442.3372781065089612, 390.0000000000074465, -141.4497041420121377 ) ) ;
#50956 = VECTOR ( 'NONE', #32173, 1000.000000000000114 ) ;
#50957 = DIRECTION ( 'NONE',  ( -0.9009688679024155933, -0.4338837391175656699, 0.000000000000000000 ) ) ;
#50958 = ORIENTED_EDGE ( 'NONE', *, *, #15343, .T. ) ;
#50959 = CARTESIAN_POINT ( 'NONE',  ( -108.2330097037575598, 35.90915053323784178, -91.63594520124935627 ) ) ;
#50960 = CARTESIAN_POINT ( 'NONE',  ( 173.9832054143776077, 73.09312616907610050, -95.00000000000133582 ) ) ;
#50961 = EDGE_LOOP ( 'NONE', ( #2279, #34138, #11425, #524 ) ) ;
#50962 = CARTESIAN_POINT ( 'NONE',  ( 0.000000000000000000, 0.000000000000000000, 0.000000000000000000 ) ) ;
#50963 = CARTESIAN_POINT ( 'NONE',  ( -62.15063206372443005, 17.75106610013994057, 62.18892694254114417 ) ) ;
#50964 = CARTESIAN_POINT ( 'NONE',  ( 444.9999999999999432, -35.00000000000000000, 380.0000000000000000 ) ) ;
#50965 = ORIENTED_EDGE ( 'NONE', *, *, #41772, .T. ) ;
#50966 = CARTESIAN_POINT ( 'NONE',  ( 100.0000000000000284, -5.000000000000000000, 18.50000000000000000 ) ) ;
#50967 = CARTESIAN_POINT ( 'NONE',  ( 150.4542242713869484, 53.63744268572192198, -67.80470997374955289 ) ) ;
#50968 = CARTESIAN_POINT ( 'NONE',  ( -31.43908319763710679, 9.591432048623758533, 45.21645440618919309 ) ) ;
#50969 =( BOUNDED_CURVE ( )  B_SPLINE_CURVE ( 3, ( #36310, #57765, #13808, #4305 ),
 .UNSPECIFIED., .F., .F. ) 
 B_SPLINE_CURVE_WITH_KNOTS ( ( 4, 4 ),
 ( 2.506209174768084136, 3.776976132411494103 ),
 .UNSPECIFIED. ) 
 CURVE ( )  GEOMETRIC_REPRESENTATION_ITEM ( )  RATIONAL_B_SPLINE_CURVE ( ( 1.000000000000000000, 0.8698961108463048042, 0.8698961108463048042, 1.000000000000000000 ) ) 
 REPRESENTATION_ITEM ( '' )  );
#50970 = CARTESIAN_POINT ( 'NONE',  ( 137.4117721579688123, 43.61242559081433257, -36.90228539602491509 ) ) ;
#50971 = EDGE_LOOP ( 'NONE', ( #30903, #67963, #31405 ) ) ;
#50972 = SHAPE_REPRESENTATION_RELATIONSHIP ( 'NONE' , 'NONE' ,  #45199, #63416 ) ;
#50973 = DIRECTION ( 'NONE',  ( -0.000000000000000000, -1.000000000000000000, -0.000000000000000000 ) ) ;
#50974 = CARTESIAN_POINT ( 'NONE',  ( -439.4229916354182706, 400.0000000000064801, 91.05029585798840230 ) ) ;
#50975 = ORIENTED_EDGE ( 'NONE', *, *, #59522, .F. ) ;
#50976 = LINE ( 'NONE', #34809, #51483 ) ;
#50977 = CARTESIAN_POINT ( 'NONE',  ( 188.5837490358996433, 86.53279111916964439, 9.653281778228306464 ) ) ;
#50978 = CARTESIAN_POINT ( 'NONE',  ( 92.51858280840788495, 21.51505926344914243, 59.38593706081789492 ) ) ;
#50979 = CARTESIAN_POINT ( 'NONE',  ( 63.72039997003709288, 12.83396383267841223, 170.0000000000000000 ) ) ;
#50980 = ADVANCED_FACE ( 'NONE', ( #30414 ), #51866, .T. ) ;
#50981 = B_SPLINE_CURVE_WITH_KNOTS ( 'NONE', 3,
 ( #162, #11064, #52929, #869, #64537, #17027, #32527, #38145, #59585, #5448 ),
 .UNSPECIFIED., .F., .F.,
 ( 4, 2, 2, 2, 4 ),
 ( 0.004323147273503695660, 0.005401969756752221172, 0.006480792240000747551, 0.007559614723249273062, 0.008638437206497798573 ),
 .UNSPECIFIED. ) ;
#50982 = DIRECTION ( 'NONE',  ( -1.000000000000000000, -0.000000000000000000, -0.000000000000000000 ) ) ;
#50983 = AXIS2_PLACEMENT_3D ( 'NONE', #54847, #60828, #49562 ) ;
#50984 = CARTESIAN_POINT ( 'NONE',  ( -121.1775535805057444, 43.46577565517554831, -63.40630286045660569 ) ) ;
#50985 = EDGE_LOOP ( 'NONE', ( #21936, #19647, #58082, #8695 ) ) ;
#50986 = LINE ( 'NONE', #2115, #32291 ) ;
#50987 = CARTESIAN_POINT ( 'NONE',  ( 100.0000000000000284, 5.000000000000000000, 18.50000000000000000 ) ) ;
#50988 = CONICAL_SURFACE ( 'NONE', #64479, 75.31295361348104223, 1.273485274044411586 ) ;
#50989 = CARTESIAN_POINT ( 'NONE',  ( 69.73342236697678231, 14.33173522011652068, 60.78623098035528471 ) ) ;
#50990 = CARTESIAN_POINT ( 'NONE',  ( 135.0005116824453921, 43.29964618809725607, 2.749954276746684023 ) ) ;
#50991 = EDGE_CURVE ( 'NONE', #37589, #14950, #44063, .T. ) ;
#50992 = DIRECTION ( 'NONE',  ( 0.9909497617679351444, -0.1342332658176522420, 0.000000000000000000 ) ) ;
#50993 = AXIS2_PLACEMENT_3D ( 'NONE', #47560, #47912, #26813 ) ;
#50994 = ORIENTED_EDGE ( 'NONE', *, *, #43887, .F. ) ;
#50995 = AXIS2_PLACEMENT_3D ( 'NONE', #66799, #61504, #35108 ) ;
#50996 = DIRECTION ( 'NONE',  ( -0.000000000000000000, -0.000000000000000000, -1.000000000000000000 ) ) ;
#50997 = VECTOR ( 'NONE', #31423, 1000.000000000000000 ) ;
#50998 = FACE_OUTER_BOUND ( 'NONE', #34777, .T. ) ;
#50999 = ORIENTED_EDGE ( 'NONE', *, *, #20170, .F. ) ;
#51000 = CARTESIAN_POINT ( 'NONE',  ( 69.72789637502502558, 15.37065610545702121, 60.80231955136558497 ) ) ;
#51001 = CARTESIAN_POINT ( 'NONE',  ( 126.4177291868981428, 37.11054216252123439, 91.72012540680618997 ) ) ;
#51002 = CIRCLE ( 'NONE', #45422, 65.00000000000000000 ) ;
#51003 = EDGE_CURVE ( 'NONE', #7734, #68664, #54971, .T. ) ;
#51004 = ORIENTED_EDGE ( 'NONE', *, *, #48121, .T. ) ;
#51005 = CARTESIAN_POINT ( 'NONE',  ( 160.9097745014957184, 61.67033591969549633, -36.95542617067341240 ) ) ;
#51006 = CARTESIAN_POINT ( 'NONE',  ( 109.9975424824652634, 179.2896996249788799, 369.5505932007772003 ) ) ;
#51007 = CARTESIAN_POINT ( 'NONE',  ( -12.99999999999999822, 84.99999999999998579, 82.99999999999998579 ) ) ;
#51008 = CARTESIAN_POINT ( 'NONE',  ( 444.9999999999999432, -35.00000000000000000, 0.000000000000000000 ) ) ;
#51009 = B_SPLINE_CURVE_WITH_KNOTS ( 'NONE', 3,
 ( #25799, #26131, #47566, #51824, #69022, #20849, #37032, #58470, #10282, #3634, #14541, #11320, #38060, #59161, #43326, #16257, #16944, #1131, #42649, #37713, #48248, #11673, #10978, #27155, #78, #22582, #32446, #64448, #44022, #64105, #48940, #64802, #32788, #427, #65500, #21877, #53875, #48587, #31747, #60215, #5364, #15916, #59504, #58817, #17299, #54220, #42976, #69379 ),
 .UNSPECIFIED., .F., .F.,
 ( 4, 2, 2, 2, 2, 2, 2, 2, 2, 2, 2, 2, 2, 2, 2, 2, 2, 2, 2, 2, 2, 2, 2, 4 ),
 ( 1.734723475976807094E-18, 0.003619254076116414955, 0.004524067595145476843, 0.005428881114174538731, 0.007238508152232685060, 0.008143321671261782510, 0.009048135190290882562, 0.01085776222834906012, 0.01176257574737815496, 0.01266738926640724981, 0.01357220278543634640, 0.01447701630446544124, 0.01538182982349453609, 0.01628664334252363094, 0.01719145686155273273, 0.01809627038058182757, 0.01900108389961092242, 0.01990589741864001727, 0.02171552445669828330, 0.02262033797572741978, 0.02352515149475655626, 0.02533477853281483616, 0.02714440557087311606, 0.02895403260893138903 ),
 .UNSPECIFIED. ) ;
#51010 = ORIENTED_EDGE ( 'NONE', *, *, #64649, .F. ) ;
#51011 = DIRECTION ( 'NONE',  ( -0.000000000000000000, 0.000000000000000000, -1.000000000000000000 ) ) ;
#51012 = CARTESIAN_POINT ( 'NONE',  ( 57.46055693957354293, 12.48011040142442241, 85.95216039237527639 ) ) ;
#51013 = LINE ( 'NONE', #51702, #52277 ) ;
#51014 = CARTESIAN_POINT ( 'NONE',  ( 81.04027388895738682, 18.64386073872847760, -11.45175216555015041 ) ) ;
#51015 = CARTESIAN_POINT ( 'NONE',  ( -174.6851410627011774, 90.41141687855389364, -88.55546965300769102 ) ) ;
#51016 = DIRECTION ( 'NONE',  ( 1.000000000000000000, 0.000000000000000000, 0.000000000000000000 ) ) ;
#51017 = CARTESIAN_POINT ( 'NONE',  ( 126.4754729582248132, 37.14269484129876275, -69.01268951799154650 ) ) ;
#51018 = VERTEX_POINT ( 'NONE', #43371 ) ;
#51019 = CARTESIAN_POINT ( 'NONE',  ( -99.10904156412046007, 32.31949011661291138, 71.67685420465566892 ) ) ;
#51020 = CARTESIAN_POINT ( 'NONE',  ( -14.33576511807126685, 8.413127487936190363, 68.21581748411188073 ) ) ;
#51021 = ORIENTED_EDGE ( 'NONE', *, *, #66117, .T. ) ;
#51022 = CARTESIAN_POINT ( 'NONE',  ( -152.9008427825210958, 68.45483453645053373, -49.00505458194412256 ) ) ;
#51023 = CARTESIAN_POINT ( 'NONE',  ( 204.6977192012829789, 108.0580384837234931, -9.481380442157895772 ) ) ;
#51024 = CARTESIAN_POINT ( 'NONE',  ( -36.89224332184167565, 11.57404295377976311, 32.56159292348578305 ) ) ;
#51025 = DIRECTION ( 'NONE',  ( -0.000000000000000000, -0.000000000000000000, -1.000000000000000000 ) ) ;
#51026 = CARTESIAN_POINT ( 'NONE',  ( -74.69807204964297398, 6.722948167756991111, 0.000000000000000000 ) ) ;
#51027 = CARTESIAN_POINT ( 'NONE',  ( -47.56463531432802228, 12.80077789972090407, -69.07071056560511124 ) ) ;
#51028 = CARTESIAN_POINT ( 'NONE',  ( 205.0999694062794276, 106.8955893716605203, -51.32593103262163226 ) ) ;
#51029 = CARTESIAN_POINT ( 'NONE',  ( 178.4027079424739100, 75.93756746109791322, 16.97168195328412210 ) ) ;
#51030 = CARTESIAN_POINT ( 'NONE',  ( -56.72814287166056602, 15.13700122306437379, 18.28720868321791571 ) ) ;
#51031 = ORIENTED_EDGE ( 'NONE', *, *, #49597, .T. ) ;
#51032 = AXIS2_PLACEMENT_3D ( 'NONE', #32997, #65721, #27713 ) ;
#51033 = CARTESIAN_POINT ( 'NONE',  ( -65.00200000000002376, -1.250000000000021982, 0.000000000000000000 ) ) ;
#51034 = VERTEX_POINT ( 'NONE', #49335 ) ;
#51035 = FILL_AREA_STYLE ('',( #29570 ) ) ;
#51036 = CARTESIAN_POINT ( 'NONE',  ( 43.96062659677687634, 10.06332325923986204, -10.29970569430655303 ) ) ;
#51037 = VECTOR ( 'NONE', #3983, 1000.000000000000227 ) ;
#51038 = CARTESIAN_POINT ( 'NONE',  ( 46.13320811200729565, 9.380653113584040526, 60.91438470745498535 ) ) ;
#51039 = LINE ( 'NONE', #33818, #37868 ) ;
#51040 = LINE ( 'NONE', #7084, #44591 ) ;
#51041 = CARTESIAN_POINT ( 'NONE',  ( -102.7494334820056849, 34.14986869751099618, -8.170026674512229192 ) ) ;
#51042 = VECTOR ( 'NONE', #51320, 1000.000000000000000 ) ;
#51043 = EDGE_CURVE ( 'NONE', #65910, #4577, #21572, .T. ) ;
#51044 = DIRECTION ( 'NONE',  ( 0.000000000000000000, 0.000000000000000000, -1.000000000000000000 ) ) ;
#51045 = CARTESIAN_POINT ( 'NONE',  ( -167.6386155194957723, 81.22597462185137829, 70.30946588916833662 ) ) ;
#51046 = ORIENTED_EDGE ( 'NONE', *, *, #54703, .F. ) ;
#51047 = VERTEX_POINT ( 'NONE', #65543 ) ;
#51048 = AXIS2_PLACEMENT_3D ( 'NONE', #2984, #56431, #40600 ) ;
#51049 = FACE_OUTER_BOUND ( 'NONE', #11237, .T. ) ;
#51050 = DIRECTION ( 'NONE',  ( -0.7071067811865475727, 4.529112861587823989E-16, -0.7071067811865475727 ) ) ;
#51051 = CARTESIAN_POINT ( 'NONE',  ( 173.5837434292113812, 71.34409607026157119, -17.16855947548079442 ) ) ;
#51052 = ADVANCED_FACE ( 'NONE', ( #22274 ), #59891, .T. ) ;
#51053 = CARTESIAN_POINT ( 'NONE',  ( 106.0228389049370605, 28.07756796303168301, 57.75107945049343527 ) ) ;
#51054 = VECTOR ( 'NONE', #41732, 1000.000000000000000 ) ;
#51055 = CARTESIAN_POINT ( 'NONE',  ( 444.9999999999999432, 225.0000000000000000, 2.000000000000000000 ) ) ;
#51056 = CARTESIAN_POINT ( 'NONE',  ( 55.57634120535661992, 12.09544293553729943, -15.39196884852826841 ) ) ;
#51057 = ORIENTED_EDGE ( 'NONE', *, *, #24333, .T. ) ;
#51058 = DIRECTION ( 'NONE',  ( -0.000000000000000000, -0.000000000000000000, -1.000000000000000000 ) ) ;
#51059 = CARTESIAN_POINT ( 'NONE',  ( 18.19858669090299585, 7.596860100017451600, -35.91253959148980357 ) ) ;
#51060 = LINE ( 'NONE', #23638, #28180 ) ;
#51061 = CARTESIAN_POINT ( 'NONE',  ( 25.12245591505646658, 0.000000000000000000, 0.000000000000000000 ) ) ;
#51062 = FACE_BOUND ( 'NONE', #16255, .T. ) ;
#51063 = EDGE_CURVE ( 'NONE', #25778, #46466, #32660, .T. ) ;
#51064 = ADVANCED_FACE ( 'NONE', ( #59201 ), #16643, .F. ) ;
#51065 = ORIENTED_EDGE ( 'NONE', *, *, #14295, .F. ) ;
#51066 = ORIENTED_EDGE ( 'NONE', *, *, #6251, .F. ) ;
#51067 = CARTESIAN_POINT ( 'NONE',  ( 46.66904755831207297, -15.55634918610412853, 85.00100000000000477 ) ) ;
#51068 = DIRECTION ( 'NONE',  ( -0.000000000000000000, 1.000000000000000000, -0.000000000000000000 ) ) ;
#51069 = DIRECTION ( 'NONE',  ( -0.000000000000000000, 1.000000000000000000, -0.000000000000000000 ) ) ;
#51070 = FACE_OUTER_BOUND ( 'NONE', #18906, .T. ) ;
#51071 = ADVANCED_FACE ( 'NONE', ( #16984 ), #826, .F. ) ;
#51072 = DIRECTION ( 'NONE',  ( -0.000000000000000000, -0.000000000000000000, -1.000000000000000000 ) ) ;
#51073 = CARTESIAN_POINT ( 'NONE',  ( -439.4229916354185548, 400.0000000000021032, 96.05029585799300662 ) ) ;
#51074 = VERTEX_POINT ( 'NONE', #16304 ) ;
#51075 = B_SPLINE_CURVE_WITH_KNOTS ( 'NONE', 3,
 ( #68107, #62472, #3385, #47308, #36088, #10039, #19913, #62115 ),
 .UNSPECIFIED., .F., .F.,
 ( 4, 2, 2, 4 ),
 ( 0.004673709593152176531, 0.005837709341827659881, 0.007001709090503144099, 0.009329708587854108198 ),
 .UNSPECIFIED. ) ;
#51076 = DIRECTION ( 'NONE',  ( -0.000000000000000000, 1.000000000000000000, -0.000000000000000000 ) ) ;
#51077 = DIRECTION ( 'NONE',  ( 0.000000000000000000, 1.000000000000000000, -0.000000000000000000 ) ) ;
#51078 = EDGE_LOOP ( 'NONE', ( #1070, #10896 ) ) ;
#51079 = CARTESIAN_POINT ( 'NONE',  ( 8.828807734115068584, -74.48902371486708773, 170.0000000000000000 ) ) ;
#51080 = EDGE_LOOP ( 'NONE', ( #38960, #68220 ) ) ;
#51081 = AXIS2_PLACEMENT_3D ( 'NONE', #34337, #46248, #67727 ) ;
#51082 = CARTESIAN_POINT ( 'NONE',  ( -86.10361028793437299, 25.29528064050657221, -70.46168237689222735 ) ) ;
#51083 = DIRECTION ( 'NONE',  ( 1.000000000000000000, -0.000000000000000000, -0.000000000000000000 ) ) ;
#51084 = DIRECTION ( 'NONE',  ( -0.000000000000000000, -0.000000000000000000, -1.000000000000000000 ) ) ;
#51086 = ORIENTED_EDGE ( 'NONE', *, *, #62806, .T. ) ;
#51085 = EDGE_CURVE ( 'NONE', #7668, #54444, #16425, .T. ) ;
#51087 = VERTEX_POINT ( 'NONE', #48627 ) ;
#51088 = CARTESIAN_POINT ( 'NONE',  ( 42.71247067544612719, 9.879726907348446829, 57.52408926830288038 ) ) ;
#51089 = ADVANCED_FACE ( 'NONE', ( #6085 ), #12487, .T. ) ;
#51091 = EDGE_CURVE ( 'NONE', #45635, #5291, #27543, .T. ) ;
#51090 = CARTESIAN_POINT ( 'NONE',  ( -102.6996017731805750, 34.12480707976105521, -88.71245073017188076 ) ) ;
#51092 = FACE_OUTER_BOUND ( 'NONE', #54021, .T. ) ;
#51093 = EDGE_LOOP ( 'NONE', ( #47074, #41203 ) ) ;
#51094 = AXIS2_PLACEMENT_3D ( 'NONE', #25959, #5188, #5863 ) ;
#51095 = VECTOR ( 'NONE', #19233, 1000.000000000000000 ) ;
#51096 = SURFACE_SIDE_STYLE ('',( #13121 ) ) ;
#51097 = CARTESIAN_POINT ( 'NONE',  ( 173.7263186949344345, 72.85225335320953377, -72.05203316818773374 ) ) ;
#51098 = AXIS2_PLACEMENT_3D ( 'NONE', #57200, #51579, #51231 ) ;
#51099 = DIRECTION ( 'NONE',  ( 0.1785568947986370392, -0.9839295885986295565, 0.000000000000000000 ) ) ;
#51100 = DIRECTION ( 'NONE',  ( -0.000000000000000000, -0.000000000000000000, -1.000000000000000000 ) ) ;
#51101 = CARTESIAN_POINT ( 'NONE',  ( 79.91920957766411959, 18.29292522273510357, -39.93360915899626207 ) ) ;
#51103 = VERTEX_POINT ( 'NONE', #6788 ) ;
#51102 = CARTESIAN_POINT ( 'NONE',  ( -102.2801239173131194, -170.0000000000000000, -96.20367844590329298 ) ) ;
#51104 = ORIENTED_EDGE ( 'NONE', *, *, #65947, .T. ) ;
#51105 = ORIENTED_EDGE ( 'NONE', *, *, #7722, .F. ) ;
#51106 = CARTESIAN_POINT ( 'NONE',  ( 41.80536115778103579, 8.734184316430665618, 3.460590674310346504 ) ) ;
#51107 = LINE ( 'NONE', #8194, #9133 ) ;
#51108 = CARTESIAN_POINT ( 'NONE',  ( -47.95468448182518983, 12.89252559348045679, -13.43679395526418396 ) ) ;
#51109 = CARTESIAN_POINT ( 'NONE',  ( 103.1567541746301657, 25.73937982110324896, -19.08631000368835373 ) ) ;
#51110 = DIRECTION ( 'NONE',  ( 0.000000000000000000, 0.000000000000000000, -1.000000000000000000 ) ) ;
#51111 = DIRECTION ( 'NONE',  ( 1.000000000000000000, 0.000000000000000000, 0.000000000000000000 ) ) ;
#51112 = CARTESIAN_POINT ( 'NONE',  ( 205.5119110209522830, 109.1913085791014453, 82.92244948186888109 ) ) ;
#51113 = CARTESIAN_POINT ( 'NONE',  ( 204.6977192012829505, 108.0580384837234931, 29.20772073876942088 ) ) ;
#51114 = FACE_OUTER_BOUND ( 'NONE', #19741, .T. ) ;
#51115 = CARTESIAN_POINT ( 'NONE',  ( -8.811275908848678284, 6.956777180392053950, 30.16455914700392427 ) ) ;
#51116 = ORIENTED_EDGE ( 'NONE', *, *, #66168, .F. ) ;
#51117 = PLANE ( 'NONE',  #2601 ) ;
#51118 = ORIENTED_EDGE ( 'NONE', *, *, #55020, .F. ) ;
#51119 = EDGE_LOOP ( 'NONE', ( #8528, #46914, #7725, #41131 ) ) ;
#51120 = DIRECTION ( 'NONE',  ( 9.109522253334613014E-16, 1.000000000000000000, -3.889846672687432470E-31 ) ) ;
#51121 = CARTESIAN_POINT ( 'NONE',  ( 188.4918087359956473, 87.93403732562657638, -71.78073924401245165 ) ) ;
#51122 = CARTESIAN_POINT ( 'NONE',  ( -165.7149569557575717, 80.68479365246975021, 39.54250311673061447 ) ) ;
#51123 = CARTESIAN_POINT ( 'NONE',  ( 209.4789161463551750, 113.1367444519304257, -76.45320715356564278 ) ) ;
#51124 = CARTESIAN_POINT ( 'NONE',  ( -26.49928411671542960, 9.848831533840664676, 16.53656075554865623 ) ) ;
#51125 = CARTESIAN_POINT ( 'NONE',  ( 15.55634918610409656, 31.11269837220803325, 0.000000000000000000 ) ) ;
#51126 = EDGE_CURVE ( 'NONE', #49516, #13372, #32482, .T. ) ;
#51127 = DIRECTION ( 'NONE',  ( -0.000000000000000000, 1.000000000000000000, -0.000000000000000000 ) ) ;
#51128 = CARTESIAN_POINT ( 'NONE',  ( 126.4324872316703079, 37.11876756822024959, -42.42733774312184636 ) ) ;
#51129 = ORIENTED_EDGE ( 'NONE', *, *, #40363, .T. ) ;
#51130 = ORIENTED_EDGE ( 'NONE', *, *, #36455, .F. ) ;
#51131 = EDGE_CURVE ( 'NONE', #41805, #10488, #39449, .T. ) ;
#51132 = CIRCLE ( 'NONE', #39926, 21.00000000000000355 ) ;
#51133 = CARTESIAN_POINT ( 'NONE',  ( 188.4735550466079417, 87.91368577883815760, 89.15183869550180873 ) ) ;
#51134 = FACE_OUTER_BOUND ( 'NONE', #8046, .T. ) ;
#51135 = CARTESIAN_POINT ( 'NONE',  ( 217.9999999999999716, 126.6235316737731580, -95.00000000000133582 ) ) ;
#51136 = CARTESIAN_POINT ( 'NONE',  ( -29.02794087136070900, 9.207646203414357799, -62.54324267984874552 ) ) ;
#51137 = AXIS2_PLACEMENT_3D ( 'NONE', #6630, #54807, #17525 ) ;
#51138 = FACE_OUTER_BOUND ( 'NONE', #34305, .T. ) ;
#51139 = VERTEX_POINT ( 'NONE', #26859 ) ;
#51140 = CARTESIAN_POINT ( 'NONE',  ( 39.40195752203892710, 9.424259417798133143, -77.46436805589148378 ) ) ;
#51141 = VECTOR ( 'NONE', #2188, 1000.000000000000000 ) ;
#51142 = B_SPLINE_CURVE_WITH_KNOTS ( 'NONE', 3,
 ( #18339, #33832, #39802, #66901, #34880, #34190, #56319, #8139, #44733, #49640, #1468, #49287 ),
 .UNSPECIFIED., .F., .F.,
 ( 4, 2, 2, 2, 2, 4 ),
 ( 0.000000000000000000, 0.002491861676607965564, 0.004983723353215931129, 0.007475585029823895826, 0.008721515868127872537, 0.009967446706431848380 ),
 .UNSPECIFIED. ) ;
#51143 = CARTESIAN_POINT ( 'NONE',  ( -60.47589866267035319, 17.25153113855768439, -74.74728964359273675 ) ) ;
#51144 = CARTESIAN_POINT ( 'NONE',  ( 197.5344433744249386, 98.61756151884685551, -68.42576040693960238 ) ) ;
#51145 = DIRECTION ( 'NONE',  ( 0.000000000000000000, 0.000000000000000000, 1.000000000000000000 ) ) ;
#51146 = CARTESIAN_POINT ( 'NONE',  ( -51.66904755831210139, 5.000000000000066613, 2.000000000000001776 ) ) ;
#51147 = CARTESIAN_POINT ( 'NONE',  ( -17.36794314067741496, 0.000000000000000000, 24.46128678263259815 ) ) ;
#51148 = LINE ( 'NONE', #40246, #39701 ) ;
#51149 =( GEOMETRIC_REPRESENTATION_CONTEXT ( 3 ) GLOBAL_UNCERTAINTY_ASSIGNED_CONTEXT ( ( #23380 ) ) GLOBAL_UNIT_ASSIGNED_CONTEXT ( ( #49026, #4751, #32522 ) ) REPRESENTATION_CONTEXT ( 'NONE', 'WORKASPACE' ) );
#51150 = EDGE_CURVE ( 'NONE', #48269, #12851, #471, .T. ) ;
#51151 = CARTESIAN_POINT ( 'NONE',  ( -47.61380558691494969, 12.81230778489787347, 65.64890909038182087 ) ) ;
#51152 = VECTOR ( 'NONE', #44774, 1000.000000000000114 ) ;
#51153 = EDGE_CURVE ( 'NONE', #66051, #17861, #57421, .T. ) ;
#51154 = VECTOR ( 'NONE', #30679, 1000.000000000000000 ) ;
#51155 = CARTESIAN_POINT ( 'NONE',  ( -4.081377963939787357, 6.676029627840589065, 57.95687600658722971 ) ) ;
#51156 = EDGE_CURVE ( 'NONE', #18323, #37531, #47429, .T. ) ;
#51157 = VERTEX_POINT ( 'NONE', #45464 ) ;
#51158 = CARTESIAN_POINT ( 'NONE',  ( 275.1286806118793038, 21.97108935923501605, 1.139020068845007838 ) ) ;
#51159 = CARTESIAN_POINT ( 'NONE',  ( 152.6804161981488619, 55.27286404993338920, 57.97779815228713574 ) ) ;
#51160 = PLANE ( 'NONE',  #50080 ) ;
#51161 = CYLINDRICAL_SURFACE ( 'NONE', #23422, 5.000000000000004441 ) ;
#51162 = DIRECTION ( 'NONE',  ( 1.000000000000000000, 0.000000000000000000, 0.000000000000000000 ) ) ;
#51163 = ORIENTED_EDGE ( 'NONE', *, *, #34499, .T. ) ;
#51164 = LINE ( 'NONE', #56786, #34767 ) ;
#51165 = DIRECTION ( 'NONE',  ( -1.000000000000000000, 0.000000000000000000, 0.000000000000000000 ) ) ;
#51166 = VERTEX_POINT ( 'NONE', #7507 ) ;
#51167 = EDGE_LOOP ( 'NONE', ( #68638, #5326, #38186, #30110 ) ) ;
#51168 = LINE ( 'NONE', #57139, #61133 ) ;
#51169 = FACE_OUTER_BOUND ( 'NONE', #55854, .T. ) ;
#51170 = CARTESIAN_POINT ( 'NONE',  ( -36.11269837220812207, -26.11269837220801193, 85.00100000000000477 ) ) ;
#51171 = ORIENTED_EDGE ( 'NONE', *, *, #21650, .T. ) ;
#51172 = LINE ( 'NONE', #51520, #30085 ) ;
#51173 = CARTESIAN_POINT ( 'NONE',  ( -175.9852529046322616, 90.37283472601129120, 18.42162745504879595 ) ) ;
#51174 = CARTESIAN_POINT ( 'NONE',  ( -0.7174461528505752250, 6.532311451815527192, 13.17673894021459446 ) ) ;
#51175 = CARTESIAN_POINT ( 'NONE',  ( -40.27405704175546930, -63.28161525591320924, 170.0000000000000000 ) ) ;
#51176 = EDGE_CURVE ( 'NONE', #17818, #54143, #66598, .T. ) ;
#51178 = ADVANCED_FACE ( 'NONE', ( #8539 ), #28605, .F. ) ;
#51177 = DIRECTION ( 'NONE',  ( -0.9959742939952382912, -0.08963930890344089242, 0.000000000000000000 ) ) ;
#51179 = CARTESIAN_POINT ( 'NONE',  ( 153.4645101005155539, 54.60099007857102293, 84.22599575989748644 ) ) ;
#51180 = CARTESIAN_POINT ( 'NONE',  ( 138.1919700334460970, 44.10401742531043823, 4.027875862906625137 ) ) ;
#51181 = EDGE_CURVE ( 'NONE', #24965, #11879, #2909, .T. ) ;
#51182 = ORIENTED_EDGE ( 'NONE', *, *, #64790, .T. ) ;
#51183 = CARTESIAN_POINT ( 'NONE',  ( 0.000000000000000000, 35.00000000000000000, -27.00000000000000000 ) ) ;
#51184 = VECTOR ( 'NONE', #23767, 1000.000000000000000 ) ;
#51185 = CARTESIAN_POINT ( 'NONE',  ( -71.26746920569851795, 20.70422440535243425, 9.820768664776275969 ) ) ;
#51186 = CARTESIAN_POINT ( 'NONE',  ( -447.6627218934913230, 399.9999999999997726, 83.55029585798818914 ) ) ;
#51187 = CARTESIAN_POINT ( 'NONE',  ( 0.000000000000000000, 0.000000000000000000, -5.000000000000000000 ) ) ;
#51189 = ORIENTED_EDGE ( 'NONE', *, *, #17755, .F. ) ;
#51188 = CARTESIAN_POINT ( 'NONE',  ( -118.9648984637947819, 42.09776532027431273, 94.69885810538663407 ) ) ;
#51190 = CARTESIAN_POINT ( 'NONE',  ( 79.14242532928585661, 17.00090225993928428, -42.81185340043884224 ) ) ;
#51191 = CIRCLE ( 'NONE', #47802, 74.95140232871122521 ) ;
#51192 = VECTOR ( 'NONE', #42991, 1000.000000000000000 ) ;
#51193 = ORIENTED_EDGE ( 'NONE', *, *, #64468, .T. ) ;
#51194 = DIRECTION ( 'NONE',  ( 0.000000000000000000, -0.000000000000000000, 1.000000000000000000 ) ) ;
#51195 = CARTESIAN_POINT ( 'NONE',  ( 188.9999999999999432, 225.0000000000000000, -2.000000000000000888 ) ) ;
#51196 = LINE ( 'NONE', #61395, #20840 ) ;
#51197 = CARTESIAN_POINT ( 'NONE',  ( 0.000000000000000000, 0.000000000000000000, 0.000000000000000000 ) ) ;
#51198 = CARTESIAN_POINT ( 'NONE',  ( -121.2008155373973750, 43.48033530165982796, 59.09401072938392474 ) ) ;
#51199 = CARTESIAN_POINT ( 'NONE',  ( -85.96384504792887071, 26.32782846176033331, -14.02102585345735974 ) ) ;
#51200 = CARTESIAN_POINT ( 'NONE',  ( -180.3114074031035727, 97.09758726817784691, -17.52189378749824300 ) ) ;
#51201 = CIRCLE ( 'NONE', #20859, 65.00000000000000000 ) ;
#51202 = CARTESIAN_POINT ( 'NONE',  ( -51.34562532494748410, 14.75613283840036871, 44.35518551528009112 ) ) ;
#51203 = ORIENTED_EDGE ( 'NONE', *, *, #51156, .F. ) ;
#51204 = APPLICATION_CONTEXT ( 'automotive_design' ) ;
#51205 = ORIENTED_EDGE ( 'NONE', *, *, #30523, .T. ) ;
#51206 = CARTESIAN_POINT ( 'NONE',  ( -109.5157885508426432, 37.76058765671429995, 13.21563288999418617 ) ) ;
#51207 = PLANE ( 'NONE',  #14744 ) ;
#51208 = CARTESIAN_POINT ( 'NONE',  ( 161.7048274740120632, 61.01946783654761219, 57.54637987710646030 ) ) ;
#51209 = CYLINDRICAL_SURFACE ( 'NONE', #21698, 7.500000000000020428 ) ;
#51210 = CARTESIAN_POINT ( 'NONE',  ( 182.5617509987553149, 80.11195108039724744, -51.08114882856880712 ) ) ;
#51211 = CARTESIAN_POINT ( 'NONE',  ( 15.78827728214693416, 6.500811158483284835, 30.01470767270522089 ) ) ;
#51212 = CARTESIAN_POINT ( 'NONE',  ( 160.5141379054754225, 60.05651755415393467, -63.59944546789614606 ) ) ;
#51213 = VERTEX_POINT ( 'NONE', #67626 ) ;
#51214 = ORIENTED_EDGE ( 'NONE', *, *, #46004, .F. ) ;
#51215 = ORIENTED_EDGE ( 'NONE', *, *, #63938, .F. ) ;
#51216 = DIRECTION ( 'NONE',  ( -0.000000000000000000, -0.000000000000000000, -1.000000000000000000 ) ) ;
#51217 = EDGE_CURVE ( 'NONE', #34928, #69323, #29356, .T. ) ;
#51218 = CARTESIAN_POINT ( 'NONE',  ( -71.43680309721476362, 19.69815736714263466, 89.58515710192457959 ) ) ;
#51219 = CARTESIAN_POINT ( 'NONE',  ( 177.6913206243945638, 75.24308051341677128, -90.71550574208795581 ) ) ;
#51220 = CARTESIAN_POINT ( 'NONE',  ( 70.51484748609223630, 14.53801151001411895, -43.73266891657371502 ) ) ;
#51221 = CARTESIAN_POINT ( 'NONE',  ( -74.75133697335806460, 5.472689625386069068, 41.38025477438755928 ) ) ;
#51222 = CARTESIAN_POINT ( 'NONE',  ( -62.29496909743952671, 17.79481128341707930, 39.78269874340612944 ) ) ;
#51223 = CARTESIAN_POINT ( 'NONE',  ( 46.66904755831212981, 20.55634918610394379, 85.00100000000000477 ) ) ;
#51224 = CARTESIAN_POINT ( 'NONE',  ( 58.08938767906775524, 12.61185010801510131, 42.98944077952003084 ) ) ;
#51225 = CARTESIAN_POINT ( 'NONE',  ( 40.71722863567654827, 8.584032429807034958, 83.71188065785378285 ) ) ;
#51226 =( NAMED_UNIT ( * ) SI_UNIT ( $, .STERADIAN. ) SOLID_ANGLE_UNIT ( ) );
#51227 = ORIENTED_EDGE ( 'NONE', *, *, #13459, .T. ) ;
#51228 = CYLINDRICAL_SURFACE ( 'NONE', #67724, 7.500000000000020428 ) ;
#51229 = DIRECTION ( 'NONE',  ( -9.729521028634720986E-15, 5.551115123125782702E-17, -1.000000000000000000 ) ) ;
#51230 = CARTESIAN_POINT ( 'NONE',  ( -190.6985136298602015, 109.1272424661243434, -37.65993730791821292 ) ) ;
#51231 = DIRECTION ( 'NONE',  ( 1.000000000000000000, 0.000000000000000000, 0.000000000000000000 ) ) ;
#51232 = DIRECTION ( 'NONE',  ( -0.2225209339563184729, 0.9749279121818227312, 0.000000000000000000 ) ) ;
#51233 = EDGE_CURVE ( 'NONE', #21755, #16701, #24892, .T. ) ;
#51234 = CARTESIAN_POINT ( 'NONE',  ( 19.11382977197791888, 7.636807742668410448, -9.434045545063515448 ) ) ;
#51235 = CARTESIAN_POINT ( 'NONE',  ( 198.3926538463958593, 98.07933330386025261, 67.65304937739811919 ) ) ;
#51236 = AXIS2_PLACEMENT_3D ( 'NONE', #33554, #24382, #56374 ) ;
#51237 = ADVANCED_FACE ( 'NONE', ( #60604 ), #50054, .T. ) ;
#51238 = EDGE_CURVE ( 'NONE', #60669, #17123, #41917, .T. ) ;
#51239 = EDGE_LOOP ( 'NONE', ( #54567, #55589 ) ) ;
#51240 = AXIS2_PLACEMENT_3D ( 'NONE', #64694, #44630, #1368 ) ;
#51241 = DIRECTION ( 'NONE',  ( 0.000000000000000000, 0.000000000000000000, 1.000000000000000000 ) ) ;
#51242 = DIRECTION ( 'NONE',  ( -0.000000000000000000, 1.000000000000000000, -0.000000000000000000 ) ) ;
#51243 = CARTESIAN_POINT ( 'NONE',  ( -125.8938041572051105, 46.49392987655492959, 3.775397282693376599 ) ) ;
#51244 = CARTESIAN_POINT ( 'NONE',  ( -442.6627218934912662, 394.9999999999998295, 92.24186470396634263 ) ) ;
#51245 = EDGE_CURVE ( 'NONE', #38218, #5375, #40712, .T. ) ;
#51246 = CARTESIAN_POINT ( 'NONE',  ( -170.0422773253271203, 83.76581591185905040, 85.16679510493294458 ) ) ;
#51247 = VERTEX_POINT ( 'NONE', #20453 ) ;
#51249 = CARTESIAN_POINT ( 'NONE',  ( 209.9999999999999716, -57.00000000000007816, 72.99999999999998579 ) ) ;
#51248 = VECTOR ( 'NONE', #65234, 1000.000000000000000 ) ;
#51250 = VECTOR ( 'NONE', #62410, 1000.000000000000000 ) ;
#51251 = AXIS2_PLACEMENT_3D ( 'NONE', #42139, #48771, #609 ) ;
#51252 = EDGE_LOOP ( 'NONE', ( #53314, #6889, #1414, #42592 ) ) ;
#51253 = FACE_BOUND ( 'NONE', #36359, .T. ) ;
#51254 = CIRCLE ( 'NONE', #37720, 246.3582898394606957 ) ;
#51255 = CARTESIAN_POINT ( 'NONE',  ( -15.55634918610396866, 31.11269837220809009, 0.000000000000000000 ) ) ;
#51256 = ORIENTED_EDGE ( 'NONE', *, *, #25060, .T. ) ;
#51257 = VECTOR ( 'NONE', #7695, 1000.000000000000000 ) ;
#51258 = CARTESIAN_POINT ( 'NONE',  ( 160.7775378522616450, 61.56282986428943360, 83.85992522728291476 ) ) ;
#51259 = ORIENTED_EDGE ( 'NONE', *, *, #65354, .T. ) ;
#51260 = DIRECTION ( 'NONE',  ( -0.8345732537213078617, 0.5508969814520945363, 0.000000000000000000 ) ) ;
#51261 = DIRECTION ( 'NONE',  ( 2.921639538487254261E-16, 1.134144525784205431E-35, 1.000000000000000000 ) ) ;
#51262 = CARTESIAN_POINT ( 'NONE',  ( -151.6797345123118532, 67.37848486615945376, 45.41297040107649252 ) ) ;
#51263 = DIRECTION ( 'NONE',  ( 1.000000000000000000, 0.000000000000000000, 0.000000000000000000 ) ) ;
#51264 = CARTESIAN_POINT ( 'NONE',  ( -20.06363881723563480, 32.66414036569511836, 13.32819397642332682 ) ) ;
#51266 = ORIENTED_EDGE ( 'NONE', *, *, #6338, .T. ) ;
#51265 = CARTESIAN_POINT ( 'NONE',  ( 204.6977192012829789, 106.3443248447423457, 44.20772073876944575 ) ) ;
#51267 = EDGE_CURVE ( 'NONE', #13791, #36942, #30678, .T. ) ;
#51268 = CARTESIAN_POINT ( 'NONE',  ( 56.19513604272051310, 11.19349063094192687, 40.44209435148105314 ) ) ;
#51269 = ORIENTED_EDGE ( 'NONE', *, *, #37012, .T. ) ;
#51270 = ORIENTED_EDGE ( 'NONE', *, *, #1113, .F. ) ;
#51271 = CARTESIAN_POINT ( 'NONE',  ( -165.9154624515710168, 80.89088623112733956, 13.57877339069360900 ) ) ;
#51272 = CARTESIAN_POINT ( 'NONE',  ( 21.73827885904430701, 6.764046335627709183, -74.43606220462095280 ) ) ;
#51274 = VERTEX_POINT ( 'NONE', #47874 ) ;
#51273 = CARTESIAN_POINT ( 'NONE',  ( -128.7724923851857852, 49.63576597317773320, 71.89386820983963844 ) ) ;
#51275 = CARTESIAN_POINT ( 'NONE',  ( -97.82962700614261564, 31.69462283565845695, 85.66353045367125674 ) ) ;
#51276 = CARTESIAN_POINT ( 'NONE',  ( -75.00452312211128003, 22.03104735285380400, -49.16518778111800714 ) ) ;
#51277 = ORIENTED_EDGE ( 'NONE', *, *, #27448, .T. ) ;
#51278 = B_SPLINE_CURVE_WITH_KNOTS ( 'NONE', 3,
 ( #43902, #17889, #66445, #22812, #18232, #39003, #65383, #7339, #23169, #33725, #60447, #55874, #44616, #54450, #55157, #16827, #50243, #6632, #39344, #27732, #28795, #28080, #22461, #65736, #29136, #6279, #17171, #38643, #39687, #50587, #49885, #60084, #60787, #12610, #11906, #33383, #34071, #54809, #2408, #55512, #61145, #12968, #23863, #45305 ),
 .UNSPECIFIED., .F., .F.,
 ( 4, 2, 2, 2, 2, 2, 2, 2, 2, 2, 2, 2, 2, 2, 2, 2, 2, 2, 2, 2, 2, 4 ),
 ( 7.152448122690996019E-18, 0.001476829494128853752, 0.002215244241193284423, 0.002953658988257715744, 0.004430488482386571447, 0.005907317976515427151, 0.007384147470644282854, 0.008122562217708703333, 0.008860976964773122078, 0.01033780645890195089, 0.01181463595303078144, 0.01255305070009518631, 0.01329146544715958944, 0.01476829494128840091, 0.01550670968835280925, 0.01624512443541721585, 0.01772195392954603946, 0.01919878342367485960, 0.01993719817073927661, 0.02067561291780369362, 0.02215244241193250682, 0.02362927190606132002 ),
 .UNSPECIFIED. ) ;
#51279 = CARTESIAN_POINT ( 'NONE',  ( 209.6642862813004626, 115.2127693334913658, -76.30817762714391961 ) ) ;
#51280 = VECTOR ( 'NONE', #31057, 1000.000000000000000 ) ;
#51281 = CARTESIAN_POINT ( 'NONE',  ( 15.55634918610403261, -3.079134169858832593E-14, 85.00100000000000477 ) ) ;
#51282 = LINE ( 'NONE', #50926, #53821 ) ;
#51283 = CARTESIAN_POINT ( 'NONE',  ( -132.4896623150434323, 52.22616402022728721, 14.85463847962715356 ) ) ;
#51284 = CARTESIAN_POINT ( 'NONE',  ( 63.01563776193090405, 13.70579113808097382, -62.56524142263340593 ) ) ;
#51285 = ORIENTED_EDGE ( 'NONE', *, *, #53580, .F. ) ;
#51286 = ORIENTED_EDGE ( 'NONE', *, *, #8768, .T. ) ;
#51287 = VECTOR ( 'NONE', #19547, 999.9999999999998863 ) ;
#51288 = CARTESIAN_POINT ( 'NONE',  ( -142.1332311300252798, 59.44822332309654911, -16.86392425921542682 ) ) ;
#51289 = CARTESIAN_POINT ( 'NONE',  ( -4.999999999999971578, 15.55634918610403084, 0.000000000000000000 ) ) ;
#51290 = AXIS2_PLACEMENT_3D ( 'NONE', #22333, #33248, #4768 ) ;
#51291 = ADVANCED_FACE ( 'NONE', ( #40880 ), #62341, .F. ) ;
#51292 = CARTESIAN_POINT ( 'NONE',  ( -49.09658814250866499, 13.16488830565666390, -91.82710492038845018 ) ) ;
#51293 = DIRECTION ( 'NONE',  ( -0.8584487936018655452, -0.5128992774059070170, 0.000000000000000000 ) ) ;
#51294 = B_SPLINE_CURVE_WITH_KNOTS ( 'NONE', 3,
 ( #47057, #36162, #47732, #8751, #4496, #46710, #69195, #19990, #42466, #31240, #4832, #63584, #15053, #68514, #46355, #9434, #30889, #51652, #68186, #41442, #42125, #14366, #20322, #52336, #15397, #36856, #36506, #57958, #9779, #52670, #25956, #3461, #47387, #68844, #58296, #67837, #31572, #53007, #26304, #19634, #21021, #63926, #62556 ),
 .UNSPECIFIED., .F., .F.,
 ( 4, 2, 2, 2, 2, 2, 2, 2, 2, 2, 2, 2, 1, 2, 2, 2, 2, 2, 2, 2, 2, 4 ),
 ( 0.02358007599568756954, 0.02505677178601661836, 0.02579511968118113757, 0.02653346757634565331, 0.02801016336667470560, 0.02948685915700375443, 0.03022520705216828404, 0.03096355494733281366, 0.03244025073766187289, 0.03391694652799093213, 0.03539364231831998442, 0.03613199021348451057, 0.03687033810864902977, 0.03760868600381355592, 0.03834703389897807513, 0.03982372968930711354, 0.04130042547963615196, 0.04277712126996519038, 0.04351546916512971652, 0.04425381706029422879, 0.04573051285062329496, 0.04720720864095235419 ),
 .UNSPECIFIED. ) ;
#51295 = LINE ( 'NONE', #6983, #61743 ) ;
#51296 = ADVANCED_FACE ( 'NONE', ( #25755 ), #36649, .F. ) ;
#51297 = CARTESIAN_POINT ( 'NONE',  ( 49.35746990687617597, -44.78219184840987310, 34.48241795236666718 ) ) ;
#51298 = CARTESIAN_POINT ( 'NONE',  ( 206.2980740120524104, 108.5619562183279925, 56.21387322886499049 ) ) ;
#51300 = ORIENTED_EDGE ( 'NONE', *, *, #54829, .T. ) ;
#51299 = EDGE_CURVE ( 'NONE', #37153, #10970, #54532, .T. ) ;
#51301 = CARTESIAN_POINT ( 'NONE',  ( -109.7686203588201153, 37.90089348911613598, 38.51078262366649341 ) ) ;
#51302 = ORIENTED_EDGE ( 'NONE', *, *, #15901, .F. ) ;
#51304 = AXIS2_PLACEMENT_3D ( 'NONE', #67242, #25703, #24322 ) ;
#51303 = CARTESIAN_POINT ( 'NONE',  ( -179.9818533554779094, 95.10411966562014641, -92.82201583766619990 ) ) ;
#51305 = EDGE_CURVE ( 'NONE', #62204, #62313, #37668, .T. ) ;
#51306 = CARTESIAN_POINT ( 'NONE',  ( 82.14396250120410059, 18.99560174459420736, 58.04072448712305743 ) ) ;
#51307 = ORIENTED_EDGE ( 'NONE', *, *, #48, .F. ) ;
#51308 = CARTESIAN_POINT ( 'NONE',  ( 0.000000000000000000, 0.000000000000000000, -9.500000000000000000 ) ) ;
#51309 = CARTESIAN_POINT ( 'NONE',  ( 11.98601804829806561, 14.28438006995821219, -38.01398195170192906 ) ) ;
#51310 = FACE_OUTER_BOUND ( 'NONE', #1233, .T. ) ;
#51311 = CARTESIAN_POINT ( 'NONE',  ( -1.224646799147352468E-15, 16.00000000000000000, -5.803681084894614095 ) ) ;
#51312 = CARTESIAN_POINT ( 'NONE',  ( 33.03621582719335237, 7.666716336587112046, 6.595962476436807442 ) ) ;
#51313 = DIRECTION ( 'NONE',  ( -0.000000000000000000, 1.000000000000000000, -0.000000000000000000 ) ) ;
#51314 = CARTESIAN_POINT ( 'NONE',  ( 150.5550643769628323, 52.46819381604269239, -46.53967426915813377 ) ) ;
#51315 = ORIENTED_EDGE ( 'NONE', *, *, #4290, .T. ) ;
#51316 = FACE_OUTER_BOUND ( 'NONE', #19960, .T. ) ;
#51317 = ORIENTED_EDGE ( 'NONE', *, *, #28417, .T. ) ;
#51318 = DIRECTION ( 'NONE',  ( -0.000000000000000000, -0.000000000000000000, -1.000000000000000000 ) ) ;
#51319 = CARTESIAN_POINT ( 'NONE',  ( -62.55184817504200367, 17.87278652436700099, 64.14626842136314622 ) ) ;
#51320 = DIRECTION ( 'NONE',  ( 0.000000000000000000, 0.000000000000000000, -1.000000000000000000 ) ) ;
#51321 = ORIENTED_EDGE ( 'NONE', *, *, #27286, .F. ) ;
#51322 = CARTESIAN_POINT ( 'NONE',  ( -25.87147652227456263, 70.00000000000000000, 77.58025477438755502 ) ) ;
#51323 = DIRECTION ( 'NONE',  ( 0.000000000000000000, -0.7071067811865474617, 0.7071067811865474617 ) ) ;
#51324 = DIRECTION ( 'NONE',  ( 0.000000000000000000, -1.000000000000000000, 0.000000000000000000 ) ) ;
#51325 = DIRECTION ( 'NONE',  ( -0.000000000000000000, -0.000000000000000000, -1.000000000000000000 ) ) ;
#51326 = EDGE_CURVE ( 'NONE', #28608, #40972, #20357, .T. ) ;
#51327 = ADVANCED_FACE ( 'NONE', ( #22190 ), #69337, .F. ) ;
#51328 = EDGE_LOOP ( 'NONE', ( #23340, #47990, #16904, #41641 ) ) ;
#51329 = CARTESIAN_POINT ( 'NONE',  ( -64.56490074351019359, -16.52204994353465395, 34.48241795236665297 ) ) ;
#51330 = CARTESIAN_POINT ( 'NONE',  ( -118.3960663196801306, 41.75130200162920602, 37.55200035001683290 ) ) ;
#51331 = CARTESIAN_POINT ( 'NONE',  ( 149.5448925222589196, -64.85527483330767495, 0.000000000000000000 ) ) ;
#51332 = ORIENTED_EDGE ( 'NONE', *, *, #63163, .F. ) ;
#51333 = CARTESIAN_POINT ( 'NONE',  ( -177.1381400275772080, 93.26609858452818003, -75.40501691932175277 ) ) ;
#51334 = CARTESIAN_POINT ( 'NONE',  ( 90.30166390191402570, 20.70652093100730440, 57.49911369470580524 ) ) ;
#51335 = PRODUCT_DEFINITION_SHAPE ( 'NONE', 'NONE',  #69577 ) ;
#51336 = CARTESIAN_POINT ( 'NONE',  ( 199.7286177451876199, 101.4075663537892069, -22.61804941524460233 ) ) ;
#51337 = VECTOR ( 'NONE', #42124, 1000.000000000000000 ) ;
#51338 = CARTESIAN_POINT ( 'NONE',  ( 15.55634918610400241, -10.55634918610406281, 85.00100000000000477 ) ) ;
#51339 = ORIENTED_EDGE ( 'NONE', *, *, #35244, .T. ) ;
#51340 = CARTESIAN_POINT ( 'NONE',  ( 200.8410151090926661, 101.2014854111317419, 43.15449351457530014 ) ) ;
#51341 = DIRECTION ( 'NONE',  ( 0.000000000000000000, 0.000000000000000000, 1.000000000000000000 ) ) ;
#51342 = AXIS2_PLACEMENT_3D ( 'NONE', #41794, #30896, #4164 ) ;
#51343 = CARTESIAN_POINT ( 'NONE',  ( 70.51484748609223630, 14.53801151001409409, 63.64553344528102485 ) ) ;
#51344 = CARTESIAN_POINT ( 'NONE',  ( 184.5165707593032209, 82.14321753839030293, -90.70306685600688468 ) ) ;
#51345 = CARTESIAN_POINT ( 'NONE',  ( -22.50000000000003197, 207.5000000000000284, -2.000000000000000000 ) ) ;
#51346 = ORIENTED_EDGE ( 'NONE', *, *, #5092, .F. ) ;
#51347 = CONICAL_SURFACE ( 'NONE', #29999, 74.99999999999998579, 0.6747409422235518539 ) ;
#51348 = B_SPLINE_CURVE_WITH_KNOTS ( 'NONE', 3,
 ( #65570, #60975, #23698, #45140, #34258, #66620, #18416, #54647, #27921, #49010, #847, #49360, #22299, #43737, #1194, #17359, #38838, #60286, #12099, #33569, #30015, #2936, #4567, #58367, #35291, #8212, #42206, #26031, #26376, #56746, #51475, #13152, #14181, #45488, #13489, #52741, #3285, #8564, #2588, #29319, #19104, #40221, #67318, #63667 ),
 .UNSPECIFIED., .F., .F.,
 ( 4, 2, 2, 2, 2, 2, 2, 2, 2, 2, 2, 2, 2, 2, 2, 2, 2, 2, 2, 2, 2, 4 ),
 ( 0.02495775893651561508, 0.02650251144344301438, 0.02804726395037041367, 0.02959201645729781296, 0.03113676896422521226, 0.03268152147115261502, 0.03345389772461631467, 0.03422627397808002125, 0.03577102648500744136, 0.03654340273847116183, 0.03731577899193488229, 0.03808815524539860276, 0.03886053149886233016, 0.04040528400578975721, 0.04117766025925346379, 0.04195003651271717038, 0.04349478901964456967, 0.04503954152657196897, 0.04581191778003566861, 0.04658429403349936826, 0.04812904654042682306, 0.04967379904735427093 ),
 .UNSPECIFIED. ) ;
#51349 = CARTESIAN_POINT ( 'NONE',  ( 163.5944442552010401, 63.88381951184481267, -12.44276307209138821 ) ) ;
#51350 = ORIENTED_EDGE ( 'NONE', *, *, #33944, .T. ) ;
#51351 = VECTOR ( 'NONE', #45648, 1000.000000000000000 ) ;
#51352 = CARTESIAN_POINT ( 'NONE',  ( 48.39383208188382213, 43.94028683479088926, 41.38025477438755928 ) ) ;
#51353 = CARTESIAN_POINT ( 'NONE',  ( 133.6177090015579267, 41.28025736076558161, 83.19673575245394659 ) ) ;
#51355 = ORIENTED_EDGE ( 'NONE', *, *, #54278, .F. ) ;
#51354 = CARTESIAN_POINT ( 'NONE',  ( -450.6627218934913230, 217.8591479523843475, 78.55029585798814651 ) ) ;
#51356 = CARTESIAN_POINT ( 'NONE',  ( -148.6409722988650515, 63.44808865916662199, -61.70444773994812238 ) ) ;
#51357 = CARTESIAN_POINT ( 'NONE',  ( 429.8372781065086770, 400.0000000000109708, 101.0502958579843948 ) ) ;
#51358 = CARTESIAN_POINT ( 'NONE',  ( 164.0158927577712689, 62.92463143894070043, -47.32386914606765771 ) ) ;
#51359 = ORIENTED_EDGE ( 'NONE', *, *, #38041, .T. ) ;
#51360 = FACE_OUTER_BOUND ( 'NONE', #42997, .T. ) ;
#51361 = DIRECTION ( 'NONE',  ( -0.5508969814520944253, -0.8345732537213078617, 0.000000000000000000 ) ) ;
#51362 = CARTESIAN_POINT ( 'NONE',  ( 26.11269837220806167, -6.375108774214766072E-14, 85.00100000000000477 ) ) ;
#51363 = CARTESIAN_POINT ( 'NONE',  ( 7.762887554996211747E-14, 46.66904755831208718, 0.000000000000000000 ) ) ;
#51364 = CARTESIAN_POINT ( 'NONE',  ( -178.7653014892675571, 95.21116012989124044, -90.95673312123581411 ) ) ;
#51365 = CARTESIAN_POINT ( 'NONE',  ( -144.2204146883836415, 59.82124005924111998, -90.66219284191375039 ) ) ;
#51366 = CARTESIAN_POINT ( 'NONE',  ( 94.06699947028484132, 23.17027898120150908, 36.21459868573237628 ) ) ;
#51367 = ORIENTED_EDGE ( 'NONE', *, *, #8041, .F. ) ;
#51368 = DIRECTION ( 'NONE',  ( 0.000000000000000000, 0.000000000000000000, -1.000000000000000000 ) ) ;
#51369 = FACE_OUTER_BOUND ( 'NONE', #25836, .T. ) ;
#51370 = ORIENTED_EDGE ( 'NONE', *, *, #52765, .T. ) ;
#51371 = CARTESIAN_POINT ( 'NONE',  ( 154.4435090467314069, 56.59612921827835663, -9.913691618128661176 ) ) ;
#51372 = EDGE_CURVE ( 'NONE', #66025, #5466, #22616, .T. ) ;
#51373 = CARTESIAN_POINT ( 'NONE',  ( -0.6225858422299265227, 41.72441810409881668, 13.79046340968177731 ) ) ;
#51374 = CARTESIAN_POINT ( 'NONE',  ( -37.93983213483221562, 11.77368372188049683, 41.48890555333869656 ) ) ;
#51375 = CARTESIAN_POINT ( 'NONE',  ( -157.0069704378502138, 70.81086990254192415, -68.57520080848023269 ) ) ;
#51376 = CONICAL_SURFACE ( 'NONE', #19944, 8.000000000000000000, 1.047197551196600296 ) ;
#51377 = CARTESIAN_POINT ( 'NONE',  ( 55.52382973330894345, 11.05893590846274499, 90.51414599712177278 ) ) ;
#51378 = CARTESIAN_POINT ( 'NONE',  ( -51.35181696773308602, 13.72007042346227834, -76.10265169357263915 ) ) ;
#51379 = DIRECTION ( 'NONE',  ( -0.9959742939952382912, -0.08963930890344087854, 0.000000000000000000 ) ) ;
#51380 = EDGE_CURVE ( 'NONE', #53918, #3968, #16562, .T. ) ;
#51381 = DIRECTION ( 'NONE',  ( 0.000000000000000000, 1.000000000000000000, -0.000000000000000000 ) ) ;
#51382 = DIRECTION ( 'NONE',  ( -0.9959742939952397345, 0.08963930890342655666, 0.000000000000000000 ) ) ;
#51383 = ORIENTED_EDGE ( 'NONE', *, *, #42878, .T. ) ;
#51384 = CIRCLE ( 'NONE', #47984, 85.31295361348101380 ) ;
#51385 = CARTESIAN_POINT ( 'NONE',  ( 183.2136430849848239, 6.000000000000000000, -9.435653166495541200 ) ) ;
#51387 = VERTEX_POINT ( 'NONE', #59464 ) ;
#51386 = EDGE_CURVE ( 'NONE', #68402, #39331, #16214, .T. ) ;
#51388 = CARTESIAN_POINT ( 'NONE',  ( 102.7571040248400749, 25.57023079238895491, -69.73951755044804202 ) ) ;
#51389 = LINE ( 'NONE', #45760, #41091 ) ;
#51390 = AXIS2_PLACEMENT_3D ( 'NONE', #24417, #41616, #52171 ) ;
#51391 = CARTESIAN_POINT ( 'NONE',  ( 41.33692564073609077, 8.668977654195472837, 57.00815978476482115 ) ) ;
#51392 = DIRECTION ( 'NONE',  ( 0.9839295885986321100, -0.1785568947986229116, 0.000000000000000000 ) ) ;
#51393 = ADVANCED_FACE ( 'NONE', ( #48205 ), #379, .F. ) ;
#51394 = CARTESIAN_POINT ( 'NONE',  ( -3.819748713895199099, 6.663105659409133352, 84.95562319304882237 ) ) ;
#51395 = AXIS2_PLACEMENT_3D ( 'NONE', #11100, #65267, #48362 ) ;
#51396 = CARTESIAN_POINT ( 'NONE',  ( -108.6622665321723247, 37.28993738537008795, -19.61751752820619643 ) ) ;
#51397 = ORIENTED_EDGE ( 'NONE', *, *, #12100, .T. ) ;
#51399 = VECTOR ( 'NONE', #48894, 1000.000000000000000 ) ;
#51398 = LINE ( 'NONE', #24323, #10596 ) ;
#51400 = CARTESIAN_POINT ( 'NONE',  ( -168.7150276173048269, 82.35404041280330034, 71.25389808330632491 ) ) ;
#51401 = ORIENTED_EDGE ( 'NONE', *, *, #39554, .T. ) ;
#51402 = ORIENTED_EDGE ( 'NONE', *, *, #31301, .F. ) ;
#51403 = PLANE ( 'NONE',  #30956 ) ;
#51404 = CARTESIAN_POINT ( 'NONE',  ( -12.77952633087662093, -21.62918162951127243, 3.061616997868437868E-16 ) ) ;
#51405 = CARTESIAN_POINT ( 'NONE',  ( 174.1364721914477229, 71.85829564941442982, -19.71991761371826968 ) ) ;
#51406 = CARTESIAN_POINT ( 'NONE',  ( 103.4725384926517222, 26.96797537091728003, 60.71934963752268999 ) ) ;
#51407 = CARTESIAN_POINT ( 'NONE',  ( 157.4703587214989398, -170.0000000000000000, -36.12418429913763163 ) ) ;
#51408 = ADVANCED_FACE ( 'NONE', ( #43977 ), #64401, .F. ) ;
#51409 = CARTESIAN_POINT ( 'NONE',  ( 61.09977118998601497, 13.26754120022606465, -23.63138592492630252 ) ) ;
#51410 = VERTEX_POINT ( 'NONE', #48896 ) ;
#51411 = CIRCLE ( 'NONE', #62799, 75.31295361348099959 ) ;
#51412 = CARTESIAN_POINT ( 'NONE',  ( 0.000000000000000000, 0.000000000000000000, 2.000000000000001776 ) ) ;
#51413 = VERTEX_POINT ( 'NONE', #33457 ) ;
#51414 = CARTESIAN_POINT ( 'NONE',  ( 19.10949903373832370, 7.636938177523842519, -49.74798475061973591 ) ) ;
#51415 = CARTESIAN_POINT ( 'NONE',  ( 9.045716588192245666, 7.384596431530731309, 67.68043104435533053 ) ) ;
#51416 = FILL_AREA_STYLE ('',( #50007 ) ) ;
#51417 = FACE_BOUND ( 'NONE', #3186, .T. ) ;
#51418 = ORIENTED_EDGE ( 'NONE', *, *, #20108, .F. ) ;
#51419 = ORIENTED_EDGE ( 'NONE', *, *, #33436, .F. ) ;
#51420 = DIRECTION ( 'NONE',  ( 0.000000000000000000, 0.000000000000000000, 1.000000000000000000 ) ) ;
#51421 = CARTESIAN_POINT ( 'NONE',  ( 64.98797965777978902, -1.250000000000021760, 40.00000000000003553 ) ) ;
#51422 = CARTESIAN_POINT ( 'NONE',  ( 33.93974911725172205, 8.773765372885563352, -75.10966096496471778 ) ) ;
#51423 = CARTESIAN_POINT ( 'NONE',  ( -173.9617926765112941, 89.58633395456783433, 18.94172030153162112 ) ) ;
#51424 = CARTESIAN_POINT ( 'NONE',  ( 15.46104383007058658, 6.490338125820253268, 83.70377566018196092 ) ) ;
#51425 = CARTESIAN_POINT ( 'NONE',  ( 22.84562496400137022, 7.837215652665284082, 93.82577997359511812 ) ) ;
#51426 = AXIS2_PLACEMENT_3D ( 'NONE', #9289, #8258, #29711 ) ;
#51427 = ORIENTED_EDGE ( 'NONE', *, *, #14986, .F. ) ;
#51428 = DIRECTION ( 'NONE',  ( -0.000000000000000000, -0.000000000000000000, 1.000000000000000000 ) ) ;
#51429 = CARTESIAN_POINT ( 'NONE',  ( 198.7123879174244507, 100.1053816708572413, -48.35335775156385552 ) ) ;
#51430 = VERTEX_POINT ( 'NONE', #28152 ) ;
#51432 = CARTESIAN_POINT ( 'NONE',  ( 60.40479419793796012, -24.00543350795315334, 40.00000000000003553 ) ) ;
#51431 = AXIS2_PLACEMENT_3D ( 'NONE', #35658, #36001, #68686 ) ;
#51433 = ORIENTED_EDGE ( 'NONE', *, *, #63021, .F. ) ;
#51434 = CARTESIAN_POINT ( 'NONE',  ( -86.06016868996614733, 25.27707703029501474, -68.17648637259551947 ) ) ;
#51435 = DIRECTION ( 'NONE',  ( -1.000000000000000000, 0.000000000000000000, 0.000000000000000000 ) ) ;
#51436 = ORIENTED_EDGE ( 'NONE', *, *, #19719, .T. ) ;
#51437 = VECTOR ( 'NONE', #49212, 1000.000000000000000 ) ;
#51438 = ORIENTED_EDGE ( 'NONE', *, *, #51217, .T. ) ;
#51439 = CARTESIAN_POINT ( 'NONE',  ( 9.416656162223558724, 6.380306691996770141, -39.05494724020170594 ) ) ;
#51440 = CARTESIAN_POINT ( 'NONE',  ( 410.0000000000000000, 0.000000000000000000, 0.000000000000000000 ) ) ;
#51441 = AXIS2_PLACEMENT_3D ( 'NONE', #2998, #7227, #30412 ) ;
#51442 = CARTESIAN_POINT ( 'NONE',  ( 427.4999999999999432, 207.5000000000000284, 378.0000000000000000 ) ) ;
#51443 = ORIENTED_EDGE ( 'NONE', *, *, #45101, .T. ) ;
#51444 = ADVANCED_FACE ( 'NONE', ( #21160 ), #5996, .T. ) ;
#51445 = DIRECTION ( 'NONE',  ( -0.000000000000000000, 1.000000000000000000, -0.000000000000000000 ) ) ;
#51446 = VECTOR ( 'NONE', #29995, 1000.000000000000000 ) ;
#51447 = CARTESIAN_POINT ( 'NONE',  ( 181.0840389613909736, 80.03940679743416808, -78.06960825634331513 ) ) ;
#51448 = DIRECTION ( 'NONE',  ( -1.000000000000000000, 0.000000000000000000, 0.000000000000000000 ) ) ;
#51449 = CARTESIAN_POINT ( 'NONE',  ( 410.9216045519012823, 190.0000000000000000, 173.9247703311572764 ) ) ;
#51450 = CARTESIAN_POINT ( 'NONE',  ( 63.01563776193091826, -170.0000000000000000, 71.65751152968501003 ) ) ;
#51451 = LINE ( 'NONE', #61304, #28755 ) ;
#51452 = VERTEX_POINT ( 'NONE', #58770 ) ;
#51453 = VERTEX_POINT ( 'NONE', #16903 ) ;
#51454 = CARTESIAN_POINT ( 'NONE',  ( 44.35071890818839790, 9.104600422692259443, 16.22605661256570997 ) ) ;
#51455 = CARTESIAN_POINT ( 'NONE',  ( 180.6713229637342693, 79.61878926895391828, 2.464043515047720678 ) ) ;
#51456 = FACE_OUTER_BOUND ( 'NONE', #48566, .T. ) ;
#51457 = DIRECTION ( 'NONE',  ( -1.000000000000000000, -1.001918046209079887E-14, 9.729495617646301779E-15 ) ) ;
#51458 = CARTESIAN_POINT ( 'NONE',  ( 134.6141278563448225, 41.88200982625879476, -89.71241211332302612 ) ) ;
#51459 = DIRECTION ( 'NONE',  ( -0.000000000000000000, 0.000000000000000000, -1.000000000000000000 ) ) ;
#51460 = CARTESIAN_POINT ( 'NONE',  ( 209.9330698459270366, 115.6170919607588985, 85.01721959398543049 ) ) ;
#51461 = EDGE_CURVE ( 'NONE', #35105, #56882, #27813, .T. ) ;
#51462 = DIRECTION ( 'NONE',  ( -0.000000000000000000, 1.000000000000000000, -0.000000000000000000 ) ) ;
#51463 = CARTESIAN_POINT ( 'NONE',  ( -77.71448999903256549, 21.96089801565737787, -62.00523686349998798 ) ) ;
#51464 = CARTESIAN_POINT ( 'NONE',  ( -11.14880195267006613, 7.129907723790827490, 44.35696964094925221 ) ) ;
#51465 = ORIENTED_EDGE ( 'NONE', *, *, #6648, .F. ) ;
#51466 = B_SPLINE_CURVE_WITH_KNOTS ( 'NONE', 3,
 ( #8431, #29882, #46049, #46741, #24615, #18978, #14730, #68214, #25655, #46390, #67869, #51344, #35853, #3159, #67519, #36196, #19666, #57307 ),
 .UNSPECIFIED., .F., .F.,
 ( 4, 2, 2, 2, 2, 2, 2, 2, 4 ),
 ( 0.000000000000000000, 0.001501532864490863093, 0.002252299296736294532, 0.003003065728981726187, 0.004504598593472635033, 0.006006131457963544314, 0.009009197186945320374, 0.01051073005143618455, 0.01201226291592704873 ),
 .UNSPECIFIED. ) ;
#51467 = CARTESIAN_POINT ( 'NONE',  ( 63.74253542338254164, 39.54050679744537433, 43.58025477438756923 ) ) ;
#51468 = ORIENTED_EDGE ( 'NONE', *, *, #44417, .F. ) ;
#51469 = DIRECTION ( 'NONE',  ( -0.000000000000000000, -0.000000000000000000, -1.000000000000000000 ) ) ;
#51470 = VERTEX_POINT ( 'NONE', #38019 ) ;
#51471 = CARTESIAN_POINT ( 'NONE',  ( 266.9165763529819628, 242.0000000000000000, 128.9999999999999716 ) ) ;
#51472 = CARTESIAN_POINT ( 'NONE',  ( 186.6075385349484179, 85.85749512876284939, -75.66779282773408966 ) ) ;
#51473 = CARTESIAN_POINT ( 'NONE',  ( -166.3231866619663606, 81.31146386205591625, 41.50210861837916809 ) ) ;
#51474 = EDGE_CURVE ( 'NONE', #15703, #29635, #5321, .T. ) ;
#51475 = CARTESIAN_POINT ( 'NONE',  ( -96.00016893459648770, 29.70347032303887858, -38.40669615010640570 ) ) ;
#51476 = CARTESIAN_POINT ( 'NONE',  ( -27.70185240367226953, 10.02491413133430775, 4.364727659495228451 ) ) ;
#51477 = DIRECTION ( 'NONE',  ( 0.000000000000000000, 0.000000000000000000, 1.000000000000000000 ) ) ;
#51478 = DIRECTION ( 'NONE',  ( 0.000000000000000000, 0.000000000000000000, 1.000000000000000000 ) ) ;
#51479 = CARTESIAN_POINT ( 'NONE',  ( 127.2397149628677369, 37.56999625068102233, -39.95516007037436879 ) ) ;
#51480 = ORIENTED_EDGE ( 'NONE', *, *, #3578, .F. ) ;
#51481 = B_SPLINE_CURVE_WITH_KNOTS ( 'NONE', 3,
 ( #39953, #6555, #34692, #22378, #50159, #66364 ),
 .UNSPECIFIED., .F., .F.,
 ( 4, 2, 4 ),
 ( 1.095770181102079639E-06, 0.03239442681617710207, 0.06478775786217311206 ),
 .UNSPECIFIED. ) ;
#51482 = ORIENTED_EDGE ( 'NONE', *, *, #55129, .T. ) ;
#51483 = VECTOR ( 'NONE', #56247, 1000.000000000000114 ) ;
#51484 = CARTESIAN_POINT ( 'NONE',  ( 188.2262945779355903, 87.63857788125626769, 88.20066469376320129 ) ) ;
#51485 = SURFACE_SIDE_STYLE ('',( #14870 ) ) ;
#51486 = CARTESIAN_POINT ( 'NONE',  ( -29.04258984626623530, 9.210213971636683539, -76.77276363795868974 ) ) ;
#51487 = ADVANCED_FACE ( 'NONE', ( #11624 ), #32744, .F. ) ;
#51488 = VECTOR ( 'NONE', #8781, 1000.000000000000000 ) ;
#51489 = UNCERTAINTY_MEASURE_WITH_UNIT (LENGTH_MEASURE( 1.000000000000000082E-05 ), #8038, 'distance_accuracy_value', 'NONE');
#51490 = ADVANCED_FACE ( 'NONE', ( #33096 ), #1084, .F. ) ;
#51491 = FACE_OUTER_BOUND ( 'NONE', #26026, .T. ) ;
#51492 = EDGE_CURVE ( 'NONE', #43935, #59387, #54884, .T. ) ;
#51493 = EDGE_LOOP ( 'NONE', ( #17600, #52570, #4956, #60934 ) ) ;
#51494 = VECTOR ( 'NONE', #21320, 1000.000000000000000 ) ;
#51495 = CARTESIAN_POINT ( 'NONE',  ( 70.65683382808195745, 25.18281821780106711, 170.0000000000000000 ) ) ;
#51496 = CARTESIAN_POINT ( 'NONE',  ( 57.61205526789942866, 9.184630482019173314, 27.58472315868180402 ) ) ;
#51497 = CARTESIAN_POINT ( 'NONE',  ( 207.8407634284391179, 112.5209879629463785, 16.68595737575994420 ) ) ;
#51498 =( NAMED_UNIT ( * ) PLANE_ANGLE_UNIT ( ) SI_UNIT ( $, .RADIAN. ) );
#51499 = CARTESIAN_POINT ( 'NONE',  ( 276.6971892993743154, -21.67618688890531686, 3.767895544566218113 ) ) ;
#51500 = CARTESIAN_POINT ( 'NONE',  ( -25.07735481787161191, 9.648965052008787069, 60.58124441867286691 ) ) ;
#51501 = DIRECTION ( 'NONE',  ( -1.000000000000000000, -0.000000000000000000, -0.000000000000000000 ) ) ;
#51502 = CARTESIAN_POINT ( 'NONE',  ( -47.80193682758677909, 12.85650137125658787, 62.68131162742057683 ) ) ;
#51503 = VECTOR ( 'NONE', #37692, 1000.000000000000000 ) ;
#51504 = CARTESIAN_POINT ( 'NONE',  ( -2.874437057892792691, 6.618922960888053986, 58.80530662568687461 ) ) ;
#51505 = VERTEX_POINT ( 'NONE', #61571 ) ;
#51506 = CARTESIAN_POINT ( 'NONE',  ( 274.9998698049113273, 22.00002958979062839, -0.3253397936367980470 ) ) ;
#51507 = DIRECTION ( 'NONE',  ( -0.6910626489868580968, -0.7227948638273978821, 0.000000000000000000 ) ) ;
#51508 = DIRECTION ( 'NONE',  ( -0.000000000000000000, 1.000000000000000000, -0.000000000000000000 ) ) ;
#51509 = CARTESIAN_POINT ( 'NONE',  ( -54.56693200831794144, 14.55131601960338905, -35.21632399845986328 ) ) ;
#51510 = LINE ( 'NONE', #19480, #17789 ) ;
#51511 = FACE_OUTER_BOUND ( 'NONE', #55861, .T. ) ;
#51512 = ORIENTED_EDGE ( 'NONE', *, *, #10735, .T. ) ;
#51513 = DIRECTION ( 'NONE',  ( -1.000000000000000000, 0.000000000000000000, 0.000000000000000000 ) ) ;
#51514 = ORIENTED_EDGE ( 'NONE', *, *, #35205, .F. ) ;
#51515 = ORIENTED_EDGE ( 'NONE', *, *, #56639, .F. ) ;
#51516 = CYLINDRICAL_SURFACE ( 'NONE', #67875, 65.36598343705435354 ) ;
#51517 = CARTESIAN_POINT ( 'NONE',  ( -180.6213815675305341, 95.88446356933846459, -69.36606367677470075 ) ) ;
#51518 = DIRECTION ( 'NONE',  ( -0.000000000000000000, -0.000000000000000000, -1.000000000000000000 ) ) ;
#51519 = EDGE_LOOP ( 'NONE', ( #37452, #14399, #48917, #11341 ) ) ;
#51520 = CARTESIAN_POINT ( 'NONE',  ( -200.0000000000000000, 0.000000000000000000, -7.000000000000000000 ) ) ;
#51521 = CARTESIAN_POINT ( 'NONE',  ( -180.4643341113398094, 95.69224917234936356, 13.03253127180882309 ) ) ;
#51522 = CARTESIAN_POINT ( 'NONE',  ( -1.728570918131775880, 6.570609986804680780, 6.396230257614674564 ) ) ;
#51523 = CARTESIAN_POINT ( 'NONE',  ( 63.01563776193091826, 13.70579113808095073, -50.72069083216976537 ) ) ;
#51524 = CARTESIAN_POINT ( 'NONE',  ( -83.53167274806554587, 25.32068190668983831, 43.64689675707840877 ) ) ;
#51525 = DIRECTION ( 'NONE',  ( -0.8160245890732938934, -0.5780171883497599028, 0.000000000000000000 ) ) ;
#51526 = CARTESIAN_POINT ( 'NONE',  ( 140.2332932573541200, 45.41010019581509027, 14.14583329522551125 ) ) ;
#51527 = ADVANCED_FACE ( 'NONE', ( #39079, #55588 ), #39764, .T. ) ;
#51528 = ORIENTED_EDGE ( 'NONE', *, *, #16588, .F. ) ;
#51530 = ADVANCED_FACE ( 'NONE', ( #35178 ), #40115, .F. ) ;
#51529 = DIRECTION ( 'NONE',  ( 0.1342332658176522420, 0.9909497617679352555, -3.104767966278886959E-17 ) ) ;
#51531 = CARTESIAN_POINT ( 'NONE',  ( 0.000000000000000000, 0.000000000000000000, 40.00000000000003553 ) ) ;
#51532 = CARTESIAN_POINT ( 'NONE',  ( 46.50207827473963107, 9.439498081273457686, -45.54875031526387374 ) ) ;
#51533 = CARTESIAN_POINT ( 'NONE',  ( 64.16679220703382214, -10.37413986118096432, 170.0000000000000000 ) ) ;
#51535 = ORIENTED_EDGE ( 'NONE', *, *, #51917, .T. ) ;
#51534 = CARTESIAN_POINT ( 'NONE',  ( -119.1064753703575718, 42.18441154001784099, 94.99999999999866418 ) ) ;
#51536 = CARTESIAN_POINT ( 'NONE',  ( 67.54641595172913071, 14.80690682047551121, 43.30947815275538915 ) ) ;
#51537 = ORIENTED_EDGE ( 'NONE', *, *, #58850, .F. ) ;
#51538 = AXIS2_PLACEMENT_3D ( 'NONE', #5915, #60083, #42533 ) ;
#51539 = ORIENTED_EDGE ( 'NONE', *, *, #65166, .T. ) ;
#51540 = CARTESIAN_POINT ( 'NONE',  ( -142.9730935922299579, 58.82921737386682537, 68.75594806298462913 ) ) ;
#51541 = DIRECTION ( 'NONE',  ( -1.000000000000000000, -1.387778780781446908E-16, 0.000000000000000000 ) ) ;
#51542 = FACE_BOUND ( 'NONE', #49591, .T. ) ;
#51543 = EDGE_CURVE ( 'NONE', #41654, #62549, #5788, .T. ) ;
#51544 = CARTESIAN_POINT ( 'NONE',  ( 181.0840389613909736, 78.60582251573003987, -9.380507075415925655 ) ) ;
#51545 = ADVANCED_FACE ( 'NONE', ( #13049 ), #23251, .F. ) ;
#51546 = CARTESIAN_POINT ( 'NONE',  ( -118.3927673406137160, 41.74929850983306068, 65.20241849948250490 ) ) ;
#51547 = CARTESIAN_POINT ( 'NONE',  ( -85.64924756730680144, 26.19583280090849442, -18.51914542751836734 ) ) ;
#51548 = CARTESIAN_POINT ( 'NONE',  ( 16.21073205782802162, 7.521094197081421129, -89.20804527961311692 ) ) ;
#51549 = CARTESIAN_POINT ( 'NONE',  ( -152.5046761101291963, 66.76407727525179325, -35.43405179214044409 ) ) ;
#51550 = ORIENTED_EDGE ( 'NONE', *, *, #6516, .T. ) ;
#51551 = ORIENTED_EDGE ( 'NONE', *, *, #18110, .T. ) ;
#51552 = EDGE_CURVE ( 'NONE', #25068, #42723, #57407, .T. ) ;
#51553 = CARTESIAN_POINT ( 'NONE',  ( -104.1393288135077455, 34.86912007524089319, 18.45559023715674840 ) ) ;
#51554 = CARTESIAN_POINT ( 'NONE',  ( -84.49322488516129681, 0.000000000000000000, 43.58025477438756212 ) ) ;
#51555 = CARTESIAN_POINT ( 'NONE',  ( -36.11269837220806522, 5.000000000000056843, 0.000000000000000000 ) ) ;
#51556 = EDGE_CURVE ( 'NONE', #31823, #47125, #8012, .T. ) ;
#51557 = CARTESIAN_POINT ( 'NONE',  ( -20.00000000000000000, 2.449293598294706513E-15, -20.00000000000000000 ) ) ;
#51558 = CARTESIAN_POINT ( 'NONE',  ( 422.4999999999999432, 207.5000000000000284, 380.0000000000000000 ) ) ;
#51559 = DIRECTION ( 'NONE',  ( -0.000000000000000000, 0.000000000000000000, -1.000000000000000000 ) ) ;
#51560 = CARTESIAN_POINT ( 'NONE',  ( -143.2582950235167800, 60.34055023774276094, 87.75006652546248631 ) ) ;
#51561 = ORIENTED_EDGE ( 'NONE', *, *, #49399, .F. ) ;
#51562 = VERTEX_POINT ( 'NONE', #3513 ) ;
#51563 = EDGE_LOOP ( 'NONE', ( #8574, #58300, #13980, #4358 ) ) ;
#51564 = CARTESIAN_POINT ( 'NONE',  ( -151.6648563624119390, 67.36546864992756412, -22.66487162737027461 ) ) ;
#51565 = DIRECTION ( 'NONE',  ( 0.9639628606958512425, 0.2660368455666826670, 0.000000000000000000 ) ) ;
#51566 = CARTESIAN_POINT ( 'NONE',  ( 63.98971758354223027, 12.90030016320051232, -35.76819646162389432 ) ) ;
#51567 = CARTESIAN_POINT ( 'NONE',  ( 106.1738623902246275, 27.04424563638256629, -90.79883557465640820 ) ) ;
#51568 = EDGE_CURVE ( 'NONE', #1887, #56564, #26014, .T. ) ;
#51569 = CARTESIAN_POINT ( 'NONE',  ( -62.55320287144887459, 17.87319849854530318, 38.05489813362841289 ) ) ;
#51570 = CARTESIAN_POINT ( 'NONE',  ( -102.2801239173131194, -170.0000000000000000, -23.17002667451225406 ) ) ;
#51571 = EDGE_CURVE ( 'NONE', #48198, #275, #46770, .T. ) ;
#51572 = EDGE_CURVE ( 'NONE', #2018, #45426, #56988, .T. ) ;
#51573 = CARTESIAN_POINT ( 'NONE',  ( 55.51637278631174865, 12.08345311280959677, 36.80331343779680253 ) ) ;
#51574 = CYLINDRICAL_SURFACE ( 'NONE', #68608, 185.0000000000000000 ) ;
#51575 = ORIENTED_EDGE ( 'NONE', *, *, #42065, .F. ) ;
#51576 = CARTESIAN_POINT ( 'NONE',  ( -0.8011128725815479523, 6.535315321814157308, -40.27799443517058364 ) ) ;
#51577 = DIRECTION ( 'NONE',  ( 2.312964634635743450E-16, -0.000000000000000000, 1.000000000000000000 ) ) ;
#51578 = CARTESIAN_POINT ( 'NONE',  ( -121.1775535805057160, 43.46577565517550568, 17.12734891093444034 ) ) ;
#51579 = DIRECTION ( 'NONE',  ( 0.000000000000000000, 0.000000000000000000, 1.000000000000000000 ) ) ;
#51580 = CARTESIAN_POINT ( 'NONE',  ( 127.6144785300460711, 37.78099129859915450, -20.84396720244194512 ) ) ;
#51581 = CARTESIAN_POINT ( 'NONE',  ( 15.78827728214693060, 7.507518794609574719, -8.674393508222097537 ) ) ;
#51582 = CARTESIAN_POINT ( 'NONE',  ( 197.9847015768255574, 97.56951352050454318, 66.90867592435427014 ) ) ;
#51583 = VECTOR ( 'NONE', #56270, 1000.000000000000000 ) ;
#51584 = ORIENTED_EDGE ( 'NONE', *, *, #8106, .T. ) ;
#51585 = APPLICATION_PROTOCOL_DEFINITION ( 'draft international standard', 'automotive_design', 1998, #68260 ) ;
#51586 = PLANE ( 'NONE',  #65509 ) ;
#51587 = CARTESIAN_POINT ( 'NONE',  ( 0.000000000000000000, 0.000000000000000000, 0.000000000000000000 ) ) ;
#51588 = CARTESIAN_POINT ( 'NONE',  ( 13.24564585880132839, -63.65041531508827433, 41.38025477438755928 ) ) ;
#51589 = STYLED_ITEM ( 'NONE', ( #37209 ), #64527 ) ;
#51590 = ITEM_DEFINED_TRANSFORMATION ( 'NONE', 'NONE', #9564,  #66832 ) ;
#51591 = CARTESIAN_POINT ( 'NONE',  ( 8.485361335568063268, 6.376707943524878353, -95.00000000000133582 ) ) ;
#51592 = ORIENTED_EDGE ( 'NONE', *, *, #58715, .F. ) ;
#51593 = EDGE_LOOP ( 'NONE', ( #59619, #63902, #60227, #36741 ) ) ;
#51594 = CARTESIAN_POINT ( 'NONE',  ( -146.5268141329886760, 61.69196909035590437, -8.582240967115531305 ) ) ;
#51595 = CARTESIAN_POINT ( 'NONE',  ( 198.7123879174243939, 100.1053816708572555, 5.335743429363529522 ) ) ;
#51596 = ORIENTED_EDGE ( 'NONE', *, *, #65922, .F. ) ;
#51597 = CARTESIAN_POINT ( 'NONE',  ( 149.9883001095526822, 53.30008207809360954, 91.24430364700101848 ) ) ;
#51598 = ORIENTED_EDGE ( 'NONE', *, *, #18406, .T. ) ;
#51599 = CARTESIAN_POINT ( 'NONE',  ( 22.07550062443499428, -11.73338281062043364, 0.000000000000000000 ) ) ;
#51600 = CARTESIAN_POINT ( 'NONE',  ( 126.8237978310704790, 37.33705012421152958, 39.62906459034504536 ) ) ;
#51601 = CARTESIAN_POINT ( 'NONE',  ( -23.98664742203151690, 23.27925779329526179, 6.893342939543522618 ) ) ;
#51602 = CARTESIAN_POINT ( 'NONE',  ( -62.66631205405185057, 18.59153367093362874, 41.38025477438755928 ) ) ;
#51603 = DIRECTION ( 'NONE',  ( 0.000000000000000000, 1.000000000000000000, 0.000000000000000000 ) ) ;
#51605 = VERTEX_POINT ( 'NONE', #36221 ) ;
#51604 = CARTESIAN_POINT ( 'NONE',  ( 0.000000000000000000, 0.000000000000000000, 85.00000000000000000 ) ) ;
#51606 = CARTESIAN_POINT ( 'NONE',  ( -2.793168949963659387, 7.622505585224017999, -91.02962397824867935 ) ) ;
#51607 = EDGE_LOOP ( 'NONE', ( #25405, #69537, #54241, #6858, #65605, #18826, #16742, #39318, #46104, #16837 ) ) ;
#51608 = ORIENTED_EDGE ( 'NONE', *, *, #45343, .F. ) ;
#51610 = EDGE_CURVE ( 'NONE', #62549, #41654, #59657, .T. ) ;
#51609 = CARTESIAN_POINT ( 'NONE',  ( -165.6397095829521788, 80.60756690931941648, 10.86796417263294856 ) ) ;
#51611 = APPLICATION_CONTEXT ( 'automotive_design' ) ;
#51612 = CARTESIAN_POINT ( 'NONE',  ( 23.28785143291466397, 6.856621069835716398, -70.36468173549914695 ) ) ;
#51614 = VERTEX_POINT ( 'NONE', #9144 ) ;
#51613 = CARTESIAN_POINT ( 'NONE',  ( -126.3453033442920628, 47.99870040347951061, 57.46449846362077807 ) ) ;
#51615 = CARTESIAN_POINT ( 'NONE',  ( -99.42452458507153779, 32.47480804767672424, 84.74605913991881323 ) ) ;
#51616 = VECTOR ( 'NONE', #52645, 1000.000000000000000 ) ;
#51617 = FACE_BOUND ( 'NONE', #26830, .T. ) ;
#51618 = EDGE_LOOP ( 'NONE', ( #33771, #26842, #7574, #6509 ) ) ;
#51619 = CARTESIAN_POINT ( 'NONE',  ( 208.9585401441655961, 114.1617785893844257, -64.48185821820443664 ) ) ;
#51620 = EDGE_CURVE ( 'NONE', #45282, #29274, #15110, .T. ) ;
#51621 = CARTESIAN_POINT ( 'NONE',  ( 141.1220430186942565, 47.19066702031172866, 38.89026279445103285 ) ) ;
#51622 = CARTESIAN_POINT ( 'NONE',  ( 0.000000000000000000, 0.000000000000000000, 0.000000000000000000 ) ) ;
#51623 = DIRECTION ( 'NONE',  ( 0.000000000000000000, 0.000000000000000000, 1.000000000000000000 ) ) ;
#51624 = EDGE_CURVE ( 'NONE', #63560, #25708, #57475, .T. ) ;
#51625 = CARTESIAN_POINT ( 'NONE',  ( 69.35866309798979046, 15.27376159675660539, -66.05564973924086303 ) ) ;
#51626 = ORIENTED_EDGE ( 'NONE', *, *, #26594, .F. ) ;
#51627 = AXIS2_PLACEMENT_3D ( 'NONE', #51783, #40879, #3258 ) ;
#51628 = EDGE_CURVE ( 'NONE', #43978, #13483, #49568, .T. ) ;
#51629 = ORIENTED_EDGE ( 'NONE', *, *, #35967, .T. ) ;
#51630 = CARTESIAN_POINT ( 'NONE',  ( 9.001060725719206346, 7.384057747890103940, -93.40660889270941425 ) ) ;
#51631 = CARTESIAN_POINT ( 'NONE',  ( -172.3057147739577033, 86.22480007276998037, -49.67904019660583259 ) ) ;
#51632 = DIRECTION ( 'NONE',  ( -1.000000000000000000, 0.000000000000000000, 2.775557561562891351E-16 ) ) ;
#51633 = COLOUR_RGB ( '',0.7921568627450980005, 0.8196078431372548767, 0.9333333333333333481 ) ;
#51634 = CARTESIAN_POINT ( 'NONE',  ( -50.64797127373722674, 13.54441475554784979, -90.31972401984275223 ) ) ;
#51635 = LINE ( 'NONE', #6724, #64630 ) ;
#51636 = LINE ( 'NONE', #9416, #55092 ) ;
#51637 = CARTESIAN_POINT ( 'NONE',  ( -147.3614567344829140, 62.37986555269942812, 45.42098636282473478 ) ) ;
#51638 = CARTESIAN_POINT ( 'NONE',  ( 0.000000000000000000, 0.000000000000000000, 170.0000000000000000 ) ) ;
#51639 = CARTESIAN_POINT ( 'NONE',  ( -169.1041038606267648, 82.76530082651281361, -75.40566809599023657 ) ) ;
#51640 = ORIENTED_EDGE ( 'NONE', *, *, #34778, .T. ) ;
#51641 = CARTESIAN_POINT ( 'NONE',  ( -108.0902552660050446, 36.97681740369922920, 33.25039213534302007 ) ) ;
#51642 = EDGE_LOOP ( 'NONE', ( #41557, #30941, #5187, #33961 ) ) ;
#51643 = CARTESIAN_POINT ( 'NONE',  ( -37.07086358537073068, 10.58360809068249964, 15.84908622039232817 ) ) ;
#51644 = FILL_AREA_STYLE_COLOUR ( '', #67808 ) ;
#51645 = VERTEX_POINT ( 'NONE', #52722 ) ;
#51646 = DIRECTION ( 'NONE',  ( 1.000000000000000000, 0.000000000000000000, 0.000000000000000000 ) ) ;
#51647 = CARTESIAN_POINT ( 'NONE',  ( 37.76691715686636996, 29.79383981485516841, -24.99999999999999645 ) ) ;
#51648 = FACE_OUTER_BOUND ( 'NONE', #59751, .T. ) ;
#51649 = SURFACE_STYLE_FILL_AREA ( #42122 ) ;
#51650 = CARTESIAN_POINT ( 'NONE',  ( 32.09567473596477782, 7.571373529017940029, 12.28090692073144119 ) ) ;
#51651 = CARTESIAN_POINT ( 'NONE',  ( -15.07235766390728671, 8.482541916553477890, -44.86552813969799303 ) ) ;
#51652 = CARTESIAN_POINT ( 'NONE',  ( -38.54712373114178092, 11.89174538567467465, -18.41568109954191002 ) ) ;
#51653 = EDGE_CURVE ( 'NONE', #51213, #35609, #35534, .T. ) ;
#51654 = VERTEX_POINT ( 'NONE', #14068 ) ;
#51655 = CARTESIAN_POINT ( 'NONE',  ( -68.11501976657811497, -31.41506934893937952, 170.0000000000000000 ) ) ;
#51656 = ORIENTED_EDGE ( 'NONE', *, *, #1578, .F. ) ;
#51657 = CARTESIAN_POINT ( 'NONE',  ( -55.05276343752909440, 14.68156374112638751, 30.31732777293113301 ) ) ;
#51658 = CARTESIAN_POINT ( 'NONE',  ( -58.33157376762796531, 16.63098604184964913, 71.41156564722952282 ) ) ;
#51660 = EDGE_CURVE ( 'NONE', #38509, #14449, #68238, .T. ) ;
#51659 = CARTESIAN_POINT ( 'NONE',  ( -28.13852122803039890, 9.072484007196644384, 4.119663645332994228 ) ) ;
#51661 = EDGE_LOOP ( 'NONE', ( #3403, #25437, #44486, #9735 ) ) ;
#51662 = DIRECTION ( 'NONE',  ( 0.000000000000000000, -0.5000000000000008882, 0.8660254037844382635 ) ) ;
#51663 = CARTESIAN_POINT ( 'NONE',  ( -60.12777185093246146, 16.10091404267868498, -90.86635757588598494 ) ) ;
#51664 = CARTESIAN_POINT ( 'NONE',  ( -38.89042640463647871, 10.93374343663409221, 38.70441581485059146 ) ) ;
#51665 = SURFACE_STYLE_FILL_AREA ( #8766 ) ;
#51666 = ORIENTED_EDGE ( 'NONE', *, *, #26205, .T. ) ;
#51667 = DIRECTION ( 'NONE',  ( 9.950807539071958118E-15, -1.000000000000000000, -4.024558464266191670E-15 ) ) ;
#51668 = AXIS2_PLACEMENT_3D ( 'NONE', #22463, #43904, #17173 ) ;
#51669 = CARTESIAN_POINT ( 'NONE',  ( -156.9232798886536671, 72.10386843399172108, 63.90848877142625639 ) ) ;
#51670 = CARTESIAN_POINT ( 'NONE',  ( -125.0023254877051784, 45.90912477771774292, 30.65933094750346299 ) ) ;
#51671 = CARTESIAN_POINT ( 'NONE',  ( 0.08224679563971432072, 7.710515798486365924, 2.644994884459109574 ) ) ;
#51672 = VERTEX_POINT ( 'NONE', #68902 ) ;
#51673 = CARTESIAN_POINT ( 'NONE',  ( -180.5200658187031877, 97.35517482626556784, -70.32344830815547709 ) ) ;
#51674 = DIRECTION ( 'NONE',  ( -0.000000000000000000, 0.000000000000000000, -1.000000000000000000 ) ) ;
#51675 = CARTESIAN_POINT ( 'NONE',  ( 112.7784411285248751, 30.07270878825233851, 30.04885473467402335 ) ) ;
#51676 = FILL_AREA_STYLE_COLOUR ( '', #27024 ) ;
#51677 = LINE ( 'NONE', #62584, #56001 ) ;
#51678 = ORIENTED_EDGE ( 'NONE', *, *, #51238, .F. ) ;
#51679 = DIRECTION ( 'NONE',  ( -0.000000000000000000, -0.000000000000000000, -1.000000000000000000 ) ) ;
#51680 = DIRECTION ( 'NONE',  ( 0.000000000000000000, 0.000000000000000000, 1.000000000000000000 ) ) ;
#51681 = CARTESIAN_POINT ( 'NONE',  ( 184.0001683447903531, 83.06228184427187955, 29.88528625916754322 ) ) ;
#51682 = CARTESIAN_POINT ( 'NONE',  ( 139.6326990672750696, 46.22017155708125102, 5.375290015202373262 ) ) ;
#51683 = FACE_OUTER_BOUND ( 'NONE', #3798, .T. ) ;
#51684 = AXIS2_PLACEMENT_3D ( 'NONE', #30314, #67954, #14480 ) ;
#51685 = ORIENTED_EDGE ( 'NONE', *, *, #60333, .F. ) ;
#51686 = EDGE_CURVE ( 'NONE', #68538, #41004, #7081, .T. ) ;
#51687 = CARTESIAN_POINT ( 'NONE',  ( 163.7403496014744633, 64.00600007368879574, -20.90330565569645316 ) ) ;
#51688 = VERTEX_POINT ( 'NONE', #26357 ) ;
#51690 = ADVANCED_FACE ( 'NONE', ( #16734 ), #12172, .F. ) ;
#51689 = CARTESIAN_POINT ( 'NONE',  ( 69.36287815987333261, 15.27486453472190142, 60.15464916579820454 ) ) ;
#51691 = CARTESIAN_POINT ( 'NONE',  ( 126.6810562747852345, 37.25730572548798136, 88.48790994800812371 ) ) ;
#51693 = EDGE_LOOP ( 'NONE', ( #35843, #30273, #44232, #43532 ) ) ;
#51692 = CARTESIAN_POINT ( 'NONE',  ( 0.000000000000000000, 0.000000000000000000, 41.38025477438755928 ) ) ;
#51694 = CARTESIAN_POINT ( 'NONE',  ( -147.3614567344829709, 62.37986555269942812, -61.95721599902998378 ) ) ;
#51695 = AXIS2_PLACEMENT_3D ( 'NONE', #59125, #27467, #22204 ) ;
#51696 = DIRECTION ( 'NONE',  ( 0.000000000000000000, 1.000000000000000000, -0.000000000000000000 ) ) ;
#51697 = CARTESIAN_POINT ( 'NONE',  ( 163.1495034066983862, 62.20479872133081045, -38.69930229318859460 ) ) ;
#51698 = ORIENTED_EDGE ( 'NONE', *, *, #48585, .F. ) ;
#51699 = CARTESIAN_POINT ( 'NONE',  ( -96.45303203827904781, 31.03218867996499242, 15.92233808110716708 ) ) ;
#51700 = EDGE_CURVE ( 'NONE', #30529, #20755, #25997, .T. ) ;
#51701 = DIRECTION ( 'NONE',  ( -0.000000000000000000, -1.000000000000000000, -0.000000000000000000 ) ) ;
#51702 = CARTESIAN_POINT ( 'NONE',  ( 74.62299871641495486, 5.461138973199027191, 43.58025477438756923 ) ) ;
#51703 = DIRECTION ( 'NONE',  ( 1.000000000000000000, 0.000000000000000000, -0.000000000000000000 ) ) ;
#51704 = CARTESIAN_POINT ( 'NONE',  ( -168.7187482717113483, 82.35796501763486788, 32.23136137619717090 ) ) ;
#51705 = CARTESIAN_POINT ( 'NONE',  ( 157.4703587214989113, 57.65129005721575339, 56.25401806271706562 ) ) ;
#51706 = EDGE_CURVE ( 'NONE', #48801, #34756, #46216, .T. ) ;
#51707 = CARTESIAN_POINT ( 'NONE',  ( 94.11595392909971736, 23.18887043179185525, 37.72638076850486044 ) ) ;
#51708 = ORIENTED_EDGE ( 'NONE', *, *, #31433, .T. ) ;
#51709 = CARTESIAN_POINT ( 'NONE',  ( -101.3502439362134595, 33.43728945125135255, 57.40693085676335983 ) ) ;
#51711 = ADVANCED_FACE ( 'NONE', ( #38544 ), #49431, .T. ) ;
#51710 = CARTESIAN_POINT ( 'NONE',  ( -9.765753193741730342, 8.033970690975920093, 57.21132304879623121 ) ) ;
#51712 = ORIENTED_EDGE ( 'NONE', *, *, #57557, .F. ) ;
#51713 = CARTESIAN_POINT ( 'NONE',  ( 157.0316110297313799, 58.58403635656377162, -9.279633708673957315 ) ) ;
#51714 = FACE_OUTER_BOUND ( 'NONE', #3854, .T. ) ;
#51715 = CARTESIAN_POINT ( 'NONE',  ( 105.7953515382196485, 27.97683113100024244, 43.16950470399848427 ) ) ;
#51716 = DIRECTION ( 'NONE',  ( 1.000000000000000000, 0.000000000000000000, -0.000000000000000000 ) ) ;
#51717 = CARTESIAN_POINT ( 'NONE',  ( 10.55634918610406281, 15.55634918610400241, 0.000000000000000000 ) ) ;
#51718 = CARTESIAN_POINT ( 'NONE',  ( 188.0094179620990928, 87.39792407168452826, 7.070946854141474169 ) ) ;
#51719 = CARTESIAN_POINT ( 'NONE',  ( 210.1633650091869185, 114.1507944623967035, -48.96769043267524069 ) ) ;
#51720 = CARTESIAN_POINT ( 'NONE',  ( 177.2011275744679040, 74.76848439756736298, 3.543480587856852715 ) ) ;
#51721 = CARTESIAN_POINT ( 'NONE',  ( -61.86403937395562025, 16.61416349803656090, 14.12202676930323086 ) ) ;
#51722 = ORIENTED_EDGE ( 'NONE', *, *, #48455, .F. ) ;
#51723 = DIRECTION ( 'NONE',  ( -0.1785568947986229393, -0.9839295885986322210, 0.000000000000000000 ) ) ;
#51724 = ORIENTED_EDGE ( 'NONE', *, *, #11405, .T. ) ;
#51725 = DIRECTION ( 'NONE',  ( -0.000000000000000000, -0.000000000000000000, -1.000000000000000000 ) ) ;
#51726 = CARTESIAN_POINT ( 'NONE',  ( 46.65974587859240330, 10.48396258569370332, -18.22915301820460598 ) ) ;
#51727 = DIRECTION ( 'NONE',  ( 0.000000000000000000, 0.000000000000000000, 1.000000000000000000 ) ) ;
#51728 = FACE_OUTER_BOUND ( 'NONE', #27260, .T. ) ;
#51729 = CARTESIAN_POINT ( 'NONE',  ( -12.11585256177172276, 7.208421262014329756, 85.14452039693073004 ) ) ;
#51730 = AXIS2_PLACEMENT_3D ( 'NONE', #15265, #48277, #69053 ) ;
#51731 = CARTESIAN_POINT ( 'NONE',  ( -104.7956873821848802, 35.21322275870669216, -22.73943902020269903 ) ) ;
#51732 = ORIENTED_EDGE ( 'NONE', *, *, #5461, .F. ) ;
#51733 = CARTESIAN_POINT ( 'NONE',  ( -76.31381168750411348, 21.43908608416556305, 71.90022727437172989 ) ) ;
#51734 = LINE ( 'NONE', #14451, #16137 ) ;
#51735 = ORIENTED_EDGE ( 'NONE', *, *, #44656, .T. ) ;
#51736 = EDGE_CURVE ( 'NONE', #53637, #30259, #43943, .T. ) ;
#51737 = ORIENTED_EDGE ( 'NONE', *, *, #35256, .T. ) ;
#51738 = CARTESIAN_POINT ( 'NONE',  ( -156.9406434201983984, 70.74968524571478667, 39.37071447540302671 ) ) ;
#51739 = LINE ( 'NONE', #24672, #26568 ) ;
#51740 = CARTESIAN_POINT ( 'NONE',  ( 178.1999009735082211, 75.73911533785329198, -9.953687985995264498 ) ) ;
#51741 = CARTESIAN_POINT ( 'NONE',  ( -169.8885678771097787, 85.07765565657315676, 58.38415322356205905 ) ) ;
#51742 = CARTESIAN_POINT ( 'NONE',  ( -430.1627218934916073, 394.9999999999956231, 91.05029585799256608 ) ) ;
#51743 = VECTOR ( 'NONE', #20303, 1000.000000000000000 ) ;
#51744 = CARTESIAN_POINT ( 'NONE',  ( 57.39233401791016576, 12.46575990788835320, -11.38927566978218664 ) ) ;
#51745 = ORIENTED_EDGE ( 'NONE', *, *, #60924, .F. ) ;
#51746 = CARTESIAN_POINT ( 'NONE',  ( 0.000000000000000000, 0.000000000000000000, 170.0000000000000000 ) ) ;
#51747 = ORIENTED_EDGE ( 'NONE', *, *, #856, .F. ) ;
#51748 = CARTESIAN_POINT ( 'NONE',  ( 211.5066273949820186, 116.1727691518062215, 6.669578147803371770 ) ) ;
#51749 = LINE ( 'NONE', #57719, #30501 ) ;
#51750 = CARTESIAN_POINT ( 'NONE',  ( 212.1962110267000696, 117.2292732107321740, 36.33105866627646918 ) ) ;
#51751 = FACE_BOUND ( 'NONE', #41536, .T. ) ;
#51752 = PRODUCT_DEFINITION_SHAPE ( 'NONE', 'NONE',  #67192 ) ;
#51753 = EDGE_LOOP ( 'NONE', ( #59560, #51350, #14440, #54590 ) ) ;
#51754 = ORIENTED_EDGE ( 'NONE', *, *, #16181, .F. ) ;
#51755 = DIRECTION ( 'NONE',  ( -0.000000000000000000, 1.000000000000000000, -0.000000000000000000 ) ) ;
#51756 = LINE ( 'NONE', #25035, #29395 ) ;
#51757 = DIRECTION ( 'NONE',  ( 1.000000000000000000, 0.000000000000000000, 0.000000000000000000 ) ) ;
#51758 = LINE ( 'NONE', #13775, #29847 ) ;
#51759 = CARTESIAN_POINT ( 'NONE',  ( 20.10458824423762891, 6.677140564692391145, 85.06154812080229988 ) ) ;
#51760 = VECTOR ( 'NONE', #28017, 1000.000000000000000 ) ;
#51761 = DIRECTION ( 'NONE',  ( -1.000000000000000000, -0.000000000000000000, 0.000000000000000000 ) ) ;
#51762 = ADVANCED_FACE ( 'NONE', ( #22717 ), #1974, .F. ) ;
#51763 = ORIENTED_EDGE ( 'NONE', *, *, #47943, .T. ) ;
#51765 = EDGE_CURVE ( 'NONE', #53693, #51871, #69102, .T. ) ;
#51764 = CARTESIAN_POINT ( 'NONE',  ( -78.66644367742111399, -170.0000000000000000, 64.76275173013681297 ) ) ;
#51766 = CARTESIAN_POINT ( 'NONE',  ( 202.7540649946182896, 105.3989460363904698, -51.08106962100063697 ) ) ;
#51767 = ADVANCED_FACE ( 'NONE', ( #66694 ), #13560, .T. ) ;
#51768 = ORIENTED_EDGE ( 'NONE', *, *, #29773, .T. ) ;
#51769 = CARTESIAN_POINT ( 'NONE',  ( -84.22570405563701001, 24.51726571826275247, 16.13179647595237043 ) ) ;
#51770 = VERTEX_POINT ( 'NONE', #25164 ) ;
#51771 = CARTESIAN_POINT ( 'NONE',  ( -80.31691774066409550, 22.95709084517031684, -62.14002771806871550 ) ) ;
#51772 = CARTESIAN_POINT ( 'NONE',  ( 0.000000000000000000, 0.000000000000000000, 0.000000000000000000 ) ) ;
#51773 = EDGE_CURVE ( 'NONE', #23032, #53791, #46592, .T. ) ;
#51774 = EDGE_LOOP ( 'NONE', ( #1464, #48966, #61703, #42399 ) ) ;
#51775 = EDGE_CURVE ( 'NONE', #60761, #53864, #8287, .T. ) ;
#51776 = ORIENTED_EDGE ( 'NONE', *, *, #32799, .F. ) ;
#51777 = CARTESIAN_POINT ( 'NONE',  ( 11.21653854975268949, 6.397128675385706842, -37.05325069752230860 ) ) ;
#51778 = FACE_OUTER_BOUND ( 'NONE', #61527, .T. ) ;
#51779 = CARTESIAN_POINT ( 'NONE',  ( 20.74093720376649230, 6.709541214524347374, 5.016829158437670522 ) ) ;
#51780 = ORIENTED_EDGE ( 'NONE', *, *, #14050, .F. ) ;
#51781 = LINE ( 'NONE', #42264, #25589 ) ;
#51782 = CARTESIAN_POINT ( 'NONE',  ( 173.9457771591584958, 73.05793967547531054, -72.88831180620124428 ) ) ;
#51783 = CARTESIAN_POINT ( 'NONE',  ( 15.55634918610409656, 36.11269837220803680, 85.00100000000000477 ) ) ;
#51784 = EDGE_CURVE ( 'NONE', #13402, #68905, #50794, .T. ) ;
#51785 = CARTESIAN_POINT ( 'NONE',  ( 107.9362503323352769, 27.82881837607801856, -36.27000779090448646 ) ) ;
#51786 = CARTESIAN_POINT ( 'NONE',  ( 83.38619203015947789, 19.39783821526630447, -50.10106600002546173 ) ) ;
#51787 = CARTESIAN_POINT ( 'NONE',  ( -165.8925458123985948, 80.86730909018719160, -93.88204572899961420 ) ) ;
#51788 = ORIENTED_EDGE ( 'NONE', *, *, #19128, .F. ) ;
#51789 = AXIS2_PLACEMENT_3D ( 'NONE', #42876, #37963, #16156 ) ;
#51790 = ORIENTED_EDGE ( 'NONE', *, *, #42590, .T. ) ;
#51791 = DIRECTION ( 'NONE',  ( -1.000000000000000000, 0.000000000000000000, 0.000000000000000000 ) ) ;
#51793 = DIRECTION ( 'NONE',  ( 1.000000000000000000, 0.000000000000000000, 0.000000000000000000 ) ) ;
#51792 = AXIS2_PLACEMENT_3D ( 'NONE', #887, #22339, #55742 ) ;
#51794 = DIRECTION ( 'NONE',  ( 5.551115123125781716E-16, 0.000000000000000000, 1.000000000000000000 ) ) ;
#51795 = DIRECTION ( 'NONE',  ( -0.000000000000000000, -1.000000000000000000, -0.000000000000000000 ) ) ;
#51796 = CARTESIAN_POINT ( 'NONE',  ( 139.6324999503821118, 45.02288024089203589, -92.41009172426876717 ) ) ;
#51797 = CARTESIAN_POINT ( 'NONE',  ( 0.000000000000000000, 0.000000000000000000, 170.0000000000000000 ) ) ;
#51798 = CARTESIAN_POINT ( 'NONE',  ( -122.8202784017355498, 45.69728649588466851, -62.41294849004252399 ) ) ;
#51800 = CARTESIAN_POINT ( 'NONE',  ( 204.6977192012829505, 108.0580384837234931, -24.48138044215792419 ) ) ;
#51799 = AXIS2_PLACEMENT_3D ( 'NONE', #58859, #49685, #32139 ) ;
#51801 = CARTESIAN_POINT ( 'NONE',  ( -78.66644367742109978, 23.39876645725289706, 57.26275173013680586 ) ) ;
#51802 = CARTESIAN_POINT ( 'NONE',  ( 410.0000000000000000, 0.000000000000000000, 175.2157797990580832 ) ) ;
#51803 = ORIENTED_EDGE ( 'NONE', *, *, #40585, .T. ) ;
#51804 = CARTESIAN_POINT ( 'NONE',  ( 10.13563904803030979, 7.391572367417535538, -11.22086992224583923 ) ) ;
#51805 = EDGE_LOOP ( 'NONE', ( #68754, #34655 ) ) ;
#51806 = DIRECTION ( 'NONE',  ( 1.000000000000000000, 0.000000000000000000, 0.000000000000000000 ) ) ;
#51807 = VERTEX_POINT ( 'NONE', #57165 ) ;
#51808 = CARTESIAN_POINT ( 'NONE',  ( 60.74750367560238828, -24.13405452624854775, 41.38025477438755928 ) ) ;
#51809 = CARTESIAN_POINT ( 'NONE',  ( 186.2680729609085120, 85.48839327635664631, -76.01000320357321982 ) ) ;
#51810 = CARTESIAN_POINT ( 'NONE',  ( -143.2587158300141539, 60.34092810886536995, 69.22125202308285452 ) ) ;
#51811 = DIRECTION ( 'NONE',  ( 0.7227948638273878901, 0.6910626489868685329, 5.102127870520021228E-18 ) ) ;
#51812 = AXIS2_PLACEMENT_3D ( 'NONE', #50752, #24029, #55327 ) ;
#51813 = LINE ( 'NONE', #3974, #59105 ) ;
#51814 = CARTESIAN_POINT ( 'NONE',  ( -104.1342612728951593, 33.73231160250196581, 3.892347345905328382 ) ) ;
#51815 = CARTESIAN_POINT ( 'NONE',  ( 10.82760985890677752, 7.398654328676808944, -37.37257414635145381 ) ) ;
#51816 = DIRECTION ( 'NONE',  ( 0.000000000000000000, 0.000000000000000000, 1.000000000000000000 ) ) ;
#51817 = EDGE_LOOP ( 'NONE', ( #61550, #59589, #58390, #11194 ) ) ;
#51818 = ORIENTED_EDGE ( 'NONE', *, *, #54648, .T. ) ;
#51819 = CARTESIAN_POINT ( 'NONE',  ( 186.5193936449931869, 85.76190592813432545, 85.31929775637671298 ) ) ;
#51820 = CARTESIAN_POINT ( 'NONE',  ( -25.00000000000000000, 0.000000000000000000, 0.000000000000000000 ) ) ;
#51821 = FACE_OUTER_BOUND ( 'NONE', #3, .T. ) ;
#51822 = CARTESIAN_POINT ( 'NONE',  ( 12.69192874957004769, 6.421326776602847453, 3.834725903590704643 ) ) ;
#51823 = CARTESIAN_POINT ( 'NONE',  ( 42.48820792780864508, 9.847387255477764612, -76.80433085855322872 ) ) ;
#51824 = CARTESIAN_POINT ( 'NONE',  ( 183.7875981612220073, 82.83906702837187197, -9.881439232383749882 ) ) ;
#51825 = CARTESIAN_POINT ( 'NONE',  ( 204.6977192012829789, 108.0580384837234931, 17.36317014830577321 ) ) ;
#51826 = EDGE_CURVE ( 'NONE', #66496, #4596, #67723, .T. ) ;
#51827 = CARTESIAN_POINT ( 'NONE',  ( -178.5790738944854184, 93.41591512785082330, -37.06229826213597534 ) ) ;
#51828 = CARTESIAN_POINT ( 'NONE',  ( 93.09528872995976201, 21.72934119836187605, -12.64476263866717431 ) ) ;
#51829 = CARTESIAN_POINT ( 'NONE',  ( -26.88635117726412815, 9.904687797303049379, 70.54110651337641968 ) ) ;
#51830 = DIRECTION ( 'NONE',  ( -0.8090169943749506709, 0.5877852522924686962, 0.000000000000000000 ) ) ;
#51832 = CARTESIAN_POINT ( 'NONE',  ( -54.56693200831792723, 14.55131601960339260, 72.16187836339486239 ) ) ;
#51831 = B_SPLINE_CURVE_WITH_KNOTS ( 'NONE', 3,
 ( #11473, #32261, #48069, #21345, #43829, #32940, #53694, #63916, #49100, #16419, #58285, #64260, #26635, #54382, #5514, #10106, #231, #69186, #10440, #21688, #6207, #43139, #31563, #37877, #37522, #4821, #26291, #21013, #59323, #31913, #53342, #69526, #11135, #32599, #5853, #27308, #48752, #22041, #43486, #50861, #1288, #60719, #39617, #65666, #2677 ),
 .UNSPECIFIED., .F., .F.,
 ( 4, 2, 2, 2, 2, 2, 2, 2, 1, 2, 2, 2, 2, 2, 2, 2, 2, 2, 2, 2, 2, 2, 4 ),
 ( 1.734723475976807094E-18, 0.001467747071934254058, 0.002201620607901382930, 0.002935494143868511586, 0.004403241215802774534, 0.005870988287737037049, 0.007338735359671300432, 0.008072608895638421281, 0.008806482431605545599, 0.009540355967572666449, 0.01027422950353978903, 0.01174197657547401165, 0.01247585011144112556, 0.01320972364740823773, 0.01467747071934244474, 0.01541134425530953436, 0.01614521779127663093, 0.01761296486321079630, 0.01908071193514496861, 0.01981458547111204088, 0.02054845900707912010, 0.02201620607901325771, 0.02348395315094739533 ),
 .UNSPECIFIED. ) ;
#51833 = CARTESIAN_POINT ( 'NONE',  ( -0.8011128725815451768, 6.535315321814157308, 67.10020792668412071 ) ) ;
#51834 = EDGE_LOOP ( 'NONE', ( #23595, #58504 ) ) ;
#51835 = LINE ( 'NONE', #25469, #13680 ) ;
#51836 = CARTESIAN_POINT ( 'NONE',  ( 156.5993887774280040, 58.24868799840904643, 56.30154359095186578 ) ) ;
#51837 = DIRECTION ( 'NONE',  ( -0.8118923937861950435, -0.5838071093367415143, 0.000000000000000000 ) ) ;
#51838 = CARTESIAN_POINT ( 'NONE',  ( -51.78153763344963068, 13.82841714689605794, -49.48256276243913021 ) ) ;
#51839 = DIRECTION ( 'NONE',  ( -0.000000000000000000, -0.000000000000000000, -1.000000000000000000 ) ) ;
#51840 = CARTESIAN_POINT ( 'NONE',  ( -0.9745223251005035170, 7.548327269165426401, 94.42701984305149665 ) ) ;
#51841 = AXIS2_PLACEMENT_3D ( 'NONE', #26072, #10570, #26417 ) ;
#51842 = ORIENTED_EDGE ( 'NONE', *, *, #49509, .T. ) ;
#51843 = DIRECTION ( 'NONE',  ( -1.387778780781398344E-15, 0.000000000000000000, -1.000000000000000000 ) ) ;
#51844 = CARTESIAN_POINT ( 'NONE',  ( 0.000000000000000000, 0.000000000000000000, 41.38025477438755928 ) ) ;
#51845 = EDGE_CURVE ( 'NONE', #67865, #53174, #34683, .T. ) ;
#51846 = ORIENTED_EDGE ( 'NONE', *, *, #49887, .T. ) ;
#51847 = AXIS2_PLACEMENT_3D ( 'NONE', #49959, #44331, #66175 ) ;
#51848 = VERTEX_POINT ( 'NONE', #50841 ) ;
#51849 = CARTESIAN_POINT ( 'NONE',  ( 0.000000000000000000, -31.50328976398030534, 5.000000000000000000 ) ) ;
#51850 = PLANE ( 'NONE',  #10800 ) ;
#51851 = CARTESIAN_POINT ( 'NONE',  ( 24.79066879238609644, 3.228426989449657114, 0.000000000000000000 ) ) ;
#51852 = ORIENTED_EDGE ( 'NONE', *, *, #15498, .T. ) ;
#51853 = CARTESIAN_POINT ( 'NONE',  ( 427.4999999999999432, -18.06806526123148160, 378.0000000000000000 ) ) ;
#51854 = FACE_BOUND ( 'NONE', #66856, .T. ) ;
#51855 = PLANE ( 'NONE',  #2744 ) ;
#51856 = EDGE_CURVE ( 'NONE', #66979, #13790, #61978, .T. ) ;
#51857 = AXIS2_PLACEMENT_3D ( 'NONE', #8210, #46176, #24045 ) ;
#51858 = CARTESIAN_POINT ( 'NONE',  ( 55.14772863908626732, 34.40534879854737227, 40.00000000000003553 ) ) ;
#51859 = CYLINDRICAL_SURFACE ( 'NONE', #24624, 25.00000000000000000 ) ;
#51860 = CARTESIAN_POINT ( 'NONE',  ( 149.9762816496916003, 52.05155590316277880, 90.11743903550856771 ) ) ;
#51861 = CARTESIAN_POINT ( 'NONE',  ( 134.3172730033263349, 41.70277427218490374, 17.66579024853170665 ) ) ;
#51862 = VERTEX_POINT ( 'NONE', #35014 ) ;
#51863 = CARTESIAN_POINT ( 'NONE',  ( 0.3157512944565053492, -3.097794232830064498, 7.999999999999998224 ) ) ;
#51864 = CARTESIAN_POINT ( 'NONE',  ( 9.057575839850576571, 6.378493414438676901, 67.67707940144546797 ) ) ;
#51865 = EDGE_CURVE ( 'NONE', #17049, #14174, #55250, .T. ) ;
#51866 = PLANE ( 'NONE',  #55144 ) ;
#51867 = DIRECTION ( 'NONE',  ( -0.000000000000000000, -0.000000000000000000, -1.000000000000000000 ) ) ;
#51869 = EDGE_LOOP ( 'NONE', ( #17001, #38419, #53902, #121 ) ) ;
#51868 = DIRECTION ( 'NONE',  ( 0.000000000000000000, 0.000000000000000000, -1.000000000000000000 ) ) ;
#51870 = CARTESIAN_POINT ( 'NONE',  ( 50.57199999999998852, 0.000000000000000000, 0.000000000000000000 ) ) ;
#51871 = VERTEX_POINT ( 'NONE', #19171 ) ;
#51872 = ORIENTED_EDGE ( 'NONE', *, *, #3418, .T. ) ;
#51873 = DIRECTION ( 'NONE',  ( 1.954612056407561701E-16, -1.558751100573736303E-16, 1.000000000000000000 ) ) ;
#51874 = DIRECTION ( 'NONE',  ( 1.000000000000000000, 0.000000000000000000, 0.000000000000000000 ) ) ;
#51875 = LINE ( 'NONE', #40978, #10739 ) ;
#51876 = CARTESIAN_POINT ( 'NONE',  ( 186.2722199822850655, 84.01218714714251234, -11.44440540467959799 ) ) ;
#51877 = CARTESIAN_POINT ( 'NONE',  ( -118.9649285217355583, 42.09781191014329949, 62.08225238709908922 ) ) ;
#51878 = CARTESIAN_POINT ( 'NONE',  ( -79.14638003838379632, 23.58242782405879012, -8.270900041254195756 ) ) ;
#51879 = CARTESIAN_POINT ( 'NONE',  ( 16.76400266940279593, 6.533513613209220416, -23.62695608403941705 ) ) ;
#51880 = CARTESIAN_POINT ( 'NONE',  ( -50.53243683205840142, 14.55237037207940531, 43.82175149422371163 ) ) ;
#51881 = VERTEX_POINT ( 'NONE', #55779 ) ;
#51882 = VERTEX_POINT ( 'NONE', #40624 ) ;
#51883 = CARTESIAN_POINT ( 'NONE',  ( -105.4642082819535887, 35.56541171990214423, 17.98124511787474589 ) ) ;
#51884 = CONICAL_SURFACE ( 'NONE', #41748, 8.000000000000001776, 1.047197551196595855 ) ;
#51885 = LINE ( 'NONE', #35371, #45071 ) ;
#51886 = CARTESIAN_POINT ( 'NONE',  ( 102.7351271102982224, 25.56094931096820488, 90.72548476243952109 ) ) ;
#51887 = DIRECTION ( 'NONE',  ( 1.000000000000000000, 0.000000000000000000, 0.000000000000000000 ) ) ;
#51888 = VECTOR ( 'NONE', #29538, 1000.000000000000000 ) ;
#51889 = DIRECTION ( 'NONE',  ( -0.000000000000000000, -1.000000000000000000, -0.000000000000000000 ) ) ;
#51890 = CARTESIAN_POINT ( 'NONE',  ( 0.3167204509598382511, 8.479269695850865318, -1.313474075707213418 ) ) ;
#51891 = CARTESIAN_POINT ( 'NONE',  ( -144.4759242270947937, 61.31787838020377279, 86.31655861621851500 ) ) ;
#51892 = EDGE_LOOP ( 'NONE', ( #43003, #42201, #5895, #8240, #6725, #9279, #18742, #68903, #25626 ) ) ;
#51893 = PRODUCT ( 'y3+', 'y3+', '', ( #56864 ) ) ;
#51894 = ORIENTED_EDGE ( 'NONE', *, *, #26818, .F. ) ;
#51895 = VERTEX_POINT ( 'NONE', #13899 ) ;
#51896 = AXIS2_PLACEMENT_3D ( 'NONE', #58522, #30778, #42359 ) ;
#51897 = CIRCLE ( 'NONE', #58602, 65.00000000000000000 ) ;
#51898 = CARTESIAN_POINT ( 'NONE',  ( -86.06489347855101357, 25.27905598459106784, 63.50647088109550964 ) ) ;
#51899 = CARTESIAN_POINT ( 'NONE',  ( 0.000000000000000000, 0.000000000000000000, 0.000000000000000000 ) ) ;
#51900 = CARTESIAN_POINT ( 'NONE',  ( 103.9024360978282999, 26.05738592538718379, -93.08474446646899025 ) ) ;
#51901 = CIRCLE ( 'NONE', #5838, 245.3095347406802489 ) ;
#51902 = DIRECTION ( 'NONE',  ( -0.4738686624730094610, 0.8805955318567321166, 0.000000000000000000 ) ) ;
#51903 = B_SPLINE_CURVE_WITH_KNOTS ( 'NONE', 3,
 ( #9936, #31389, #22558, #22910, #1107, #33123, #65128, #39104, #17272, #44002 ),
 .UNSPECIFIED., .F., .F.,
 ( 4, 2, 2, 2, 4 ),
 ( 0.000000000000000000, 0.001080786818375976174, 0.002161573636751952347, 0.003242360455127928521, 0.004323147273503904695 ),
 .UNSPECIFIED. ) ;
#51904 = CARTESIAN_POINT ( 'NONE',  ( -435.1627218934913799, 399.9999999999998295, 96.05029585798821756 ) ) ;
#51905 = CARTESIAN_POINT ( 'NONE',  ( 187.5246323291926842, 86.86207184872515086, 67.53503301494710342 ) ) ;
#51906 = CARTESIAN_POINT ( 'NONE',  ( 8.288104306525688969, 6.376394648992967262, -16.66097189769440945 ) ) ;
#51907 =( LENGTH_UNIT ( ) NAMED_UNIT ( * ) SI_UNIT ( .MILLI., .METRE. ) );
#51909 = VERTEX_POINT ( 'NONE', #14256 ) ;
#51908 = ADVANCED_FACE ( 'NONE', ( #34333 ), #35714, .F. ) ;
#51910 = CARTESIAN_POINT ( 'NONE',  ( -1.088326810997878091, 6.545818265928951440, -46.25019226022950392 ) ) ;
#51911 = DIRECTION ( 'NONE',  ( 0.000000000000000000, 0.000000000000000000, -1.000000000000000000 ) ) ;
#51912 = CARTESIAN_POINT ( 'NONE',  ( -124.3331814159187161, 45.47486189329070072, 3.936062064721631337 ) ) ;
#51913 = LINE ( 'NONE', #3720, #20763 ) ;
#51914 = CARTESIAN_POINT ( 'NONE',  ( -442.6627218934918915, 394.9999999999998295, -136.4497041420123367 ) ) ;
#51915 = CARTESIAN_POINT ( 'NONE',  ( 23.23965501943000334, 7.861749956303023978, -17.15812566989634291 ) ) ;
#51916 = CARTESIAN_POINT ( 'NONE',  ( 8.763528846667105299, 7.383598436776578566, 13.30899920650040080 ) ) ;
#51917 = EDGE_CURVE ( 'NONE', #11940, #5635, #58868, .T. ) ;
#51918 = ORIENTED_EDGE ( 'NONE', *, *, #34884, .T. ) ;
#51919 = APPLICATION_PROTOCOL_DEFINITION ( 'draft international standard', 'automotive_design', 1998, #59285 ) ;
#51920 = CARTESIAN_POINT ( 'NONE',  ( 126.8114659053431694, 38.48351437375816175, -46.14626030992690175 ) ) ;
#51921 = FACE_OUTER_BOUND ( 'NONE', #18893, .T. ) ;
#51922 = CARTESIAN_POINT ( 'NONE',  ( -109.6657532478350845, 37.84376708859253569, -43.84539487966294757 ) ) ;
#51923 = CARTESIAN_POINT ( 'NONE',  ( 188.2091813586561670, 87.61952156613881471, -41.36644826682314857 ) ) ;
#51924 = ORIENTED_EDGE ( 'NONE', *, *, #66493, .F. ) ;
#51925 = EDGE_LOOP ( 'NONE', ( #33173, #53677, #1364, #50355 ) ) ;
#51926 = EDGE_CURVE ( 'NONE', #34612, #50750, #42014, .T. ) ;
#51927 = CARTESIAN_POINT ( 'NONE',  ( -28.13852122803041311, 9.072484007196637279, -22.72488694513067031 ) ) ;
#51928 = DIRECTION ( 'NONE',  ( 1.084727855779380319E-16, 2.252460601983949986E-16, 1.000000000000000000 ) ) ;
#51929 = EDGE_CURVE ( 'NONE', #68939, #8769, #23033, .T. ) ;
#51930 = ORIENTED_EDGE ( 'NONE', *, *, #3318, .F. ) ;
#51931 = CARTESIAN_POINT ( 'NONE',  ( 164.9053016786531316, 64.98846293739913449, 89.59488780726475454 ) ) ;
#51932 = VERTEX_POINT ( 'NONE', #47966 ) ;
#51933 = CARTESIAN_POINT ( 'NONE',  ( -59.58556642339446086, 16.99097764963621060, 16.96804118674567974 ) ) ;
#51934 = DIRECTION ( 'NONE',  ( 0.000000000000000000, 0.000000000000000000, 1.000000000000000000 ) ) ;
#51935 = CARTESIAN_POINT ( 'NONE',  ( -155.1359377029286009, 70.46175948311804405, 43.20321676328643434 ) ) ;
#51936 = VECTOR ( 'NONE', #17937, 1000.000000000000000 ) ;
#51937 = EDGE_CURVE ( 'NONE', #16320, #53253, #52564, .T. ) ;
#51938 = EDGE_CURVE ( 'NONE', #6273, #56020, #8066, .T. ) ;
#51939 = DIRECTION ( 'NONE',  ( -0.000000000000000000, -0.000000000000000000, -1.000000000000000000 ) ) ;
#51940 = CARTESIAN_POINT ( 'NONE',  ( -447.6627218934912662, 369.9999999999998295, 108.5502958579877060 ) ) ;
#51941 = AXIS2_PLACEMENT_3D ( 'NONE', #32668, #657, #17167 ) ;
#51943 = ORIENTED_EDGE ( 'NONE', *, *, #34796, .T. ) ;
#51942 = LINE ( 'NONE', #67788, #62290 ) ;
#51944 = CARTESIAN_POINT ( 'NONE',  ( 3.904274594239516283, -38.13466019661239415, 13.32819397642333392 ) ) ;
#51945 = VERTEX_POINT ( 'NONE', #36745 ) ;
#51946 = VECTOR ( 'NONE', #14352, 1000.000000000000114 ) ;
#51947 = EDGE_LOOP ( 'NONE', ( #9659, #39456, #66339, #49325 ) ) ;
#51948 = CARTESIAN_POINT ( 'NONE',  ( -65.36598343705435354, 0.000000000000000000, 41.38025477438755928 ) ) ;
#51949 = ADVANCED_FACE ( 'NONE', ( #5062 ), #57849, .F. ) ;
#51950 = CARTESIAN_POINT ( 'NONE',  ( -34.34470740021929913, 11.10817648171062366, -89.58872634471485696 ) ) ;
#51952 = ORIENTED_EDGE ( 'NONE', *, *, #1578, .T. ) ;
#51951 = DIRECTION ( 'NONE',  ( 0.000000000000000000, 0.000000000000000000, 1.000000000000000000 ) ) ;
#51953 = CARTESIAN_POINT ( 'NONE',  ( 133.8566784816069344, -170.0000000000000000, -43.52331093239567394 ) ) ;
#51954 = ADVANCED_FACE ( 'NONE', ( #41334 ), #58188, .F. ) ;
#51955 = EDGE_CURVE ( 'NONE', #5719, #52465, #36397, .T. ) ;
#51956 = CARTESIAN_POINT ( 'NONE',  ( -28.32746765835430836, -69.45586423092646555, 170.0000000000000000 ) ) ;
#51957 = EDGE_CURVE ( 'NONE', #8171, #2857, #10011, .T. ) ;
#51958 = VERTEX_POINT ( 'NONE', #20907 ) ;
#51959 = CARTESIAN_POINT ( 'NONE',  ( -56.02027488966933078, 14.94257193099085868, -8.418912259423796840 ) ) ;
#51960 = CARTESIAN_POINT ( 'NONE',  ( -128.1282195935087884, 49.19720162550164844, -76.42132434122385121 ) ) ;
#51961 = CARTESIAN_POINT ( 'NONE',  ( 117.4711568421289627, 33.49899443629671936, 39.17702909593091931 ) ) ;
#51962 = CARTESIAN_POINT ( 'NONE',  ( -126.3495878770406193, 48.00153794568855403, 18.77539728269342234 ) ) ;
#51963 = CARTESIAN_POINT ( 'NONE',  ( 70.26639875985989647, 15.51307715494296069, -68.08326665301770220 ) ) ;
#51964 = ORIENTED_EDGE ( 'NONE', *, *, #30989, .T. ) ;
#51965 = ORIENTED_EDGE ( 'NONE', *, *, #56523, .T. ) ;
#51966 = LINE ( 'NONE', #56552, #21467 ) ;
#51967 = CARTESIAN_POINT ( 'NONE',  ( -171.4814970982680222, 85.32124710276291069, -34.88158325180384622 ) ) ;
#51968 = CARTESIAN_POINT ( 'NONE',  ( 19.00668540189274225, -62.54164772954691642, 43.58025477438756212 ) ) ;
#51969 = DIRECTION ( 'NONE',  ( 1.000000000000000000, 0.000000000000000000, 0.000000000000000000 ) ) ;
#51970 = CARTESIAN_POINT ( 'NONE',  ( 262.2516123306975260, 190.0000000000000000, -21.28179539054375624 ) ) ;
#51971 = FACE_OUTER_BOUND ( 'NONE', #23529, .T. ) ;
#51972 = CARTESIAN_POINT ( 'NONE',  ( -144.9287131874381771, 60.39056348581543432, 44.18048465558430848 ) ) ;
#51973 = FACE_OUTER_BOUND ( 'NONE', #66292, .T. ) ;
#51974 = CARTESIAN_POINT ( 'NONE',  ( 209.9944361927104808, 113.8994774711241007, 58.23723418828768672 ) ) ;
#51975 = ORIENTED_EDGE ( 'NONE', *, *, #12159, .F. ) ;
#51976 = CARTESIAN_POINT ( 'NONE',  ( -109.5157885508426574, 37.76058765671428574, 40.06018348045786581 ) ) ;
#51978 = EDGE_LOOP ( 'NONE', ( #7118, #65192, #69317, #45119 ) ) ;
#51977 = B_SPLINE_CURVE_WITH_KNOTS ( 'NONE', 3,
 ( #63759, #15567, #69013, #26808, #26467, #52506 ),
 .UNSPECIFIED., .F., .F.,
 ( 4, 2, 4 ),
 ( 0.03218937259408877899, 0.06469834484649478190, 0.09720731709890076400 ),
 .UNSPECIFIED. ) ;
#51979 = CARTESIAN_POINT ( 'NONE',  ( 86.62931800182292363, 20.48449268398425716, -89.51066537983906812 ) ) ;
#51980 = CARTESIAN_POINT ( 'NONE',  ( 79.52639011421921111, 18.17129627604991171, 66.51676211103118419 ) ) ;
#51981 = ORIENTED_EDGE ( 'NONE', *, *, #5307, .F. ) ;
#51982 = CARTESIAN_POINT ( 'NONE',  ( -83.23830101421552286, 24.11594324015501201, -90.35514600372840732 ) ) ;
#51983 = CARTESIAN_POINT ( 'NONE',  ( 31.71171398032105060, -10.56647026444650272, 6.893342932883488317 ) ) ;
#51984 = PLANE ( 'NONE',  #15276 ) ;
#51985 = LINE ( 'NONE', #68511, #45068 ) ;
#51986 = CARTESIAN_POINT ( 'NONE',  ( 33.76124497394584267, 7.742545529019360551, 15.53639134207576511 ) ) ;
#51987 = CARTESIAN_POINT ( 'NONE',  ( -10.92576759990585167, 8.121994053275063408, -36.08453108487010752 ) ) ;
#51988 = VECTOR ( 'NONE', #66929, 1000.000000000000000 ) ;
#51989 = CARTESIAN_POINT ( 'NONE',  ( -125.8938041572051389, -170.0000000000000000, -88.60280507916129977 ) ) ;
#51990 = EDGE_LOOP ( 'NONE', ( #14251, #61370, #67660, #60470 ) ) ;
#51991 = VECTOR ( 'NONE', #47037, 1000.000000000000114 ) ;
#51992 = CARTESIAN_POINT ( 'NONE',  ( -121.9323109100150191, 45.13109664935808496, -89.73066178333888843 ) ) ;
#51993 = ORIENTED_EDGE ( 'NONE', *, *, #13358, .T. ) ;
#51994 = CARTESIAN_POINT ( 'NONE',  ( -59.95707852844800101, 16.05120821151903954, 32.12152303550877264 ) ) ;
#51995 = CARTESIAN_POINT ( 'NONE',  ( -26.00000000000000000, 0.000000000000000000, -2.818925648462311923E-15 ) ) ;
#51996 = CARTESIAN_POINT ( 'NONE',  ( -190.4966031023458584, 108.8421921967458843, 15.75534704198573088 ) ) ;
#51997 = CARTESIAN_POINT ( 'NONE',  ( 0.000000000000000000, 50.00000000000000000, 0.000000000000000000 ) ) ;
#51998 = CARTESIAN_POINT ( 'NONE',  ( -61.25157674566710853, 16.43158121994553511, -92.17786549963551579 ) ) ;
#51999 = CARTESIAN_POINT ( 'NONE',  ( -95.61819996182573789, 29.52346081122277255, -12.21564220075769391 ) ) ;
#52000 = CIRCLE ( 'NONE', #48596, 8.000000000000000000 ) ;
#52001 =( LENGTH_UNIT ( ) NAMED_UNIT ( * ) SI_UNIT ( .MILLI., .METRE. ) );
#52002 = EDGE_CURVE ( 'NONE', #7110, #56044, #21552, .T. ) ;
#52003 = VECTOR ( 'NONE', #45154, 1000.000000000000000 ) ;
#52004 = VERTEX_POINT ( 'NONE', #52899 ) ;
#52006 = CONICAL_SURFACE ( 'NONE', #54232, 74.95140232871122521, 0.8777644062502172329 ) ;
#52005 = DIRECTION ( 'NONE',  ( 0.3794257103289241928, 3.271872096745526795E-17, 0.9252222059275228006 ) ) ;
#52007 = CARTESIAN_POINT ( 'NONE',  ( -156.0209085498132140, 71.27066046086517304, 61.30830681328009035 ) ) ;
#52008 = DIRECTION ( 'NONE',  ( 0.000000000000000000, 1.000000000000000000, 0.000000000000000000 ) ) ;
#52009 = CARTESIAN_POINT ( 'NONE',  ( -121.5921196778232058, 43.72569502503144179, 31.95820139695877771 ) ) ;
#52010 = CYLINDRICAL_SURFACE ( 'NONE', #52385, 7.500000000000020428 ) ;
#52011 = VERTEX_POINT ( 'NONE', #31130 ) ;
#52012 = CARTESIAN_POINT ( 'NONE',  ( -180.5234362879039622, 97.35934147644944403, -67.80900013366066048 ) ) ;
#52013 = CARTESIAN_POINT ( 'NONE',  ( 127.0069430753658395, 38.59356149538464109, 93.77475522799868202 ) ) ;
#52014 = EDGE_CURVE ( 'NONE', #44986, #29362, #18791, .T. ) ;
#52016 = EDGE_CURVE ( 'NONE', #52425, #21098, #3711, .T. ) ;
#52015 = CARTESIAN_POINT ( 'NONE',  ( 113.8568724296587504, 30.58972477291342784, 30.52184481816738781 ) ) ;
#52017 = DIRECTION ( 'NONE',  ( 0.4578834044730071828, 0.000000000000000000, -0.8890122540821405739 ) ) ;
#52018 = ADVANCED_FACE ( 'NONE', ( #60963 ), #66957, .T. ) ;
#52019 = CARTESIAN_POINT ( 'NONE',  ( -20.63749999999999929, 2.632990618166809235E-15, 21.50000000000000000 ) ) ;
#52020 = EDGE_CURVE ( 'NONE', #29274, #67595, #16291, .T. ) ;
#52021 = EDGE_LOOP ( 'NONE', ( #30600, #2790, #62447, #44200 ) ) ;
#52022 = DIRECTION ( 'NONE',  ( 0.000000000000000000, 0.000000000000000000, 1.000000000000000000 ) ) ;
#52023 = CARTESIAN_POINT ( 'NONE',  ( 116.6457744947906860, 31.95847117670279403, -74.18078547863080985 ) ) ;
#52024 = CARTESIAN_POINT ( 'NONE',  ( 186.6075385349484463, 85.85749512876287781, 31.71040953412066088 ) ) ;
#52025 = CARTESIAN_POINT ( 'NONE',  ( 141.3586046882815310, 47.34625111366352712, 9.656894089140847015 ) ) ;
#52026 = DIRECTION ( 'NONE',  ( 0.000000000000000000, 1.000000000000000000, 0.000000000000000000 ) ) ;
#52027 = EDGE_LOOP ( 'NONE', ( #33669, #16968, #41083, #38105 ) ) ;
#52028 = DIRECTION ( 'NONE',  ( 1.000000000000000000, 0.000000000000000000, 0.000000000000000000 ) ) ;
#52029 = ORIENTED_EDGE ( 'NONE', *, *, #34901, .T. ) ;
#52030 = CARTESIAN_POINT ( 'NONE',  ( 70.51522979775972999, 15.57935281015687146, 64.65971896463177870 ) ) ;
#52031 = CARTESIAN_POINT ( 'NONE',  ( 132.6840581302284079, 40.72084251088482176, 83.28510945087752759 ) ) ;
#52032 = VECTOR ( 'NONE', #6655, 1000.000000000000000 ) ;
#52033 = AXIS2_PLACEMENT_3D ( 'NONE', #13821, #53160, #58790 ) ;
#52035 = VERTEX_POINT ( 'NONE', #14508 ) ;
#52034 = CARTESIAN_POINT ( 'NONE',  ( -51.84164840787130402, -39.21024726209533640, 170.0000000000000000 ) ) ;
#52036 = CARTESIAN_POINT ( 'NONE',  ( -180.3153482337535252, 95.51031295027644319, 40.46297689070883763 ) ) ;
#52037 = CARTESIAN_POINT ( 'NONE',  ( 447.3372781065086201, 400.0000000000044338, 113.5502958579838122 ) ) ;
#52038 = ADVANCED_FACE ( 'NONE', ( #36313 ), #65356, .T. ) ;
#52039 = EDGE_CURVE ( 'NONE', #44366, #40373, #63394, .T. ) ;
#52040 = CARTESIAN_POINT ( 'NONE',  ( 115.7731501832035832, 32.64791439093733061, -48.51258337113941366 ) ) ;
#52041 = ORIENTED_EDGE ( 'NONE', *, *, #23993, .T. ) ;
#52042 = ADVANCED_FACE ( 'NONE', ( #9582 ), #63039, .F. ) ;
#52043 = CARTESIAN_POINT ( 'NONE',  ( 16.92909695399013259, -28.82167194761692386, 6.893342934305374925 ) ) ;
#52044 = VECTOR ( 'NONE', #1453, 1000.000000000000000 ) ;
#52045 = AXIS2_PLACEMENT_3D ( 'NONE', #16448, #64986, #53024 ) ;
#52046 = CARTESIAN_POINT ( 'NONE',  ( -132.4819073909166320, 50.98736898418872698, 41.74248034566528531 ) ) ;
#52047 = DIRECTION ( 'NONE',  ( 0.000000000000000000, 0.000000000000000000, 1.000000000000000000 ) ) ;
#52048 = CARTESIAN_POINT ( 'NONE',  ( 79.14113188808478583, 18.05280674635442040, -15.98610417696640695 ) ) ;
#52049 = CARTESIAN_POINT ( 'NONE',  ( -175.8203575500379259, 91.72143465022357134, -88.89240186285151424 ) ) ;
#52050 = AXIS2_PLACEMENT_3D ( 'NONE', #27942, #55370, #55730 ) ;
#52051 = CARTESIAN_POINT ( 'NONE',  ( 0.000000000000000000, 0.000000000000000000, 0.000000000000000000 ) ) ;
#52052 = CARTESIAN_POINT ( 'NONE',  ( 86.62931800182293784, 20.48449268398423229, 44.71208757247933363 ) ) ;
#52053 = ORIENTED_EDGE ( 'NONE', *, *, #10223, .T. ) ;
#52054 = DIRECTION ( 'NONE',  ( -0.000000000000000000, -0.000000000000000000, 1.000000000000000000 ) ) ;
#52055 = DIRECTION ( 'NONE',  ( 2.220446049250313081E-16, 0.000000000000000000, 1.000000000000000000 ) ) ;
#52056 = VERTEX_POINT ( 'NONE', #46509 ) ;
#52057 = VECTOR ( 'NONE', #65938, 1000.000000000000000 ) ;
#52058 = CARTESIAN_POINT ( 'NONE',  ( 152.1153500913667358, 54.85403770686897218, -11.52264547865338429 ) ) ;
#52059 = CARTESIAN_POINT ( 'NONE',  ( 210.6584452238134872, 116.7138338345753965, -21.56006559325671645 ) ) ;
#52060 = CARTESIAN_POINT ( 'NONE',  ( 106.0228389049370463, 28.07756796303168656, 30.90652886002973077 ) ) ;
#52061 = CARTESIAN_POINT ( 'NONE',  ( -0.7076388175553600668, 7.538734751903869657, 35.20121844452963700 ) ) ;
#52062 = CARTESIAN_POINT ( 'NONE',  ( -173.1211646369891355, -170.0000000000000000, 30.82169460664101734 ) ) ;
#52063 = CARTESIAN_POINT ( 'NONE',  ( 186.6075385349484463, 85.85749512876287781, 4.865858943656973246 ) ) ;
#52064 = CARTESIAN_POINT ( 'NONE',  ( 211.1200456646897123, 115.5868795682034005, -39.94236214982109345 ) ) ;
#52065 = CARTESIAN_POINT ( 'NONE',  ( 176.6214367443247681, 74.20967084876664899, 16.01070763406217523 ) ) ;
#52066 = EDGE_LOOP ( 'NONE', ( #57377, #16403 ) ) ;
#52067 = CARTESIAN_POINT ( 'NONE',  ( 16.78635691501517613, 0.000000000000000000, -9.435653166495500344 ) ) ;
#52068 = ORIENTED_EDGE ( 'NONE', *, *, #69261, .F. ) ;
#52069 = CARTESIAN_POINT ( 'NONE',  ( -73.81801970646056077, 21.60231032711190835, 70.49010474810707194 ) ) ;
#52070 = DIRECTION ( 'NONE',  ( -1.000000000000000000, -1.387778780781438033E-16, 0.000000000000000000 ) ) ;
#52071 = DIRECTION ( 'NONE',  ( 0.000000000000000000, -1.000000000000000000, 0.000000000000000000 ) ) ;
#52072 = CARTESIAN_POINT ( 'NONE',  ( -8.487474335736092002, 6.934846266162439044, 83.82687023565640061 ) ) ;
#52073 = CARTESIAN_POINT ( 'NONE',  ( -108.1180879163843116, 36.99199941971029659, -10.93529391401303386 ) ) ;
#52074 = EDGE_LOOP ( 'NONE', ( #59799, #66898 ) ) ;
#52075 = CARTESIAN_POINT ( 'NONE',  ( -74.19961951691010427, 20.67022044985852602, 58.73306680916620337 ) ) ;
#52076 = CARTESIAN_POINT ( 'NONE',  ( 202.1083097594007256, 102.8573673850798542, -90.44468564295731028 ) ) ;
#52077 = EDGE_LOOP ( 'NONE', ( #16080, #23231, #32812, #45638 ) ) ;
#52078 = ORIENTED_EDGE ( 'NONE', *, *, #21365, .F. ) ;
#52079 = CARTESIAN_POINT ( 'NONE',  ( -156.3790798118593273, 70.23422112803315542, 35.20372313786793228 ) ) ;
#52080 = CARTESIAN_POINT ( 'NONE',  ( -49.45633250947157933, 14.94581096590798630, 26.66469104408688295 ) ) ;
#52081 = CARTESIAN_POINT ( 'NONE',  ( 175.3815143714021190, 73.02838262206998365, -12.00236747850586916 ) ) ;
#52082 = CARTESIAN_POINT ( 'NONE',  ( -33.00963958485551331, 25.52799196440124163, 13.79046340968177553 ) ) ;
#52083 = EDGE_CURVE ( 'NONE', #41324, #6058, #47199, .T. ) ;
#52084 = VECTOR ( 'NONE', #5701, 1000.000000000000000 ) ;
#52085 = CARTESIAN_POINT ( 'NONE',  ( 133.8566784816069060, 42.60093787723652525, -9.178760341931967659 ) ) ;
#52086 = ORIENTED_EDGE ( 'NONE', *, *, #14382, .F. ) ;
#52087 = DIRECTION ( 'NONE',  ( 0.8724002309921654597, 0.000000000000000000, 0.4887922226926451619 ) ) ;
#52088 = ORIENTED_EDGE ( 'NONE', *, *, #12416, .F. ) ;
#52089 = CARTESIAN_POINT ( 'NONE',  ( 207.4696221732442041, 110.2206209205162253, 2.882253511827710835 ) ) ;
#52090 = CARTESIAN_POINT ( 'NONE',  ( 9.050324533885198974, 7.384616180193985358, 61.02893197393973423 ) ) ;
#52091 = AXIS2_PLACEMENT_3D ( 'NONE', #38764, #59845, #55626 ) ;
#52092 = FACE_BOUND ( 'NONE', #34102, .T. ) ;
#52093 = EDGE_CURVE ( 'NONE', #41218, #22868, #41251, .T. ) ;
#52094 = CIRCLE ( 'NONE', #58807, 65.00000000000000000 ) ;
#52095 = CONICAL_SURFACE ( 'NONE', #36338, 74.95140232871122521, 0.8777644062502172329 ) ;
#52096 = EDGE_CURVE ( 'NONE', #29274, #29060, #15937, .T. ) ;
#52097 = ORIENTED_EDGE ( 'NONE', *, *, #45878, .T. ) ;
#52098 = EDGE_CURVE ( 'NONE', #18617, #24506, #10426, .T. ) ;
#52099 = ORIENTED_EDGE ( 'NONE', *, *, #34734, .F. ) ;
#52100 = LINE ( 'NONE', #9889, #56998 ) ;
#52101 = CARTESIAN_POINT ( 'NONE',  ( -118.5222689009585935, 43.00653498780619088, 90.38654037676664643 ) ) ;
#52102 = VECTOR ( 'NONE', #31736, 1000.000000000000000 ) ;
#52103 = CARTESIAN_POINT ( 'NONE',  ( -165.7138623879809529, 79.24467249981145756, -14.15247808995200174 ) ) ;
#52104 = CARTESIAN_POINT ( 'NONE',  ( -179.8989115484066872, 96.59045402602909292, 14.70008741146901343 ) ) ;
#52105 = CARTESIAN_POINT ( 'NONE',  ( 8.313220962251200774, 6.376421556596937990, 91.89783802061894846 ) ) ;
#52106 = CARTESIAN_POINT ( 'NONE',  ( -7.825402957745083654, 6.891034867348166060, 3.271030448983516692 ) ) ;
#52107 = ORIENTED_EDGE ( 'NONE', *, *, #29153, .F. ) ;
#52108 = DIRECTION ( 'NONE',  ( 1.000000000000000000, 0.000000000000000000, 0.000000000000000000 ) ) ;
#52109 = CARTESIAN_POINT ( 'NONE',  ( -96.78198318406116130, 30.07417864442863120, 59.73932225907307014 ) ) ;
#52110 = ORIENTED_EDGE ( 'NONE', *, *, #63682, .F. ) ;
#52111 = CARTESIAN_POINT ( 'NONE',  ( -79.61931371420119774, 22.68640080971621842, 18.52793425929278825 ) ) ;
#52112 = ORIENTED_EDGE ( 'NONE', *, *, #21051, .F. ) ;
#52113 = CARTESIAN_POINT ( 'NONE',  ( -61.53550548562875377, 17.56596194025585334, -12.06819366122919845 ) ) ;
#52114 =( REPRESENTATION_RELATIONSHIP ('NONE','NONE', #40274, #60409 ) REPRESENTATION_RELATIONSHIP_WITH_TRANSFORMATION ( #35048 )SHAPE_REPRESENTATION_RELATIONSHIP( ) );
#52115 = ORIENTED_EDGE ( 'NONE', *, *, #60502, .T. ) ;
#52116 = EDGE_LOOP ( 'NONE', ( #55373, #40097, #39935, #43228 ) ) ;
#52117 = CARTESIAN_POINT ( 'NONE',  ( 10.13846145460683346, 6.385368868491632988, -38.06222546885739888 ) ) ;
#52118 = CARTESIAN_POINT ( 'NONE',  ( -107.3393890951915068, 36.56899896043363185, -90.64997796909688077 ) ) ;
#52119 = CARTESIAN_POINT ( 'NONE',  ( 109.7732660198864210, 29.77277639096405792, 17.76666361527367144 ) ) ;
#52120 = ORIENTED_EDGE ( 'NONE', *, *, #7147, .T. ) ;
#52121 = EDGE_CURVE ( 'NONE', #13679, #35908, #23840, .T. ) ;
#52122 = CARTESIAN_POINT ( 'NONE',  ( -38.44802608776349473, 10.84733462796151215, 88.71676382914708370 ) ) ;
#52123 = CARTESIAN_POINT ( 'NONE',  ( 175.5429257635130682, 74.57009623370768736, -65.48940413290104345 ) ) ;
#52124 = AXIS2_PLACEMENT_3D ( 'NONE', #19044, #49649, #22938 ) ;
#52125 = DIRECTION ( 'NONE',  ( -0.000000000000000000, -0.000000000000000000, -1.000000000000000000 ) ) ;
#52126 = CARTESIAN_POINT ( 'NONE',  ( 105.4375968828853587, 26.72149058755205786, -37.65901433614699556 ) ) ;
#52127 = CARTESIAN_POINT ( 'NONE',  ( 86.62931800182293784, 20.48449268398422873, -50.82156419891174437 ) ) ;
#52128 = LINE ( 'NONE', #45117, #68074 ) ;
#52129 = ORIENTED_EDGE ( 'NONE', *, *, #15323, .T. ) ;
#52130 = VECTOR ( 'NONE', #9335, 1000.000000000000000 ) ;
#52131 = ORIENTED_EDGE ( 'NONE', *, *, #47955, .T. ) ;
#52132 = DIRECTION ( 'NONE',  ( 1.000000000000000000, 0.000000000000000000, 0.000000000000000000 ) ) ;
#52133 = VECTOR ( 'NONE', #32440, 1000.000000000000000 ) ;
#52134 = CARTESIAN_POINT ( 'NONE',  ( -83.15209219203883606, 25.16621997697721014, -63.42963256430944341 ) ) ;
#52135 = CARTESIAN_POINT ( 'NONE',  ( -6.972640973861005342, 6.835494286893509575, -89.10717191287116634 ) ) ;
#52136 = CYLINDRICAL_SURFACE ( 'NONE', #50292, 200.0000000000000000 ) ;
#52137 = CARTESIAN_POINT ( 'NONE',  ( 0.000000000000000000, 70.00000000000000000, 0.000000000000000000 ) ) ;
#52138 = CARTESIAN_POINT ( 'NONE',  ( 129.5193594945038740, 38.86618897895341718, 16.30267058858694895 ) ) ;
#52139 = AXIS2_PLACEMENT_3D ( 'NONE', #54204, #27488, #48927 ) ;
#52140 = CARTESIAN_POINT ( 'NONE',  ( 34.01806748219127741, 7.770218348519284390, -91.58336029640328491 ) ) ;
#52141 = CARTESIAN_POINT ( 'NONE',  ( -118.3918229753714826, 42.92682904595257298, -69.76788943947511257 ) ) ;
#52142 = VECTOR ( 'NONE', #3320, 999.9999999999998863 ) ;
#52143 = CARTESIAN_POINT ( 'NONE',  ( -189.8133172329396814, -170.0000000000000000, 94.99999999999866418 ) ) ;
#52144 = LINE ( 'NONE', #57083, #25297 ) ;
#52145 = CARTESIAN_POINT ( 'NONE',  ( -102.2801239173131194, 32.78103895658057354, 45.51907450641513009 ) ) ;
#52146 = ORIENTED_EDGE ( 'NONE', *, *, #55443, .F. ) ;
#52147 = CIRCLE ( 'NONE', #44246, 25.12245591505646303 ) ;
#52148 = CARTESIAN_POINT ( 'NONE',  ( -59.23442743245837505, 16.88959283244545162, 85.27218783227613130 ) ) ;
#52149 = ORIENTED_EDGE ( 'NONE', *, *, #50040, .F. ) ;
#52150 = DIRECTION ( 'NONE',  ( 0.000000000000000000, 1.000000000000000000, 0.000000000000000000 ) ) ;
#52151 = EDGE_LOOP ( 'NONE', ( #62887, #294 ) ) ;
#52152 = DIRECTION ( 'NONE',  ( 0.000000000000000000, 0.000000000000000000, 1.000000000000000000 ) ) ;
#52153 = CARTESIAN_POINT ( 'NONE',  ( -447.6627218934916073, 369.9999999999953957, 108.5502958579925377 ) ) ;
#52154 = FACE_OUTER_BOUND ( 'NONE', #49674, .T. ) ;
#52155 = LINE ( 'NONE', #18500, #58053 ) ;
#52156 = CARTESIAN_POINT ( 'NONE',  ( 138.1901928158493149, 45.29454828899442731, -37.38403742761511950 ) ) ;
#52157 = CARTESIAN_POINT ( 'NONE',  ( 34.84173759613680943, 7.859847277726513148, -37.14537742033876100 ) ) ;
#52158 = CARTESIAN_POINT ( 'NONE',  ( 198.7765072002625288, 98.56267746775340299, 94.99999999999866418 ) ) ;
#52159 = CARTESIAN_POINT ( 'NONE',  ( 8.336237313193160858, 7.382629160459401874, -42.04131975006048094 ) ) ;
#52160 = CARTESIAN_POINT ( 'NONE',  ( 127.4953815656694758, 37.71366486045444333, -39.51891617239016341 ) ) ;
#52161 = ORIENTED_EDGE ( 'NONE', *, *, #17452, .T. ) ;
#52162 = ADVANCED_FACE ( 'NONE', ( #48558 ), #27470, .T. ) ;
#52163 = VERTEX_POINT ( 'NONE', #65831 ) ;
#52164 = ADVANCED_FACE ( 'NONE', ( #54188 ), #17626, .F. ) ;
#52165 = CARTESIAN_POINT ( 'NONE',  ( 173.5849338432005879, 72.72001811100811608, 90.26313734863605021 ) ) ;
#52166 = CARTESIAN_POINT ( 'NONE',  ( -63.33140416796853600, 16.18162651919394435, 43.58025477438756212 ) ) ;
#52167 = ADVANCED_FACE ( 'NONE', ( #5337 ), #59127, .F. ) ;
#52168 = DIRECTION ( 'NONE',  ( -0.000000000000000000, 0.000000000000000000, -1.000000000000000000 ) ) ;
#52169 = UNCERTAINTY_MEASURE_WITH_UNIT (LENGTH_MEASURE( 1.000000000000000082E-05 ), #7025, 'distance_accuracy_value', 'NONE');
#52170 = CARTESIAN_POINT ( 'NONE',  ( 15.29293866748103881, 6.484959508098435244, 18.17015708224156967 ) ) ;
#52171 = DIRECTION ( 'NONE',  ( 0.000000000000000000, 0.000000000000000000, 1.000000000000000000 ) ) ;
#52172 = PLANE ( 'NONE',  #33509 ) ;
#52173 = CARTESIAN_POINT ( 'NONE',  ( 174.2469308602415197, 71.96142024047684060, -73.66458895490379177 ) ) ;
#52174 = DIRECTION ( 'NONE',  ( -0.000000000000000000, -0.000000000000000000, -1.000000000000000000 ) ) ;
#52175 = CARTESIAN_POINT ( 'NONE',  ( 88.28780346671264567, 19.99350429399659035, -23.79527902889355673 ) ) ;
#52176 = CARTESIAN_POINT ( 'NONE',  ( -24.61094659556677655, 9.585225265507402170, 67.67335607608715975 ) ) ;
#52177 = DIRECTION ( 'NONE',  ( -1.000000000000000000, -0.000000000000000000, -0.000000000000000000 ) ) ;
#52178 = CARTESIAN_POINT ( 'NONE',  ( -48.99162761293258228, 13.13973062091724131, 60.23760786283060753 ) ) ;
#52179 = VECTOR ( 'NONE', #25921, 1000.000000000000000 ) ;
#52180 = EDGE_CURVE ( 'NONE', #52822, #21908, #66652, .T. ) ;
#52181 = ORIENTED_EDGE ( 'NONE', *, *, #37320, .F. ) ;
#52182 = EDGE_CURVE ( 'NONE', #45785, #5837, #6194, .T. ) ;
#52183 = CARTESIAN_POINT ( 'NONE',  ( 48.39383208188444030, -43.94028683479018582, 41.38025477438755928 ) ) ;
#52184 = DIRECTION ( 'NONE',  ( 0.000000000000000000, 0.000000000000000000, 1.000000000000000000 ) ) ;
#52185 = CARTESIAN_POINT ( 'NONE',  ( -107.0809603157386505, 36.42942792191063006, -63.57645921949710299 ) ) ;
#52186 = CARTESIAN_POINT ( 'NONE',  ( -47.61380558691494258, 12.81230778489787880, -41.72929327147289058 ) ) ;
#52187 = CYLINDRICAL_SURFACE ( 'NONE', #36869, 5.000000000000000888 ) ;
#52188 = CARTESIAN_POINT ( 'NONE',  ( 0.000000000000000000, 0.000000000000000000, 0.000000000000000000 ) ) ;
#52189 = CIRCLE ( 'NONE', #27419, 5.000000000000018652 ) ;
#52190 = ORIENTED_EDGE ( 'NONE', *, *, #60571, .F. ) ;
#52191 = VECTOR ( 'NONE', #62199, 1000.000000000000000 ) ;
#52192 = CONICAL_SURFACE ( 'NONE', #16228, 65.00000000000000000, 0.7853981633974497223 ) ;
#52193 = CARTESIAN_POINT ( 'NONE',  ( -57.65733424639441296, 15.39521790791522804, 71.69929679271069745 ) ) ;
#52194 = ORIENTED_EDGE ( 'NONE', *, *, #356, .F. ) ;
#52195 = ORIENTED_EDGE ( 'NONE', *, *, #3730, .F. ) ;
#52196 = B_SPLINE_CURVE_WITH_KNOTS ( 'NONE', 3,
 ( #10941, #38370, #1092, #54181, #32412, #6002, #22544, #59471, #28522, #65465, #48550, #1802, #65113, #385, #53837, #16910, #17257, #43636, #59815, #27461, #5656, #33800, #27116, #11630, #33468, #60173, #21840, #22894, #1441, #43286, #54540, #6367, #27821, #44337, #49258, #11281, #65824, #38728, #48906, #43985, #39089, #42940, #11994, #54890, #6713 ),
 .UNSPECIFIED., .F., .F.,
 ( 4, 2, 2, 1, 2, 2, 2, 2, 2, 2, 2, 2, 2, 2, 2, 2, 2, 2, 2, 2, 2, 2, 4 ),
 ( 0.02348395315094737798, 0.02495010856601295041, 0.02568318627354573488, 0.02641626398107851936, 0.02714934168861130731, 0.02788241939614409179, 0.02934857481120968503, 0.03008165251874248339, 0.03081473022627528174, 0.03228088564134087846, 0.03301396334887367334, 0.03374704105640646823, 0.03521319647147206494, 0.03667935188653766165, 0.03741242959407043572, 0.03814550730160321673, 0.03961166271666881344, 0.04107781813173440322, 0.04254397354679999299, 0.04327705125433278094, 0.04401012896186556889, 0.04547628437693113784, 0.04694243979199670680 ),
 .UNSPECIFIED. ) ;
#52197 = AXIS2_PLACEMENT_3D ( 'NONE', #31780, #10317, #52203 ) ;
#52198 = DIRECTION ( 'NONE',  ( -0.1342332658176522420, -0.9909497617679352555, 3.104767966278886959E-17 ) ) ;
#52199 = FACE_OUTER_BOUND ( 'NONE', #53640, .T. ) ;
#52200 = CARTESIAN_POINT ( 'NONE',  ( -102.2801239173131052, 32.78103895658057354, 57.36362509687880618 ) ) ;
#52201 = VERTEX_POINT ( 'NONE', #19356 ) ;
#52202 = CARTESIAN_POINT ( 'NONE',  ( 31.11269837220806522, 4.999999999999936939, 0.000000000000000000 ) ) ;
#52203 = DIRECTION ( 'NONE',  ( 1.000000000000000000, 0.000000000000000000, 0.000000000000000000 ) ) ;
#52204 = CARTESIAN_POINT ( 'NONE',  ( 56.52885800925552928, 12.28784885070978561, -47.01758796310792832 ) ) ;
#52205 = CARTESIAN_POINT ( 'NONE',  ( -86.16710354151693707, 26.41338104675946497, 38.15269484146957524 ) ) ;
#52206 = CARTESIAN_POINT ( 'NONE',  ( -24.71645982722742119, 9.599558729461499240, -12.63840101433433993 ) ) ;
#52207 = CARTESIAN_POINT ( 'NONE',  ( 89.87518614971251907, 20.55373388674513180, 30.43397069802014698 ) ) ;
#52208 = EDGE_LOOP ( 'NONE', ( #57021, #69455, #1518, #55989 ) ) ;
#52209 = FILL_AREA_STYLE ('',( #53223 ) ) ;
#52210 = CARTESIAN_POINT ( 'NONE',  ( 13.37820144534468092, 6.435512790162279728, 71.46574325679264916 ) ) ;
#52211 = LINE ( 'NONE', #36039, #34074 ) ;
#52212 = CARTESIAN_POINT ( 'NONE',  ( 197.3119541548906568, 98.33923235143194574, 35.39365102528960705 ) ) ;
#52213 = CARTESIAN_POINT ( 'NONE',  ( -71.16355647947769114, 20.66831286809284762, 91.86052901098470613 ) ) ;
#52215 = ORIENTED_EDGE ( 'NONE', *, *, #50188, .T. ) ;
#52214 = DIRECTION ( 'NONE',  ( 0.000000000000000000, -1.000000000000000000, 0.000000000000000000 ) ) ;
#52216 = CARTESIAN_POINT ( 'NONE',  ( 66.30636076182547356, 14.49616748423541779, 44.07007479522269477 ) ) ;
#52217 = EDGE_LOOP ( 'NONE', ( #68830, #56707, #33982, #65800 ) ) ;
#52218 = ORIENTED_EDGE ( 'NONE', *, *, #15902, .F. ) ;
#52219 = CARTESIAN_POINT ( 'NONE',  ( 110.2429982417149574, 29.99119854320845846, -77.76698815611739235 ) ) ;
#52220 = PLANE ( 'NONE',  #18805 ) ;
#52221 = CARTESIAN_POINT ( 'NONE',  ( 200.8410151090926377, 101.2014854111317561, -64.22370884727946816 ) ) ;
#52222 = CARTESIAN_POINT ( 'NONE',  ( -19.44450014243025748, 27.18813181980454274, 6.893342935626288970 ) ) ;
#52223 = CARTESIAN_POINT ( 'NONE',  ( -84.49322488516129681, 0.000000000000000000, 43.58025477438756212 ) ) ;
#52224 = FACE_OUTER_BOUND ( 'NONE', #36047, .T. ) ;
#52225 = CARTESIAN_POINT ( 'NONE',  ( 15.78827728214693416, 6.500811158483284835, -23.67439350822212774 ) ) ;
#52226 = CIRCLE ( 'NONE', #552, 24.99999999999985434 ) ;
#52227 = CARTESIAN_POINT ( 'NONE',  ( -49.44484229820456278, 14.28460989390479519, 42.82150934049000313 ) ) ;
#52228 = ORIENTED_EDGE ( 'NONE', *, *, #46685, .T. ) ;
#52229 = ORIENTED_EDGE ( 'NONE', *, *, #42110, .T. ) ;
#52230 = CARTESIAN_POINT ( 'NONE',  ( -109.6657532478350987, 37.84376708859254990, 9.843706301264420588 ) ) ;
#52231 = VECTOR ( 'NONE', #5246, 1000.000000000000000 ) ;
#52232 = DIRECTION ( 'NONE',  ( -4.270088556250601699E-16, -0.000000000000000000, -1.000000000000000000 ) ) ;
#52233 = CARTESIAN_POINT ( 'NONE',  ( 103.5744911984874221, 25.91722113382955683, 87.35084054165872658 ) ) ;
#52234 = CARTESIAN_POINT ( 'NONE',  ( 8.000000000000000000, 4.618802153517024500, -8.785468820183664818 ) ) ;
#52235 = AXIS2_PLACEMENT_3D ( 'NONE', #68333, #3961, #45478 ) ;
#52236 = AXIS2_PLACEMENT_3D ( 'NONE', #38582, #37537, #33326 ) ;
#52237 = CARTESIAN_POINT ( 'NONE',  ( 186.6118452967671999, 84.37814701615437230, -38.63095407981293761 ) ) ;
#52238 = CARTESIAN_POINT ( 'NONE',  ( 109.9975424824652634, 172.0000000000000284, 418.0000000000000568 ) ) ;
#52239 = DIRECTION ( 'NONE',  ( -1.000000000000000000, 0.000000000000000000, 0.000000000000000000 ) ) ;
#52240 = ORIENTED_EDGE ( 'NONE', *, *, #40894, .F. ) ;
#52241 = ORIENTED_EDGE ( 'NONE', *, *, #15120, .T. ) ;
#52242 = VECTOR ( 'NONE', #43536, 1000.000000000000000 ) ;
#52243 = ADVANCED_FACE ( 'NONE', ( #40128 ), #66189, .F. ) ;
#52244 = ORIENTED_EDGE ( 'NONE', *, *, #39014, .F. ) ;
#52245 = CARTESIAN_POINT ( 'NONE',  ( -149.9471644042847345, 65.87751327280743396, -22.95857820982234543 ) ) ;
#52246 = EDGE_CURVE ( 'NONE', #2801, #49554, #34520, .T. ) ;
#52247 = PLANE ( 'NONE',  #17281 ) ;
#52248 = CARTESIAN_POINT ( 'NONE',  ( 64.93495251696903381, 13.12601614965099373, -50.47501578450074078 ) ) ;
#52249 = CARTESIAN_POINT ( 'NONE',  ( 103.6901687706621118, 25.96661075370345984, -93.43913290534256078 ) ) ;
#52250 = EDGE_CURVE ( 'NONE', #53656, #29332, #67230, .T. ) ;
#52251 = CARTESIAN_POINT ( 'NONE',  ( -35.99414836699285303, 11.40630460607620833, -75.64038296020707719 ) ) ;
#52252 = CARTESIAN_POINT ( 'NONE',  ( -156.3790798118593273, 70.23422112803315542, -18.48537804305940924 ) ) ;
#52253 = DIRECTION ( 'NONE',  ( -1.000000000000000000, 0.000000000000000000, 0.000000000000000000 ) ) ;
#52254 = CARTESIAN_POINT ( 'NONE',  ( 8.288451200428832877, 6.376395059685424194, -15.68249724139179158 ) ) ;
#52255 = ORIENTED_EDGE ( 'NONE', *, *, #46307, .T. ) ;
#52256 = CARTESIAN_POINT ( 'NONE',  ( 22.28700331106867694, 7.803633676228380445, 14.42207042821974561 ) ) ;
#52257 = CARTESIAN_POINT ( 'NONE',  ( 188.5662303205147055, 86.51341602961785782, 64.25165609669510047 ) ) ;
#52258 = CARTESIAN_POINT ( 'NONE',  ( -118.8504142000305706, 42.02789424825282083, 13.86596505667573709 ) ) ;
#52259 = CARTESIAN_POINT ( 'NONE',  ( 63.50528314073024205, 12.78634332146812547, -62.56524142263340593 ) ) ;
#52260 = CARTESIAN_POINT ( 'NONE',  ( 10.55634918610406281, 15.55634918610400241, 2.000000000000000000 ) ) ;
#52261 = CARTESIAN_POINT ( 'NONE',  ( 15.78827728214693416, 7.507518794609588042, -23.67439350822212774 ) ) ;
#52262 = CARTESIAN_POINT ( 'NONE',  ( 199.3671895066314903, 99.30947926630331324, 58.25206002476129896 ) ) ;
#52263 = EDGE_CURVE ( 'NONE', #26979, #32844, #45046, .T. ) ;
#52264 = EDGE_LOOP ( 'NONE', ( #24963, #49223, #65007, #31853 ) ) ;
#52265 = CARTESIAN_POINT ( 'NONE',  ( 311.9975424824652350, 170.0000000000000284, 256.6193948016162381 ) ) ;
#52266 = APPLICATION_PROTOCOL_DEFINITION ( 'draft international standard', 'automotive_design', 1998, #3140 ) ;
#52267 = DIRECTION ( 'NONE',  ( 0.4338837391175525693, 0.9009688679024218105, 5.102127870520019688E-18 ) ) ;
#52268 = CARTESIAN_POINT ( 'NONE',  ( 429.8372781065087338, 395.0000000000042633, 96.05029585798436642 ) ) ;
#52269 = LINE ( 'NONE', #19924, #62683 ) ;
#52270 = CONTEXT_DEPENDENT_SHAPE_REPRESENTATION ( #40921, #43884 ) ;
#52271 = CARTESIAN_POINT ( 'NONE',  ( 0.000000000000000000, 0.000000000000000000, 43.58025477438756212 ) ) ;
#52272 = ORIENTED_EDGE ( 'NONE', *, *, #11992, .T. ) ;
#52273 = VERTEX_POINT ( 'NONE', #55963 ) ;
#52274 = CARTESIAN_POINT ( 'NONE',  ( -30.95355748062275936, 9.511738996772313826, -23.47264677473818395 ) ) ;
#52275 = CARTESIAN_POINT ( 'NONE',  ( 0.000000000000000000, 0.000000000000000000, -9.500000000000000000 ) ) ;
#52276 = VERTEX_POINT ( 'NONE', #49977 ) ;
#52277 = VECTOR ( 'NONE', #9139, 1000.000000000000000 ) ;
#52278 = CARTESIAN_POINT ( 'NONE',  ( 151.1900544856616762, 54.17358268150817224, 94.71353523477451120 ) ) ;
#52279 = ORIENTED_EDGE ( 'NONE', *, *, #18682, .F. ) ;
#52280 = CARTESIAN_POINT ( 'NONE',  ( 56.42997683260146857, -32.25922681454192542, 40.00000000000003553 ) ) ;
#52281 = CARTESIAN_POINT ( 'NONE',  ( 127.2397149628677369, 37.56999625068102233, 40.57849170101663816 ) ) ;
#52282 = AXIS2_PLACEMENT_3D ( 'NONE', #14939, #68742, #10689 ) ;
#52283 = CYLINDRICAL_SURFACE ( 'NONE', #65667, 65.36598343705435354 ) ;
#52284 = CARTESIAN_POINT ( 'NONE',  ( -94.78109144324893975, 29.13179392050637162, 37.73384696942510885 ) ) ;
#52285 = VECTOR ( 'NONE', #18515, 1000.000000000000000 ) ;
#52286 = DIRECTION ( 'NONE',  ( -0.000000000000000000, -0.000000000000000000, -1.000000000000000000 ) ) ;
#52288 = ORIENTED_EDGE ( 'NONE', *, *, #24565, .T. ) ;
#52287 = DIRECTION ( 'NONE',  ( 0.000000000000000000, 0.000000000000000000, -1.000000000000000000 ) ) ;
#52289 = AXIS2_PLACEMENT_3D ( 'NONE', #3820, #31256, #62913 ) ;
#52290 = DIRECTION ( 'NONE',  ( 0.7071067811865408004, -2.275957200481570908E-15, -0.7071067811865543451 ) ) ;
#52291 = AXIS2_PLACEMENT_3D ( 'NONE', #44425, #33545, #6790 ) ;
#52292 = ORIENTED_EDGE ( 'NONE', *, *, #27150, .F. ) ;
#52293 = VERTEX_POINT ( 'NONE', #7775 ) ;
#52294 = CARTESIAN_POINT ( 'NONE',  ( -123.6699087229882110, 45.04696784753415528, -22.73548513474139909 ) ) ;
#52295 = LINE ( 'NONE', #47689, #58292 ) ;
#52296 = CARTESIAN_POINT ( 'NONE',  ( -173.9548930713590948, 88.06040582145364226, -22.83265499627751893 ) ) ;
#52297 = B_SPLINE_CURVE_WITH_KNOTS ( 'NONE', 3,
 ( #29851, #19638, #62560, #14372 ),
 .UNSPECIFIED., .F., .F.,
 ( 4, 4 ),
 ( 0.1259919275528358917, 0.1829744153748748547 ),
 .UNSPECIFIED. ) ;
#52299 = EDGE_LOOP ( 'NONE', ( #68752, #4037, #37737, #48898 ) ) ;
#52298 = CARTESIAN_POINT ( 'NONE',  ( -131.6253556217204732, 51.61436399519948282, 60.10113730160578172 ) ) ;
#52300 = CARTESIAN_POINT ( 'NONE',  ( -109.7479544825926183, 37.88941408414071077, 92.47845238461742667 ) ) ;
#52301 = DIRECTION ( 'NONE',  ( -0.9195277725514544587, 0.3930250316539147803, 0.000000000000000000 ) ) ;
#52302 = ORIENTED_EDGE ( 'NONE', *, *, #58330, .T. ) ;
#52303 = EDGE_CURVE ( 'NONE', #16320, #32410, #56534, .T. ) ;
#52304 = CARTESIAN_POINT ( 'NONE',  ( -58.10608953386397957, 15.52134062643864532, -22.72640478715415568 ) ) ;
#52305 = CARTESIAN_POINT ( 'NONE',  ( -132.6092625803567842, 52.31125232006265691, -65.90852614572540347 ) ) ;
#52306 = LINE ( 'NONE', #26269, #19056 ) ;
#52307 = CARTESIAN_POINT ( 'NONE',  ( -128.9863978264385196, 49.78205252558956317, 18.11205277819082227 ) ) ;
#52308 = CARTESIAN_POINT ( 'NONE',  ( 66.94365390260637128, 14.65531706601758977, -76.45896609455289195 ) ) ;
#52309 = ORIENTED_EDGE ( 'NONE', *, *, #27368, .T. ) ;
#52310 = ORIENTED_EDGE ( 'NONE', *, *, #3981, .T. ) ;
#52311 = CARTESIAN_POINT ( 'NONE',  ( -142.3187766126154656, 59.59460822661994683, -17.67785402409575468 ) ) ;
#52312 = CARTESIAN_POINT ( 'NONE',  ( -166.3175803736862122, 79.86140754556167565, -39.04379056814254767 ) ) ;
#52313 = DIRECTION ( 'NONE',  ( 0.000000000000000000, 0.000000000000000000, 1.000000000000000000 ) ) ;
#52314 = LINE ( 'NONE', #41766, #8606 ) ;
#52315 = CARTESIAN_POINT ( 'NONE',  ( -71.42546113164833343, 20.75891408601218302, 39.93699313454726507 ) ) ;
#52316 = CYLINDRICAL_SURFACE ( 'NONE', #58453, 7.500000000000013323 ) ;
#52317 = CARTESIAN_POINT ( 'NONE',  ( 0.08224679563971232232, 6.145890662064651622, -5.355005115540898863 ) ) ;
#52318 = EDGE_CURVE ( 'NONE', #59777, #22589, #21270, .T. ) ;
#52319 = DIRECTION ( 'NONE',  ( -0.000000000000000000, 1.000000000000000000, -0.000000000000000000 ) ) ;
#52320 = CARTESIAN_POINT ( 'NONE',  ( -166.3188283541502415, 79.86268666707381669, -72.22739220925680570 ) ) ;
#52321 = EDGE_LOOP ( 'NONE', ( #9676, #22652, #44609, #57990 ) ) ;
#52322 = CARTESIAN_POINT ( 'NONE',  ( -106.6940984894958007, 35.07986071359380986, -21.75232707253212538 ) ) ;
#52323 = EDGE_CURVE ( 'NONE', #2893, #56182, #41856, .T. ) ;
#52324 = EDGE_LOOP ( 'NONE', ( #4359, #24857 ) ) ;
#52325 = VECTOR ( 'NONE', #29731, 1000.000000000000114 ) ;
#52326 = CARTESIAN_POINT ( 'NONE',  ( -38.26497993382596263, 10.81185389040528300, 13.98917590912293996 ) ) ;
#52327 = CARTESIAN_POINT ( 'NONE',  ( 81.74250361646211616, 18.86685472882137660, 69.76712954530790967 ) ) ;
#52328 = CARTESIAN_POINT ( 'NONE',  ( -84.62094424603726850, 24.67969995822045348, -91.73912349652042053 ) ) ;
#52329 = CARTESIAN_POINT ( 'NONE',  ( 23.93060502292685499, -7.646171227524485303, 3.061616997868437868E-16 ) ) ;
#52330 = CARTESIAN_POINT ( 'NONE',  ( 33.31166872005965729, 8.707041209322239794, 6.185351823203305344 ) ) ;
#52332 = FACE_OUTER_BOUND ( 'NONE', #63013, .T. ) ;
#52331 = VECTOR ( 'NONE', #24499, 999.9999999999998863 ) ;
#52333 = CYLINDRICAL_SURFACE ( 'NONE', #52482, 4.999999999999997335 ) ;
#52334 = DIRECTION ( 'NONE',  ( -1.001915251000354105E-14, 1.000000000000000000, -5.551115123125782702E-17 ) ) ;
#52335 = ADVANCED_FACE ( 'NONE', ( #68913 ), #26368, .F. ) ;
#52336 = CARTESIAN_POINT ( 'NONE',  ( -38.87871322265799279, 11.95691939779334234, -14.99132105584396513 ) ) ;
#52337 = AXIS2_PLACEMENT_3D ( 'NONE', #16350, #32877, #27593 ) ;
#52338 = VERTEX_POINT ( 'NONE', #30614 ) ;
#52339 = CARTESIAN_POINT ( 'NONE',  ( -9.964117946889913924, 64.24592483216710548, 0.000000000000000000 ) ) ;
#52340 = ORIENTED_EDGE ( 'NONE', *, *, #66483, .F. ) ;
#52341 = PRODUCT_DEFINITION_FORMATION_WITH_SPECIFIED_SOURCE ( 'ANY', '', #6321, .NOT_KNOWN. ) ;
#52342 = LINE ( 'NONE', #24243, #57579 ) ;
#52343 = CARTESIAN_POINT ( 'NONE',  ( 8.679939806240511757, 7.383357464882124077, -67.45892186114495814 ) ) ;
#52344 = CARTESIAN_POINT ( 'NONE',  ( -189.2826425734428994, 107.1493800926106132, 12.45157081075467609 ) ) ;
#52345 = LINE ( 'NONE', #58639, #10891 ) ;
#52346 = AXIS2_PLACEMENT_3D ( 'NONE', #19005, #24644, #35182 ) ;
#52347 = DIRECTION ( 'NONE',  ( -0.000000000000000000, -0.000000000000000000, -1.000000000000000000 ) ) ;
#52348 = FACE_BOUND ( 'NONE', #44012, .T. ) ;
#52349 = CARTESIAN_POINT ( 'NONE',  ( 150.5538013146980347, 53.70974888488128585, -40.71184894097334706 ) ) ;
#52350 = VECTOR ( 'NONE', #40546, 1000.000000000000000 ) ;
#52351 = EDGE_CURVE ( 'NONE', #3906, #3129, #48496, .T. ) ;
#52352 = VERTEX_POINT ( 'NONE', #69268 ) ;
#52353 = DIRECTION ( 'NONE',  ( 9.950807539071958118E-15, -1.000000000000000000, -4.024558464266191670E-15 ) ) ;
#52354 = CARTESIAN_POINT ( 'NONE',  ( -156.8728827992623849, 72.05711009495561825, 63.62291505455890217 ) ) ;
#52356 = EDGE_CURVE ( 'NONE', #37187, #44519, #66530, .T. ) ;
#52355 = CARTESIAN_POINT ( 'NONE',  ( 181.0840389613909451, 80.03940679743416808, -9.380507075415923879 ) ) ;
#52357 = EDGE_CURVE ( 'NONE', #5511, #20487, #30270, .T. ) ;
#52358 = DIRECTION ( 'NONE',  ( -1.000000000000000000, 0.000000000000000000, 0.000000000000000000 ) ) ;
#52359 = CARTESIAN_POINT ( 'NONE',  ( -125.8938041572051389, 47.69968343338778283, -49.91370389823397602 ) ) ;
#52360 = VERTEX_POINT ( 'NONE', #5585 ) ;
#52361 = CARTESIAN_POINT ( 'NONE',  ( -176.3856149167965555, 92.38076834121982017, -62.29001654799212417 ) ) ;
#52362 = CARTESIAN_POINT ( 'NONE',  ( 93.71772995179816235, 21.96265635001558536, 66.51989931170464843 ) ) ;
#52363 = CARTESIAN_POINT ( 'NONE',  ( 203.9228889538744625, 106.9879579748728418, -24.45170175305141314 ) ) ;
#52364 = CARTESIAN_POINT ( 'NONE',  ( 110.2429982417149290, 28.88204397445231209, -24.07788697519002596 ) ) ;
#52365 = CARTESIAN_POINT ( 'NONE',  ( -119.5267374018686724, 42.44190186039716650, -65.26197758995584763 ) ) ;
#52366 = ORIENTED_EDGE ( 'NONE', *, *, #53660, .T. ) ;
#52367 = CARTESIAN_POINT ( 'NONE',  ( 200.8298320869470501, 101.1869877914233484, 30.26769475748699989 ) ) ;
#52368 = CARTESIAN_POINT ( 'NONE',  ( 112.7784411285248751, 30.07270878825233851, -77.32934762718066679 ) ) ;
#52369 = CARTESIAN_POINT ( 'NONE',  ( 186.2575601542430661, 85.47765906955505955, 42.24398978463538157 ) ) ;
#52370 = CARTESIAN_POINT ( 'NONE',  ( 157.4703587214989398, 58.92748579479258808, 17.56491688178971700 ) ) ;
#52371 = LINE ( 'NONE', #18632, #38633 ) ;
#52372 = ORIENTED_EDGE ( 'NONE', *, *, #67996, .F. ) ;
#52373 = DIRECTION ( 'NONE',  ( 1.000000000000000000, 0.000000000000000000, 0.000000000000000000 ) ) ;
#52374 = ORIENTED_EDGE ( 'NONE', *, *, #21208, .F. ) ;
#52375 = AXIS2_PLACEMENT_3D ( 'NONE', #27553, #48995, #37413 ) ;
#52376 = CARTESIAN_POINT ( 'NONE',  ( -107.7743374187916885, 35.66028478413599601, -37.38574911014553948 ) ) ;
#52377 = CARTESIAN_POINT ( 'NONE',  ( 447.3372781065083927, 395.0000000000043769, 83.55029585798381220 ) ) ;
#52378 = DIRECTION ( 'NONE',  ( -0.000000000000000000, -1.000000000000000000, -0.000000000000000000 ) ) ;
#52379 = VECTOR ( 'NONE', #35213, 1000.000000000000000 ) ;
#52381 = ORIENTED_EDGE ( 'NONE', *, *, #47480, .F. ) ;
#52380 = DIRECTION ( 'NONE',  ( -0.000000000000000000, 0.000000000000000000, 1.000000000000000000 ) ) ;
#52382 = CARTESIAN_POINT ( 'NONE',  ( -180.5231752320737257, 95.76423526868921954, 39.56937748859167669 ) ) ;
#52383 = FACE_OUTER_BOUND ( 'NONE', #45683, .T. ) ;
#52384 = CARTESIAN_POINT ( 'NONE',  ( 116.9197133427646804, 33.22079464767577406, -46.87639412244661941 ) ) ;
#52385 = AXIS2_PLACEMENT_3D ( 'NONE', #30910, #10131, #52687 ) ;
#52386 = ORIENTED_EDGE ( 'NONE', *, *, #68391, .T. ) ;
#52387 = EDGE_CURVE ( 'NONE', #51881, #26997, #5829, .T. ) ;
#52388 = CARTESIAN_POINT ( 'NONE',  ( 126.8114659053431694, 38.48351437375816886, 61.23194205192785944 ) ) ;
#52389 = PLANE ( 'NONE',  #46818 ) ;
#52390 = EDGE_CURVE ( 'NONE', #8516, #45779, #38647, .T. ) ;
#52391 = DIRECTION ( 'NONE',  ( -7.703719777548943412E-34, 1.479221584281240009E-31, -1.000000000000000000 ) ) ;
#52392 = CONICAL_SURFACE ( 'NONE', #45673, 63.58578643762691485, 0.7853981633974497223 ) ;
#52393 = ORIENTED_EDGE ( 'NONE', *, *, #55773, .T. ) ;
#52394 = DIRECTION ( 'NONE',  ( 0.000000000000000000, 0.000000000000000000, -1.000000000000000000 ) ) ;
#52395 = CARTESIAN_POINT ( 'NONE',  ( -173.1211646369891355, 87.12891641440857882, 30.82169460664101734 ) ) ;
#52396 = CARTESIAN_POINT ( 'NONE',  ( -33.36721086971961370, 9.915747831546608992, -62.40970415560823170 ) ) ;
#52397 = CARTESIAN_POINT ( 'NONE',  ( 90.30732934992394689, 21.77797012484621320, 43.76604365556254095 ) ) ;
#52398 = ORIENTED_EDGE ( 'NONE', *, *, #68753, .T. ) ;
#52399 = CARTESIAN_POINT ( 'NONE',  ( 49.76301652092226391, -41.81676920493045202, 170.0000000000000000 ) ) ;
#52400 = ORIENTED_EDGE ( 'NONE', *, *, #51957, .T. ) ;
#52401 = CARTESIAN_POINT ( 'NONE',  ( 152.8672128926848188, 55.41186463791522954, -22.70565529590070497 ) ) ;
#52402 = CARTESIAN_POINT ( 'NONE',  ( -62.13370439300283721, 16.69510293645669563, 89.01348188984179899 ) ) ;
#52403 = CARTESIAN_POINT ( 'NONE',  ( 105.4376736768159475, 27.81988511842610023, 31.34766073213387472 ) ) ;
#52404 = B_SPLINE_CURVE_WITH_KNOTS ( 'NONE', 3,
 ( #16559, #46942, #3679, #25157, #59112, #38015, #68067, #52216, #59460, #51536, #68403, #20207, #62433, #5647, #19870, #3342, #14584, #36044, #42931, #57500, #41663, #37665, #30771, #57843, #4034, #53487, #27, #21482, #10929, #32402, #27106, #48541, #376, #43278, #6703, #44693, #23590, #33791, #45028, #60517, #55230, #65100, #60859, #49956 ),
 .UNSPECIFIED., .F., .F.,
 ( 4, 2, 2, 2, 2, 2, 2, 2, 2, 2, 2, 2, 2, 2, 2, 2, 2, 2, 2, 2, 2, 4 ),
 ( 0.000000000000000000, 0.001487235713946824349, 0.002230853570920217441, 0.002974471427893610534, 0.004461707141840360290, 0.005948942855787110046, 0.007436178569733859801, 0.008179796426707235113, 0.008923414283680609557, 0.01041064999762737579, 0.01189788571157414203, 0.01264150356854752515, 0.01338512142552090653, 0.01487235713946766583, 0.01561597499644105068, 0.01635959285341443553, 0.01784682856736120871, 0.01933406428130798535, 0.02007768213828137194, 0.02082129999525475159, 0.02230853570920152129, 0.02379577142314828753 ),
 .UNSPECIFIED. ) ;
#52405 = CARTESIAN_POINT ( 'NONE',  ( -1.862553927312063040, 7.582910205528084369, 33.04026090934276993 ) ) ;
#52406 = LINE ( 'NONE', #52062, #12376 ) ;
#52407 = CARTESIAN_POINT ( 'NONE',  ( 184.5867277229703802, 83.68414666546580349, 16.59965183973755387 ) ) ;
#52408 = EDGE_CURVE ( 'NONE', #65008, #49164, #10517, .T. ) ;
#52409 = CARTESIAN_POINT ( 'NONE',  ( 212.1700216741373310, 117.1889356120870929, -44.55361903701415116 ) ) ;
#52410 = CARTESIAN_POINT ( 'NONE',  ( 181.0840389613909736, 78.60582251573003987, 2.464043515047718458 ) ) ;
#52411 = EDGE_CURVE ( 'NONE', #32718, #4563, #31986, .T. ) ;
#52412 = EDGE_LOOP ( 'NONE', ( #25334, #60504, #24914, #39337 ) ) ;
#52413 = CARTESIAN_POINT ( 'NONE',  ( 49.99999999999998579, -19.99999999999996447, 1.999999999999984457 ) ) ;
#52414 = VERTEX_POINT ( 'NONE', #11206 ) ;
#52415 = CARTESIAN_POINT ( 'NONE',  ( -72.35078170365748917, 21.08176362823952843, 60.71011165796286235 ) ) ;
#52416 = EDGE_CURVE ( 'NONE', #39147, #49450, #32674, .T. ) ;
#52417 = CARTESIAN_POINT ( 'NONE',  ( 55.90536342106781120, 11.13510150712953184, -72.50233492501236299 ) ) ;
#52418 = CYLINDRICAL_SURFACE ( 'NONE', #57485, 5.000000000000000888 ) ;
#52419 = PLANE ( 'NONE',  #35626 ) ;
#52420 = CARTESIAN_POINT ( 'NONE',  ( 19.54452863209719382, 7.657034792877146501, 44.02475270524415407 ) ) ;
#52421 = DIRECTION ( 'NONE',  ( -0.000000000000000000, -1.000000000000000000, -0.000000000000000000 ) ) ;
#52422 = ORIENTED_EDGE ( 'NONE', *, *, #58661, .F. ) ;
#52423 = CARTESIAN_POINT ( 'NONE',  ( 9.133089864015637716, 32.15384528989822854, 6.893342932533050416 ) ) ;
#52424 = DIRECTION ( 'NONE',  ( 0.000000000000000000, 0.000000000000000000, -1.000000000000000000 ) ) ;
#52425 = VERTEX_POINT ( 'NONE', #43207 ) ;
#52426 = VERTEX_POINT ( 'NONE', #33386 ) ;
#52427 = CARTESIAN_POINT ( 'NONE',  ( -151.2410113808308552, 65.66338888995507261, 30.91080334718760980 ) ) ;
#52428 = CARTESIAN_POINT ( 'NONE',  ( 62.04664474957770182, 12.44961624115901877, -35.76790967155817924 ) ) ;
#52429 = CARTESIAN_POINT ( 'NONE',  ( 5.799999999999999822, 0.000000000000000000, 0.000000000000000000 ) ) ;
#52430 = AXIS2_PLACEMENT_3D ( 'NONE', #25442, #51811, #56129 ) ;
#52431 = CARTESIAN_POINT ( 'NONE',  ( 24.39800339187929978, -60.26242556095670722, 41.38025477438755928 ) ) ;
#52432 = LINE ( 'NONE', #42221, #48740 ) ;
#52433 = VECTOR ( 'NONE', #28736, 1000.000000000000000 ) ;
#52434 = ORIENTED_EDGE ( 'NONE', *, *, #60180, .F. ) ;
#52435 = ADVANCED_FACE ( 'NONE', ( #54098 ), #6635, .F. ) ;
#52436 = EDGE_CURVE ( 'NONE', #20959, #20719, #20409, .T. ) ;
#52437 = CARTESIAN_POINT ( 'NONE',  ( -126.3453033442920344, 47.99870040347946087, 30.61994787315706645 ) ) ;
#52438 = VERTEX_POINT ( 'NONE', #37596 ) ;
#52439 = CARTESIAN_POINT ( 'NONE',  ( 210.5178985598939505, 114.6803933586780317, 14.59982085240562988 ) ) ;
#52440 = CARTESIAN_POINT ( 'NONE',  ( 9.819093282782489496, 7.389085782749408970, 68.92638477701862598 ) ) ;
#52441 = CARTESIAN_POINT ( 'NONE',  ( 210.6741002223296846, 114.9147155784838077, 41.24653036116778537 ) ) ;
#52442 = FACE_BOUND ( 'NONE', #33838, .T. ) ;
#52443 = EDGE_CURVE ( 'NONE', #57527, #11698, #29409, .T. ) ;
#52444 = AXIS2_PLACEMENT_3D ( 'NONE', #14061, #24977, #51011 ) ;
#52445 = VERTEX_POINT ( 'NONE', #33021 ) ;
#52446 = EDGE_LOOP ( 'NONE', ( #68569, #9919, #25171, #47490 ) ) ;
#52447 = CARTESIAN_POINT ( 'NONE',  ( 113.7689755057786272, -21.75207715352313542, 3.301879156304019070 ) ) ;
#52448 = CARTESIAN_POINT ( 'NONE',  ( -122.1036342099435501, 45.23906970976855746, 85.31054657959678877 ) ) ;
#52449 = CARTESIAN_POINT ( 'NONE',  ( -168.7187482717113767, 82.35796501763486788, -21.45773980473016351 ) ) ;
#52450 = CARTESIAN_POINT ( 'NONE',  ( 57.84269237198510893, 33.10328505625795970, 34.48241795236666007 ) ) ;
#52451 = CARTESIAN_POINT ( 'NONE',  ( 63.01563776193091826, 12.67277567978498176, 29.81296093922127710 ) ) ;
#52452 = DIRECTION ( 'NONE',  ( 0.000000000000000000, 1.000000000000000000, 0.000000000000000000 ) ) ;
#52453 = ORIENTED_EDGE ( 'NONE', *, *, #38908, .T. ) ;
#52454 = FACE_OUTER_BOUND ( 'NONE', #41502, .T. ) ;
#52455 = CARTESIAN_POINT ( 'NONE',  ( -101.3602137809054540, 32.31558061113913283, 57.40576275019232355 ) ) ;
#52456 = VERTEX_POINT ( 'NONE', #54453 ) ;
#52457 = CARTESIAN_POINT ( 'NONE',  ( -84.97622048504842951, 24.82614411847757907, 7.011873618776862216 ) ) ;
#52458 = ORIENTED_EDGE ( 'NONE', *, *, #17307, .T. ) ;
#52459 = DIRECTION ( 'NONE',  ( -1.000000000000000000, 0.000000000000000000, 0.000000000000000000 ) ) ;
#52460 = VERTEX_POINT ( 'NONE', #58699 ) ;
#52461 = ORIENTED_EDGE ( 'NONE', *, *, #17533, .F. ) ;
#52462 = CARTESIAN_POINT ( 'NONE',  ( -120.6739978760426197, 44.33795494230366785, 16.66634037272415014 ) ) ;
#52463 = CARTESIAN_POINT ( 'NONE',  ( -178.5790738944854468, 93.41591512785086593, 70.31590409971879296 ) ) ;
#52464 = CARTESIAN_POINT ( 'NONE',  ( 126.6395826915640299, 37.23416510613626684, 61.79751572699002793 ) ) ;
#52465 = VERTEX_POINT ( 'NONE', #53417 ) ;
#52466 = VECTOR ( 'NONE', #42820, 1000.000000000000000 ) ;
#52467 = CARTESIAN_POINT ( 'NONE',  ( -38.55722845454012315, 10.86859975449739402, 89.02085468374171739 ) ) ;
#52468 = VECTOR ( 'NONE', #27315, 1000.000000000000000 ) ;
#52469 = ADVANCED_FACE ( 'NONE', ( #53764 ), #32860, .T. ) ;
#52470 = CARTESIAN_POINT ( 'NONE',  ( 174.6242782760050147, 73.69713439533578025, -66.74970077171313676 ) ) ;
#52471 = LINE ( 'NONE', #67625, #24676 ) ;
#52472 = CARTESIAN_POINT ( 'NONE',  ( 209.3223706822284100, 0.000000000000000000, 31.44247402469554942 ) ) ;
#52473 = CARTESIAN_POINT ( 'NONE',  ( 79.18180043629686793, 18.06526831600445959, -44.34015328538779954 ) ) ;
#52474 = CARTESIAN_POINT ( 'NONE',  ( 0.000000000000000000, 0.000000000000000000, 0.000000000000000000 ) ) ;
#52475 = ORIENTED_EDGE ( 'NONE', *, *, #24778, .T. ) ;
#52476 = DIRECTION ( 'NONE',  ( 0.000000000000000000, 0.000000000000000000, -1.000000000000000000 ) ) ;
#52477 = CARTESIAN_POINT ( 'NONE',  ( 39.89571693415785347, 8.473773298340393723, 18.06928371549960133 ) ) ;
#52478 = CARTESIAN_POINT ( 'NONE',  ( 177.0027897064244655, 75.97676392242546228, 16.27253295564755931 ) ) ;
#52479 = B_SPLINE_CURVE_WITH_KNOTS ( 'NONE', 3,
 ( #49322, #60241, #28221, #44408, #101, #48613, #1153, #33864, #44049, #21557, #453, #43002, #16288, #37740, #59183, #21907, #808, #8525, #39481, #45451, #8170, #50393, #24004, #7490, #13789, #18725, #18033, #55306, #61290, #60937, #44767, #13112, #40183, #34577, #45099, #28942, #34912, #56018, #23659, #61967, #7126, #56350, #12757, #45804, #24360 ),
 .UNSPECIFIED., .F., .F.,
 ( 4, 2, 2, 2, 2, 2, 2, 2, 2, 2, 2, 1, 2, 2, 2, 2, 2, 2, 2, 2, 2, 2, 4 ),
 ( 0.000000000000000000, 0.001510509505235982548, 0.002265764257853956475, 0.003021019010471930402, 0.004531528515707878256, 0.005286783268325870831, 0.006042038020943863406, 0.007552547526179844220, 0.009063057031415825901, 0.01057356653665180758, 0.01132882128926979842, 0.01208407604188778753, 0.01283933079450577837, 0.01359458554712377094, 0.01510509505235972140, 0.01586034980497767755, 0.01661560455759563543, 0.01812611406283149221, 0.01963662356806735246, 0.02039187832068526524, 0.02114713307330317801, 0.02265764257853904520, 0.02416815208377490545 ),
 .UNSPECIFIED. ) ;
#52480 = CARTESIAN_POINT ( 'NONE',  ( 13.24564585880136036, -63.65041531508826012, 170.0000000000000000 ) ) ;
#52481 = DIRECTION ( 'NONE',  ( 0.000000000000000000, 0.000000000000000000, 1.000000000000000000 ) ) ;
#52482 = AXIS2_PLACEMENT_3D ( 'NONE', #47055, #20319, #63238 ) ;
#52483 = CARTESIAN_POINT ( 'NONE',  ( 129.1137093889808511, 38.63348691920623423, 4.350904459445209760 ) ) ;
#52484 = CARTESIAN_POINT ( 'NONE',  ( 32.22469126021599095, 7.584221829288119388, -94.59231775885801596 ) ) ;
#52485 = EDGE_CURVE ( 'NONE', #36200, #60290, #666, .T. ) ;
#52486 = CARTESIAN_POINT ( 'NONE',  ( -120.1650841064594033, 44.02024060322520427, -64.41117799840883151 ) ) ;
#52487 = CARTESIAN_POINT ( 'NONE',  ( 211.7318474105134385, 118.3631723164074145, 34.08830694803145178 ) ) ;
#52488 = CARTESIAN_POINT ( 'NONE',  ( -102.2801239173131052, 33.91021738430207222, 18.67452391595144334 ) ) ;
#52489 = CARTESIAN_POINT ( 'NONE',  ( -107.7743374187916885, 35.66028478413599601, 43.14790266124550300 ) ) ;
#52490 = EDGE_LOOP ( 'NONE', ( #52507, #64571, #52161, #7029 ) ) ;
#52491 = AXIS2_PLACEMENT_3D ( 'NONE', #41668, #30425, #51874 ) ;
#52492 = CARTESIAN_POINT ( 'NONE',  ( -47.70992047900629274, 13.86859651505968039, 89.94426166759667751 ) ) ;
#52493 = VERTEX_POINT ( 'NONE', #59047 ) ;
#52494 = EDGE_CURVE ( 'NONE', #31358, #54401, #1983, .T. ) ;
#52495 = FACE_OUTER_BOUND ( 'NONE', #29244, .T. ) ;
#52496 = ORIENTED_EDGE ( 'NONE', *, *, #62047, .T. ) ;
#52497 = EDGE_CURVE ( 'NONE', #16199, #34775, #30615, .T. ) ;
#52498 = CARTESIAN_POINT ( 'NONE',  ( 19.11382977197791533, 7.636807742668409560, -63.12314672599089960 ) ) ;
#52499 = CARTESIAN_POINT ( 'NONE',  ( 107.3013380801408658, 400.0000000000066507, -128.9497041420121093 ) ) ;
#52500 = CARTESIAN_POINT ( 'NONE',  ( -146.7404675333698663, 63.17262273741978618, 72.03985599882574320 ) ) ;
#52501 = CARTESIAN_POINT ( 'NONE',  ( -34.96012151086515019, 55.23134702900888016, 41.38025477438755928 ) ) ;
#52502 = CARTESIAN_POINT ( 'NONE',  ( 134.0849965622593913, 42.73957449886184889, -51.02331093239570947 ) ) ;
#52503 = CARTESIAN_POINT ( 'NONE',  ( -30.95341298663140961, 10.53108683215056196, 3.371903815725489473 ) ) ;
#52504 = CARTESIAN_POINT ( 'NONE',  ( 2.999999999999993339, 20.30000000000000071, 0.000000000000000000 ) ) ;
#52505 = CARTESIAN_POINT ( 'NONE',  ( -15.55634918610408945, -26.11269837220804035, 0.000000000000000000 ) ) ;
#52506 = CARTESIAN_POINT ( 'NONE',  ( -28.30427060690011132, -69.40159203110334829, 41.38025477438755928 ) ) ;
#52507 = ORIENTED_EDGE ( 'NONE', *, *, #63069, .F. ) ;
#52508 = ORIENTED_EDGE ( 'NONE', *, *, #10795, .F. ) ;
#52509 = CARTESIAN_POINT ( 'NONE',  ( 184.8109923074100607, 83.92257297578457553, 83.98258588058325813 ) ) ;
#52510 = CARTESIAN_POINT ( 'NONE',  ( 129.2375969008351717, 39.86537432630840527, -91.29033810975268182 ) ) ;
#52511 = CARTESIAN_POINT ( 'NONE',  ( 67.23580198090078852, 14.72857320832442696, -90.69627056048217639 ) ) ;
#52512 = EDGE_CURVE ( 'NONE', #58381, #7619, #58659, .T. ) ;
#52513 = CARTESIAN_POINT ( 'NONE',  ( 46.23304607317102466, 10.41544405387738514, -73.07032476065955962 ) ) ;
#52514 = CARTESIAN_POINT ( 'NONE',  ( 41.26323044930809658, 6.217756198492188524, 13.79046340968177908 ) ) ;
#52515 = CARTESIAN_POINT ( 'NONE',  ( 208.9585401441656529, 114.1617785893844399, 16.05179355318660583 ) ) ;
#52516 = VECTOR ( 'NONE', #40163, 1000.000000000000114 ) ;
#52517 = CARTESIAN_POINT ( 'NONE',  ( 181.0840389613909736, 78.60582251573003987, -24.38050707541595230 ) ) ;
#52518 = DIRECTION ( 'NONE',  ( 0.5000000000000014433, 0.8660254037844379305, -0.000000000000000000 ) ) ;
#52519 = CARTESIAN_POINT ( 'NONE',  ( -172.7116702014379541, 86.67317892691256986, 18.97714401617737323 ) ) ;
#52520 = CARTESIAN_POINT ( 'NONE',  ( 0.000000000000000000, 0.000000000000000000, 170.0000000000000000 ) ) ;
#52521 = ADVANCED_FACE ( 'NONE', ( #2755, #23522 ), #60790, .T. ) ;
#52522 = CARTESIAN_POINT ( 'NONE',  ( 31.11269837220800127, -31.11269837220812562, 85.00100000000000477 ) ) ;
#52523 = VECTOR ( 'NONE', #12722, 1000.000000000000000 ) ;
#52524 = ORIENTED_EDGE ( 'NONE', *, *, #14434, .F. ) ;
#52525 = CIRCLE ( 'NONE', #22193, 299.9999999999999432 ) ;
#52526 = CARTESIAN_POINT ( 'NONE',  ( 128.4157044224114088, 39.39296260757092227, 4.980963091233736151 ) ) ;
#52527 = CARTESIAN_POINT ( 'NONE',  ( 24.39800339187933176, -60.26242556095669300, 170.0000000000000000 ) ) ;
#52528 = CARTESIAN_POINT ( 'NONE',  ( -54.08816720029308556, 15.46531105893042302, 72.11509934368264396 ) ) ;
#52529 = DIRECTION ( 'NONE',  ( 0.000000000000000000, 0.000000000000000000, 1.000000000000000000 ) ) ;
#52530 = CARTESIAN_POINT ( 'NONE',  ( -48.56549579811110817, 13.03742088415616074, -38.92047726962127996 ) ) ;
#52531 = DIRECTION ( 'NONE',  ( 0.000000000000000000, -1.000000000000000000, 0.000000000000000000 ) ) ;
#52532 = EDGE_LOOP ( 'NONE', ( #726, #5084, #60319, #58229, #3167, #14647, #28090 ) ) ;
#52533 = CARTESIAN_POINT ( 'NONE',  ( 15.78827728214693416, -170.0000000000000000, -16.17439350822211352 ) ) ;
#52534 = CARTESIAN_POINT ( 'NONE',  ( -59.56523643198713813, 15.93788386494078146, 70.65753556899086618 ) ) ;
#52535 = ORIENTED_EDGE ( 'NONE', *, *, #25969, .T. ) ;
#52536 = AXIS2_PLACEMENT_3D ( 'NONE', #1621, #54727, #6554 ) ;
#52537 = ORIENTED_EDGE ( 'NONE', *, *, #18804, .F. ) ;
#52538 = CARTESIAN_POINT ( 'NONE',  ( 41.99370981210045528, 9.776766948428255333, 84.05726211029711692 ) ) ;
#52539 = CARTESIAN_POINT ( 'NONE',  ( -176.3896317155480347, 90.84057090619018027, -75.82101722059705651 ) ) ;
#52540 = CARTESIAN_POINT ( 'NONE',  ( 0.000000000000000000, 190.0000000000000000, 380.0000000000000000 ) ) ;
#52541 = VERTEX_POINT ( 'NONE', #2069 ) ;
#52542 = LINE ( 'NONE', #31439, #23278 ) ;
#52543 = CARTESIAN_POINT ( 'NONE',  ( 0.000000000000000000, 0.000000000000000000, 0.000000000000000000 ) ) ;
#52544 = CARTESIAN_POINT ( 'NONE',  ( -0.5658006089934857208, 7.533733779014708531, 8.824489085581655345 ) ) ;
#52545 = CARTESIAN_POINT ( 'NONE',  ( 157.4703587214989113, 58.92748579479260229, 44.40946747225338953 ) ) ;
#52546 = CARTESIAN_POINT ( 'NONE',  ( 162.3437785836964053, 61.54175036639340135, 84.88835865730561636 ) ) ;
#52547 = CARTESIAN_POINT ( 'NONE',  ( 94.02921784728459897, 22.08005910033065788, 38.45896049467276612 ) ) ;
#52548 = EDGE_CURVE ( 'NONE', #35180, #1235, #24218, .T. ) ;
#52549 = VERTEX_POINT ( 'NONE', #33728 ) ;
#52550 = CARTESIAN_POINT ( 'NONE',  ( 26.11269837220803325, -10.55634918610409656, 2.000000000000001776 ) ) ;
#52551 = EDGE_CURVE ( 'NONE', #2737, #41122, #39347, .T. ) ;
#52552 = LINE ( 'NONE', #57494, #57248 ) ;
#52553 = CARTESIAN_POINT ( 'NONE',  ( -29.04400972079232801, 10.22852224114065400, 44.82796049359348700 ) ) ;
#52554 = CARTESIAN_POINT ( 'NONE',  ( 197.8598785550297521, 99.02620879292953759, 33.61171724563484986 ) ) ;
#52555 = CARTESIAN_POINT ( 'NONE',  ( -75.70982523951138887, 22.28913922295978267, 84.70770602012026984 ) ) ;
#52557 = ORIENTED_EDGE ( 'NONE', *, *, #52387, .F. ) ;
#52556 = CARTESIAN_POINT ( 'NONE',  ( 0.000000000000000000, 0.000000000000000000, 0.000000000000000000 ) ) ;
#52558 = VERTEX_POINT ( 'NONE', #56210 ) ;
#52559 = VERTEX_POINT ( 'NONE', #45309 ) ;
#52560 = PRESENTATION_STYLE_ASSIGNMENT (( #46945 ) ) ;
#52561 = VECTOR ( 'NONE', #61110, 1000.000000000000000 ) ;
#52562 = DIRECTION ( 'NONE',  ( 0.000000000000000000, 0.000000000000000000, -1.000000000000000000 ) ) ;
#52563 = CARTESIAN_POINT ( 'NONE',  ( 201.9869293910475676, 102.6997661182767274, -63.66579325029184133 ) ) ;
#52564 = LINE ( 'NONE', #4388, #43994 ) ;
#52565 = CARTESIAN_POINT ( 'NONE',  ( -118.6157340058429668, 41.88485941274767299, 66.79490357616732865 ) ) ;
#52566 = VECTOR ( 'NONE', #4665, 1000.000000000000000 ) ;
#52567 = CARTESIAN_POINT ( 'NONE',  ( -82.33596576276354995, 24.83688096733768447, -9.211860750952368448 ) ) ;
#52568 = CARTESIAN_POINT ( 'NONE',  ( -39.29440389294403246, -17.09499999999999886, 0.000000000000000000 ) ) ;
#52569 = CARTESIAN_POINT ( 'NONE',  ( -156.3790798118593273, 70.23422112803314121, -45.32992863352309598 ) ) ;
#52570 = ORIENTED_EDGE ( 'NONE', *, *, #20170, .T. ) ;
#52571 = EDGE_CURVE ( 'NONE', #26997, #68407, #1088, .T. ) ;
#52572 = ORIENTED_EDGE ( 'NONE', *, *, #43023, .T. ) ;
#52573 = B_SPLINE_CURVE_WITH_KNOTS ( 'NONE', 3,
 ( #9137, #52043, #63293, #3859, #15104, #11529 ),
 .UNSPECIFIED., .F., .F.,
 ( 4, 2, 4 ),
 ( 0.03218939915585350420, 0.06469836417558690045, 0.09720732919532029670 ),
 .UNSPECIFIED. ) ;
#52574 = VECTOR ( 'NONE', #22331, 1000.000000000000000 ) ;
#52575 = EDGE_CURVE ( 'NONE', #12492, #4891, #44259, .T. ) ;
#52576 = CARTESIAN_POINT ( 'NONE',  ( -20.55634918610408945, -26.11269837220804035, 2.000000000000001776 ) ) ;
#52577 = FACE_OUTER_BOUND ( 'NONE', #24366, .T. ) ;
#52578 = CARTESIAN_POINT ( 'NONE',  ( 111.5744020652610118, 29.50263541599086992, 83.41251877751304278 ) ) ;
#52579 = CARTESIAN_POINT ( 'NONE',  ( 115.0485321076020568, 32.28990710985443968, -10.79877544804474354 ) ) ;
#52580 = AXIS2_PLACEMENT_3D ( 'NONE', #64150, #10336, #32148 ) ;
#52581 = DIRECTION ( 'NONE',  ( -0.000000000000000000, -0.000000000000000000, -1.000000000000000000 ) ) ;
#52582 = DIRECTION ( 'NONE',  ( 0.000000000000000000, 6.123233995736762338E-17, -1.000000000000000000 ) ) ;
#52583 = ORIENTED_EDGE ( 'NONE', *, *, #53979, .T. ) ;
#52584 = VERTEX_POINT ( 'NONE', #7692 ) ;
#52585 = EDGE_LOOP ( 'NONE', ( #52475, #55422, #22007, #9519 ) ) ;
#52586 = VECTOR ( 'NONE', #28712, 1000.000000000000000 ) ;
#52587 = DIRECTION ( 'NONE',  ( -1.387778780781445429E-16, 1.000000000000000000, 3.081487911019577365E-33 ) ) ;
#52588 = CARTESIAN_POINT ( 'NONE',  ( 76.57571471437145760, 6.000000000000000000, -20.00000000000000000 ) ) ;
#52589 = FACE_OUTER_BOUND ( 'NONE', #32598, .T. ) ;
#52590 = CARTESIAN_POINT ( 'NONE',  ( -38.54237244144231056, 11.89088379031760567, -67.24215503103580716 ) ) ;
#52591 = FACE_OUTER_BOUND ( 'NONE', #1021, .T. ) ;
#52592 = CARTESIAN_POINT ( 'NONE',  ( 32.29989959354726636, 7.591763852038296179, 66.68145312022730309 ) ) ;
#52593 = CARTESIAN_POINT ( 'NONE',  ( 45.58404625205363203, 9.294209029025518376, 86.84349537472557756 ) ) ;
#52594 = CARTESIAN_POINT ( 'NONE',  ( 17.48988570800758424, 7.568061572928497682, 17.97865980060091928 ) ) ;
#52595 = PLANE ( 'NONE',  #45294 ) ;
#52596 = CARTESIAN_POINT ( 'NONE',  ( -118.4553071845214447, 41.78724769484929880, 10.17744028903938336 ) ) ;
#52597 = DIRECTION ( 'NONE',  ( 0.000000000000000000, 1.000000000000000000, 0.000000000000000000 ) ) ;
#52598 = CARTESIAN_POINT ( 'NONE',  ( -445.5916540816261318, 394.9999999999995453, -139.3786363301466054 ) ) ;
#52599 = CARTESIAN_POINT ( 'NONE',  ( 22.15943197741200166, 7.796127622097904109, -20.13900179068516394 ) ) ;
#52600 = CARTESIAN_POINT ( 'NONE',  ( 157.4703587214989113, 57.65129005721575339, -36.12418429913763163 ) ) ;
#52601 = ORIENTED_EDGE ( 'NONE', *, *, #31760, .F. ) ;
#52602 = CARTESIAN_POINT ( 'NONE',  ( 157.4703587214989113, 58.92748579479260229, -36.12418429913763163 ) ) ;
#52603 = SHAPE_DEFINITION_REPRESENTATION ( #3588, #48255 ) ;
#52604 = LINE ( 'NONE', #27248, #48692 ) ;
#52605 = DIRECTION ( 'NONE',  ( -0.000000000000000000, -0.000000000000000000, -1.000000000000000000 ) ) ;
#52606 = CARTESIAN_POINT ( 'NONE',  ( 42.70988075781782811, 8.862408058333494765, -76.71303559248512727 ) ) ;
#52607 = ITEM_DEFINED_TRANSFORMATION ( 'NONE', 'NONE', #8571,  #66832 ) ;
#52608 = CARTESIAN_POINT ( 'NONE',  ( 73.57152302639893549, 14.62167909564604429, 170.0000000000000000 ) ) ;
#52609 = EDGE_LOOP ( 'NONE', ( #18573, #34527, #34689, #49496, #44680, #63663, #28924, #43537, #68070 ) ) ;
#52610 = ORIENTED_EDGE ( 'NONE', *, *, #19611, .F. ) ;
#52611 = CARTESIAN_POINT ( 'NONE',  ( -25.35398647985413234, 8.671412257862231243, -20.36380365964988570 ) ) ;
#52612 = CARTESIAN_POINT ( 'NONE',  ( 197.6329787101073805, 98.74106466892200729, 7.327278958723961289 ) ) ;
#52613 = ORIENTED_EDGE ( 'NONE', *, *, #8624, .T. ) ;
#52614 = VECTOR ( 'NONE', #63783, 1000.000000000000000 ) ;
#52615 = DIRECTION ( 'NONE',  ( -0.000000000000000000, -0.000000000000000000, -1.000000000000000000 ) ) ;
#52616 = ORIENTED_EDGE ( 'NONE', *, *, #16464, .T. ) ;
#52617 = CARTESIAN_POINT ( 'NONE',  ( 132.9557829392755366, 42.05591979570418459, -77.82755400474042062 ) ) ;
#52618 = CARTESIAN_POINT ( 'NONE',  ( 18.89356949897823768, 62.19351277735707839, 40.00000000000003553 ) ) ;
#52619 = AXIS2_PLACEMENT_3D ( 'NONE', #20346, #26668, #26328 ) ;
#52620 = LINE ( 'NONE', #14992, #38690 ) ;
#52622 = EDGE_CURVE ( 'NONE', #66690, #12453, #2543, .T. ) ;
#52621 = CARTESIAN_POINT ( 'NONE',  ( -99.11448999425219597, 31.20120877265620507, 31.20370467994214891 ) ) ;
#52623 = STYLED_ITEM ( 'NONE', ( #21088 ), #64062 ) ;
#52624 = FACE_OUTER_BOUND ( 'NONE', #9517, .T. ) ;
#52626 = VERTEX_POINT ( 'NONE', #40040 ) ;
#52625 = CARTESIAN_POINT ( 'NONE',  ( -56.92000000000000171, 0.000000000000000000, 30.00000000000000000 ) ) ;
#52627 = DIRECTION ( 'NONE',  ( 0.000000000000000000, 0.000000000000000000, -1.000000000000000000 ) ) ;
#52628 = EDGE_CURVE ( 'NONE', #56478, #35701, #61499, .T. ) ;
#52629 = EDGE_LOOP ( 'NONE', ( #45657, #53020, #22175, #58271 ) ) ;
#52630 = ORIENTED_EDGE ( 'NONE', *, *, #64505, .F. ) ;
#52631 = CARTESIAN_POINT ( 'NONE',  ( -118.9649285217355867, 42.09781191014327817, -18.45139938429198168 ) ) ;
#52632 = EDGE_CURVE ( 'NONE', #65565, #4244, #63569, .T. ) ;
#52633 = CARTESIAN_POINT ( 'NONE',  ( -39.09764951710989322, -70.01774562958885895, 133.5802547743875550 ) ) ;
#52634 = CARTESIAN_POINT ( 'NONE',  ( -178.5835577246388368, 93.42126246260829703, -20.51231665930944459 ) ) ;
#52636 = VERTEX_POINT ( 'NONE', #63227 ) ;
#52635 = CARTESIAN_POINT ( 'NONE',  ( -133.3923804760465543, 52.87100816290224969, 64.39721494377326394 ) ) ;
#52637 = CARTESIAN_POINT ( 'NONE',  ( 59.30258796551118650, 12.87111270082601244, 3.933392210405418865 ) ) ;
#52638 = B_SPLINE_CURVE_WITH_KNOTS ( 'NONE', 3,
 ( #65763, #6305, #44278, #39367 ),
 .UNSPECIFIED., .F., .F.,
 ( 4, 4 ),
 ( 9.900409499040004042E-07, 0.05658314289920114010 ),
 .UNSPECIFIED. ) ;
#52639 = EDGE_CURVE ( 'NONE', #49146, #7569, #68827, .T. ) ;
#52640 = LINE ( 'NONE', #63553, #1422 ) ;
#52641 = EDGE_LOOP ( 'NONE', ( #6029, #7904, #18602, #44437 ) ) ;
#52642 = CARTESIAN_POINT ( 'NONE',  ( -57.65733424639444138, 15.39521790791522982, -8.834354978680334369 ) ) ;
#52643 = CARTESIAN_POINT ( 'NONE',  ( -131.3096895243911035, 51.39228038925229924, -64.04718217629171306 ) ) ;
#52644 = CARTESIAN_POINT ( 'NONE',  ( -64.61430802170482934, -7.070445451048283481, 40.00000000000003553 ) ) ;
#52645 = DIRECTION ( 'NONE',  ( -0.000000000000000000, -0.000000000000000000, 1.000000000000000000 ) ) ;
#52646 = CARTESIAN_POINT ( 'NONE',  ( -150.3157714147627360, 64.86772057656135360, -88.53461949308422163 ) ) ;
#52647 = ORIENTED_EDGE ( 'NONE', *, *, #12388, .F. ) ;
#52648 = ADVANCED_FACE ( 'NONE', ( #51973 ), #56919, .F. ) ;
#52649 = ORIENTED_EDGE ( 'NONE', *, *, #5789, .F. ) ;
#52650 = CARTESIAN_POINT ( 'NONE',  ( 185.1647878987787124, 82.82967084668432278, -76.87782371961525030 ) ) ;
#52651 = CARTESIAN_POINT ( 'NONE',  ( 99.71998884745383407, 2.000000000000000000, 0.000000000000000000 ) ) ;
#52652 = CARTESIAN_POINT ( 'NONE',  ( 8.000000000000007105, 249.8719672152120381, -95.00000000000133582 ) ) ;
#52653 = DIRECTION ( 'NONE',  ( -0.000000000000000000, 1.000000000000000000, -0.000000000000000000 ) ) ;
#52654 = CARTESIAN_POINT ( 'NONE',  ( -73.63128929564828695, 21.53548093502884342, 43.48216365791507343 ) ) ;
#52655 = CARTESIAN_POINT ( 'NONE',  ( 84.73231936899557581, 18.78199960571076943, 29.94021395482606707 ) ) ;
#52656 = CARTESIAN_POINT ( 'NONE',  ( -149.0732005398558044, 63.81212100765655748, 45.71137907923015575 ) ) ;
#52657 = CARTESIAN_POINT ( 'NONE',  ( -118.9668643994983483, 43.27909474462861539, 41.00722457807798804 ) ) ;
#52658 = CARTESIAN_POINT ( 'NONE',  ( -165.6210506643949145, 79.15024150453837137, -68.75523839542780991 ) ) ;
#52659 = VERTEX_POINT ( 'NONE', #4142 ) ;
#52660 = CARTESIAN_POINT ( 'NONE',  ( -108.9452487746634404, 36.29752968355630571, -19.14672792289445624 ) ) ;
#52661 = VERTEX_POINT ( 'NONE', #42112 ) ;
#52662 = DIRECTION ( 'NONE',  ( 0.000000000000000000, 0.000000000000000000, 1.000000000000000000 ) ) ;
#52663 = CARTESIAN_POINT ( 'NONE',  ( 19.84876914995301078, -26.89441360497561107, 6.893343212288940869 ) ) ;
#52664 = CARTESIAN_POINT ( 'NONE',  ( 213.7144841804914392, 190.0000000000000000, 277.7626788299629652 ) ) ;
#52665 = CARTESIAN_POINT ( 'NONE',  ( -64.18058723658640474, -10.37664328995274055, 170.0000000000000000 ) ) ;
#52666 = CARTESIAN_POINT ( 'NONE',  ( 35.66087318222938762, 8.964867769223229033, 4.050215094464022059 ) ) ;
#52667 = CARTESIAN_POINT ( 'NONE',  ( 442.3372781065085633, 370.0000000000001137, -146.4497041420116830 ) ) ;
#52668 = LINE ( 'NONE', #24233, #21006 ) ;
#52669 = CARTESIAN_POINT ( 'NONE',  ( -97.49665543375860466, 31.53324358035375496, -63.56147199533193515 ) ) ;
#52670 = CARTESIAN_POINT ( 'NONE',  ( -37.93983213483220851, 11.77368372188049506, -12.20019562758866627 ) ) ;
#52671 = CONICAL_SURFACE ( 'NONE', #34726, 74.95140232871122521, 0.8777644062502172329 ) ;
#52672 = ORIENTED_EDGE ( 'NONE', *, *, #67437, .T. ) ;
#52673 = CARTESIAN_POINT ( 'NONE',  ( -125.4861769891490439, 47.42972183831692234, -88.60280507916131398 ) ) ;
#52674 = ORIENTED_EDGE ( 'NONE', *, *, #66788, .T. ) ;
#52675 = DIRECTION ( 'NONE',  ( -0.9988488985473030768, 0.000000000000000000, 0.04796746679614544151 ) ) ;
#52676 = CARTESIAN_POINT ( 'NONE',  ( 8.336237313193162635, 7.382629160459400985, -68.88587034052414992 ) ) ;
#52677 = CARTESIAN_POINT ( 'NONE',  ( -23.93880457192868860, 8.479983864459176957, 11.11157786848920637 ) ) ;
#52678 = CARTESIAN_POINT ( 'NONE',  ( 410.0000000000000000, 190.0000000000000000, -90.00000000000000000 ) ) ;
#52679 = CARTESIAN_POINT ( 'NONE',  ( 75.00000000000000000, 1.250000000000011102, 43.58025477438756923 ) ) ;
#52680 = FACE_BOUND ( 'NONE', #28936, .T. ) ;
#52681 = CARTESIAN_POINT ( 'NONE',  ( 150.2805372522807374, 53.51147386362155345, -41.47252479654510893 ) ) ;
#52682 = ORIENTED_EDGE ( 'NONE', *, *, #66822, .F. ) ;
#52683 = DIRECTION ( 'NONE',  ( -0.0003772202979824377123, 0.9999999288524207275, 4.066191827689635829E-15 ) ) ;
#52684 = CARTESIAN_POINT ( 'NONE',  ( -151.2511071212632032, 67.00426547928870491, 72.37311975729836888 ) ) ;
#52685 = CARTESIAN_POINT ( 'NONE',  ( 173.7263186949343776, 72.85225335320953377, -18.36293198726037801 ) ) ;
#52686 = CARTESIAN_POINT ( 'NONE',  ( -48.12872802574265307, 43.70867239603709464, 43.58025477438756923 ) ) ;
#52687 = DIRECTION ( 'NONE',  ( 0.000000000000000000, 0.000000000000000000, 1.000000000000000000 ) ) ;
#52688 = VERTEX_POINT ( 'NONE', #9419 ) ;
#52689 = DIRECTION ( 'NONE',  ( 1.000000000000000000, 0.000000000000000000, 0.000000000000000000 ) ) ;
#52690 = EDGE_CURVE ( 'NONE', #18889, #17838, #28338, .T. ) ;
#52691 = CARTESIAN_POINT ( 'NONE',  ( 94.12811352634518869, 22.11743943276049507, 63.53265709158580421 ) ) ;
#52692 = CARTESIAN_POINT ( 'NONE',  ( 117.7447573007802930, 32.50990724960317380, 37.60142151178813918 ) ) ;
#52693 = CARTESIAN_POINT ( 'NONE',  ( -147.4626691880993690, 62.46326773148431499, 84.67342306922898842 ) ) ;
#52694 = CARTESIAN_POINT ( 'NONE',  ( 136.9798231265810671, 43.34196232604180921, 30.17573291222522869 ) ) ;
#52695 = EDGE_LOOP ( 'NONE', ( #8596, #28818, #39679, #47865 ) ) ;
#52696 = CARTESIAN_POINT ( 'NONE',  ( 197.2200752504831485, 96.62072041958357715, 37.37195676832524782 ) ) ;
#52697 = LINE ( 'NONE', #46388, #23833 ) ;
#52698 = CARTESIAN_POINT ( 'NONE',  ( 187.8973304652193406, 87.27378997243177139, 33.66165893027326916 ) ) ;
#52699 = CARTESIAN_POINT ( 'NONE',  ( 156.3797504404255960, 58.07856685387021400, 29.48589258846897465 ) ) ;
#52700 = CARTESIAN_POINT ( 'NONE',  ( -12.99999999999999822, 0.000000000000000000, -17.00000000000000355 ) ) ;
#52701 = EDGE_LOOP ( 'NONE', ( #2902, #30410, #36110, #67537 ) ) ;
#52702 = CARTESIAN_POINT ( 'NONE',  ( 175.8947993867357411, 74.90689716047909030, 58.21729185181819588 ) ) ;
#52703 = ADVANCED_FACE ( 'NONE', ( #3788 ), #25258, .T. ) ;
#52704 = ORIENTED_EDGE ( 'NONE', *, *, #18818, .F. ) ;
#52705 = CARTESIAN_POINT ( 'NONE',  ( -108.6634958860518338, 36.14357436892402831, -38.56921122755016995 ) ) ;
#52706 = CARTESIAN_POINT ( 'NONE',  ( 68.93219921887761359, 14.12322281954860692, -74.68096442457768092 ) ) ;
#52707 = CARTESIAN_POINT ( 'NONE',  ( -61.86845765289633192, 16.61548683002700955, 34.67755665058201942 ) ) ;
#52708 = VECTOR ( 'NONE', #10075, 999.9999999999998863 ) ;
#52710 = EDGE_LOOP ( 'NONE', ( #42896, #33492, #10335, #43339 ) ) ;
#52709 = CARTESIAN_POINT ( 'NONE',  ( 150.2193536046551685, 53.46717047532149536, 8.129190380543040106 ) ) ;
#52711 = CARTESIAN_POINT ( 'NONE',  ( -178.0658882571760842, 92.80593104957425510, 32.67775869025225433 ) ) ;
#52712 = EDGE_CURVE ( 'NONE', #51562, #66812, #9764, .T. ) ;
#52713 = FACE_OUTER_BOUND ( 'NONE', #55969, .T. ) ;
#52714 = AXIS2_PLACEMENT_3D ( 'NONE', #15338, #11079, #36797 ) ;
#52715 = CARTESIAN_POINT ( 'NONE',  ( -450.6627218934913230, 217.8591479523843475, 78.55029585798814651 ) ) ;
#52716 = EDGE_LOOP ( 'NONE', ( #2621, #9400, #51465, #18642 ) ) ;
#52717 = DIRECTION ( 'NONE',  ( -1.000000000000000000, -1.001918046209079887E-14, 9.729495617646301779E-15 ) ) ;
#52718 = DIRECTION ( 'NONE',  ( 0.7530714660036099684, 0.6579387259397136978, 0.000000000000000000 ) ) ;
#52719 = CARTESIAN_POINT ( 'NONE',  ( 139.7928618793172859, 45.12615179300591706, 68.44561210618307712 ) ) ;
#52720 = CARTESIAN_POINT ( 'NONE',  ( -165.9111709580270997, 79.44576090485632847, 40.40830571265144755 ) ) ;
#52721 = CARTESIAN_POINT ( 'NONE',  ( 150.9184679586218749, 52.73111408630722252, 67.41327876333463109 ) ) ;
#52722 = CARTESIAN_POINT ( 'NONE',  ( -452.6627218934913230, 399.9999999999997726, 78.55029585798818914 ) ) ;
#52723 = EDGE_CURVE ( 'NONE', #20392, #48439, #46693, .T. ) ;
#52724 = EDGE_LOOP ( 'NONE', ( #10088, #19662, #23626, #51259 ) ) ;
#52725 = CARTESIAN_POINT ( 'NONE',  ( 46.90208227351340753, 10.52324439420451085, 10.32737426675875625 ) ) ;
#52726 = ORIENTED_EDGE ( 'NONE', *, *, #22875, .T. ) ;
#52727 = VECTOR ( 'NONE', #49513, 1000.000000000000000 ) ;
#52728 = EDGE_CURVE ( 'NONE', #34501, #52414, #14683, .T. ) ;
#52729 = CARTESIAN_POINT ( 'NONE',  ( 150.0516754638056227, 53.34587188591233797, -17.91502814048503112 ) ) ;
#52730 = CARTESIAN_POINT ( 'NONE',  ( 208.9583973663598329, 114.1615900753670871, -23.16983956928563160 ) ) ;
#52731 = CARTESIAN_POINT ( 'NONE',  ( 103.5589117581614715, 27.00490790413959985, 40.55142818294542906 ) ) ;
#52732 = DIRECTION ( 'NONE',  ( 0.000000000000000000, 0.000000000000000000, -1.000000000000000000 ) ) ;
#52733 = DIRECTION ( 'NONE',  ( 0.000000000000000000, 0.000000000000000000, 1.000000000000000000 ) ) ;
#52734 = DIRECTION ( 'NONE',  ( -1.000000000000000000, 1.421085471520200372E-14, 2.135044278125301096E-16 ) ) ;
#52735 = CARTESIAN_POINT ( 'NONE',  ( 47.70222499156840712, -57.81185381817577706, 41.38025477438755928 ) ) ;
#52736 = CARTESIAN_POINT ( 'NONE',  ( 46.39999999999999858, 0.000000000000000000, 0.000000000000000000 ) ) ;
#52737 = VERTEX_POINT ( 'NONE', #30876 ) ;
#52738 = PLANE ( 'NONE',  #26237 ) ;
#52739 = ORIENTED_EDGE ( 'NONE', *, *, #3817, .F. ) ;
#52740 = SURFACE_SIDE_STYLE ('',( #8475 ) ) ;
#52741 = CARTESIAN_POINT ( 'NONE',  ( -98.46684543088107944, 30.88557736720388647, -36.05183115025165819 ) ) ;
#52742 = CARTESIAN_POINT ( 'NONE',  ( 57.07734607129820148, 11.37318329671159844, -74.67266595444631605 ) ) ;
#52743 = DIRECTION ( 'NONE',  ( -0.000000000000000000, -1.000000000000000000, -0.000000000000000000 ) ) ;
#52744 = CARTESIAN_POINT ( 'NONE',  ( 444.9999999999999432, 225.0000000000000000, -2.000000000000000000 ) ) ;
#52745 = CARTESIAN_POINT ( 'NONE',  ( -11.28398375431312317, 7.140872483779192592, 84.64184783976759263 ) ) ;
#52746 = AXIS2_PLACEMENT_3D ( 'NONE', #18580, #61824, #50939 ) ;
#52747 = CARTESIAN_POINT ( 'NONE',  ( 164.8914542114683854, 64.97670918603527923, -71.58997600903566649 ) ) ;
#52748 = ORIENTED_EDGE ( 'NONE', *, *, #8440, .F. ) ;
#52749 = CARTESIAN_POINT ( 'NONE',  ( 19.40210676408052137, 63.75862954620263423, 34.48241823983693166 ) ) ;
#52750 = DIRECTION ( 'NONE',  ( -0.8118923937861950435, -0.5838071093367415143, 0.000000000000000000 ) ) ;
#52751 = ORIENTED_EDGE ( 'NONE', *, *, #46841, .T. ) ;
#52752 = ORIENTED_EDGE ( 'NONE', *, *, #56079, .T. ) ;
#52753 = CARTESIAN_POINT ( 'NONE',  ( 16.62148331457517969, -18.83783649008704586, 3.061616997868437868E-16 ) ) ;
#52754 = CYLINDRICAL_SURFACE ( 'NONE', #18699, 22.00000000000000355 ) ;
#52755 = CARTESIAN_POINT ( 'NONE',  ( 44.74620948996083314, -37.43371689815204917, 27.58472369426657522 ) ) ;
#52756 = DIRECTION ( 'NONE',  ( 1.000000000000000000, 0.000000000000000000, 0.000000000000000000 ) ) ;
#52757 = CIRCLE ( 'NONE', #38149, 243.4957430088094839 ) ;
#52758 = B_SPLINE_CURVE_WITH_KNOTS ( 'NONE', 3,
 ( #64742, #38001, #29528, #34489, #33779, #24271 ),
 .UNSPECIFIED., .F., .F.,
 ( 4, 2, 4 ),
 ( 0.03218933327099875868, 0.06469831623231236950, 0.09720729919362600113 ),
 .UNSPECIFIED. ) ;
#52759 = ORIENTED_EDGE ( 'NONE', *, *, #15180, .T. ) ;
#52760 = CARTESIAN_POINT ( 'NONE',  ( -126.8016613879753578, 48.30316697011515004, 45.57846390221672550 ) ) ;
#52761 = VERTEX_POINT ( 'NONE', #3446 ) ;
#52762 = CARTESIAN_POINT ( 'NONE',  ( 209.4789161463552034, 113.1367444519304399, 4.080444617825434328 ) ) ;
#52763 = CARTESIAN_POINT ( 'NONE',  ( -144.2155061717026285, 61.10843690942982676, 43.54120042493494225 ) ) ;
#52764 = CARTESIAN_POINT ( 'NONE',  ( 207.4696221732442609, 110.2206209205162395, 29.72680410229139270 ) ) ;
#52765 = EDGE_CURVE ( 'NONE', #35021, #51770, #36149, .T. ) ;
#52766 = CYLINDRICAL_SURFACE ( 'NONE', #58754, 7.500000000000020428 ) ;
#52767 = EDGE_CURVE ( 'NONE', #62345, #4217, #32983, .T. ) ;
#52768 = EDGE_LOOP ( 'NONE', ( #15862, #29719, #5756, #27956 ) ) ;
#52769 = ORIENTED_EDGE ( 'NONE', *, *, #28339, .F. ) ;
#52770 = DIRECTION ( 'NONE',  ( -0.000000000000000000, -0.000000000000000000, -1.000000000000000000 ) ) ;
#52771 = FACE_OUTER_BOUND ( 'NONE', #37639, .T. ) ;
#52772 = CARTESIAN_POINT ( 'NONE',  ( -165.9111709580270997, 79.44576090485637110, -13.28079546827590107 ) ) ;
#52773 = CARTESIAN_POINT ( 'NONE',  ( 140.8984307802396359, 45.84194788389004316, -73.00036953962161590 ) ) ;
#52774 = CARTESIAN_POINT ( 'NONE',  ( 68.45098769362923008, 13.99935947269946546, 32.13933842162290233 ) ) ;
#52775 = AXIS2_PLACEMENT_3D ( 'NONE', #66955, #18752, #51110 ) ;
#52776 = CARTESIAN_POINT ( 'NONE',  ( 9.152181272685988134, 7.385093848481300682, 94.71409728783903859 ) ) ;
#52777 = ORIENTED_EDGE ( 'NONE', *, *, #38703, .F. ) ;
#52779 = EDGE_CURVE ( 'NONE', #64948, #53864, #27112, .T. ) ;
#52778 = DIRECTION ( 'NONE',  ( -0.000000000000000000, -1.000000000000000000, -0.000000000000000000 ) ) ;
#52780 = CARTESIAN_POINT ( 'NONE',  ( -94.85061234775062644, 29.16417548023186868, 63.80561842459411537 ) ) ;
#52781 = EDGE_LOOP ( 'NONE', ( #59376, #37561, #6360, #13917, #47034, #9780, #21817 ) ) ;
#52782 = EDGE_CURVE ( 'NONE', #30284, #59205, #4459, .T. ) ;
#52783 = SHAPE_REPRESENTATION ( 'bearing', ( #66832 ), #47807 ) ;
#52784 = CARTESIAN_POINT ( 'NONE',  ( -81.01337222286372253, 23.22902179892322394, 3.934242872625056453 ) ) ;
#52785 = ORIENTED_EDGE ( 'NONE', *, *, #61099, .T. ) ;
#52786 = VERTEX_POINT ( 'NONE', #45229 ) ;
#52787 = ADVANCED_FACE ( 'NONE', ( #28356 ), #34352, .F. ) ;
#52788 = ORIENTED_EDGE ( 'NONE', *, *, #61745, .T. ) ;
#52789 = CARTESIAN_POINT ( 'NONE',  ( 15.29899606819416569, 6.485153354884285015, -50.51894409868581448 ) ) ;
#52790 = ADVANCED_FACE ( 'NONE', ( #23449 ), #55792, .F. ) ;
#52791 = AXIS2_PLACEMENT_3D ( 'NONE', #19537, #36410, #52582 ) ;
#52792 = CARTESIAN_POINT ( 'NONE',  ( -179.9014775667592971, 95.00669833041665413, 61.94859390510309538 ) ) ;
#52793 = CARTESIAN_POINT ( 'NONE',  ( 133.8566784816069344, 41.42467568809808398, 71.35489142945907304 ) ) ;
#52794 = ORIENTED_EDGE ( 'NONE', *, *, #46833, .T. ) ;
#52795 = B_SPLINE_CURVE_WITH_KNOTS ( 'NONE', 3,
 ( #55369, #1216, #12125, #61690, #17384, #44475, #18096, #7551, #50101, #22669, #13514, #6495, #2610, #1931, #38863, #23389, #50453, #66997, #65591, #61002 ),
 .UNSPECIFIED., .F., .F.,
 ( 4, 2, 2, 2, 2, 2, 2, 2, 2, 4 ),
 ( 0.000000000000000000, 0.001710655815380748542, 0.002565983723071116416, 0.003421311630761484073, 0.005131967446142231097, 0.006842623261522978555, 0.008553279076903725145, 0.01026393489228447087, 0.01197459070766521833, 0.01368524652304596405 ),
 .UNSPECIFIED. ) ;
#52796 = CARTESIAN_POINT ( 'NONE',  ( -24.41584901541038377, 8.543511933900191480, 88.69366999283610653 ) ) ;
#52797 = CARTESIAN_POINT ( 'NONE',  ( 152.8430172091323413, 54.14068524174422237, 31.00228809141104236 ) ) ;
#52798 = CARTESIAN_POINT ( 'NONE',  ( -26.07811460555695859, -76.21509903021815546, 73.58025477438756923 ) ) ;
#52799 = DIRECTION ( 'NONE',  ( 0.000000000000000000, -0.7660444431189770143, 0.6427876096865403621 ) ) ;
#52800 = ADVANCED_FACE ( 'NONE', ( #7617 ), #2333, .F. ) ;
#52801 = CARTESIAN_POINT ( 'NONE',  ( -26.49516976694651049, 8.831756547364859600, 43.37753662398635157 ) ) ;
#52802 = CARTESIAN_POINT ( 'NONE',  ( -142.0070007485041117, 59.34878529741516218, -69.42688443671409004 ) ) ;
#52803 = EDGE_LOOP ( 'NONE', ( #31300, #21781, #5802, #15894, #1747, #58059, #36071, #23244, #33564 ) ) ;
#52804 = EDGE_CURVE ( 'NONE', #12488, #22095, #7950, .T. ) ;
#52805 = EDGE_CURVE ( 'NONE', #22725, #30259, #6559, .T. ) ;
#52806 = AXIS2_PLACEMENT_3D ( 'NONE', #59533, #47945, #31442 ) ;
#52807 = EDGE_CURVE ( 'NONE', #51157, #33219, #37019, .T. ) ;
#52808 = DIRECTION ( 'NONE',  ( -0.000000000000000000, -0.000000000000000000, -1.000000000000000000 ) ) ;
#52809 = CARTESIAN_POINT ( 'NONE',  ( -81.90760111942957167, 24.66532273091450378, -62.67973089774071838 ) ) ;
#52810 = CARTESIAN_POINT ( 'NONE',  ( 177.7886308167536527, 76.74396398590873503, 16.71637049643586082 ) ) ;
#52811 = DIRECTION ( 'NONE',  ( 0.000000000000000000, -1.000000000000000000, 0.000000000000000000 ) ) ;
#52812 = DIRECTION ( 'NONE',  ( -0.000000000000000000, 1.000000000000000000, -0.000000000000000000 ) ) ;
#52813 = CARTESIAN_POINT ( 'NONE',  ( 128.3856248084844651, 38.21741401878865929, 5.012217174567255462 ) ) ;
#52814 = CARTESIAN_POINT ( 'NONE',  ( -153.7005182577089499, 67.81869626254724892, 17.61129303604968754 ) ) ;
#52815 = CARTESIAN_POINT ( 'NONE',  ( 197.2059918558470031, 98.20695231513643364, 90.81591397967092405 ) ) ;
#52816 = CARTESIAN_POINT ( 'NONE',  ( 63.50528314073022784, 12.78634332146811836, 17.96841034875761167 ) ) ;
#52817 = CARTESIAN_POINT ( 'NONE',  ( 164.6406716478538783, 63.44801348349344039, 7.848966783923891910 ) ) ;
#52818 = LINE ( 'NONE', #68996, #41034 ) ;
#52819 = EDGE_LOOP ( 'NONE', ( #30700, #38801, #9363, #42867 ) ) ;
#52820 = CONTEXT_DEPENDENT_SHAPE_REPRESENTATION ( #57057, #23787 ) ;
#52821 = CARTESIAN_POINT ( 'NONE',  ( -54.44781833988737674, 15.56115186513848414, 84.02420198347161318 ) ) ;
#52822 = VERTEX_POINT ( 'NONE', #53167 ) ;
#52823 = CARTESIAN_POINT ( 'NONE',  ( 141.9165763529819344, -2.000000000000001776, 129.0000000000000000 ) ) ;
#52824 = ORIENTED_EDGE ( 'NONE', *, *, #67854, .T. ) ;
#52825 = CARTESIAN_POINT ( 'NONE',  ( 16.28382582968307446, 7.523443033994206885, -62.36349468914945504 ) ) ;
#52826 = LINE ( 'NONE', #58794, #22628 ) ;
#52827 = CARTESIAN_POINT ( 'NONE',  ( 0.000000000000000000, 0.000000000000000000, 170.0000000000000000 ) ) ;
#52828 = CARTESIAN_POINT ( 'NONE',  ( 89.99999999999998579, 0.000000000000000000, -10.00000000000000000 ) ) ;
#52829 = AXIS2_PLACEMENT_3D ( 'NONE', #55078, #16751, #22380 ) ;
#52830 = CARTESIAN_POINT ( 'NONE',  ( 141.0517870458593848, 47.14452711594499590, -41.39047569224774037 ) ) ;
#52831 = CARTESIAN_POINT ( 'NONE',  ( 36.76746179515744473, 8.081433644308900099, -36.09346771175318480 ) ) ;
#52832 = CARTESIAN_POINT ( 'NONE',  ( 0.000000000000000000, 0.000000000000000000, -8.000000000000000000 ) ) ;
#52833 = CARTESIAN_POINT ( 'NONE',  ( 0.000000000000000000, 0.000000000000000000, 2.000000000000000000 ) ) ;
#52834 = DIRECTION ( 'NONE',  ( 1.156482317317871478E-16, 0.000000000000000000, 1.000000000000000000 ) ) ;
#52835 = EDGE_LOOP ( 'NONE', ( #18367, #14030, #8206, #58365 ) ) ;
#52836 = ORIENTED_EDGE ( 'NONE', *, *, #22290, .T. ) ;
#52837 = CARTESIAN_POINT ( 'NONE',  ( 173.6087636303235513, 72.74229495189189265, 89.85593697944948133 ) ) ;
#52838 = CARTESIAN_POINT ( 'NONE',  ( -167.6566265204789374, 82.70140535081088728, -10.22451876400831772 ) ) ;
#52839 = PRODUCT_DEFINITION_CONTEXT ( 'detailed design', #12058, 'design' ) ;
#52840 = AXIS2_PLACEMENT_3D ( 'NONE', #20667, #3806, #4158 ) ;
#52841 = FACE_BOUND ( 'NONE', #20358, .T. ) ;
#52842 = CARTESIAN_POINT ( 'NONE',  ( 280.6583185015672370, 21.43197767180794244, 4.967364376802513526 ) ) ;
#52843 = CARTESIAN_POINT ( 'NONE',  ( -31.11269837220809364, -10.55634918610397932, 85.00100000000000477 ) ) ;
#52844 = CARTESIAN_POINT ( 'NONE',  ( 180.2572128312847610, 77.77323980479698662, -78.03573907910868002 ) ) ;
#52845 = CARTESIAN_POINT ( 'NONE',  ( -180.2244609727085560, 95.39945930389649220, -44.63604071467989343 ) ) ;
#52846 = CARTESIAN_POINT ( 'NONE',  ( 94.02921784728461319, 22.08005910033071117, -15.23014068625460027 ) ) ;
#52847 = CARTESIAN_POINT ( 'NONE',  ( -10.00000000000000000, 0.000000000000000000, 0.000000000000000000 ) ) ;
#52848 = DIRECTION ( 'NONE',  ( 1.000000000000000000, 0.000000000000000000, 0.000000000000000000 ) ) ;
#52849 = CARTESIAN_POINT ( 'NONE',  ( -417.6627218934916073, 397.0710678118612691, 78.55029585799223923 ) ) ;
#52850 = ADVANCED_FACE ( 'NONE', ( #57438 ), #36676, .F. ) ;
#52851 = ORIENTED_EDGE ( 'NONE', *, *, #13200, .T. ) ;
#52852 = CARTESIAN_POINT ( 'NONE',  ( 128.0540543950622236, 39.18660671946770435, 14.94423530046998572 ) ) ;
#52853 = DIRECTION ( 'NONE',  ( 0.000000000000000000, 0.000000000000000000, -1.000000000000000000 ) ) ;
#52854 = CARTESIAN_POINT ( 'NONE',  ( 157.4703587214989398, -170.0000000000000000, -43.62418429913764584 ) ) ;
#52855 = CARTESIAN_POINT ( 'NONE',  ( -78.66644367742111399, -170.0000000000000000, -69.46000122218158879 ) ) ;
#52856 = CARTESIAN_POINT ( 'NONE',  ( 150.0501577908835884, 52.10460126680129633, 11.19079014285864204 ) ) ;
#52857 = FACE_OUTER_BOUND ( 'NONE', #17453, .T. ) ;
#52858 = EDGE_LOOP ( 'NONE', ( #21653, #68474, #58943, #51952 ) ) ;
#52860 = EDGE_CURVE ( 'NONE', #36237, #11965, #21185, .T. ) ;
#52859 = CARTESIAN_POINT ( 'NONE',  ( -15.55634918610403439, 2.818925648462311528E-14, 2.000000000000001776 ) ) ;
#52861 = EDGE_CURVE ( 'NONE', #62679, #18878, #69366, .T. ) ;
#52862 = CARTESIAN_POINT ( 'NONE',  ( 5.850262805259840881, 192.0000000000000000, -1.724042536399416514 ) ) ;
#52863 = ORIENTED_EDGE ( 'NONE', *, *, #15489, .T. ) ;
#52864 = EDGE_CURVE ( 'NONE', #25590, #59450, #64001, .T. ) ;
#52865 = EDGE_LOOP ( 'NONE', ( #25745, #60772 ) ) ;
#52866 = CARTESIAN_POINT ( 'NONE',  ( 32.32377689436478363, 8.605407956458130059, 88.60103337961240300 ) ) ;
#52867 = CARTESIAN_POINT ( 'NONE',  ( -179.9014775667593256, 95.00669833041665413, -72.27415904721529216 ) ) ;
#52868 = B_SPLINE_CURVE_WITH_KNOTS ( 'NONE', 3,
 ( #45529, #67009, #45880, #3656, #25476, #46213, #46562, #46915, #25129, #18459 ),
 .UNSPECIFIED., .F., .F.,
 ( 4, 2, 2, 2, 4 ),
 ( 0.000000000000000000, 0.001117128179507491988, 0.002234256359014983977, 0.003351384538522475965, 0.004468512718029967953 ),
 .UNSPECIFIED. ) ;
#52869 = FACE_OUTER_BOUND ( 'NONE', #35557, .T. ) ;
#52870 = ORIENTED_EDGE ( 'NONE', *, *, #46259, .F. ) ;
#52871 = ADVANCED_FACE ( 'NONE', ( #22219 ), #765, .F. ) ;
#52872 = FACE_OUTER_BOUND ( 'NONE', #63731, .T. ) ;
#52873 = LINE ( 'NONE', #14571, #64544 ) ;
#52874 = VECTOR ( 'NONE', #65046, 1000.000000000000000 ) ;
#52875 = CARTESIAN_POINT ( 'NONE',  ( -0.3732240621745017695, 7.527003275829100559, 11.75034198667222718 ) ) ;
#52876 = CARTESIAN_POINT ( 'NONE',  ( 174.4912080999798718, 73.57140295268875718, -40.13899342073425913 ) ) ;
#52877 = CARTESIAN_POINT ( 'NONE',  ( 159.9380463867843503, 59.59435412114020636, 83.49017641889444974 ) ) ;
#52878 = DIRECTION ( 'NONE',  ( -1.000000000000000000, -0.000000000000000000, -0.000000000000000000 ) ) ;
#52879 = VECTOR ( 'NONE', #68206, 1000.000000000000000 ) ;
#52880 = PRODUCT ( 'pulley', 'pulley', '', ( #67767 ) ) ;
#52881 = ORIENTED_EDGE ( 'NONE', *, *, #52246, .F. ) ;
#52882 = VECTOR ( 'NONE', #67711, 1000.000000000000000 ) ;
#52883 = PRESENTATION_STYLE_ASSIGNMENT (( #63112 ) ) ;
#52884 = CARTESIAN_POINT ( 'NONE',  ( 13.37366753069832903, 6.435102282077983737, 57.24155959848373243 ) ) ;
#52885 = CARTESIAN_POINT ( 'NONE',  ( 14.81290967676422277, 7.477658233646010899, 30.06210274491325407 ) ) ;
#52886 = CARTESIAN_POINT ( 'NONE',  ( 204.6977192012829789, 108.0580384837235073, 44.20772073876944575 ) ) ;
#52887 = B_SPLINE_CURVE_WITH_KNOTS ( 'NONE', 3,
 ( #6588, #50542, #28034, #60742, #29096, #6932 ),
 .UNSPECIFIED., .F., .F.,
 ( 4, 2, 4 ),
 ( 1.095770181096429506E-06, 0.03239442681617710207, 0.06478775786217309818 ),
 .UNSPECIFIED. ) ;
#52888 = CARTESIAN_POINT ( 'NONE',  ( -86.13811263329068879, 26.40116547045850837, 90.87883607248001283 ) ) ;
#52890 = VERTEX_POINT ( 'NONE', #5677 ) ;
#52889 = DIRECTION ( 'NONE',  ( -0.000000000000000000, 1.000000000000000000, -0.000000000000000000 ) ) ;
#52891 = ORIENTED_EDGE ( 'NONE', *, *, #11992, .F. ) ;
#52892 = AXIS2_PLACEMENT_3D ( 'NONE', #3602, #3953, #46859 ) ;
#52893 = EDGE_CURVE ( 'NONE', #889, #59217, #37959, .T. ) ;
#52894 = VERTEX_POINT ( 'NONE', #27841 ) ;
#52895 = CARTESIAN_POINT ( 'NONE',  ( 116.0963032583228483, 32.80867113471310148, -74.98255735860550431 ) ) ;
#52896 = DIRECTION ( 'NONE',  ( 0.000000000000000000, 0.000000000000000000, 1.000000000000000000 ) ) ;
#52897 = CARTESIAN_POINT ( 'NONE',  ( 204.6977192012829789, 106.3443248447423457, -63.17048162308526571 ) ) ;
#52898 = ADVANCED_FACE ( 'NONE', ( #54909 ), #49632, .F. ) ;
#52899 = CARTESIAN_POINT ( 'NONE',  ( -55.05276343752909440, 14.68156374112638929, -23.37177340799619785 ) ) ;
#52900 = LINE ( 'NONE', #4721, #53378 ) ;
#52901 = CARTESIAN_POINT ( 'NONE',  ( 152.2940756559019064, 53.73566983921583784, -75.90150279893470042 ) ) ;
#52902 = LINE ( 'NONE', #4048, #19646 ) ;
#52903 = CARTESIAN_POINT ( 'NONE',  ( -152.9119739516381173, 67.12135129037710612, -49.01105990250665911 ) ) ;
#52904 = ORIENTED_EDGE ( 'NONE', *, *, #1100, .T. ) ;
#52905 = VERTEX_POINT ( 'NONE', #21735 ) ;
#52906 = CARTESIAN_POINT ( 'NONE',  ( 69.72564955710448942, 15.37006465677308675, -13.01647048107183124 ) ) ;
#52907 = CARTESIAN_POINT ( 'NONE',  ( -85.64924756730678723, 26.19583280090850153, -45.36369601798204343 ) ) ;
#52908 = CARTESIAN_POINT ( 'NONE',  ( 159.2389084450349515, 59.03884018680375334, 71.05616836873035425 ) ) ;
#52909 = CARTESIAN_POINT ( 'NONE',  ( 117.3145357257065484, 33.41973663092564095, -14.02774205371277638 ) ) ;
#52910 = CARTESIAN_POINT ( 'NONE',  ( 204.6977192012829789, 106.3443248447423173, -9.481380442157895772 ) ) ;
#52911 = DIRECTION ( 'NONE',  ( 1.000000000000000000, 1.387778780781445676E-16, -1.110223024625156294E-16 ) ) ;
#52912 = CARTESIAN_POINT ( 'NONE',  ( 133.8566784816069060, 42.60093787723652525, -9.178760341931967659 ) ) ;
#52913 = VERTEX_POINT ( 'NONE', #27016 ) ;
#52914 = ORIENTED_EDGE ( 'NONE', *, *, #43171, .T. ) ;
#52915 = ORIENTED_EDGE ( 'NONE', *, *, #17367, .F. ) ;
#52916 = CARTESIAN_POINT ( 'NONE',  ( 34.43940527065477397, -66.63700071734618291, 43.58025477438756212 ) ) ;
#52917 = CARTESIAN_POINT ( 'NONE',  ( 37.46876540261052924, 9.179568636624026112, -50.37052167088771881 ) ) ;
#52918 = DIRECTION ( 'NONE',  ( 0.000000000000000000, -0.000000000000000000, -1.000000000000000000 ) ) ;
#52919 = VECTOR ( 'NONE', #23298, 1000.000000000000000 ) ;
#52920 = CARTESIAN_POINT ( 'NONE',  ( 0.000000000000000000, 0.000000000000000000, 0.000000000000000000 ) ) ;
#52921 = CARTESIAN_POINT ( 'NONE',  ( 197.3119541548906568, 98.33923235143190311, 62.23820161575331866 ) ) ;
#52922 = ORIENTED_EDGE ( 'NONE', *, *, #16382, .T. ) ;
#52923 = CARTESIAN_POINT ( 'NONE',  ( 0.000000000000000000, 0.000000000000000000, 170.0000000000000000 ) ) ;
#52924 = CARTESIAN_POINT ( 'NONE',  ( 15.78827728214693416, 6.500811158483328356, -8.674393508222097537 ) ) ;
#52925 =( NAMED_UNIT ( * ) PLANE_ANGLE_UNIT ( ) SI_UNIT ( $, .RADIAN. ) );
#52926 = CARTESIAN_POINT ( 'NONE',  ( 23.28845814680232351, 7.864847136539610872, 10.18352427007710759 ) ) ;
#52927 = CARTESIAN_POINT ( 'NONE',  ( 187.2354698746857196, 85.05376776489248414, 59.33325302814636615 ) ) ;
#52928 = DIRECTION ( 'NONE',  ( 1.000000000000000000, -0.000000000000000000, -0.000000000000000000 ) ) ;
#52929 = CARTESIAN_POINT ( 'NONE',  ( -444.3832201885271616, 394.6953840236894280, -129.6748612749917129 ) ) ;
#52930 = CARTESIAN_POINT ( 'NONE',  ( 15.55634918610396511, -41.66904755831214402, 0.000000000000000000 ) ) ;
#52932 = EDGE_CURVE ( 'NONE', #50048, #2626, #44044, .T. ) ;
#52931 = CYLINDRICAL_SURFACE ( 'NONE', #69139, 5.000000000000004441 ) ;
#52933 = CARTESIAN_POINT ( 'NONE',  ( 9.689943677145723910, 7.388265075009363692, 6.297457479611937359 ) ) ;
#52934 = VECTOR ( 'NONE', #31237, 1000.000000000000000 ) ;
#52935 = EDGE_CURVE ( 'NONE', #46646, #28268, #5884, .T. ) ;
#52936 = VERTEX_POINT ( 'NONE', #42839 ) ;
#52937 = CARTESIAN_POINT ( 'NONE',  ( 188.4359598230020367, 86.36951380984524462, 8.452180733291799086 ) ) ;
#52938 = APPLICATION_PROTOCOL_DEFINITION ( 'draft international standard', 'automotive_design', 1998, #58769 ) ;
#52939 = VECTOR ( 'NONE', #39436, 1000.000000000000000 ) ;
#52940 = CARTESIAN_POINT ( 'NONE',  ( 174.2469308602415197, 71.96142024047685481, 33.71361340695089126 ) ) ;
#52941 = CARTESIAN_POINT ( 'NONE',  ( 9.850262805259839993, 192.0000000000000000, -1.724042536399416514 ) ) ;
#52942 = CARTESIAN_POINT ( 'NONE',  ( -109.7643866341847314, 37.89854104106755983, -43.06589634579863457 ) ) ;
#52943 = CARTESIAN_POINT ( 'NONE',  ( 188.0094179620990928, 87.39792407168452826, -46.61815432678586291 ) ) ;
#52944 = ORIENTED_EDGE ( 'NONE', *, *, #42506, .F. ) ;
#52945 = B_SPLINE_CURVE_WITH_KNOTS ( 'NONE', 3,
 ( #32024, #27418, #22153, #16529, #59080, #43598, #26058, #15504, #37984, #54137, #5283, #42898, #36954, #48856, #33061, #47837 ),
 .UNSPECIFIED., .F., .F.,
 ( 4, 2, 2, 2, 2, 2, 2, 4 ),
 ( 0.01170309506547633979, 0.01321020703997516713, 0.01471731901447399446, 0.01773154296347164566, 0.01923865493797047993, 0.02074576691246931073, 0.02225287888696814154, 0.02375999086146697581 ),
 .UNSPECIFIED. ) ;
#52946 = EDGE_LOOP ( 'NONE', ( #56917, #52751, #39825 ) ) ;
#52948 = EDGE_CURVE ( 'NONE', #54192, #29393, #24998, .T. ) ;
#52947 = CARTESIAN_POINT ( 'NONE',  ( 121.4242852856285140, 6.000000000000000000, -30.00000000000000355 ) ) ;
#52949 = CARTESIAN_POINT ( 'NONE',  ( 204.3091227790962705, 107.5190503136782638, 17.36317014830577676 ) ) ;
#52950 = ORIENTED_EDGE ( 'NONE', *, *, #28862, .F. ) ;
#52951 = ADVANCED_FACE ( 'NONE', ( #65919 ), #33976, .T. ) ;
#52952 = CARTESIAN_POINT ( 'NONE',  ( 112.1164716692773879, 29.75790342121401366, 71.23340654744586686 ) ) ;
#52953 = EDGE_LOOP ( 'NONE', ( #15325, #10918, #48648, #62316, #51277, #5383, #13816, #60848, #30044, #59410, #48698, #55893, #46021, #51512, #41882, #23951, #35596, #532, #67397, #68587, #57855, #10450, #53438, #19210, #13496, #6190, #24357, #50553, #15447, #37298, #29836, #33011, #67876, #39220, #65167, #36704, #57142, #26605, #724, #65777, #64421, #52241, #47442, #29032, #45330, #51539, #44718, #58329, #12586, #30853, #4906, #2, #2807, #5411, #32437, #13931, #37845, #56358, #64847, #51332, #5172, #29812, #53990, #30479, #58382, #30828, #28074, #19816, #37007, #36137, #259, #30417, #12691, #39339, #42336, #49637, #12399, #25858, #37778, #8190, #58917, #20310, #8474, #67630, #59511, #46715, #23440, #25354, #3247, #33888, #61546, #52149, #29579, #49071, #69341, #61503, #47015, #22164, #42589, #15525, #1684, #1269, #40512, #61618, #60242, #56726, #425, #55097, #23123, #40044, #49806, #66071, #12759, #4619, #49891, #54144, #38667, #20042, #23704, #32304, #63641, #67330, #68094, #9733, #8090, #10509, #3758, #12080, #8946, #50592, #31456, #62050, #731, #68619, #28470, #47983, #16962, #57357, #19641, #56274, #12461 ) ) ;
#52954 = DIRECTION ( 'NONE',  ( 0.000000000000000000, -0.000000000000000000, -1.000000000000000000 ) ) ;
#52955 = DIRECTION ( 'NONE',  ( -0.000000000000000000, -0.000000000000000000, 1.000000000000000000 ) ) ;
#52956 = ADVANCED_FACE ( 'NONE', ( #31614 ), #4536, .F. ) ;
#52957 = DIRECTION ( 'NONE',  ( -0.000000000000000000, -0.000000000000000000, -1.000000000000000000 ) ) ;
#52958 = DIRECTION ( 'NONE',  ( -0.000000000000000000, -0.000000000000000000, -1.000000000000000000 ) ) ;
#52959 = CARTESIAN_POINT ( 'NONE',  ( 61.91366885787729046, 28.42865614899000448, 41.38025477438755928 ) ) ;
#52961 = ORIENTED_EDGE ( 'NONE', *, *, #43446, .F. ) ;
#52960 = CARTESIAN_POINT ( 'NONE',  ( -64.18058723658653264, 10.37664328995176888, 43.58025477438756923 ) ) ;
#52962 = CARTESIAN_POINT ( 'NONE',  ( 0.000000000000000000, 0.000000000000000000, 170.0000000000000000 ) ) ;
#52963 = ORIENTED_EDGE ( 'NONE', *, *, #21924, .F. ) ;
#52964 = VERTEX_POINT ( 'NONE', #26685 ) ;
#52965 = CARTESIAN_POINT ( 'NONE',  ( -167.1619226259399511, 82.18315278115417755, 6.916214303503440242 ) ) ;
#52966 = DIRECTION ( 'NONE',  ( -1.000000000000000000, 0.000000000000000000, 0.000000000000000000 ) ) ;
#52967 = CARTESIAN_POINT ( 'NONE',  ( 149.0250918491436494, 0.000000000000000000, -41.68900338898718871 ) ) ;
#52968 = FACE_OUTER_BOUND ( 'NONE', #8085, .T. ) ;
#52970 = ORIENTED_EDGE ( 'NONE', *, *, #22943, .F. ) ;
#52969 = CARTESIAN_POINT ( 'NONE',  ( -147.3614567344829709, 62.37986555269943523, -35.11266540856631480 ) ) ;
#52971 = CARTESIAN_POINT ( 'NONE',  ( -107.0277617056979551, 36.40097422522767090, 85.89409362202775355 ) ) ;
#52972 = CIRCLE ( 'NONE', #21542, 65.36598343705435354 ) ;
#52973 = EDGE_LOOP ( 'NONE', ( #20104, #53244, #6315, #12005 ) ) ;
#52974 = AXIS2_PLACEMENT_3D ( 'NONE', #46309, #30156, #19941 ) ;
#52975 = DIRECTION ( 'NONE',  ( -1.000000000000000000, 0.000000000000000000, 0.000000000000000000 ) ) ;
#52976 = EDGE_CURVE ( 'NONE', #47695, #38528, #21393, .T. ) ;
#52977 = AXIS2_PLACEMENT_3D ( 'NONE', #11288, #64769, #22902 ) ;
#52978 = STYLED_ITEM ( 'NONE', ( #19645 ), #17922 ) ;
#52979 = CARTESIAN_POINT ( 'NONE',  ( -133.0835080491124813, 52.64966140620843049, -71.40981646950953632 ) ) ;
#52980 = LINE ( 'NONE', #4803, #28033 ) ;
#52981 = DIRECTION ( 'NONE',  ( 0.4738686624729966379, 0.8805955318567391110, 0.000000000000000000 ) ) ;
#52982 = CARTESIAN_POINT ( 'NONE',  ( -95.88718821240198054, 29.65015105908824822, -73.28914486612443113 ) ) ;
#52983 = ORIENTED_EDGE ( 'NONE', *, *, #16814, .F. ) ;
#52984 = ORIENTED_EDGE ( 'NONE', *, *, #50213, .F. ) ;
#52985 = CIRCLE ( 'NONE', #23844, 5.000000000000000000 ) ;
#52986 = DIRECTION ( 'NONE',  ( -0.000000000000000000, -0.000000000000000000, -1.000000000000000000 ) ) ;
#52987 = AXIS2_PLACEMENT_3D ( 'NONE', #62933, #14735, #52028 ) ;
#52988 = CARTESIAN_POINT ( 'NONE',  ( 39.54205320694339321, 51.58901073076764021, 40.00000000000003553 ) ) ;
#52989 = CARTESIAN_POINT ( 'NONE',  ( 444.9999999999999432, -35.00000000000000000, 380.0000000000000000 ) ) ;
#52990 = LINE ( 'NONE', #38556, #17580 ) ;
#52991 = CARTESIAN_POINT ( 'NONE',  ( -71.57025115638937507, 20.80908992785612810, 35.43902869127500566 ) ) ;
#52992 = CARTESIAN_POINT ( 'NONE',  ( 82.34195123877069022, 18.00239921638039320, 43.37057751023843366 ) ) ;
#52993 = CARTESIAN_POINT ( 'NONE',  ( 69.83260694998126894, 15.39825517924929521, -40.08384761986350497 ) ) ;
#52994 = CARTESIAN_POINT ( 'NONE',  ( -120.6420427933462207, 44.31795133507804252, 32.75998872186478650 ) ) ;
#52995 = CARTESIAN_POINT ( 'NONE',  ( 210.9747454890631673, 115.3673079504855963, 67.66528286333071662 ) ) ;
#52996 = ORIENTED_EDGE ( 'NONE', *, *, #51571, .T. ) ;
#52997 = FACE_OUTER_BOUND ( 'NONE', #39961, .T. ) ;
#52998 = EDGE_LOOP ( 'NONE', ( #36045, #37406, #44427, #19359, #38636, #35284, #23544, #48167, #49480 ) ) ;
#52999 = CARTESIAN_POINT ( 'NONE',  ( -59.09450113343203270, -27.07101652673575032, 40.00000000000003553 ) ) ;
#53000 = CARTESIAN_POINT ( 'NONE',  ( 40.56810594101300893, -52.87564016363982233, 34.48241795236665297 ) ) ;
#53001 = DIRECTION ( 'NONE',  ( 0.000000000000000000, 0.000000000000000000, 1.000000000000000000 ) ) ;
#53002 = CARTESIAN_POINT ( 'NONE',  ( 154.4429418375332546, 55.33424769452791026, -23.65634912063520545 ) ) ;
#53003 = DIRECTION ( 'NONE',  ( -0.7071067811865405783, -7.105427357601001070E-15, 0.7071067811865545671 ) ) ;
#53004 = DIRECTION ( 'NONE',  ( -0.8160245890732938934, -0.5780171883497599028, 0.000000000000000000 ) ) ;
#53005 = CARTESIAN_POINT ( 'NONE',  ( 32.09567473596477072, 7.571373529017936477, -68.25274485065961017 ) ) ;
#53006 = LINE ( 'NONE', #10447, #63723 ) ;
#53007 = CARTESIAN_POINT ( 'NONE',  ( -34.52542994698664813, 11.14027065218092361, -9.132801045176456967 ) ) ;
#53008 = EDGE_LOOP ( 'NONE', ( #17921, #39583, #36764, #66662 ) ) ;
#53009 = CARTESIAN_POINT ( 'NONE',  ( -124.2594596607281119, 46.62660695211089745, -88.78007805360886096 ) ) ;
#53010 = ORIENTED_EDGE ( 'NONE', *, *, #36051, .F. ) ;
#53011 = DIRECTION ( 'NONE',  ( 1.000000000000000000, 0.000000000000000000, 0.000000000000000000 ) ) ;
#53012 = CARTESIAN_POINT ( 'NONE',  ( -16.43619359402603664, -18.99971924381128474, 3.061616997868437868E-16 ) ) ;
#53013 = DIRECTION ( 'NONE',  ( -1.000000000000000000, 0.000000000000000000, 0.000000000000000000 ) ) ;
#53014 = LINE ( 'NONE', #68193, #68212 ) ;
#53016 = EDGE_CURVE ( 'NONE', #1969, #28828, #10151, .T. ) ;
#53015 = CARTESIAN_POINT ( 'NONE',  ( -0.5183605925911985990, 6.525266619725956119, 35.90767484529200004 ) ) ;
#53017 = CARTESIAN_POINT ( 'NONE',  ( -94.78109144324895396, 29.13179392050636451, -15.95525421150224155 ) ) ;
#53018 = CARTESIAN_POINT ( 'NONE',  ( 151.1700480242206197, 54.15904440870136227, -39.54687096424860471 ) ) ;
#53019 = EDGE_CURVE ( 'NONE', #45299, #66935, #12814, .T. ) ;
#53020 = ORIENTED_EDGE ( 'NONE', *, *, #57584, .T. ) ;
#53021 = EDGE_CURVE ( 'NONE', #61986, #55566, #14706, .T. ) ;
#53022 = AXIS2_PLACEMENT_3D ( 'NONE', #39390, #50296, #6682 ) ;
#53023 = DIRECTION ( 'NONE',  ( 0.8144611520881498423, 0.5802180898069654313, 2.459837888935112854E-15 ) ) ;
#53024 = DIRECTION ( 'NONE',  ( -1.000000000000000000, 0.000000000000000000, 0.000000000000000000 ) ) ;
#53025 = CARTESIAN_POINT ( 'NONE',  ( 174.1422537179815322, 73.24254491731257133, -19.73406368843727066 ) ) ;
#53026 = CARTESIAN_POINT ( 'NONE',  ( -107.0544991134679265, 36.41543129049374272, 59.07449925621195774 ) ) ;
#53027 = ITEM_DEFINED_TRANSFORMATION ( 'NONE', 'NONE', #19812,  #66832 ) ;
#53028 = CARTESIAN_POINT ( 'NONE',  ( 0.1306530452038109080, 7.903938623646869388, 2.309976723937612775 ) ) ;
#53029 = ORIENTED_EDGE ( 'NONE', *, *, #32611, .F. ) ;
#53030 = DIRECTION ( 'NONE',  ( 1.000000000000000000, 0.000000000000000000, 0.000000000000000000 ) ) ;
#53031 = CONICAL_SURFACE ( 'NONE', #20444, 65.00000000000000000, 0.7853981633974497223 ) ;
#53032 = CARTESIAN_POINT ( 'NONE',  ( -7.336760511143403107, 6.859209474528208617, -23.57352014148015584 ) ) ;
#53033 = CARTESIAN_POINT ( 'NONE',  ( 203.1414537950835779, 105.9225671689748225, -9.634034691959321606 ) ) ;
#53034 = AXIS2_PLACEMENT_3D ( 'NONE', #64686, #27383, #54812 ) ;
#53035 = CARTESIAN_POINT ( 'NONE',  ( -142.1225587277077409, 58.16021019177119200, 90.55535391989825200 ) ) ;
#53036 = EDGE_CURVE ( 'NONE', #9288, #42925, #3130, .T. ) ;
#53037 = CARTESIAN_POINT ( 'NONE',  ( 136.9934874058118055, 43.35050367224292245, 43.83853296350712014 ) ) ;
#53038 = EDGE_CURVE ( 'NONE', #308, #28975, #29498, .T. ) ;
#53039 = ORIENTED_EDGE ( 'NONE', *, *, #3880, .T. ) ;
#53040 = DIRECTION ( 'NONE',  ( -1.156482317317871232E-16, -0.000000000000000000, -1.000000000000000000 ) ) ;
#53041 = CARTESIAN_POINT ( 'NONE',  ( -53.60725281709859757, -37.40286400928327026, 43.58025477438756212 ) ) ;
#53042 = EDGE_CURVE ( 'NONE', #11991, #66081, #24591, .T. ) ;
#53043 = CARTESIAN_POINT ( 'NONE',  ( 153.2523375521184335, 55.69936538551847605, 30.70342358034734787 ) ) ;
#53044 = DIRECTION ( 'NONE',  ( -0.000000000000000000, 1.000000000000000000, -0.000000000000000000 ) ) ;
#53045 = ORIENTED_EDGE ( 'NONE', *, *, #32383, .T. ) ;
#53046 = CARTESIAN_POINT ( 'NONE',  ( -58.33959211650994803, -29.48226216511402242, 41.38025477438755928 ) ) ;
#53047 = VERTEX_POINT ( 'NONE', #41101 ) ;
#53048 = LINE ( 'NONE', #58002, #5280 ) ;
#53049 = CARTESIAN_POINT ( 'NONE',  ( 63.49940197359692462, 12.78497925206076502, -77.56524142263349120 ) ) ;
#53050 = DIRECTION ( 'NONE',  ( 1.000000000000000000, 0.000000000000000000, 0.000000000000000000 ) ) ;
#53052 = ORIENTED_EDGE ( 'NONE', *, *, #45896, .T. ) ;
#53051 = CARTESIAN_POINT ( 'NONE',  ( 150.7770046255792522, 53.87214803240242844, 13.45895202400941848 ) ) ;
#53053 = CARTESIAN_POINT ( 'NONE',  ( -176.3791001330698975, 90.82833141237287577, 45.09165477967572855 ) ) ;
#53054 = CARTESIAN_POINT ( 'NONE',  ( 0.000000000000000000, 9.237604307034020579, -9.500000000000000000 ) ) ;
#53055 = CARTESIAN_POINT ( 'NONE',  ( -7.486743542469090684, -64.58150799671139453, 170.0000000000000000 ) ) ;
#53056 = ORIENTED_EDGE ( 'NONE', *, *, #5241, .F. ) ;
#53057 = DIRECTION ( 'NONE',  ( -0.000000000000000000, 1.000000000000000000, -0.000000000000000000 ) ) ;
#53058 = CARTESIAN_POINT ( 'NONE',  ( 6.400000000000000355, -4.618802153517012954, -8.000000000000001776 ) ) ;
#53059 = CARTESIAN_POINT ( 'NONE',  ( -175.9864315813574933, 91.91454246454364352, 31.37775927267171738 ) ) ;
#53060 = CARTESIAN_POINT ( 'NONE',  ( -37.92542950990690542, 10.74638084523341774, -73.43514582413676806 ) ) ;
#53061 = CARTESIAN_POINT ( 'NONE',  ( 186.2651679807462699, 84.00458780104314371, -22.32374867702027998 ) ) ;
#53062 = ORIENTED_EDGE ( 'NONE', *, *, #8768, .F. ) ;
#53063 = CARTESIAN_POINT ( 'NONE',  ( 46.23113030541875901, 10.41513832761375902, 13.67933782382501917 ) ) ;
#53064 = ORIENTED_EDGE ( 'NONE', *, *, #34550, .T. ) ;
#53065 = TOROIDAL_SURFACE ( 'NONE', #1417, 24.69999999999999929, 0.3000000000000035971 ) ;
#53066 = SURFACE_SIDE_STYLE ('',( #27377 ) ) ;
#53067 = CARTESIAN_POINT ( 'NONE',  ( -52.00013736311785806, 13.88364424352426774, 84.62652642927972124 ) ) ;
#53068 = CARTESIAN_POINT ( 'NONE',  ( 105.4134760436918583, 27.80903124201758203, 42.87025001487361209 ) ) ;
#53069 = AXIS2_PLACEMENT_3D ( 'NONE', #53756, #298, #31631 ) ;
#53070 = DIRECTION ( 'NONE',  ( 0.000000000000000000, 0.000000000000000000, 1.000000000000000000 ) ) ;
#53071 = PLANE ( 'NONE',  #29201 ) ;
#53072 = CARTESIAN_POINT ( 'NONE',  ( 182.7745872728868051, 81.77554423487157464, 17.32141904578063318 ) ) ;
#53073 = CARTESIAN_POINT ( 'NONE',  ( 212.0850679406003678, 117.0583048437722340, -42.48649401792513203 ) ) ;
#53075 = PLANE ( 'NONE',  #53422 ) ;
#53074 = AXIS2_PLACEMENT_3D ( 'NONE', #19469, #45161, #51145 ) ;
#53076 = ORIENTED_EDGE ( 'NONE', *, *, #32234, .T. ) ;
#53077 = CARTESIAN_POINT ( 'NONE',  ( 412.3372781065086201, 400.0000000000000568, -146.4497041420118251 ) ) ;
#53078 = EDGE_LOOP ( 'NONE', ( #9726, #34098, #35281, #2946 ) ) ;
#53079 = CIRCLE ( 'NONE', #4792, 185.0000000000000000 ) ;
#53080 = DIRECTION ( 'NONE',  ( -1.000000000000000000, 0.000000000000000000, 0.000000000000000000 ) ) ;
#53081 = DIRECTION ( 'NONE',  ( -0.000000000000000000, 1.000000000000000000, -0.000000000000000000 ) ) ;
#53082 = CARTESIAN_POINT ( 'NONE',  ( 55.76066037845577483, 11.10616952318092032, -72.03042357651290217 ) ) ;
#53083 = DIRECTION ( 'NONE',  ( 1.000000000000000000, 0.000000000000000000, 0.000000000000000000 ) ) ;
#53084 = PLANE ( 'NONE',  #4192 ) ;
#53085 = CARTESIAN_POINT ( 'NONE',  ( 0.000000000000000000, 0.000000000000000000, 170.0000000000000000 ) ) ;
#53086 = AXIS2_PLACEMENT_3D ( 'NONE', #14514, #18409, #14173 ) ;
#53087 = CARTESIAN_POINT ( 'NONE',  ( 149.4165763529819344, -26.99999999999998224, 138.9999999999999716 ) ) ;
#53088 = ORIENTED_EDGE ( 'NONE', *, *, #13251, .F. ) ;
#53089 = CARTESIAN_POINT ( 'NONE',  ( -74.79002408692174697, 20.88280597089420709, 71.18791309357050068 ) ) ;
#53090 = CARTESIAN_POINT ( 'NONE',  ( 198.3695851305816973, 98.05090906089078828, -93.48290386845097544 ) ) ;
#53091 = ORIENTED_EDGE ( 'NONE', *, *, #34475, .T. ) ;
#53092 = ORIENTED_EDGE ( 'NONE', *, *, #48705, .F. ) ;
#53094 = EDGE_CURVE ( 'NONE', #8293, #46372, #67164, .T. ) ;
#53093 = CARTESIAN_POINT ( 'NONE',  ( -155.2912910578197057, 69.24479901948498650, 43.00208789238233464 ) ) ;
#53095 = CARTESIAN_POINT ( 'NONE',  ( 55.51597771111714508, 11.05737652677076177, -42.72098034633929586 ) ) ;
#53096 = DIRECTION ( 'NONE',  ( 0.000000000000000000, -1.000000000000000000, 0.000000000000000000 ) ) ;
#53097 = CARTESIAN_POINT ( 'NONE',  ( 0.000000000000000000, 0.000000000000000000, 170.0000000000000000 ) ) ;
#53098 = CARTESIAN_POINT ( 'NONE',  ( -55.05276343752910151, -170.0000000000000000, -88.90542517938720835 ) ) ;
#53099 = ADVANCED_FACE ( 'NONE', ( #24926 ), #13336, .F. ) ;
#53100 = VERTEX_POINT ( 'NONE', #68190 ) ;
#53101 = EDGE_CURVE ( 'NONE', #20867, #5511, #52342, .T. ) ;
#53102 = ORIENTED_EDGE ( 'NONE', *, *, #36250, .T. ) ;
#53103 = CARTESIAN_POINT ( 'NONE',  ( -132.0738857626834033, 51.93126104279146205, 33.86320823520932066 ) ) ;
#53104 = ORIENTED_EDGE ( 'NONE', *, *, #46533, .T. ) ;
#53105 = DIRECTION ( 'NONE',  ( -0.000000000000000000, 0.000000000000000000, -1.000000000000000000 ) ) ;
#53106 = CARTESIAN_POINT ( 'NONE',  ( -144.9417090887490929, 61.69631066549397502, 32.26605393151823620 ) ) ;
#53107 = CARTESIAN_POINT ( 'NONE',  ( 56.30171512200996631, 11.21502580416396100, 67.50933623815409135 ) ) ;
#53108 = CARTESIAN_POINT ( 'NONE',  ( -41.43037391101678679, 4.983853614416524636, 13.79046340968177731 ) ) ;
#53109 = DIRECTION ( 'NONE',  ( -1.000000000000000000, 0.000000000000000000, 0.000000000000000000 ) ) ;
#53110 = LINE ( 'NONE', #26406, #47264 ) ;
#53111 = EDGE_CURVE ( 'NONE', #59242, #38638, #66813, .T. ) ;
#53112 = VERTEX_POINT ( 'NONE', #35828 ) ;
#53113 = ORIENTED_EDGE ( 'NONE', *, *, #43804, .F. ) ;
#53114 = CARTESIAN_POINT ( 'NONE',  ( 111.6139602183311155, -21.48286796535249721, 4.743729604094153451 ) ) ;
#53115 = CARTESIAN_POINT ( 'NONE',  ( -62.66631205405186478, 18.59153367093363229, 43.58025477438756212 ) ) ;
#53116 = CARTESIAN_POINT ( 'NONE',  ( -169.8842709557925161, 83.59602878049477681, -22.14760816498463214 ) ) ;
#53117 = CARTESIAN_POINT ( 'NONE',  ( 429.8372781065084496, 400.0000000000042633, 96.05029585798401115 ) ) ;
#53118 = DIRECTION ( 'NONE',  ( -0.8160245890732938934, -0.5780171883497599028, 0.000000000000000000 ) ) ;
#53119 = CARTESIAN_POINT ( 'NONE',  ( 22.46018177512842584, 7.813889158582806083, 87.76227202242357350 ) ) ;
#53120 = CIRCLE ( 'NONE', #29539, 65.36598343705435354 ) ;
#53121 = ORIENTED_EDGE ( 'NONE', *, *, #53818, .F. ) ;
#53122 = CYLINDRICAL_SURFACE ( 'NONE', #23622, 27.00000000000000000 ) ;
#53123 = DIRECTION ( 'NONE',  ( 1.000000000000000000, 0.000000000000000000, 0.000000000000000000 ) ) ;
#53124 = EDGE_LOOP ( 'NONE', ( #13916, #9563, #61752, #57394 ) ) ;
#53125 = CIRCLE ( 'NONE', #3742, 66.50000000000000000 ) ;
#53126 = CARTESIAN_POINT ( 'NONE',  ( -85.75947274862031122, 25.15128705015480648, 8.585276764537949745 ) ) ;
#53127 = EDGE_LOOP ( 'NONE', ( #60139, #51924, #32702, #65204 ) ) ;
#53128 = AXIS2_PLACEMENT_3D ( 'NONE', #16263, #52848, #4670 ) ;
#53129 = VECTOR ( 'NONE', #33653, 1000.000000000000114 ) ;
#53130 = ORIENTED_EDGE ( 'NONE', *, *, #43591, .F. ) ;
#53131 = CARTESIAN_POINT ( 'NONE',  ( 13.84120792123769128, 6.445822122644895735, -50.27834514783636166 ) ) ;
#53132 = CARTESIAN_POINT ( 'NONE',  ( -173.9656771507955000, 88.06879734510549440, 72.66624519710475738 ) ) ;
#53133 = CARTESIAN_POINT ( 'NONE',  ( 126.3580543567275640, 37.07735301062819389, 64.15879660461148148 ) ) ;
#53134 = EDGE_LOOP ( 'NONE', ( #45882, #58791, #1629, #12659, #24053 ) ) ;
#53135 = CARTESIAN_POINT ( 'NONE',  ( -38.33502649974140297, 10.82522693986058471, 94.42607965810407222 ) ) ;
#53136 = DIRECTION ( 'NONE',  ( -0.000000000000000000, 0.000000000000000000, 1.000000000000000000 ) ) ;
#53137 = FACE_OUTER_BOUND ( 'NONE', #35863, .T. ) ;
#53138 = CARTESIAN_POINT ( 'NONE',  ( 102.7551177910568612, 25.56939188780864924, -43.91997128112426196 ) ) ;
#53139 = CARTESIAN_POINT ( 'NONE',  ( -29.02794087136069834, 9.207646203414352470, 44.83495968200595172 ) ) ;
#53140 = DIRECTION ( 'NONE',  ( 1.000000000000000000, 0.000000000000000000, 0.000000000000000000 ) ) ;
#53141 = ORIENTED_EDGE ( 'NONE', *, *, #16250, .F. ) ;
#53142 = CARTESIAN_POINT ( 'NONE',  ( 46.66904755831210139, -9.150666335777657423E-14, 2.000000000000001776 ) ) ;
#53143 = CARTESIAN_POINT ( 'NONE',  ( -0.6527133886630317461, 8.860760056385744932, -9.003039949738242953 ) ) ;
#53144 = CARTESIAN_POINT ( 'NONE',  ( -3.792733964105130084, 6.661044795567934607, -90.22612808589047972 ) ) ;
#53145 = CARTESIAN_POINT ( 'NONE',  ( -118.3948752128398922, 42.92869324237091888, -42.11633704353932472 ) ) ;
#53146 = EDGE_CURVE ( 'NONE', #56869, #67388, #14017, .T. ) ;
#53147 = DIRECTION ( 'NONE',  ( -0.8160245890732938934, -0.5780171883497599028, 0.000000000000000000 ) ) ;
#53148 = DIRECTION ( 'NONE',  ( 0.000000000000000000, 0.000000000000000000, -1.000000000000000000 ) ) ;
#53149 = CARTESIAN_POINT ( 'NONE',  ( -155.1355020251929488, 69.10372769512068203, 6.393537426473839602 ) ) ;
#53150 = CARTESIAN_POINT ( 'NONE',  ( 197.5084910509550298, 98.58493024928847603, 92.57377601736234851 ) ) ;
#53151 = CARTESIAN_POINT ( 'NONE',  ( 68.95451040317568925, 14.12887482153123742, 15.07515996775212841 ) ) ;
#53152 = CARTESIAN_POINT ( 'NONE',  ( -15.45727656667583005, -73.34020256436187424, 41.38025477438755928 ) ) ;
#53153 = CARTESIAN_POINT ( 'NONE',  ( 90.30840373526895348, 21.77864858272153725, -23.01712743521610349 ) ) ;
#53155 = ORIENTED_EDGE ( 'NONE', *, *, #17966, .T. ) ;
#53154 = EDGE_CURVE ( 'NONE', #56804, #26121, #35477, .T. ) ;
#53156 = VECTOR ( 'NONE', #28290, 1000.000000000000000 ) ;
#53157 = CONTEXT_DEPENDENT_SHAPE_REPRESENTATION ( #41340, #67061 ) ;
#53158 = CARTESIAN_POINT ( 'NONE',  ( -50.13240733217616452, 14.45347886670807647, 85.83683214817698115 ) ) ;
#53159 = ORIENTED_EDGE ( 'NONE', *, *, #17946, .F. ) ;
#53160 = DIRECTION ( 'NONE',  ( -0.000000000000000000, 1.000000000000000000, -0.000000000000000000 ) ) ;
#53161 = ORIENTED_EDGE ( 'NONE', *, *, #63925, .F. ) ;
#53162 = CARTESIAN_POINT ( 'NONE',  ( 21.44191228441539110, 7.755009954762316582, -74.81642095281917193 ) ) ;
#53163 = MECHANICAL_DESIGN_GEOMETRIC_PRESENTATION_REPRESENTATION (  '', ( #36372 ), #21736 ) ;
#53164 = LINE ( 'NONE', #30703, #49580 ) ;
#53165 = CARTESIAN_POINT ( 'NONE',  ( -142.0729208125266325, 59.40063722436775606, 66.20298747330664924 ) ) ;
#53166 = CARTESIAN_POINT ( 'NONE',  ( 69.08240197259641491, 14.16210831900843736, -20.79263225278958771 ) ) ;
#53167 = CARTESIAN_POINT ( 'NONE',  ( -71.28077210551055032, 19.64439276383075850, -95.00000000000133582 ) ) ;
#53168 = CARTESIAN_POINT ( 'NONE',  ( -47.55256438668344998, 13.83151366677316751, -69.80307781500179942 ) ) ;
#53169 = AXIS2_PLACEMENT_3D ( 'NONE', #35111, #44266, #56219 ) ;
#53170 = CARTESIAN_POINT ( 'NONE',  ( 410.0000000000000000, 0.000000000000000000, -2.000000000000000000 ) ) ;
#53171 = FACE_OUTER_BOUND ( 'NONE', #26953, .T. ) ;
#53172 = ORIENTED_EDGE ( 'NONE', *, *, #10644, .T. ) ;
#53173 = ADVANCED_FACE ( 'NONE', ( #30893 ), #13670, .F. ) ;
#53174 = VERTEX_POINT ( 'NONE', #67841 ) ;
#53175 = VECTOR ( 'NONE', #57464, 1000.000000000000000 ) ;
#53176 = EDGE_CURVE ( 'NONE', #67695, #44050, #52297, .T. ) ;
#53177 = CARTESIAN_POINT ( 'NONE',  ( 178.9724693410834391, 77.91338280736979982, 83.29495941411636295 ) ) ;
#53178 = DIRECTION ( 'NONE',  ( 0.000000000000000000, 0.000000000000000000, -1.000000000000000000 ) ) ;
#53179 = DIRECTION ( 'NONE',  ( -0.000000000000000000, -0.000000000000000000, -1.000000000000000000 ) ) ;
#53180 = AXIS2_PLACEMENT_3D ( 'NONE', #38308, #60469, #10884 ) ;
#53181 = ADVANCED_FACE ( 'NONE', ( #34792 ), #9094, .F. ) ;
#53182 = CARTESIAN_POINT ( 'NONE',  ( 70.02150084181303669, 15.44810330738962634, -94.20035217677271078 ) ) ;
#53183 = CARTESIAN_POINT ( 'NONE',  ( 285.0001299725262243, 22.00002953920830606, 0.3279435515783846178 ) ) ;
#53184 = CARTESIAN_POINT ( 'NONE',  ( -9.525868120571908904, 7.007646177566257073, 71.76889433962945475 ) ) ;
#53185 = CARTESIAN_POINT ( 'NONE',  ( -81.23297981660235223, 23.31577157498398378, -8.719607575958333356 ) ) ;
#53186 = DIRECTION ( 'NONE',  ( 1.000000000000000000, 0.000000000000000000, 0.000000000000000000 ) ) ;
#53187 = CARTESIAN_POINT ( 'NONE',  ( 46.66904755831212981, 15.55634918610394379, 0.000000000000000000 ) ) ;
#53188 = CARTESIAN_POINT ( 'NONE',  ( 86.62931800182293784, -170.0000000000000000, -89.51066537983906812 ) ) ;
#53189 = CARTESIAN_POINT ( 'NONE',  ( 105.0001309909291365, 21.99997022933652246, 0.3293293811575764285 ) ) ;
#53190 = CARTESIAN_POINT ( 'NONE',  ( 160.2883311361770211, 61.16711613734478448, 70.70813550747246268 ) ) ;
#53191 =( BOUNDED_CURVE ( )  B_SPLINE_CURVE ( 3, ( #59601, #7570, #50466, #2287 ),
 .UNSPECIFIED., .F., .F. ) 
 B_SPLINE_CURVE_WITH_KNOTS ( ( 4, 4 ),
 ( 2.506209174768084580, 3.776976132411493658 ),
 .UNSPECIFIED. ) 
 CURVE ( )  GEOMETRIC_REPRESENTATION_ITEM ( )  RATIONAL_B_SPLINE_CURVE ( ( 1.000000000000000000, 0.8698961108463049152, 0.8698961108463049152, 1.000000000000000000 ) ) 
 REPRESENTATION_ITEM ( '' )  );
#53192 = ADVANCED_FACE ( 'NONE', ( #21702 ), #43151, .T. ) ;
#53193 = ORIENTED_EDGE ( 'NONE', *, *, #15624, .T. ) ;
#53194 = CARTESIAN_POINT ( 'NONE',  ( -124.3250225421925848, 45.46958056770282752, -35.07612196727420439 ) ) ;
#53195 = LINE ( 'NONE', #31087, #64230 ) ;
#53196 = LINE ( 'NONE', #63085, #37466 ) ;
#53197 = DIRECTION ( 'NONE',  ( -0.000000000000000000, 1.000000000000000000, -0.000000000000000000 ) ) ;
#53198 = CARTESIAN_POINT ( 'NONE',  ( 150.4550062612853765, 52.39582885725847206, 12.76969944096150478 ) ) ;
#53199 = EDGE_CURVE ( 'NONE', #13968, #37838, #21358, .T. ) ;
#53200 = ADVANCED_FACE ( 'NONE', ( #68520 ), #47737, .F. ) ;
#53201 = DIRECTION ( 'NONE',  ( 0.000000000000000000, 0.000000000000000000, 1.000000000000000000 ) ) ;
#53202 = ADVANCED_FACE ( 'NONE', ( #20326 ), #36860, .T. ) ;
#53203 = ORIENTED_EDGE ( 'NONE', *, *, #534, .F. ) ;
#53204 = CARTESIAN_POINT ( 'NONE',  ( -3.476223215531647803E-15, 7.124194613927619990, 3.660532965668822580 ) ) ;
#53205 = VERTEX_POINT ( 'NONE', #16081 ) ;
#53206 = EDGE_LOOP ( 'NONE', ( #5997, #26843, #16999, #50031 ) ) ;
#53207 = VECTOR ( 'NONE', #13089, 1000.000000000000000 ) ;
#53208 = CARTESIAN_POINT ( 'NONE',  ( 266.9165763529819628, -52.00000000000000711, 128.9999999999999716 ) ) ;
#53209 = DIRECTION ( 'NONE',  ( -1.850169831522831466E-16, 1.000000000000000000, 1.110223024625156294E-16 ) ) ;
#53210 = CARTESIAN_POINT ( 'NONE',  ( 109.9975424824652634, 18.00000000000002842, 401.6295345748407613 ) ) ;
#53211 = VERTEX_POINT ( 'NONE', #31576 ) ;
#53212 = CARTESIAN_POINT ( 'NONE',  ( -60.66241560458682613, 16.25736033771447708, -74.56350396580954509 ) ) ;
#53213 = DIRECTION ( 'NONE',  ( -0.000000000000000000, -0.000000000000000000, -1.000000000000000000 ) ) ;
#53214 = CIRCLE ( 'NONE', #21789, 195.0000000000000000 ) ;
#53215 = CARTESIAN_POINT ( 'NONE',  ( 34.83825437341838693, 7.859462995505738014, -22.24695001896300539 ) ) ;
#53216 = CARTESIAN_POINT ( 'NONE',  ( 179.4074606910091632, 78.34362448405029511, -36.36429642586875843 ) ) ;
#53217 = CARTESIAN_POINT ( 'NONE',  ( -5.354491962338125965, 6.146186931204403514, -9.431901280394573206 ) ) ;
#53218 = AXIS2_PLACEMENT_3D ( 'NONE', #67934, #3219, #67581 ) ;
#53219 = PLANE ( 'NONE',  #1682 ) ;
#53220 = AXIS2_PLACEMENT_3D ( 'NONE', #41433, #15388, #36154 ) ;
#53221 = ORIENTED_EDGE ( 'NONE', *, *, #27751, .T. ) ;
#53222 = VECTOR ( 'NONE', #7488, 1000.000000000000000 ) ;
#53223 = FILL_AREA_STYLE_COLOUR ( '', #6490 ) ;
#53224 = CIRCLE ( 'NONE', #47605, 20.00000000000000000 ) ;
#53225 = DIRECTION ( 'NONE',  ( -0.8160245890732938934, -0.5780171883497599028, 0.000000000000000000 ) ) ;
#53226 = CARTESIAN_POINT ( 'NONE',  ( 14.08810621383467065, 7.458732232275139928, 30.20580324848959464 ) ) ;
#53227 = CARTESIAN_POINT ( 'NONE',  ( 198.4045886930829568, 99.71425793793709147, 32.61891997574733182 ) ) ;
#53228 = CARTESIAN_POINT ( 'NONE',  ( 55.14772863908626732, 34.40534879854737227, 170.0000000000000000 ) ) ;
#53230 = VERTEX_POINT ( 'NONE', #10806 ) ;
#53229 = CARTESIAN_POINT ( 'NONE',  ( -74.99999999999998579, 9.184850993605147156E-15, 25.00000000000007816 ) ) ;
#53231 = EDGE_LOOP ( 'NONE', ( #9271, #65433, #36859, #40386, #56315, #65991, #52129, #60706, #33013, #66826, #25559, #57919, #25001, #27373, #50774 ) ) ;
#53232 = VECTOR ( 'NONE', #55278, 1000.000000000000000 ) ;
#53233 = ORIENTED_EDGE ( 'NONE', *, *, #53338, .T. ) ;
#53234 =( NAMED_UNIT ( * ) SI_UNIT ( $, .STERADIAN. ) SOLID_ANGLE_UNIT ( ) );
#53235 = CARTESIAN_POINT ( 'NONE',  ( 412.3372781065085633, 179.4906275429376024, -144.4497041420117682 ) ) ;
#53236 = EDGE_CURVE ( 'NONE', #23774, #19589, #68801, .T. ) ;
#53237 = CARTESIAN_POINT ( 'NONE',  ( 99.71998884745383407, 188.0000000000000000, -23.09547038499562888 ) ) ;
#53238 = CARTESIAN_POINT ( 'NONE',  ( -33.83721310978699393, 11.01869210665941523, 57.45054862161848774 ) ) ;
#53239 = CARTESIAN_POINT ( 'NONE',  ( -13.79190010541702982, 8.363435739308560102, -11.50286335269423788 ) ) ;
#53240 = CARTESIAN_POINT ( 'NONE',  ( 155.7277429502854318, 56.30804678861343149, -77.77684271661371440 ) ) ;
#53241 = DIRECTION ( 'NONE',  ( -1.000000000000000000, 0.000000000000000000, 0.000000000000000000 ) ) ;
#53242 = ADVANCED_FACE ( 'NONE', ( #5528 ), #28392, .T. ) ;
#53243 = LINE ( 'NONE', #5068, #25054 ) ;
#53244 = ORIENTED_EDGE ( 'NONE', *, *, #44386, .F. ) ;
#53245 = ORIENTED_EDGE ( 'NONE', *, *, #67684, .T. ) ;
#53246 = CARTESIAN_POINT ( 'NONE',  ( 70.12389542974196388, 15.47520081968154848, -18.81922647478308619 ) ) ;
#53247 = CARTESIAN_POINT ( 'NONE',  ( -80.31482177285907653, 24.03632224640839254, -49.93594921041977130 ) ) ;
#53248 = CARTESIAN_POINT ( 'NONE',  ( 158.3604774538084428, 58.34594647925809596, 71.21437032374478804 ) ) ;
#53249 = CARTESIAN_POINT ( 'NONE',  ( -156.4966862384868307, 71.70877417666511633, 14.14904641178471323 ) ) ;
#53250 = CARTESIAN_POINT ( 'NONE',  ( 182.7789203043889756, 80.33475476315295793, -36.40670569473370222 ) ) ;
#53251 = CARTESIAN_POINT ( 'NONE',  ( 23.28869764673362397, 6.856674305776598644, 38.00306743024603406 ) ) ;
#53252 = CARTESIAN_POINT ( 'NONE',  ( -156.1162923254352961, 71.35845171916716367, 88.34953077652313880 ) ) ;
#53253 = VERTEX_POINT ( 'NONE', #58301 ) ;
#53254 = EDGE_CURVE ( 'NONE', #68965, #47435, #63254, .T. ) ;
#53255 = EDGE_LOOP ( 'NONE', ( #50539, #58336, #44637, #8246, #17399, #20605, #51193, #18101, #31137 ) ) ;
#53256 = ORIENTED_EDGE ( 'NONE', *, *, #8961, .T. ) ;
#53257 = EDGE_CURVE ( 'NONE', #41387, #47508, #66626, .T. ) ;
#53258 = CARTESIAN_POINT ( 'NONE',  ( -452.6627218934912662, 399.9999999999953957, 113.5502958579925661 ) ) ;
#53259 = CARTESIAN_POINT ( 'NONE',  ( 32.38493285958205092, 8.611594965040671568, -45.77910956698918454 ) ) ;
#53260 = CARTESIAN_POINT ( 'NONE',  ( 179.0096185093687779, 76.53352131383246615, 56.43267003127355963 ) ) ;
#53261 = EDGE_CURVE ( 'NONE', #56288, #47772, #52000, .T. ) ;
#53262 = CIRCLE ( 'NONE', #22964, 10.00000000000000178 ) ;
#53263 = CARTESIAN_POINT ( 'NONE',  ( -37.79823708645147917, 10.72197716414928870, 60.57713633437269607 ) ) ;
#53264 = CARTESIAN_POINT ( 'NONE',  ( -152.9119739516381458, 67.12135129037709191, -22.16650931204297237 ) ) ;
#53265 = EDGE_LOOP ( 'NONE', ( #31152, #44671, #12503, #39415 ) ) ;
#53266 = AXIS2_PLACEMENT_3D ( 'NONE', #46026, #39716, #39368 ) ;
#53267 = CARTESIAN_POINT ( 'NONE',  ( 186.2575601542430377, 85.47765906955505955, 69.08854037509910029 ) ) ;
#53268 = CARTESIAN_POINT ( 'NONE',  ( 45.80999061969644970, 9.329701754959341287, 94.99999999999866418 ) ) ;
#53269 =( LENGTH_UNIT ( ) NAMED_UNIT ( * ) SI_UNIT ( .MILLI., .METRE. ) );
#53270 = CARTESIAN_POINT ( 'NONE',  ( 15.78827728214693060, 7.507518794609573831, 18.17015708224157322 ) ) ;
#53271 = CARTESIAN_POINT ( 'NONE',  ( 186.2722199822849518, 84.01218714714249813, 69.08924636671144981 ) ) ;
#53272 = DIRECTION ( 'NONE',  ( 9.899279560275165216E-15, -1.665334536937735057E-16, 1.000000000000000000 ) ) ;
#53273 = CARTESIAN_POINT ( 'NONE',  ( -85.34215807311494473, 24.97769003780924635, -39.18790712996867853 ) ) ;
#53274 = VECTOR ( 'NONE', #38663, 1000.000000000000000 ) ;
#53275 = CARTESIAN_POINT ( 'NONE',  ( 19.53470118933705280, 6.649487981843461348, 57.85738236312793248 ) ) ;
#53276 = FACE_OUTER_BOUND ( 'NONE', #20266, .T. ) ;
#53277 = CARTESIAN_POINT ( 'NONE',  ( 200.8298320869470217, 101.1869877914233626, 57.11224534795069729 ) ) ;
#53278 = ORIENTED_EDGE ( 'NONE', *, *, #32863, .T. ) ;
#53279 = CARTESIAN_POINT ( 'NONE',  ( 183.1910712700538397, 80.76073941711163684, 17.17481853169963912 ) ) ;
#53280 = CARTESIAN_POINT ( 'NONE',  ( 173.7246046907418986, 71.47482343504563573, 38.28278645884536502 ) ) ;
#53281 = CARTESIAN_POINT ( 'NONE',  ( -133.1093894320205777, 51.43221067881454189, -44.53048774310489932 ) ) ;
#53282 = EDGE_CURVE ( 'NONE', #17365, #43631, #10118, .T. ) ;
#53283 = CARTESIAN_POINT ( 'NONE',  ( -102.2801239173131194, 33.91021738430207222, -35.01457726497591239 ) ) ;
#53284 = ADVANCED_FACE ( 'NONE', ( #58636 ), #9783, .F. ) ;
#53285 = CARTESIAN_POINT ( 'NONE',  ( 57.57684776206772170, 12.50442334002048561, -75.23527395922451433 ) ) ;
#53286 = ORIENTED_EDGE ( 'NONE', *, *, #32135, .T. ) ;
#53287 = EDGE_LOOP ( 'NONE', ( #53607, #65012 ) ) ;
#53288 = EDGE_CURVE ( 'NONE', #14559, #12765, #963, .T. ) ;
#53289 = ADVANCED_BREP_SHAPE_REPRESENTATION ( '', ( #65002, #66832 ), #63539 ) ;
#53290 = DIRECTION ( 'NONE',  ( -0.000000000000000000, -0.000000000000000000, 1.000000000000000000 ) ) ;
#53291 = CARTESIAN_POINT ( 'NONE',  ( 173.5758067325220395, 71.33673452833791373, 90.29149762729994677 ) ) ;
#53292 = ORIENTED_EDGE ( 'NONE', *, *, #44454, .T. ) ;
#53293 = CARTESIAN_POINT ( 'NONE',  ( 0.000000000000000000, 0.000000000000000000, 0.000000000000000000 ) ) ;
#53294 = ORIENTED_EDGE ( 'NONE', *, *, #44284, .T. ) ;
#53295 = CARTESIAN_POINT ( 'NONE',  ( 26.11269837220812562, 36.11269837220800838, 85.00100000000000477 ) ) ;
#53296 = CARTESIAN_POINT ( 'NONE',  ( 129.6961120139403647, 38.96846414226718736, 30.76564539126953335 ) ) ;
#53297 = CARTESIAN_POINT ( 'NONE',  ( 0.000000000000000000, 50.00000000000000000, 0.000000000000000000 ) ) ;
#53298 = DIRECTION ( 'NONE',  ( -1.000000000000000000, 0.000000000000000000, 0.000000000000000000 ) ) ;
#53299 = CARTESIAN_POINT ( 'NONE',  ( 93.61951000632932107, 21.92572933971849380, -46.05087944202944072 ) ) ;
#53301 = ORIENTED_EDGE ( 'NONE', *, *, #23229, .F. ) ;
#53300 = LINE ( 'NONE', #59277, #67929 ) ;
#53302 = ORIENTED_EDGE ( 'NONE', *, *, #18054, .F. ) ;
#53303 = EDGE_LOOP ( 'NONE', ( #52302, #61588, #28269, #28578 ) ) ;
#53304 = CARTESIAN_POINT ( 'NONE',  ( -118.8689810167775676, 42.03922634358558952, -18.20944547944688452 ) ) ;
#53305 = FACE_BOUND ( 'NONE', #60069, .T. ) ;
#53306 = CARTESIAN_POINT ( 'NONE',  ( 26.99999999999999645, 0.000000000000000000, 12.00000000000000000 ) ) ;
#53307 = DIRECTION ( 'NONE',  ( 0.000000000000000000, 0.000000000000000000, 1.000000000000000000 ) ) ;
#53308 = AXIS2_PLACEMENT_3D ( 'NONE', #5554, #64300, #33607 ) ;
#53310 = ORIENTED_EDGE ( 'NONE', *, *, #2005, .F. ) ;
#53309 = CARTESIAN_POINT ( 'NONE',  ( -146.5341851369306028, 61.69744206542952014, -49.21242434289558076 ) ) ;
#53311 = CARTESIAN_POINT ( 'NONE',  ( 61.33840119549016379, 13.32121602003046945, 3.154318263180942772 ) ) ;
#53312 = AXIS2_PLACEMENT_3D ( 'NONE', #34336, #44874, #39944 ) ;
#53313 = AXIS2_PLACEMENT_3D ( 'NONE', #4163, #14708, #53013 ) ;
#53314 = ORIENTED_EDGE ( 'NONE', *, *, #63944, .F. ) ;
#53315 = CARTESIAN_POINT ( 'NONE',  ( -133.3926783185152090, 51.63401075114364858, 38.42124472836754023 ) ) ;
#53316 = CARTESIAN_POINT ( 'NONE',  ( -58.33245019990695113, 15.58496056636070293, -9.109388937163927835 ) ) ;
#53317 = VECTOR ( 'NONE', #61083, 1000.000000000000000 ) ;
#53318 = VECTOR ( 'NONE', #10401, 1000.000000000000000 ) ;
#53319 = CARTESIAN_POINT ( 'NONE',  ( 49.99999999999998579, -19.99999999999996447, 1.999999999999984457 ) ) ;
#53320 = CARTESIAN_POINT ( 'NONE',  ( 135.0005116824453921, 43.29964618809725607, 29.59450486721033258 ) ) ;
#53321 = ADVANCED_FACE ( 'NONE', ( #12551 ), #6575, .F. ) ;
#53322 = CARTESIAN_POINT ( 'NONE',  ( -190.6985136298601731, 109.1272424661242582, -95.00000000000133582 ) ) ;
#53323 = AXIS2_PLACEMENT_3D ( 'NONE', #62116, #52597, #45945 ) ;
#53324 = CARTESIAN_POINT ( 'NONE',  ( -95.63568360745007624, 29.53168204475775838, 7.686534007699536097 ) ) ;
#53325 = CARTESIAN_POINT ( 'NONE',  ( -153.4231522284453320, 67.57115137896495582, -89.54656928398240723 ) ) ;
#53326 = ORIENTED_EDGE ( 'NONE', *, *, #40419, .F. ) ;
#53327 = ORIENTED_EDGE ( 'NONE', *, *, #36274, .T. ) ;
#53328 = CARTESIAN_POINT ( 'NONE',  ( 188.5645326065591405, 86.51153908883290455, -71.18896735030770628 ) ) ;
#53329 = PLANE ( 'NONE',  #18292 ) ;
#53330 = LINE ( 'NONE', #5161, #8780 ) ;
#53331 = CARTESIAN_POINT ( 'NONE',  ( 26.69682282325795697, -59.27986298182186431, 41.38025477438755928 ) ) ;
#53332 = CARTESIAN_POINT ( 'NONE',  ( 102.7938674513918897, 26.67851209377773003, -69.25574476757175546 ) ) ;
#53333 = CARTESIAN_POINT ( 'NONE',  ( -78.66644367742109978, 23.39876645725290061, 45.41820113967312977 ) ) ;
#53334 = CARTESIAN_POINT ( 'NONE',  ( 85.67452303415194592, 19.09699411916382061, 44.66627896201372749 ) ) ;
#53335 = CARTESIAN_POINT ( 'NONE',  ( 63.01563776193091826, 13.70579113808095073, -50.72069083216976537 ) ) ;
#53336 = CARTESIAN_POINT ( 'NONE',  ( 43.96421756700841144, 10.06386361114660133, -49.09255290175231323 ) ) ;
#53337 = CARTESIAN_POINT ( 'NONE',  ( 210.1954643503415525, 114.1986276268024056, 68.65963326422985347 ) ) ;
#53338 = EDGE_CURVE ( 'NONE', #62136, #36801, #48763, .T. ) ;
#53339 = ORIENTED_EDGE ( 'NONE', *, *, #24976, .F. ) ;
#53340 = DIRECTION ( 'NONE',  ( 0.000000000000000000, 0.000000000000000000, 1.000000000000000000 ) ) ;
#53341 = ORIENTED_EDGE ( 'NONE', *, *, #61209, .F. ) ;
#53342 = CARTESIAN_POINT ( 'NONE',  ( -14.32120159453989494, 7.401444311907543039, -46.67511467244946033 ) ) ;
#53343 = CARTESIAN_POINT ( 'NONE',  ( 80.71682498289318630, 18.54204664833076066, 68.69748318965059752 ) ) ;
#53344 = EDGE_CURVE ( 'NONE', #36414, #4959, #44093, .T. ) ;
#53345 = CARTESIAN_POINT ( 'NONE',  ( 91.49210130311621469, 22.20929244416437598, 69.77178660558656986 ) ) ;
#53346 = DIRECTION ( 'NONE',  ( -0.000000000000000000, -0.000000000000000000, -1.000000000000000000 ) ) ;
#53347 = DIRECTION ( 'NONE',  ( 0.000000000000000000, 0.000000000000000000, 1.000000000000000000 ) ) ;
#53348 = EDGE_CURVE ( 'NONE', #32164, #22494, #5922, .T. ) ;
#53349 = CARTESIAN_POINT ( 'NONE',  ( 33.03722315490662709, 7.666819786578624729, -65.98931375990046888 ) ) ;
#53350 = LINE ( 'NONE', #20665, #52468 ) ;
#53351 = CARTESIAN_POINT ( 'NONE',  ( -13.90880041226882824, 35.72171523751327982, 13.32819397642331971 ) ) ;
#53352 = EDGE_LOOP ( 'NONE', ( #49985, #67121, #35476, #63123 ) ) ;
#53353 = DIRECTION ( 'NONE',  ( 1.000000000000000000, 0.000000000000000000, 0.000000000000000000 ) ) ;
#53354 = EDGE_LOOP ( 'NONE', ( #66472, #16755, #31196 ) ) ;
#53355 = CARTESIAN_POINT ( 'NONE',  ( 61.33840119549017089, 13.32121602003047478, 56.84341944410832781 ) ) ;
#53356 = CARTESIAN_POINT ( 'NONE',  ( 9.050324533885209632, 7.384616180193988022, -73.19382097837868173 ) ) ;
#53357 = FACE_OUTER_BOUND ( 'NONE', #18680, .T. ) ;
#53358 = CARTESIAN_POINT ( 'NONE',  ( 39.40195752203892710, 9.424259417798131366, 56.75838489642694640 ) ) ;
#53359 = CARTESIAN_POINT ( 'NONE',  ( -0.8055628312658249524, 6.535476276302842003, 34.96376056659171638 ) ) ;
#53360 = CARTESIAN_POINT ( 'NONE',  ( -94.77925136849377452, 29.13093715379786275, -15.43817801418533797 ) ) ;
#53361 = CARTESIAN_POINT ( 'NONE',  ( 79.12226143468465978, 18.04701779285957741, 90.79126889306922976 ) ) ;
#53362 = VECTOR ( 'NONE', #61317, 1000.000000000000000 ) ;
#53363 = ORIENTED_EDGE ( 'NONE', *, *, #54690, .F. ) ;
#53364 = VECTOR ( 'NONE', #67901, 1000.000000000000000 ) ;
#53365 = DIRECTION ( 'NONE',  ( -9.950807539071958118E-15, 1.000000000000000000, 4.024558464266191670E-15 ) ) ;
#53366 = CARTESIAN_POINT ( 'NONE',  ( 8.000000000000001776, -0.7805016046291016751, -9.500000000000005329 ) ) ;
#53367 = CARTESIAN_POINT ( 'NONE',  ( 173.9405361758638264, 73.05302209498819366, -14.57814776013407965 ) ) ;
#53368 = DIRECTION ( 'NONE',  ( -1.000000000000000000, 0.000000000000000000, -2.168404344971009361E-16 ) ) ;
#53369 = ITEM_DEFINED_TRANSFORMATION ( 'NONE', 'NONE', #13040,  #66832 ) ;
#53370 = CARTESIAN_POINT ( 'NONE',  ( -132.4776673493542773, 52.21763813822158085, -46.01489453234746207 ) ) ;
#53371 = ORIENTED_EDGE ( 'NONE', *, *, #69541, .F. ) ;
#53372 = CARTESIAN_POINT ( 'NONE',  ( -63.73419499958981049, -12.83646726144931449, 43.58025477438756923 ) ) ;
#53373 = CARTESIAN_POINT ( 'NONE',  ( -0.7174461528505726715, 6.532311451815525416, -13.66781165024909228 ) ) ;
#53374 = EDGE_CURVE ( 'NONE', #8997, #772, #13783, .T. ) ;
#53375 = CARTESIAN_POINT ( 'NONE',  ( 202.7506655727288774, 105.3943386412348957, -9.726947921299894162 ) ) ;
#53376 = TOROIDAL_SURFACE ( 'NONE', #37661, 24.69999999999999929, 0.3000000000000035971 ) ;
#53377 = CARTESIAN_POINT ( 'NONE',  ( -142.0374482299984891, 58.09359183931726278, 92.66567792160763872 ) ) ;
#53378 = VECTOR ( 'NONE', #64507, 1000.000000000000000 ) ;
#53379 = CARTESIAN_POINT ( 'NONE',  ( 138.5721691894144101, 44.34516164557649631, 31.15771391547428948 ) ) ;
#53380 = ORIENTED_EDGE ( 'NONE', *, *, #32135, .F. ) ;
#53381 = DIRECTION ( 'NONE',  ( 0.000000000000000000, -1.000000000000000000, 0.000000000000000000 ) ) ;
#53382 = LINE ( 'NONE', #10482, #6999 ) ;
#53383 = CARTESIAN_POINT ( 'NONE',  ( 159.6614743841974473, 60.66237087206236112, 2.878128257468113738 ) ) ;
#53384 = FACE_OUTER_BOUND ( 'NONE', #69436, .T. ) ;
#53385 = ORIENTED_EDGE ( 'NONE', *, *, #69390, .F. ) ;
#53386 = CARTESIAN_POINT ( 'NONE',  ( 174.2468109002382448, 73.34092405459590225, 66.74791253496901788 ) ) ;
#53387 = ORIENTED_EDGE ( 'NONE', *, *, #9009, .F. ) ;
#53388 = CARTESIAN_POINT ( 'NONE',  ( -105.4589068214114178, 34.42476264325678414, -49.32389774318545506 ) ) ;
#53389 = DIRECTION ( 'NONE',  ( 0.000000000000000000, 1.156482317317871725E-15, 1.000000000000000000 ) ) ;
#53390 = CARTESIAN_POINT ( 'NONE',  ( -61.75629144857964548, 16.58190704077737720, 41.18998502750409330 ) ) ;
#53392 = ORIENTED_EDGE ( 'NONE', *, *, #50768, .F. ) ;
#53391 = LINE ( 'NONE', #37578, #52242 ) ;
#53393 = CARTESIAN_POINT ( 'NONE',  ( -180.2244609727085560, 95.39945930389649220, 35.89761105671116326 ) ) ;
#53394 = CARTESIAN_POINT ( 'NONE',  ( 15.78827728214693416, -170.0000000000000000, 56.85925826316891829 ) ) ;
#53395 = DIRECTION ( 'NONE',  ( -0.000000000000000000, -0.000000000000000000, -1.000000000000000000 ) ) ;
#53396 = VERTEX_POINT ( 'NONE', #61085 ) ;
#53397 = CARTESIAN_POINT ( 'NONE',  ( 16.78635691501517613, 6.000000000000000000, -9.435653166495500344 ) ) ;
#53398 = EDGE_CURVE ( 'NONE', #66949, #69361, #12912, .T. ) ;
#53399 = EDGE_CURVE ( 'NONE', #11896, #4675, #7279, .T. ) ;
#53400 = CARTESIAN_POINT ( 'NONE',  ( 140.4586216751744985, 45.55624550472995793, 60.28699697572574223 ) ) ;
#53401 = EDGE_CURVE ( 'NONE', #57196, #30930, #34368, .T. ) ;
#53402 = CARTESIAN_POINT ( 'NONE',  ( -177.5100621450480105, 93.70693725195826573, 32.22205096411517644 ) ) ;
#53403 = CARTESIAN_POINT ( 'NONE',  ( 127.2358066117906787, 38.72257733469226082, 60.29414159756798597 ) ) ;
#53404 = ORIENTED_EDGE ( 'NONE', *, *, #7555, .F. ) ;
#53405 = CARTESIAN_POINT ( 'NONE',  ( 42.03719354205839664, 9.783015072457470040, 17.59534908508582518 ) ) ;
#53406 = ORIENTED_EDGE ( 'NONE', *, *, #57399, .F. ) ;
#53407 = AXIS2_PLACEMENT_3D ( 'NONE', #66617, #51120, #7866 ) ;
#53408 = VERTEX_POINT ( 'NONE', #17466 ) ;
#53409 = FACE_OUTER_BOUND ( 'NONE', #52629, .T. ) ;
#53410 = CARTESIAN_POINT ( 'NONE',  ( -47.71021106038689652, 12.83493994394914672, 89.94366651930251066 ) ) ;
#53411 = AXIS2_PLACEMENT_3D ( 'NONE', #59587, #520, #5450 ) ;
#53412 = CIRCLE ( 'NONE', #31008, 22.00000000000000000 ) ;
#53413 = FACE_OUTER_BOUND ( 'NONE', #41128, .T. ) ;
#53414 = CARTESIAN_POINT ( 'NONE',  ( -109.7470238012287496, 36.73863861880653303, 92.48605150114060791 ) ) ;
#53415 = AXIS2_PLACEMENT_3D ( 'NONE', #55907, #29865, #14027 ) ;
#53416 = CARTESIAN_POINT ( 'NONE',  ( -35.00000000000002842, 225.0000000000000000, 380.0000000000000000 ) ) ;
#53417 = CARTESIAN_POINT ( 'NONE',  ( -31.11269837220812207, -26.11269837220801193, 0.000000000000000000 ) ) ;
#53418 = VECTOR ( 'NONE', #42687, 1000.000000000000000 ) ;
#53419 = CARTESIAN_POINT ( 'NONE',  ( 55.61348889666937367, 50.24791103897128863, 41.38025477438755928 ) ) ;
#53420 = EDGE_LOOP ( 'NONE', ( #62543, #61172, #45389, #38614 ) ) ;
#53422 = AXIS2_PLACEMENT_3D ( 'NONE', #69270, #27039, #16145 ) ;
#53421 = LINE ( 'NONE', #5254, #40892 ) ;
#53423 = ORIENTED_EDGE ( 'NONE', *, *, #42026, .F. ) ;
#53424 =( LENGTH_UNIT ( ) NAMED_UNIT ( * ) SI_UNIT ( .MILLI., .METRE. ) );
#53426 = EDGE_CURVE ( 'NONE', #47929, #23514, #12205, .T. ) ;
#53425 =( REPRESENTATION_RELATIONSHIP ('NONE','NONE', #40274, #34334 ) REPRESENTATION_RELATIONSHIP_WITH_TRANSFORMATION ( #15555 )SHAPE_REPRESENTATION_RELATIONSHIP( ) );
#53427 = CARTESIAN_POINT ( 'NONE',  ( 210.9506883977752523, 115.3310071214937125, -74.81997715654915737 ) ) ;
#53428 = DIRECTION ( 'NONE',  ( -0.9989930665413151445, 0.04486483035050447404, 5.102127870520021999E-18 ) ) ;
#53429 = EDGE_CURVE ( 'NONE', #60705, #57073, #55098, .T. ) ;
#53430 = CARTESIAN_POINT ( 'NONE',  ( -71.26675986148647723, 19.63956187826083877, 12.32191659035411391 ) ) ;
#53431 = CARTESIAN_POINT ( 'NONE',  ( -120.0051930351106790, 43.92079660368834482, 69.61615127784293122 ) ) ;
#53432 = CARTESIAN_POINT ( 'NONE',  ( 22.28700331106867338, 7.803633676228379557, 41.26662101868341637 ) ) ;
#53433 = CARTESIAN_POINT ( 'NONE',  ( 199.7240524537553483, 99.76461913835838402, 84.77326177708235377 ) ) ;
#53434 = CARTESIAN_POINT ( 'NONE',  ( 159.2325040199866919, 60.31699144791973310, -63.12323753459439502 ) ) ;
#53435 = ORIENTED_EDGE ( 'NONE', *, *, #24333, .F. ) ;
#53436 = LINE ( 'NONE', #5265, #49974 ) ;
#53437 = CARTESIAN_POINT ( 'NONE',  ( 3.000000000000004441, 2.999999999999969802, -50.00000000000000000 ) ) ;
#53438 = ORIENTED_EDGE ( 'NONE', *, *, #44051, .F. ) ;
#53439 = VERTEX_POINT ( 'NONE', #22404 ) ;
#53440 = CARTESIAN_POINT ( 'NONE',  ( -23.93933407965396398, 9.495050561681678047, -69.16614878619023443 ) ) ;
#53441 = FACE_OUTER_BOUND ( 'NONE', #48839, .T. ) ;
#53442 = B_SPLINE_CURVE_WITH_KNOTS ( 'NONE', 3,
 ( #68946, #43244, #21457, #58066, #16178, #9885, #26060, #64720, #16531, #20770, #63691, #15506, #58394, #10206, #66480, #12654, #5962, #54848, #28121, #18276, #49563, #1395, #22849, #7382, #16868, #11584, #1052, #12301, #34113, #65420, #54494, #39382, #43940, #17210, #65069, #38326, #54139, #28834, #59770, #6320, #44665, #23214, #11241 ),
 .UNSPECIFIED., .F., .F.,
 ( 4, 2, 2, 2, 2, 2, 2, 2, 1, 2, 2, 2, 2, 2, 2, 2, 2, 2, 2, 2, 2, 4 ),
 ( 0.000000000000000000, 0.001466540241398126216, 0.002199810362097189432, 0.002933080482796252431, 0.004399620724194360649, 0.005866160965592469301, 0.007332701206990578820, 0.008065971327689634013, 0.008799241448388690073, 0.009532511569087746134, 0.01026578168978680046, 0.01173232193118494901, 0.01319886217258310103, 0.01466540241398124958, 0.01539867253468032472, 0.01613194265537939986, 0.01759848289677755015, 0.01906502313817570043, 0.01979829325887477384, 0.02053156337957384725, 0.02199810362097200794, 0.02346464386237016517 ),
 .UNSPECIFIED. ) ;
#53443 = LINE ( 'NONE', #5272, #9853 ) ;
#53444 = CARTESIAN_POINT ( 'NONE',  ( -19.56458807131854627, 15.75959024859389324, 0.000000000000000000 ) ) ;
#53445 = CARTESIAN_POINT ( 'NONE',  ( -143.8794621588508846, 59.54894433207191184, 6.412744670210712705 ) ) ;
#53446 = ORIENTED_EDGE ( 'NONE', *, *, #46473, .T. ) ;
#53447 = ORIENTED_EDGE ( 'NONE', *, *, #25598, .F. ) ;
#53448 = DIRECTION ( 'NONE',  ( 1.000000000000000000, 0.000000000000000000, 0.000000000000000000 ) ) ;
#53449 = EDGE_LOOP ( 'NONE', ( #44890, #47473, #51004, #27401, #32389 ) ) ;
#53450 = CARTESIAN_POINT ( 'NONE',  ( -12.50000000000002842, 207.5000000000000284, 378.0000000000000000 ) ) ;
#53451 = CARTESIAN_POINT ( 'NONE',  ( -144.2038301586456157, 61.09856042007388766, 32.89561146611724496 ) ) ;
#53452 = CARTESIAN_POINT ( 'NONE',  ( 62.04664474957769471, 12.44961624115900634, 71.61029269029653221 ) ) ;
#53453 = CARTESIAN_POINT ( 'NONE',  ( 44.99999999999999289, 20.00000000000000355, 2.000000000000015543 ) ) ;
#53454 = SURFACE_STYLE_USAGE ( .BOTH. , #32372 ) ;
#53455 = CARTESIAN_POINT ( 'NONE',  ( -65.20298343242136241, 4.613322252417249913, 3.125053320693571104E-16 ) ) ;
#53456 = VECTOR ( 'NONE', #68653, 1000.000000000000000 ) ;
#53457 = DIRECTION ( 'NONE',  ( -0.000000000000000000, -0.000000000000000000, -1.000000000000000000 ) ) ;
#53458 = VERTEX_POINT ( 'NONE', #43843 ) ;
#53459 = ORIENTED_EDGE ( 'NONE', *, *, #27290, .F. ) ;
#53460 = CARTESIAN_POINT ( 'NONE',  ( 440.2662102946430309, 394.9999999999997726, 106.4792280461226994 ) ) ;
#53461 = LINE ( 'NONE', #48181, #5823 ) ;
#53462 = VECTOR ( 'NONE', #16761, 1000.000000000000000 ) ;
#53463 = DIRECTION ( 'NONE',  ( -0.000000000000000000, 1.000000000000000000, -0.000000000000000000 ) ) ;
#53464 = DIRECTION ( 'NONE',  ( -0.000000000000000000, 1.000000000000000000, -0.000000000000000000 ) ) ;
#53465 = CARTESIAN_POINT ( 'NONE',  ( 67.56108154898467433, 13.77276756375644595, 43.29870974333168476 ) ) ;
#53466 = CARTESIAN_POINT ( 'NONE',  ( 16.45324200325260122, 7.529580975261485065, 83.72611423296160638 ) ) ;
#53467 = VECTOR ( 'NONE', #68367, 1000.000000000000000 ) ;
#53468 = EDGE_LOOP ( 'NONE', ( #47400, #9183, #9284, #62089 ) ) ;
#53469 = AXIS2_PLACEMENT_3D ( 'NONE', #64634, #16447, #37899 ) ;
#53470 = CIRCLE ( 'NONE', #46720, 4.999999999999997335 ) ;
#53471 = CARTESIAN_POINT ( 'NONE',  ( -95.50384525802327573, 29.46973564057716644, 68.08823763800167228 ) ) ;
#53472 = ORIENTED_EDGE ( 'NONE', *, *, #52303, .F. ) ;
#53473 = CARTESIAN_POINT ( 'NONE',  ( -71.16584859396995455, 19.60484997908767824, 38.15316589600989516 ) ) ;
#53474 = ORIENTED_EDGE ( 'NONE', *, *, #14554, .F. ) ;
#53475 = VECTOR ( 'NONE', #45843, 1000.000000000000227 ) ;
#53476 = B_SPLINE_CURVE_WITH_KNOTS ( 'NONE', 3,
 ( #44944, #12953, #18220, #46936, #67123, #52553, #42003, #12596, #68397, #36385, #28777, #18915, #29120, #14915, #9300, #41658, #34753, #13297, #50227, #30766, #61125, #55856, #2390, #50920, #2734, #18563, #41320, #40016, #56189, #20202, #61478, #14579, #8006, #57495, #25500, #63116, #5052, #47954, #27542, #43370, #58858, #59541, #69421, #37068 ),
 .UNSPECIFIED., .F., .F.,
 ( 4, 2, 2, 2, 2, 2, 2, 2, 2, 2, 2, 2, 2, 2, 2, 2, 2, 2, 2, 2, 2, 4 ),
 ( 0.000000000000000000, 0.001473754749730452713, 0.002210632124595686334, 0.002947509499460920172, 0.004421264249191396087, 0.005895018998921872436, 0.007368773748652348785, 0.008105651123517581755, 0.008842528498382814725, 0.01031628324811327893, 0.01179003799784374487, 0.01252691537270897611, 0.01326379274757420734, 0.01473754749730467328, 0.01547442487216991840, 0.01621130224703516004, 0.01768505699676564333, 0.01915881174649612662, 0.01989568912136136999, 0.02063256649622660990, 0.02210632124595708972, 0.02358007599568756954 ),
 .UNSPECIFIED. ) ;
#53477 = EDGE_LOOP ( 'NONE', ( #13302, #54828, #38502, #3929 ) ) ;
#53478 = CARTESIAN_POINT ( 'NONE',  ( -125.8938041572051389, 47.69968343338780414, 18.77539728269342945 ) ) ;
#53479 = CARTESIAN_POINT ( 'NONE',  ( -174.7869898116916545, 88.99756909636811031, 72.52766040328414476 ) ) ;
#53480 = B_SPLINE_CURVE_WITH_KNOTS ( 'NONE', 3,
 ( #16996, #64855, #53927, #16314, #37770, #21249, #59905, #11726, #32496, #21933, #42360, #38465, #10680, #15969, #32157, #837, #59555, #63819, #33198, #54636, #48642, #27207, #42698, #15631, #485, #11372, #47621, #64155, #22286, #59214, #43385, #5750, #53239, #129, #43033, #16656, #43725, #47967, #65201, #26185, #69072, #37081, #20908, #58523, #38111 ),
 .UNSPECIFIED., .F., .F.,
 ( 4, 2, 2, 1, 2, 2, 2, 2, 2, 2, 2, 2, 2, 2, 2, 2, 2, 2, 2, 2, 2, 2, 4 ),
 ( 0.02346464386237014782, 0.02493212228186625357, 0.02566586149161430644, 0.02639960070136235584, 0.02713333991111040872, 0.02786707912085845812, 0.02933455754035455346, 0.03006829675010259939, 0.03080203595985064879, 0.03226951437934675454, 0.03300325358909480394, 0.03373699279884285335, 0.03520447121833895909, 0.03667194963783507178, 0.03740568884758313506, 0.03813942805733119140, 0.03960690647682731103, 0.04107438489632342371, 0.04254186331581955027, 0.04327560252556761355, 0.04400934173531566990, 0.04547682015481180340, 0.04694429857430792302 ),
 .UNSPECIFIED. ) ;
#53481 = EDGE_CURVE ( 'NONE', #17325, #45082, #19405, .T. ) ;
#53482 = CARTESIAN_POINT ( 'NONE',  ( 21.75684465274323998, 6.764994602232764720, 15.23809131227820046 ) ) ;
#53483 = EDGE_LOOP ( 'NONE', ( #19751, #11329, #7145, #63187, #25707, #33747, #32231, #6538 ) ) ;
#53484 = ADVANCED_FACE ( 'NONE', ( #61764 ), #51228, .F. ) ;
#53485 = SURFACE_STYLE_FILL_AREA ( #21825 ) ;
#53486 = DIRECTION ( 'NONE',  ( -0.000000000000000000, -0.000000000000000000, -1.000000000000000000 ) ) ;
#53487 = CARTESIAN_POINT ( 'NONE',  ( 70.26936813788618963, 15.51386666370915535, 35.34273349493187766 ) ) ;
#53488 = EDGE_CURVE ( 'NONE', #29070, #34941, #67409, .T. ) ;
#53489 = CARTESIAN_POINT ( 'NONE',  ( 0.000000000000000000, 0.000000000000000000, 170.0000000000000000 ) ) ;
#53490 = CARTESIAN_POINT ( 'NONE',  ( 39.48989012082040517, 13.48566859677802299, 13.79046340968177908 ) ) ;
#53491 = DIRECTION ( 'NONE',  ( -0.000000000000000000, 1.000000000000000000, -0.000000000000000000 ) ) ;
#53492 = CARTESIAN_POINT ( 'NONE',  ( 140.7888851157410102, 46.97220912571251006, -67.49339367180394333 ) ) ;
#53493 = CARTESIAN_POINT ( 'NONE',  ( -145.3233446620409666, 62.00659513626050767, -62.91606084811092359 ) ) ;
#53494 = ORIENTED_EDGE ( 'NONE', *, *, #48484, .T. ) ;
#53495 = EDGE_CURVE ( 'NONE', #52786, #21788, #48769, .T. ) ;
#53496 = FACE_BOUND ( 'NONE', #26521, .T. ) ;
#53497 = DIRECTION ( 'NONE',  ( -0.000000000000000000, -1.000000000000000000, 0.000000000000000000 ) ) ;
#53498 = SURFACE_STYLE_USAGE ( .BOTH. , #65466 ) ;
#53499 = CARTESIAN_POINT ( 'NONE',  ( -417.6627218934913230, 219.4906275429376308, 111.5502958579881749 ) ) ;
#53500 = CARTESIAN_POINT ( 'NONE',  ( 307.2575771313985342, 0.000000000000000000, 256.6193948016162381 ) ) ;
#53501 = DIRECTION ( 'NONE',  ( -0.000000000000000000, 0.000000000000000000, 1.000000000000000000 ) ) ;
#53502 = FACE_OUTER_BOUND ( 'NONE', #44441, .T. ) ;
#53503 = CARTESIAN_POINT ( 'NONE',  ( -155.1302201283145337, 69.09929365814129198, 16.34568025258033330 ) ) ;
#53504 = CARTESIAN_POINT ( 'NONE',  ( -122.8011284400168392, 45.68452922414297035, -76.10641211455910593 ) ) ;
#53505 = CARTESIAN_POINT ( 'NONE',  ( 21.98745393275193294, 71.71550996510526943, 170.0000000000000000 ) ) ;
#53506 = CARTESIAN_POINT ( 'NONE',  ( 26.11269837220806167, 4.999999999999936939, 85.00100000000000477 ) ) ;
#53507 = CARTESIAN_POINT ( 'NONE',  ( 45.45802413036135903, 10.29289344693338393, -92.36508079978824526 ) ) ;
#53508 = VERTEX_POINT ( 'NONE', #66727 ) ;
#53509 = CIRCLE ( 'NONE', #23218, 5.000000000000004441 ) ;
#53510 = CARTESIAN_POINT ( 'NONE',  ( -38.87871322265799279, 11.95691939779334412, 11.85322953461970741 ) ) ;
#53511 = ORIENTED_EDGE ( 'NONE', *, *, #34494, .F. ) ;
#53512 = CARTESIAN_POINT ( 'NONE',  ( 313.9975424824652350, 172.0000000000000284, 256.6193948016162381 ) ) ;
#53513 = VERTEX_POINT ( 'NONE', #34712 ) ;
#53514 = EDGE_CURVE ( 'NONE', #61455, #9355, #60984, .T. ) ;
#53515 = DIRECTION ( 'NONE',  ( -0.000000000000000000, 1.000000000000000000, -0.000000000000000000 ) ) ;
#53516 = AXIS2_PLACEMENT_3D ( 'NONE', #68603, #15492, #10193 ) ;
#53517 = LINE ( 'NONE', #38750, #29014 ) ;
#53518 = CARTESIAN_POINT ( 'NONE',  ( 63.98971758354224448, 12.90030016320050876, -8.923645871160223564 ) ) ;
#53519 = CARTESIAN_POINT ( 'NONE',  ( 141.0792860804899362, 47.16255757051796138, -45.61442408848115093 ) ) ;
#53520 = VECTOR ( 'NONE', #25616, 1000.000000000000114 ) ;
#53521 = CARTESIAN_POINT ( 'NONE',  ( -51.34562532494748410, 14.75613283840036871, -63.02301684657460612 ) ) ;
#53522 = FACE_OUTER_BOUND ( 'NONE', #41228, .T. ) ;
#53523 = CARTESIAN_POINT ( 'NONE',  ( 5.850262805259839993, 200.0000000000000000, -1.724042536399416070 ) ) ;
#53524 = CARTESIAN_POINT ( 'NONE',  ( 5.799999999999999822, -4.618802153516998743, 7.999999999999998224 ) ) ;
#53525 = ORIENTED_EDGE ( 'NONE', *, *, #6413, .T. ) ;
#53526 = VERTEX_POINT ( 'NONE', #39974 ) ;
#53527 = FACE_OUTER_BOUND ( 'NONE', #36462, .T. ) ;
#53528 = B_SPLINE_CURVE_WITH_KNOTS ( 'NONE', 3,
 ( #40748, #34460, #67845, #2778, #18957, #3469 ),
 .UNSPECIFIED., .F., .F.,
 ( 4, 2, 4 ),
 ( 1.095770181118997428E-06, 0.03239442681617710901, 0.06478775786217309818 ),
 .UNSPECIFIED. ) ;
#53529 = CARTESIAN_POINT ( 'NONE',  ( 175.7684093698864558, 74.78503214758480055, 85.16604023312240201 ) ) ;
#53530 = VECTOR ( 'NONE', #6649, 1000.000000000000000 ) ;
#53531 = DIRECTION ( 'NONE',  ( 0.000000000000000000, 0.000000000000000000, 1.000000000000000000 ) ) ;
#53532 = PRODUCT_DEFINITION_CONTEXT ( 'detailed design', #33642, 'design' ) ;
#53533 = CARTESIAN_POINT ( 'NONE',  ( 7.484861546145031852, 64.56761454192836425, 133.5802547743875550 ) ) ;
#53534 = VERTEX_POINT ( 'NONE', #18524 ) ;
#53535 = CARTESIAN_POINT ( 'NONE',  ( -46.66904755831212981, -15.55634918610397222, 0.000000000000000000 ) ) ;
#53536 = CARTESIAN_POINT ( 'NONE',  ( -15.32550079334879456, 7.496023944924842475, 64.21821511530063731 ) ) ;
#53537 = CARTESIAN_POINT ( 'NONE',  ( 211.8382652195006699, 118.5282575235989952, 12.17967590094709074 ) ) ;
#53538 = DIRECTION ( 'NONE',  ( 1.000000000000000000, 0.000000000000000000, 0.000000000000000000 ) ) ;
#53539 = CARTESIAN_POINT ( 'NONE',  ( 447.3372781065085633, 177.8591479523844612, -111.4497041420119388 ) ) ;
#53540 = CARTESIAN_POINT ( 'NONE',  ( 207.8484262634767958, 110.7633525054914543, -23.80039066132988523 ) ) ;
#53541 = CARTESIAN_POINT ( 'NONE',  ( 105.0326735325357248, 21.99250842598269173, -0.6579281897535147472 ) ) ;
#53542 = B_SPLINE_CURVE_WITH_KNOTS ( 'NONE', 3,
 ( #47071, #41113, #68535, #5202, #69213, #58311, #31585, #63261, #31258, #15067, #21037, #20338, #66911, #41463, #36524, #15415, #53025, #10129, #3823, #52685, #36873, #25291, #62916, #4852, #9795, #68860, #57980, #14388, #53367, #35840, #31940, #4511, #46728, #25974, #26318, #45431, #57292, #47404, #42486, #9105, #14717, #36180, #9448, #52355 ),
 .UNSPECIFIED., .F., .F.,
 ( 4, 2, 2, 2, 2, 2, 2, 2, 2, 2, 2, 2, 2, 2, 2, 2, 2, 2, 2, 2, 2, 4 ),
 ( 0.02895403260893138903, 0.03071603688922224656, 0.03247804116951310410, 0.03424004544980396164, 0.03600204973009481918, 0.03776405401038567672, 0.03864505615053111937, 0.03952605829067656201, 0.04040706043082200466, 0.04128806257096744731, 0.04216906471111288995, 0.04305006685125833260, 0.04393106899140377525, 0.04481207113154921096, 0.04569307327169465360, 0.04657407541184009625, 0.04745507755198553890, 0.04833607969213098154, 0.05009808397242186684, 0.05186008825271275213, 0.05362209253300363743, 0.05714610109358543577 ),
 .UNSPECIFIED. ) ;
#53543 = CARTESIAN_POINT ( 'NONE',  ( 164.8914542114683570, 64.97670918603526502, 62.63277694328278500 ) ) ;
#53544 = VERTEX_POINT ( 'NONE', #24507 ) ;
#53545 = CARTESIAN_POINT ( 'NONE',  ( 63.01563776193091826, -170.0000000000000000, -96.90979201309711755 ) ) ;
#53546 = DIRECTION ( 'NONE',  ( -0.9959742939952397345, 0.08963930890342655666, 0.000000000000000000 ) ) ;
#53547 = PLANE ( 'NONE',  #62182 ) ;
#53548 = CARTESIAN_POINT ( 'NONE',  ( -44.00727179482577611, 47.83680621839560132, 40.00000000000003553 ) ) ;
#53549 = CARTESIAN_POINT ( 'NONE',  ( 154.6667526376337491, 55.50347409140648836, 17.02485824898109001 ) ) ;
#53550 = DIRECTION ( 'NONE',  ( 1.387778780781445429E-16, -1.000000000000000000, -3.081487911019577365E-33 ) ) ;
#53551 = EDGE_CURVE ( 'NONE', #47781, #52360, #22757, .T. ) ;
#53552 = ORIENTED_EDGE ( 'NONE', *, *, #20114, .T. ) ;
#53553 = FACE_OUTER_BOUND ( 'NONE', #30532, .T. ) ;
#53554 = DIRECTION ( 'NONE',  ( -1.000000000000000000, -0.000000000000000000, -0.000000000000000000 ) ) ;
#53555 = ORIENTED_EDGE ( 'NONE', *, *, #51568, .F. ) ;
#53556 = AXIS2_PLACEMENT_3D ( 'NONE', #27718, #58710, #10185 ) ;
#53557 = VERTEX_POINT ( 'NONE', #5445 ) ;
#53558 = CARTESIAN_POINT ( 'NONE',  ( 32.71619935235103327, 8.645270090896708837, 87.68833691130073760 ) ) ;
#53559 = LINE ( 'NONE', #16965, #59097 ) ;
#53560 = DIRECTION ( 'NONE',  ( 0.000000000000000000, -1.000000000000000000, 0.000000000000000000 ) ) ;
#53561 = EDGE_LOOP ( 'NONE', ( #49571, #3400, #7449, #25665 ) ) ;
#53562 = VECTOR ( 'NONE', #66817, 1000.000000000000000 ) ;
#53563 = CARTESIAN_POINT ( 'NONE',  ( 111.9975424824652634, 179.2896996249788799, 369.5505932007772003 ) ) ;
#53564 = CARTESIAN_POINT ( 'NONE',  ( -4.506365319453811580, 7.705038994660874607, 4.040912142253615613 ) ) ;
#53565 = CARTESIAN_POINT ( 'NONE',  ( 174.1422537179814753, 73.24254491731255712, -46.57861427890096451 ) ) ;
#53566 = AXIS2_PLACEMENT_3D ( 'NONE', #60679, #45538, #34307 ) ;
#53567 = CARTESIAN_POINT ( 'NONE',  ( 163.0608430180613198, 62.13093644261793003, 85.55641011433075960 ) ) ;
#53568 = FACE_OUTER_BOUND ( 'NONE', #53134, .T. ) ;
#53569 = AXIS2_PLACEMENT_3D ( 'NONE', #12276, #45322, #50259 ) ;
#53570 = ORIENTED_EDGE ( 'NONE', *, *, #45268, .F. ) ;
#53571 = EDGE_CURVE ( 'NONE', #22494, #53439, #9699, .T. ) ;
#53572 = CARTESIAN_POINT ( 'NONE',  ( -53.14657859411973817, 15.21831473227210552, -35.45855742538594768 ) ) ;
#53573 = VECTOR ( 'NONE', #9666, 1000.000000000000000 ) ;
#53574 = CARTESIAN_POINT ( 'NONE',  ( -56.92000000000000171, -36.09918303830819752, 30.00000000000000000 ) ) ;
#53575 = CARTESIAN_POINT ( 'NONE',  ( 12.47451846520756646, 7.423604437114564192, 30.78201781477134702 ) ) ;
#53576 = CARTESIAN_POINT ( 'NONE',  ( -12.50000000000002842, -18.06806526123148160, 0.000000000000000000 ) ) ;
#53577 = CARTESIAN_POINT ( 'NONE',  ( 112.3013380801406811, 400.0000000000077307, 101.0502958579874644 ) ) ;
#53578 = ORIENTED_EDGE ( 'NONE', *, *, #69235, .T. ) ;
#53579 = ORIENTED_EDGE ( 'NONE', *, *, #63698, .F. ) ;
#53580 = EDGE_CURVE ( 'NONE', #35602, #17986, #4336, .T. ) ;
#53581 = VERTEX_POINT ( 'NONE', #63503 ) ;
#53582 = CARTESIAN_POINT ( 'NONE',  ( 113.8724110608469147, 31.71510301790680941, -76.84776400044430034 ) ) ;
#53583 = CARTESIAN_POINT ( 'NONE',  ( -165.9827517816028717, 80.96014358007563771, 94.34005317371386923 ) ) ;
#53584 = CYLINDRICAL_SURFACE ( 'NONE', #50233, 7.500000000000013323 ) ;
#53585 = FACE_OUTER_BOUND ( 'NONE', #38513, .T. ) ;
#53586 = CARTESIAN_POINT ( 'NONE',  ( -447.6627218934913230, 394.9999999999998295, 108.5502958579881181 ) ) ;
#53587 = CARTESIAN_POINT ( 'NONE',  ( -6.123233995736762338E-16, 16.00000000000000000, -5.803681084894614095 ) ) ;
#53588 = DIRECTION ( 'NONE',  ( 1.000000000000000000, 0.000000000000000000, 0.000000000000000000 ) ) ;
#53589 = CARTESIAN_POINT ( 'NONE',  ( 22.80839748737789208, 6.826915557457465589, -18.82546783934041201 ) ) ;
#53590 = VERTEX_POINT ( 'NONE', #5099 ) ;
#53591 = FACE_OUTER_BOUND ( 'NONE', #53206, .T. ) ;
#53592 = EDGE_LOOP ( 'NONE', ( #35971, #41903 ) ) ;
#53593 = ORIENTED_EDGE ( 'NONE', *, *, #18453, .F. ) ;
#53594 = ADVANCED_FACE ( 'NONE', ( #36779 ), #4078, .F. ) ;
#53595 = CARTESIAN_POINT ( 'NONE',  ( 66.73467315386238852, 14.60276727483218906, -9.845064874592072357 ) ) ;
#53596 = CARTESIAN_POINT ( 'NONE',  ( -83.15209219203883606, 25.16621997697722790, -36.58508197384574601 ) ) ;
#53597 = DIRECTION ( 'NONE',  ( 0.000000000000000000, 1.000000000000000000, 0.000000000000000000 ) ) ;
#53599 = EDGE_CURVE ( 'NONE', #26979, #43082, #20271, .T. ) ;
#53598 = CARTESIAN_POINT ( 'NONE',  ( -156.0204364459165163, 71.27041535366187475, 15.10448288493537738 ) ) ;
#53600 = EDGE_CURVE ( 'NONE', #34095, #3682, #58876, .T. ) ;
#53602 = CARTESIAN_POINT ( 'NONE',  ( -38.12207019443992095, 16.97122609182251196, 13.79046412329103077 ) ) ;
#53601 = AXIS2_PLACEMENT_3D ( 'NONE', #22510, #16875, #38695 ) ;
#53603 = B_SPLINE_CURVE_WITH_KNOTS ( 'NONE', 3,
 ( #38587, #60031, #49470, #1305 ),
 .UNSPECIFIED., .F., .F.,
 ( 4, 4 ),
 ( 9.900409499016060538E-07, 0.05658314289920114704 ),
 .UNSPECIFIED. ) ;
#53604 = CARTESIAN_POINT ( 'NONE',  ( 20.37135563017390893, 6.690359945346062709, 43.47186685453966959 ) ) ;
#53605 = CARTESIAN_POINT ( 'NONE',  ( -150.9451284960939006, 66.73881725783795105, 84.54405725442943265 ) ) ;
#53606 = ORIENTED_EDGE ( 'NONE', *, *, #15549, .T. ) ;
#53607 = ORIENTED_EDGE ( 'NONE', *, *, #54911, .F. ) ;
#53608 = ORIENTED_EDGE ( 'NONE', *, *, #46121, .F. ) ;
#53609 = CIRCLE ( 'NONE', #39033, 75.31295361348099959 ) ;
#53610 = CARTESIAN_POINT ( 'NONE',  ( -155.5977325361977819, 70.88311713755696530, -11.08395381880265518 ) ) ;
#53611 = CARTESIAN_POINT ( 'NONE',  ( 38.42095780754793566, 9.297684251045554404, -35.66794142809995805 ) ) ;
#53612 = AXIS2_PLACEMENT_3D ( 'NONE', #61609, #52087, #68278 ) ;
#53613 = CARTESIAN_POINT ( 'NONE',  ( -38.26732153931116898, 10.81230693396213205, 61.44875431616114270 ) ) ;
#53614 = CARTESIAN_POINT ( 'NONE',  ( 197.6329787101074089, 98.74106466892202150, 61.01638013965135343 ) ) ;
#53615 = ORIENTED_EDGE ( 'NONE', *, *, #13111, .T. ) ;
#53616 = PRESENTATION_LAYER_ASSIGNMENT (  '', '', ( #14333 ) ) ;
#53617 = CARTESIAN_POINT ( 'NONE',  ( 188.0103583326377930, 87.39896620268127947, 66.54395642386660370 ) ) ;
#53618 = CARTESIAN_POINT ( 'NONE',  ( -154.0775378574014098, 68.15437918458557931, 71.03131665102951331 ) ) ;
#53619 = VECTOR ( 'NONE', #4213, 1000.000000000000000 ) ;
#53620 = CARTESIAN_POINT ( 'NONE',  ( 19.54452863209719737, 7.657034792877148277, 17.18020211478049220 ) ) ;
#53621 = CYLINDRICAL_SURFACE ( 'NONE', #22853, 21.02500000000000213 ) ;
#53622 = CARTESIAN_POINT ( 'NONE',  ( 0.000000000000000000, 0.000000000000000000, 0.000000000000000000 ) ) ;
#53623 = CARTESIAN_POINT ( 'NONE',  ( -86.15275984831843914, 25.31588180512565600, -42.09545882965587538 ) ) ;
#53624 = CARTESIAN_POINT ( 'NONE',  ( 22.30016284075436772, 6.796348835713780012, 68.11227918755604094 ) ) ;
#53625 = CARTESIAN_POINT ( 'NONE',  ( -149.5074843970971017, 64.17983161892347255, -7.968279941028269420 ) ) ;
#53626 = CARTESIAN_POINT ( 'NONE',  ( 10.13846145460683523, 6.385368868491637429, -64.90677605932107497 ) ) ;
#53627 = AXIS2_PLACEMENT_3D ( 'NONE', #44705, #62532, #39092 ) ;
#53628 = VERTEX_POINT ( 'NONE', #16344 ) ;
#53629 = LINE ( 'NONE', #23034, #55193 ) ;
#53630 = SHAPE_DEFINITION_REPRESENTATION ( #14271, #57739 ) ;
#53631 = CARTESIAN_POINT ( 'NONE',  ( -31.43908319763710679, -170.0000000000000000, 72.06100499665289760 ) ) ;
#53632 = CARTESIAN_POINT ( 'NONE',  ( 0.000000000000000000, 0.000000000000000000, 43.58025477438756212 ) ) ;
#53633 = CARTESIAN_POINT ( 'NONE',  ( 46.90141780929663895, 9.503798448769781970, -70.46900398398989296 ) ) ;
#53634 = CARTESIAN_POINT ( 'NONE',  ( 61.33840119549014958, 13.32121602003046235, -77.37933350821008105 ) ) ;
#53635 = EDGE_LOOP ( 'NONE', ( #62632, #69437, #30288, #19768 ) ) ;
#53636 = ADVANCED_FACE ( 'NONE', ( #65953 ), #11398, .T. ) ;
#53637 = VERTEX_POINT ( 'NONE', #32524 ) ;
#53638 = DIRECTION ( 'NONE',  ( -0.000000000000000000, -1.000000000000000000, -0.000000000000000000 ) ) ;
#53639 = CARTESIAN_POINT ( 'NONE',  ( -27.38060252176762077, -26.82905652391248807, 13.32819397642333215 ) ) ;
#53640 = EDGE_LOOP ( 'NONE', ( #35400, #4025, #60885, #7393 ) ) ;
#53641 = EDGE_CURVE ( 'NONE', #11717, #37319, #56460, .T. ) ;
#53642 = ORIENTED_EDGE ( 'NONE', *, *, #48557, .T. ) ;
#53643 = CYLINDRICAL_SURFACE ( 'NONE', #50426, 7.500000000000013323 ) ;
#53644 = ORIENTED_EDGE ( 'NONE', *, *, #62368, .T. ) ;
#53645 = CARTESIAN_POINT ( 'NONE',  ( 110.7167338301703836, 30.21148223254618159, 71.45576479620105204 ) ) ;
#53646 = CARTESIAN_POINT ( 'NONE',  ( 111.9975424824652634, 170.0000000000000284, 256.6193948016162381 ) ) ;
#53647 = CARTESIAN_POINT ( 'NONE',  ( 136.1037846510192821, 43.98155406734452555, 71.02523018034077040 ) ) ;
#53648 = DIRECTION ( 'NONE',  ( 0.000000000000000000, 1.000000000000000000, -1.224646799147353207E-16 ) ) ;
#53649 = CARTESIAN_POINT ( 'NONE',  ( 81.37856278600284554, 17.69577192910746888, -91.65141974325806018 ) ) ;
#53650 = DIRECTION ( 'NONE',  ( 1.000000000000000000, 0.000000000000000000, 0.000000000000000000 ) ) ;
#53651 = DIRECTION ( 'NONE',  ( 0.000000000000000000, 0.000000000000000000, 1.000000000000000000 ) ) ;
#53652 = AXIS2_PLACEMENT_3D ( 'NONE', #17853, #29106, #66061 ) ;
#53653 = EDGE_CURVE ( 'NONE', #61883, #6204, #6126, .T. ) ;
#53654 = EDGE_LOOP ( 'NONE', ( #9384, #6312, #24284, #50810 ) ) ;
#53656 = VERTEX_POINT ( 'NONE', #27588 ) ;
#53655 = ADVANCED_FACE ( 'NONE', ( #17382 ), #55013, .F. ) ;
#53657 = CARTESIAN_POINT ( 'NONE',  ( -125.8938041572051105, 46.49392987655492959, -23.06915330777029638 ) ) ;
#53658 = DIRECTION ( 'NONE',  ( 0.000000000000000000, 1.000000000000000000, -0.000000000000000000 ) ) ;
#53659 = CARTESIAN_POINT ( 'NONE',  ( -147.7895256390024485, 64.04409735547010030, -34.95785904615254225 ) ) ;
#53660 = EDGE_CURVE ( 'NONE', #39848, #16987, #14427, .T. ) ;
#53661 = VECTOR ( 'NONE', #882, 1000.000000000000000 ) ;
#53662 = CARTESIAN_POINT ( 'NONE',  ( -165.6404838346738870, 80.60836113891890875, -68.43868871235946472 ) ) ;
#53664 = EDGE_LOOP ( 'NONE', ( #30158, #9753 ) ) ;
#53663 = CARTESIAN_POINT ( 'NONE',  ( -142.2626321327577728, 58.26997216742664421, -44.27203299751281662 ) ) ;
#53665 = CARTESIAN_POINT ( 'NONE',  ( 57.07246224906425169, 12.39953617563782906, 15.06960304992271560 ) ) ;
#53666 = EDGE_CURVE ( 'NONE', #41122, #55255, #18784, .T. ) ;
#53667 = AXIS2_PLACEMENT_3D ( 'NONE', #39759, #29543, #50316 ) ;
#53668 = ORIENTED_EDGE ( 'NONE', *, *, #26828, .F. ) ;
#53669 = CARTESIAN_POINT ( 'NONE',  ( 55.50974873964668888, 12.08212941291357012, 90.84068197934951172 ) ) ;
#53670 = LINE ( 'NONE', #27638, #46870 ) ;
#53671 = CARTESIAN_POINT ( 'NONE',  ( 134.7697261969508986, 41.97802808873667146, -24.13692694190012489 ) ) ;
#53672 = AXIS2_PLACEMENT_3D ( 'NONE', #20831, #42291, #9594 ) ;
#53673 = CARTESIAN_POINT ( 'NONE',  ( 91.49345572560149265, 21.13836538408681065, -75.88006259688719979 ) ) ;
#53674 = CARTESIAN_POINT ( 'NONE',  ( 58.14386731224344373, 11.59506827749133429, -91.19280277787788691 ) ) ;
#53675 = CARTESIAN_POINT ( 'NONE',  ( 100.0000000000000284, 0.000000000000000000, -21.99999999999997158 ) ) ;
#53676 = CARTESIAN_POINT ( 'NONE',  ( -94.79166046756729713, 29.13671350128077364, -68.86817510426273259 ) ) ;
#53677 = ORIENTED_EDGE ( 'NONE', *, *, #4191, .F. ) ;
#53678 = EDGE_LOOP ( 'NONE', ( #16792, #42665 ) ) ;
#53679 = ADVANCED_FACE ( 'NONE', ( #2271 ), #8234, .T. ) ;
#53680 = CARTESIAN_POINT ( 'NONE',  ( 188.4904153916305063, 86.42965364612517476, -71.78902575509843587 ) ) ;
#53681 = CYLINDRICAL_SURFACE ( 'NONE', #30702, 25.00000000000296296 ) ;
#53682 = DIRECTION ( 'NONE',  ( 0.000000000000000000, 0.000000000000000000, -1.000000000000000000 ) ) ;
#53684 = EDGE_CURVE ( 'NONE', #31812, #68783, #24534, .T. ) ;
#53683 = DIRECTION ( 'NONE',  ( -0.000000000000000000, 1.000000000000000000, -0.000000000000000000 ) ) ;
#53685 = ADVANCED_FACE ( 'NONE', ( #10630 ), #9618, .F. ) ;
#53686 = CARTESIAN_POINT ( 'NONE',  ( 107.0555969502564011, 28.53646637607230119, -77.07238525624649128 ) ) ;
#53687 = CARTESIAN_POINT ( 'NONE',  ( 79.11678589158262298, 16.99307320450158443, 37.22067676483509757 ) ) ;
#53688 = DIRECTION ( 'NONE',  ( -0.000000000000000000, -0.000000000000000000, -1.000000000000000000 ) ) ;
#53689 = CARTESIAN_POINT ( 'NONE',  ( 45.89268866913129585, 10.36133864615982958, -39.35403686315040517 ) ) ;
#53690 = CARTESIAN_POINT ( 'NONE',  ( 205.5105258529713410, 107.4632495673648549, 71.01916293991351381 ) ) ;
#53691 = ORIENTED_EDGE ( 'NONE', *, *, #16349, .F. ) ;
#53692 = CARTESIAN_POINT ( 'NONE',  ( -105.8768181937898873, 34.64545164169049229, -9.071693415820034190 ) ) ;
#53693 = VERTEX_POINT ( 'NONE', #52517 ) ;
#53694 = CARTESIAN_POINT ( 'NONE',  ( -10.46803069297986077, 7.077485182625207649, -35.89476353789692809 ) ) ;
#53695 = CARTESIAN_POINT ( 'NONE',  ( -85.30133330826032534, 24.96073847331896189, 88.09538619317125097 ) ) ;
#53696 = CARTESIAN_POINT ( 'NONE',  ( 92.52113039222220436, 22.58921125235802307, 68.72354153264095089 ) ) ;
#53697 = CARTESIAN_POINT ( 'NONE',  ( 154.4550750032602195, 55.34393534448155805, -9.908619237073862607 ) ) ;
#53698 = CARTESIAN_POINT ( 'NONE',  ( 32.30062460741316244, 8.603096374765344834, 8.143925628932546346 ) ) ;
#53699 = CARTESIAN_POINT ( 'NONE',  ( -95.88693721180811735, 30.76307528361165922, -65.42962194985348390 ) ) ;
#53700 = LINE ( 'NONE', #32607, #53937 ) ;
#53701 = ORIENTED_EDGE ( 'NONE', *, *, #36445, .T. ) ;
#53702 = CARTESIAN_POINT ( 'NONE',  ( 211.0199171616895342, 115.4353716546810205, 94.44800888915801806 ) ) ;
#53703 = CARTESIAN_POINT ( 'NONE',  ( 40.56810615702079303, 52.87564043450657181, 34.48241824003539335 ) ) ;
#53704 = EDGE_LOOP ( 'NONE', ( #61631, #2241, #53787, #64149 ) ) ;
#53705 = CARTESIAN_POINT ( 'NONE',  ( -4.000000000000000000, 188.0000000000000000, 0.000000000000000000 ) ) ;
#53706 = CARTESIAN_POINT ( 'NONE',  ( -25.99999999999999645, 1.117010584002392767E-15, -17.00000000000000355 ) ) ;
#53707 = LINE ( 'NONE', #64274, #23017 ) ;
#53708 = CARTESIAN_POINT ( 'NONE',  ( 46.90208227351340753, 10.52324439420451441, -70.20627750463229688 ) ) ;
#53709 = CARTESIAN_POINT ( 'NONE',  ( 10.55634918610409656, 31.11269837220803325, 85.00100000000000477 ) ) ;
#53710 = CARTESIAN_POINT ( 'NONE',  ( -104.1244073710069671, 33.72720758483609416, -62.07464707146255023 ) ) ;
#53711 = AXIS2_PLACEMENT_3D ( 'NONE', #23643, #44389, #35231 ) ;
#53712 = CARTESIAN_POINT ( 'NONE',  ( 86.01230605172118260, 20.27366317264618800, 83.41941906375110705 ) ) ;
#53713 = VECTOR ( 'NONE', #37637, 1000.000000000000227 ) ;
#53714 = VERTEX_POINT ( 'NONE', #58145 ) ;
#53715 = CARTESIAN_POINT ( 'NONE',  ( 620.5106130828496589, 928.6907676558209914, 535.2366127225711807 ) ) ;
#53716 = CARTESIAN_POINT ( 'NONE',  ( -25.00000000000000000, 65.13282190615278466, -9.999999999999998224 ) ) ;
#53717 = CARTESIAN_POINT ( 'NONE',  ( -130.2196570250629009, 49.40815211106349381, 5.130512497953152895 ) ) ;
#53718 = CARTESIAN_POINT ( 'NONE',  ( -107.0809603157386505, 36.42942792191063717, 70.64629373282132008 ) ) ;
#53719 = COLOUR_RGB ( '',0.7921568627450980005, 0.8196078431372548767, 0.9333333333333333481 ) ;
#53720 = ITEM_DEFINED_TRANSFORMATION ( 'NONE', 'NONE', #63591,  #66832 ) ;
#53721 = CARTESIAN_POINT ( 'NONE',  ( -126.8016613879753294, 48.30316697011514293, -34.95518786917430987 ) ) ;
#53722 = ORIENTED_EDGE ( 'NONE', *, *, #22475, .T. ) ;
#53723 = FACE_OUTER_BOUND ( 'NONE', #67488, .T. ) ;
#53724 = CARTESIAN_POINT ( 'NONE',  ( 89.88695630745282017, 20.55793566325393940, 70.82916094545055330 ) ) ;
#53725 = CARTESIAN_POINT ( 'NONE',  ( -145.1840176520338161, 60.59722987250436432, 85.77424136295870483 ) ) ;
#53726 = EDGE_CURVE ( 'NONE', #16032, #7544, #15296, .T. ) ;
#53727 = CARTESIAN_POINT ( 'NONE',  ( 141.2894128405439176, 46.09731134920846074, 38.04785505188484507 ) ) ;
#53728 = ORIENTED_EDGE ( 'NONE', *, *, #50914, .F. ) ;
#53729 = DIRECTION ( 'NONE',  ( 0.000000000000000000, -1.000000000000000000, 0.000000000000000000 ) ) ;
#53730 = CARTESIAN_POINT ( 'NONE',  ( 81.74250361646204510, 18.86685472882136949, 16.07802836438051486 ) ) ;
#53731 = CARTESIAN_POINT ( 'NONE',  ( 160.9099843287284557, 61.67000084894968381, 3.384304814524660365 ) ) ;
#53732 = DIRECTION ( 'NONE',  ( -0.000000000000000000, 1.000000000000000000, -0.000000000000000000 ) ) ;
#53733 = EDGE_LOOP ( 'NONE', ( #50837, #67716 ) ) ;
#53734 = EDGE_CURVE ( 'NONE', #42734, #37998, #59860, .T. ) ;
#53735 = CARTESIAN_POINT ( 'NONE',  ( 141.9165763529819344, 242.0000000000000000, 129.0000000000000000 ) ) ;
#53736 = ORIENTED_EDGE ( 'NONE', *, *, #9097, .F. ) ;
#53737 = CARTESIAN_POINT ( 'NONE',  ( -73.10694748374054086, 20.28107308417882493, -20.82856601646535566 ) ) ;
#53738 = CARTESIAN_POINT ( 'NONE',  ( 70.46452034227868921, 14.52462608639674535, -71.07036406642562554 ) ) ;
#53739 = CARTESIAN_POINT ( 'NONE',  ( 57.30278335769610010, -48.40406511297319980, 170.0000000000000000 ) ) ;
#53740 = ADVANCED_FACE ( 'NONE', ( #47568 ), #15585, .T. ) ;
#53742 = VERTEX_POINT ( 'NONE', #4343 ) ;
#53741 = CARTESIAN_POINT ( 'NONE',  ( 153.8224167330182297, 56.12711234192240539, 16.62213432411530789 ) ) ;
#53743 = CARTESIAN_POINT ( 'NONE',  ( 164.0298848570287191, 62.93631132702878972, 40.58462181814118708 ) ) ;
#53744 = CARTESIAN_POINT ( 'NONE',  ( 32.12337157895397866, 8.585320123189577046, -95.00000000000133582 ) ) ;
#53745 = EDGE_CURVE ( 'NONE', #11417, #25097, #31757, .T. ) ;
#53746 = CARTESIAN_POINT ( 'NONE',  ( 0.000000000000000000, 0.000000000000000000, 0.000000000000000000 ) ) ;
#53747 = EDGE_LOOP ( 'NONE', ( #2709, #21718, #62414, #10148, #41270, #48030 ) ) ;
#53748 = CARTESIAN_POINT ( 'NONE',  ( 174.1361937581588677, 73.23677172949255976, -94.55001106689485368 ) ) ;
#53749 = CARTESIAN_POINT ( 'NONE',  ( 139.1353280997809350, 44.70436000187870462, 69.18824476712693183 ) ) ;
#53750 = CARTESIAN_POINT ( 'NONE',  ( 412.3372781065086770, 0.000000000000000000, 113.5502958579881749 ) ) ;
#53751 = CARTESIAN_POINT ( 'NONE',  ( 132.0563630623056497, 41.51825634609594573, 56.57050957695005877 ) ) ;
#53752 = EDGE_LOOP ( 'NONE', ( #65273, #51105 ) ) ;
#53753 = AXIS2_PLACEMENT_3D ( 'NONE', #61369, #3322, #8949 ) ;
#53754 = VERTEX_POINT ( 'NONE', #69383 ) ;
#53755 = ORIENTED_EDGE ( 'NONE', *, *, #62591, .T. ) ;
#53757 = EDGE_CURVE ( 'NONE', #33258, #913, #30727, .T. ) ;
#53756 = CARTESIAN_POINT ( 'NONE',  ( -30.00000000000000355, -27.00000000000000355, 15.00000000000000000 ) ) ;
#53758 = CARTESIAN_POINT ( 'NONE',  ( -107.2385267828037456, 36.51474259889399576, 5.542223241171852166 ) ) ;
#53759 = CARTESIAN_POINT ( 'NONE',  ( 2.905661822261151883E-14, 15.55634918610403084, 85.00100000000000477 ) ) ;
#53760 = DIRECTION ( 'NONE',  ( -0.000000000000000000, -1.000000000000000000, -0.000000000000000000 ) ) ;
#53761 = CARTESIAN_POINT ( 'NONE',  ( -109.7362175185300543, 36.73266838575884208, 90.83257743108923421 ) ) ;
#53762 = EDGE_CURVE ( 'NONE', #68312, #57391, #47230, .T. ) ;
#53763 = CARTESIAN_POINT ( 'NONE',  ( 412.3372781065085633, 400.0000000000000568, -146.4497041420118535 ) ) ;
#53764 = FACE_OUTER_BOUND ( 'NONE', #54786, .T. ) ;
#53765 = DIRECTION ( 'NONE',  ( -0.000000000000000000, 1.000000000000000000, -0.000000000000000000 ) ) ;
#53766 = ORIENTED_EDGE ( 'NONE', *, *, #53641, .T. ) ;
#53767 = DIRECTION ( 'NONE',  ( 1.000000000000000000, 0.000000000000000000, 0.000000000000000000 ) ) ;
#53768 = ORIENTED_EDGE ( 'NONE', *, *, #8341, .F. ) ;
#53769 = DIRECTION ( 'NONE',  ( 0.000000000000000000, 0.000000000000000000, 1.000000000000000000 ) ) ;
#53770 = CARTESIAN_POINT ( 'NONE',  ( 210.6741002223296846, 114.9147155784838503, -66.13167200068693319 ) ) ;
#53771 = FACE_OUTER_BOUND ( 'NONE', #1531, .T. ) ;
#53772 = CARTESIAN_POINT ( 'NONE',  ( 5.737557066527558369, 192.0000000000000000, 2.275957463600585040 ) ) ;
#53773 = CARTESIAN_POINT ( 'NONE',  ( -33.74415167774779434, 9.981065646265545155, -89.36609339537675112 ) ) ;
#53774 = CARTESIAN_POINT ( 'NONE',  ( 18.20314211955701822, 7.596739727129572906, 30.39710523511859108 ) ) ;
#53775 = CARTESIAN_POINT ( 'NONE',  ( 197.2367704513663966, 96.64129968056330711, 91.28287337347603625 ) ) ;
#53776 = CYLINDRICAL_SURFACE ( 'NONE', #69209, 7.500000000000013323 ) ;
#53777 = EDGE_LOOP ( 'NONE', ( #63959, #50366, #9555, #51359 ) ) ;
#53778 = DIRECTION ( 'NONE',  ( -0.000000000000000000, 1.000000000000000000, -0.000000000000000000 ) ) ;
#53779 = CYLINDRICAL_SURFACE ( 'NONE', #54337, 65.36598343705435354 ) ;
#53780 = ORIENTED_EDGE ( 'NONE', *, *, #66678, .F. ) ;
#53781 = EDGE_LOOP ( 'NONE', ( #33812, #61308 ) ) ;
#53782 = CARTESIAN_POINT ( 'NONE',  ( -30.95341298663138829, 10.53108683215057795, -77.16174795566554678 ) ) ;
#53783 = CARTESIAN_POINT ( 'NONE',  ( 57.39083379741710900, 11.43779987330584369, -48.20640899083532105 ) ) ;
#53784 = LINE ( 'NONE', #48848, #64236 ) ;
#53785 = CARTESIAN_POINT ( 'NONE',  ( -146.5341851369306596, 61.69744206542952014, 4.476676838031795391 ) ) ;
#53786 = ORIENTED_EDGE ( 'NONE', *, *, #17427, .T. ) ;
#53787 = ORIENTED_EDGE ( 'NONE', *, *, #5183, .T. ) ;
#53788 = AXIS2_PLACEMENT_3D ( 'NONE', #25596, #25246, #47031 ) ;
#53789 = DIRECTION ( 'NONE',  ( 0.9362348706397369824, 0.3513748240813435175, 0.000000000000000000 ) ) ;
#53790 = PRODUCT_DEFINITION ( 'UNKNOWN', '', #25447, #32442 ) ;
#53791 = VERTEX_POINT ( 'NONE', #42311 ) ;
#53792 = CARTESIAN_POINT ( 'NONE',  ( 38.91512155099543691, 9.360679678889624711, -23.77526687496408897 ) ) ;
#53793 = CARTESIAN_POINT ( 'NONE',  ( 0.4988340113754565208, 3.871605243940355656, -8.000000000000000000 ) ) ;
#53794 = CARTESIAN_POINT ( 'NONE',  ( 6.564829507346109594, 24.24955267099648992, 3.061616997868437868E-16 ) ) ;
#53795 = FACE_OUTER_BOUND ( 'NONE', #20774, .T. ) ;
#53796 = EDGE_CURVE ( 'NONE', #25958, #17560, #20600, .T. ) ;
#53797 = CARTESIAN_POINT ( 'NONE',  ( -53.60725281709914469, 37.40286400928249577, 43.58025477438756212 ) ) ;
#53798 = CARTESIAN_POINT ( 'NONE',  ( 0.000000000000000000, 0.000000000000000000, 2.000000000000000000 ) ) ;
#53799 = EDGE_CURVE ( 'NONE', #65633, #66303, #13550, .T. ) ;
#53800 = FACE_BOUND ( 'NONE', #9386, .T. ) ;
#53801 = ORIENTED_EDGE ( 'NONE', *, *, #40510, .F. ) ;
#53802 = AXIS2_PLACEMENT_3D ( 'NONE', #63545, #34837, #55935 ) ;
#53803 = EDGE_LOOP ( 'NONE', ( #22232, #22889, #34439 ) ) ;
#53804 = CARTESIAN_POINT ( 'NONE',  ( -156.3413281584584809, -170.0000000000000000, 94.99999999999866418 ) ) ;
#53805 = CARTESIAN_POINT ( 'NONE',  ( 26.11269837220803325, -15.55634918610409656, 2.000000000000000000 ) ) ;
#53806 = FACE_OUTER_BOUND ( 'NONE', #49424, .T. ) ;
#53807 = CARTESIAN_POINT ( 'NONE',  ( 69.74037587279242700, 14.33355757956376131, 40.67087411745646364 ) ) ;
#53808 = CARTESIAN_POINT ( 'NONE',  ( 9.120338347441469651, 7.384947993289908474, 87.75479786978895902 ) ) ;
#53809 = VECTOR ( 'NONE', #63521, 1000.000000000000000 ) ;
#53810 = B_SPLINE_CURVE_WITH_KNOTS ( 'NONE', 3,
 ( #11383, #39190, #55346, #17007, #7172, #28627, #23364, #38840, #39527, #48657, #43397, #16671, #32853, #33215, #6475, #54288, #6110, #27569, #49011, #849, #22301, #43738, #1195, #45142, #62012, #28986, #50432, #3288, #67654, #30362, #35645, #14185, #8912, #18769, #51814, #46181, #66975, #66621 ),
 .UNSPECIFIED., .F., .F.,
 ( 4, 2, 2, 2, 2, 2, 2, 2, 2, 2, 2, 2, 2, 2, 2, 2, 2, 2, 4 ),
 ( 1.589900327696125378E-17, 0.001559859933532243290, 0.003119719867064470967, 0.004679579800596697994, 0.006239439734128925455, 0.007799299667661153783, 0.008579229634427268381, 0.009359159601193383846, 0.01091901953472561304, 0.01169894950149172504, 0.01247887946825783877, 0.01403873940179006276, 0.01559859933532228848, 0.01715845926885451248, 0.01871831920238673300, 0.02027817913591895352, 0.02183803906945117751, 0.02339789900298339803, 0.02495775893651561855 ),
 .UNSPECIFIED. ) ;
#53811 = ORIENTED_EDGE ( 'NONE', *, *, #52782, .F. ) ;
#53812 = EDGE_CURVE ( 'NONE', #15169, #40853, #60217, .T. ) ;
#53813 = CARTESIAN_POINT ( 'NONE',  ( -78.66644367742111399, -170.0000000000000000, -96.30455181264525777 ) ) ;
#53814 = ORIENTED_EDGE ( 'NONE', *, *, #53036, .F. ) ;
#53815 = CARTESIAN_POINT ( 'NONE',  ( -75.01314391403411719, 20.96328762434824711, 31.35011065199344671 ) ) ;
#53816 = VERTEX_POINT ( 'NONE', #12035 ) ;
#53817 = EDGE_CURVE ( 'NONE', #41104, #10412, #6752, .T. ) ;
#53818 = EDGE_CURVE ( 'NONE', #8968, #35032, #7108, .T. ) ;
#53819 = EDGE_LOOP ( 'NONE', ( #64678, #30124, #45342, #59961, #64219 ) ) ;
#53820 = CARTESIAN_POINT ( 'NONE',  ( -122.3759299995709426, 45.41285412136510047, 4.634680028069846358 ) ) ;
#53821 = VECTOR ( 'NONE', #56904, 1000.000000000000000 ) ;
#53822 = CARTESIAN_POINT ( 'NONE',  ( -173.1211646369891071, 87.12891641440857882, 57.66624519710472185 ) ) ;
#53823 = CARTESIAN_POINT ( 'NONE',  ( 126.8947007444828614, 37.37669340849690514, 61.05352645786824439 ) ) ;
#53824 = ORIENTED_EDGE ( 'NONE', *, *, #53111, .F. ) ;
#53825 = CARTESIAN_POINT ( 'NONE',  ( 183.2136430849847955, 6.000000000000000000, -46.68900338898722424 ) ) ;
#53826 = CARTESIAN_POINT ( 'NONE',  ( 150.8925291903903769, 52.71218673668931842, 33.26698628395256918 ) ) ;
#53827 = DIRECTION ( 'NONE',  ( -0.000000000000000000, 1.000000000000000000, -0.000000000000000000 ) ) ;
#53828 = FACE_OUTER_BOUND ( 'NONE', #1418, .T. ) ;
#53829 = CARTESIAN_POINT ( 'NONE',  ( -15.55634918610400597, 15.55634918610405748, 0.000000000000000000 ) ) ;
#53830 = APPLICATION_CONTEXT ( 'automotive_design' ) ;
#53831 = DIRECTION ( 'NONE',  ( -0.000000000000000000, -1.000000000000000000, -0.000000000000000000 ) ) ;
#53832 = CARTESIAN_POINT ( 'NONE',  ( -24.93568128341083678, 8.613819379861711312, 41.48431949557672027 ) ) ;
#53833 = DIRECTION ( 'NONE',  ( -0.000000000000000000, 1.000000000000000000, -0.000000000000000000 ) ) ;
#53834 = VERTEX_POINT ( 'NONE', #81 ) ;
#53835 = VECTOR ( 'NONE', #18319, 1000.000000000000000 ) ;
#53836 = FACE_BOUND ( 'NONE', #26177, .T. ) ;
#53837 = CARTESIAN_POINT ( 'NONE',  ( -1.876547441458565668, 6.576559737910140591, -74.33668192632359251 ) ) ;
#53838 = CARTESIAN_POINT ( 'NONE',  ( -180.3114074031035727, 97.09758726817783270, 63.01175798389278526 ) ) ;
#53839 = CARTESIAN_POINT ( 'NONE',  ( 57.25833571151868284, 48.36523237396223607, 41.38025477438755928 ) ) ;
#53840 = CARTESIAN_POINT ( 'NONE',  ( -121.1841775822197604, 44.65790002524552449, -48.27118250510603303 ) ) ;
#53841 = CARTESIAN_POINT ( 'NONE',  ( 89.99999999999998579, 0.000000000000000000, -10.00000000000000000 ) ) ;
#53842 = DIRECTION ( 'NONE',  ( 0.000000000000000000, 0.000000000000000000, 1.000000000000000000 ) ) ;
#53843 = ADVANCED_FACE ( 'NONE', ( #33146 ), #42979, .F. ) ;
#53844 = CARTESIAN_POINT ( 'NONE',  ( 114.8405205227988546, 21.96421596965998901, 1.294720749503662116 ) ) ;
#53845 = CARTESIAN_POINT ( 'NONE',  ( 112.3013380801408658, 388.0000000000065938, -128.9497041420121093 ) ) ;
#53846 = DIRECTION ( 'NONE',  ( -7.703719777548945123E-34, -1.479221584281240009E-31, 1.000000000000000000 ) ) ;
#53847 = CARTESIAN_POINT ( 'NONE',  ( -84.55783695959762269, 25.74181993349143838, 69.43046075343895041 ) ) ;
#53848 = CARTESIAN_POINT ( 'NONE',  ( 87.58754341703161117, 20.81465688423122984, -9.023248056753891078 ) ) ;
#53849 = ORIENTED_EDGE ( 'NONE', *, *, #32658, .F. ) ;
#53850 = CARTESIAN_POINT ( 'NONE',  ( -35.17718245314463132, 11.25729435722178629, 17.37854247445588740 ) ) ;
#53851 = ORIENTED_EDGE ( 'NONE', *, *, #18014, .F. ) ;
#53852 = DIRECTION ( 'NONE',  ( -0.000000000000000000, -0.000000000000000000, -1.000000000000000000 ) ) ;
#53853 = ORIENTED_EDGE ( 'NONE', *, *, #3014, .F. ) ;
#53854 = AXIS2_PLACEMENT_3D ( 'NONE', #27191, #6083, #11711 ) ;
#53855 = CARTESIAN_POINT ( 'NONE',  ( 17.73567516211396367, 7.577454475141604640, -77.12280871073899391 ) ) ;
#53856 = CARTESIAN_POINT ( 'NONE',  ( 102.7603480884046405, 26.66430664428465036, 91.41953138856987948 ) ) ;
#53857 = CARTESIAN_POINT ( 'NONE',  ( -149.5074843970971017, 65.50121172469319220, 57.56537183036274286 ) ) ;
#53858 = CARTESIAN_POINT ( 'NONE',  ( 68.61679388097593346, 14.04192738700837495, -21.36990119259161958 ) ) ;
#53860 = CARTESIAN_POINT ( 'NONE',  ( -25.79929641484369540, 9.749255553662436569, -47.78593713492852402 ) ) ;
#53859 = STYLED_ITEM ( 'NONE', ( #41298 ), #65110 ) ;
#53861 = CARTESIAN_POINT ( 'NONE',  ( -47.79955240516189008, 13.88975739862079806, -71.53314426491067479 ) ) ;
#53862 = CARTESIAN_POINT ( 'NONE',  ( -71.36019764570897905, 20.73631042140123171, -94.55033525794866023 ) ) ;
#53863 = CARTESIAN_POINT ( 'NONE',  ( -29.87147652227456263, 100.0000000000000000, 73.58025477438756923 ) ) ;
#53864 = VERTEX_POINT ( 'NONE', #16260 ) ;
#53865 = ORIENTED_EDGE ( 'NONE', *, *, #63141, .T. ) ;
#53866 = CARTESIAN_POINT ( 'NONE',  ( 211.9978709542735373, 18.00000000000003553, 276.7363262511108815 ) ) ;
#53867 = CARTESIAN_POINT ( 'NONE',  ( -168.7314919967218145, 83.83749564070832605, 71.26571717153785812 ) ) ;
#53868 = CARTESIAN_POINT ( 'NONE',  ( 126.9799862522376372, 38.57834705404714271, -94.18946796078350303 ) ) ;
#53869 = B_SPLINE_CURVE_WITH_KNOTS ( 'NONE', 3,
 ( #31633, #26020, #26364, #57687, #62622, #8815 ),
 .UNSPECIFIED., .F., .F.,
 ( 4, 2, 4 ),
 ( 1.095770181108978510E-06, 0.03239442681617710901, 0.06478775786217311206 ),
 .UNSPECIFIED. ) ;
#53870 = AXIS2_PLACEMENT_3D ( 'NONE', #51026, #19012, #3875 ) ;
#53871 = CARTESIAN_POINT ( 'NONE',  ( 29.99999999999999645, -30.00000000000000355, 12.00000000000000000 ) ) ;
#53872 = EDGE_LOOP ( 'NONE', ( #56676, #9372, #45378 ) ) ;
#53873 = EDGE_CURVE ( 'NONE', #13204, #44574, #59855, .T. ) ;
#53874 = CARTESIAN_POINT ( 'NONE',  ( 283.0554507864566176, 21.63937313260594664, 3.971423903130205879 ) ) ;
#53875 = CARTESIAN_POINT ( 'NONE',  ( 186.2680729609084551, 85.48839327635670315, -22.32090202264587120 ) ) ;
#53876 = CARTESIAN_POINT ( 'NONE',  ( 207.4566510040494336, 111.9649643341356438, 2.885941162796656911 ) ) ;
#53877 = DIRECTION ( 'NONE',  ( 0.000000000000000000, 1.000000000000000000, -0.000000000000000000 ) ) ;
#53878 = CARTESIAN_POINT ( 'NONE',  ( 43.14712943604300222, 8.926114770663666320, -9.772680129153844319 ) ) ;
#53879 = DIRECTION ( 'NONE',  ( 0.000000000000000000, 0.000000000000000000, 1.000000000000000000 ) ) ;
#53880 = CARTESIAN_POINT ( 'NONE',  ( 106.2331853604024587, 21.75170065437620437, -3.304351318131959925 ) ) ;
#53881 = DIRECTION ( 'NONE',  ( 0.000000000000000000, 0.000000000000000000, -1.000000000000000000 ) ) ;
#53882 = EDGE_CURVE ( 'NONE', #55296, #22681, #27504, .T. ) ;
#53883 = EDGE_CURVE ( 'NONE', #60359, #56353, #54273, .T. ) ;
#53884 = ORIENTED_EDGE ( 'NONE', *, *, #46306, .F. ) ;
#53885 = DIRECTION ( 'NONE',  ( 0.000000000000000000, 1.000000000000000000, -0.000000000000000000 ) ) ;
#53886 = CARTESIAN_POINT ( 'NONE',  ( 93.43270425363542131, 22.93046121381056679, -46.48805702006733753 ) ) ;
#53887 = EDGE_CURVE ( 'NONE', #35508, #64034, #12738, .T. ) ;
#53888 = DIRECTION ( 'NONE',  ( 1.000000000000000000, -0.000000000000000000, -0.000000000000000000 ) ) ;
#53889 = CARTESIAN_POINT ( 'NONE',  ( 412.3372781065085633, 400.0000000000000568, -146.4497041420118535 ) ) ;
#53890 = CARTESIAN_POINT ( 'NONE',  ( 153.2384531768736338, 54.43344429203622781, 16.27428681065648775 ) ) ;
#53891 = AXIS2_PLACEMENT_3D ( 'NONE', #46963, #31148, #67738 ) ;
#53892 = CYLINDRICAL_SURFACE ( 'NONE', #64784, 7.500000000000013323 ) ;
#53893 = ORIENTED_EDGE ( 'NONE', *, *, #39885, .F. ) ;
#53894 = CARTESIAN_POINT ( 'NONE',  ( 61.10129719786243641, 12.23677173834304988, 17.72406295025428946 ) ) ;
#53895 = CARTESIAN_POINT ( 'NONE',  ( -59.57733000654213384, 15.94108165424593437, 58.66074221055215077 ) ) ;
#53896 = ORIENTED_EDGE ( 'NONE', *, *, #14910, .F. ) ;
#53897 = ORIENTED_EDGE ( 'NONE', *, *, #138, .F. ) ;
#53898 = CARTESIAN_POINT ( 'NONE',  ( 46.09329439034695497, 10.39313452975435048, 87.69915135060715272 ) ) ;
#53899 = LINE ( 'NONE', #21906, #50133 ) ;
#53900 = CARTESIAN_POINT ( 'NONE',  ( 105.4193882736795871, 26.71329717705294726, 31.34684377997668747 ) ) ;
#53901 = EDGE_CURVE ( 'NONE', #41002, #42064, #44024, .T. ) ;
#53902 = ORIENTED_EDGE ( 'NONE', *, *, #32783, .T. ) ;
#53903 = EDGE_CURVE ( 'NONE', #54103, #68068, #65503, .T. ) ;
#53904 = CARTESIAN_POINT ( 'NONE',  ( -59.95707852844800811, 16.05120821151901467, -75.25667932634594592 ) ) ;
#53905 = CARTESIAN_POINT ( 'NONE',  ( 32.67604581760324578, 7.629767527669975458, -12.94769449661993121 ) ) ;
#53906 = CARTESIAN_POINT ( 'NONE',  ( 177.7964363391244831, 76.75162026635257462, -50.48114945074676996 ) ) ;
#53907 = VECTOR ( 'NONE', #24183, 1000.000000000000000 ) ;
#53908 = CARTESIAN_POINT ( 'NONE',  ( -40.27405704175634327, 63.28161525591265502, 170.0000000000000000 ) ) ;
#53909 = DIRECTION ( 'NONE',  ( -1.000000000000000000, 0.000000000000000000, 0.000000000000000000 ) ) ;
#53910 = VERTEX_POINT ( 'NONE', #17663 ) ;
#53911 = CARTESIAN_POINT ( 'NONE',  ( -51.77431913897918037, 14.86466849149171310, -35.95328652352582566 ) ) ;
#53912 = DIRECTION ( 'NONE',  ( -1.000000000000000000, -2.309263891220325604E-14, 2.135044278125301096E-16 ) ) ;
#53913 = CARTESIAN_POINT ( 'NONE',  ( 11.81843724556921238, 7.412394300769733491, 43.88267239520089902 ) ) ;
#53914 = CARTESIAN_POINT ( 'NONE',  ( 10.55634918610396511, -46.66904755831214402, 2.000000000000001776 ) ) ;
#53915 = DIRECTION ( 'NONE',  ( 0.000000000000000000, 0.000000000000000000, 1.000000000000000000 ) ) ;
#53916 = DIRECTION ( 'NONE',  ( -0.000000000000000000, -0.000000000000000000, 1.000000000000000000 ) ) ;
#53918 = VERTEX_POINT ( 'NONE', #430 ) ;
#53917 = CARTESIAN_POINT ( 'NONE',  ( -48.41612563322100016, 13.00196567016870297, 94.99999999999866418 ) ) ;
#53919 = ORIENTED_EDGE ( 'NONE', *, *, #25435, .F. ) ;
#53920 = AXIS2_PLACEMENT_3D ( 'NONE', #22033, #32932, #12186 ) ;
#53921 = ORIENTED_EDGE ( 'NONE', *, *, #34056, .F. ) ;
#53922 = CARTESIAN_POINT ( 'NONE',  ( -8.320652113663527416, 6.923290556636831461, -8.573520141480127421 ) ) ;
#53923 = CARTESIAN_POINT ( 'NONE',  ( -172.2883581164155657, 87.70586714890205826, 84.53995063412840238 ) ) ;
#53924 = CARTESIAN_POINT ( 'NONE',  ( 31.11269837220803325, -15.55634918610409656, 85.00100000000000477 ) ) ;
#53925 = DIRECTION ( 'NONE',  ( 0.000000000000000000, 0.000000000000000000, 1.000000000000000000 ) ) ;
#53926 = CARTESIAN_POINT ( 'NONE',  ( -38.87871322265797858, 11.95691939779334234, 65.54233071554708090 ) ) ;
#53927 = CARTESIAN_POINT ( 'NONE',  ( -8.800520192024524846, 7.964629484975262130, -23.52613853675388711 ) ) ;
#53928 = DIRECTION ( 'NONE',  ( 1.000000000000000000, 0.000000000000000000, 0.000000000000000000 ) ) ;
#53929 = CARTESIAN_POINT ( 'NONE',  ( 21.42484406671929520, 6.746536496442162800, -21.12818067883022266 ) ) ;
#53930 = EDGE_LOOP ( 'NONE', ( #60593, #9888, #8902, #55653 ) ) ;
#53931 = CARTESIAN_POINT ( 'NONE',  ( -12.50000000000002842, 207.5000000000000284, 0.000000000000000000 ) ) ;
#53932 = ORIENTED_EDGE ( 'NONE', *, *, #24472, .F. ) ;
#53933 = EDGE_LOOP ( 'NONE', ( #43021, #39509, #10637, #50126 ) ) ;
#53934 = CARTESIAN_POINT ( 'NONE',  ( 6.000000000000000000, 23.07878402833891229, 5.000000000000000000 ) ) ;
#53935 = DIRECTION ( 'NONE',  ( 1.000000000000000000, 0.000000000000000000, -2.921639538487254261E-16 ) ) ;
#53936 = CARTESIAN_POINT ( 'NONE',  ( 117.7510095710447615, 32.51306356638684036, 90.73932576073276834 ) ) ;
#53937 = VECTOR ( 'NONE', #38574, 1000.000000000000227 ) ;
#53938 = CARTESIAN_POINT ( 'NONE',  ( -156.9262190792699130, 72.10659547035875505, 12.51482676534390848 ) ) ;
#53939 = DIRECTION ( 'NONE',  ( 1.000000000000000000, 0.000000000000000000, 0.000000000000000000 ) ) ;
#53940 = CARTESIAN_POINT ( 'NONE',  ( 21.88606409348644277, 6.772455198693822176, 33.14124745247766413 ) ) ;
#53941 = CARTESIAN_POINT ( 'NONE',  ( -150.6785516065348531, 66.50778382752601203, 84.49707106786556210 ) ) ;
#53942 = ORIENTED_EDGE ( 'NONE', *, *, #12785, .T. ) ;
#53943 = ORIENTED_EDGE ( 'NONE', *, *, #66738, .T. ) ;
#53944 = ORIENTED_EDGE ( 'NONE', *, *, #62591, .F. ) ;
#53945 = DIRECTION ( 'NONE',  ( -0.000000000000000000, -0.000000000000000000, -1.000000000000000000 ) ) ;
#53946 = DIRECTION ( 'NONE',  ( 0.000000000000000000, 0.000000000000000000, -1.000000000000000000 ) ) ;
#53947 = DIRECTION ( 'NONE',  ( 0.7071067811865475727, 0.000000000000000000, 0.7071067811865474617 ) ) ;
#53948 = CARTESIAN_POINT ( 'NONE',  ( 198.4045886930829852, 99.71425793793713410, 59.46347056621107896 ) ) ;
#53949 = EDGE_LOOP ( 'NONE', ( #25704, #67807, #31872, #4278 ) ) ;
#53950 = CARTESIAN_POINT ( 'NONE',  ( 75.31295361348102801, 0.000000000000000000, 0.000000000000000000 ) ) ;
#53951 = CARTESIAN_POINT ( 'NONE',  ( 0.000000000000000000, 0.000000000000000000, 0.000000000000000000 ) ) ;
#53952 = DIRECTION ( 'NONE',  ( -0.000000000000000000, -0.000000000000000000, 1.000000000000000000 ) ) ;
#53953 = CARTESIAN_POINT ( 'NONE',  ( 103.5839822277949622, 25.92130892112108143, 13.72661071236549724 ) ) ;
#53954 = CARTESIAN_POINT ( 'NONE',  ( -6.000000000000000000, 23.07878402833891229, 9.999999999999998224 ) ) ;
#53955 = CARTESIAN_POINT ( 'NONE',  ( 26.11269837220809364, 20.55634918610396866, 85.00100000000000477 ) ) ;
#53956 = CARTESIAN_POINT ( 'NONE',  ( 21.73827885904430346, 6.764046335627706519, 59.78669074769747027 ) ) ;
#53957 = CARTESIAN_POINT ( 'NONE',  ( -65.36598343705435354, 0.000000000000000000, 41.38025477438755928 ) ) ;
#53958 = CARTESIAN_POINT ( 'NONE',  ( 11.82322073186612421, 6.406156243758798219, -76.23436747048188522 ) ) ;
#53959 = EDGE_CURVE ( 'NONE', #59320, #42164, #40072, .T. ) ;
#53960 = EDGE_LOOP ( 'NONE', ( #31470, #12966, #49995 ) ) ;
#53961 = LINE ( 'NONE', #13523, #39485 ) ;
#53962 = EDGE_CURVE ( 'NONE', #2204, #43521, #13347, .T. ) ;
#53963 = CIRCLE ( 'NONE', #5676, 20.30000000000000071 ) ;
#53964 = CARTESIAN_POINT ( 'NONE',  ( 177.7960900018544805, 75.34533826015461955, 43.55310789600767407 ) ) ;
#53965 = CARTESIAN_POINT ( 'NONE',  ( -132.8123438040340147, 51.22132183644642822, -39.50633901085532074 ) ) ;
#53966 = CARTESIAN_POINT ( 'NONE',  ( 417.3372781065086201, 399.9999999999998863, 108.5502958579882034 ) ) ;
#53967 = CARTESIAN_POINT ( 'NONE',  ( -50.88541732109811022, 55.03078243218087806, 41.38025477438755928 ) ) ;
#53968 = EDGE_LOOP ( 'NONE', ( #56937, #15344 ) ) ;
#53969 = PRODUCT_DEFINITION_SHAPE ( 'NONE', 'NONE',  #69628 ) ;
#53970 = AXIS2_PLACEMENT_3D ( 'NONE', #55917, #55205, #66836 ) ;
#53971 = ORIENTED_EDGE ( 'NONE', *, *, #35090, .F. ) ;
#53972 = DIRECTION ( 'NONE',  ( 0.000000000000000000, 1.000000000000000000, 0.000000000000000000 ) ) ;
#53973 = CARTESIAN_POINT ( 'NONE',  ( 197.8598785550297237, 99.02620879292952338, 6.767166655171187095 ) ) ;
#53974 = ORIENTED_EDGE ( 'NONE', *, *, #46433, .F. ) ;
#53975 = AXIS2_PLACEMENT_3D ( 'NONE', #51007, #45376, #67533 ) ;
#53976 = ORIENTED_EDGE ( 'NONE', *, *, #1502, .T. ) ;
#53977 = CARTESIAN_POINT ( 'NONE',  ( 185.5412249395995730, 84.70425786165998261, 30.77240809119399145 ) ) ;
#53978 = CARTESIAN_POINT ( 'NONE',  ( 196.9999999999999716, 0.000000000000000000, -46.99999999999997158 ) ) ;
#53979 = EDGE_CURVE ( 'NONE', #22403, #192, #53125, .T. ) ;
#53980 = ORIENTED_EDGE ( 'NONE', *, *, #12785, .F. ) ;
#53981 = CARTESIAN_POINT ( 'NONE',  ( 110.2429982417149432, 29.99119854320844070, 71.45576479620103783 ) ) ;
#53982 = CARTESIAN_POINT ( 'NONE',  ( 103.3187396002585672, 26.90210317967632747, -94.19991905147882960 ) ) ;
#53983 = CARTESIAN_POINT ( 'NONE',  ( 137.5911612413395062, 44.91497189902065656, 70.36324336602153551 ) ) ;
#53984 = CARTESIAN_POINT ( 'NONE',  ( -71.21970990337017327, 19.62334883444993494, -43.64161293005157916 ) ) ;
#53985 = CONICAL_SURFACE ( 'NONE', #32667, 8.000000000000001776, 1.047197551196595855 ) ;
#53986 = CARTESIAN_POINT ( 'NONE',  ( -101.3492134984965105, 32.31003911421601060, 45.47588113239901020 ) ) ;
#53987 = CARTESIAN_POINT ( 'NONE',  ( 94.07616572255074061, 22.09777530676769430, -44.34594446716025828 ) ) ;
#53988 = CARTESIAN_POINT ( 'NONE',  ( 313.9975424824652350, 18.08738615523480675, 402.4289050101931480 ) ) ;
#53989 = ORIENTED_EDGE ( 'NONE', *, *, #9009, .T. ) ;
#53990 = ORIENTED_EDGE ( 'NONE', *, *, #18185, .F. ) ;
#53991 = CARTESIAN_POINT ( 'NONE',  ( -7.825402957745087207, 6.891034867348159842, 71.96013162991091860 ) ) ;
#53992 = CARTESIAN_POINT ( 'NONE',  ( 157.4703587214989113, 58.92748579479260229, -9.279633708673953763 ) ) ;
#53993 = CARTESIAN_POINT ( 'NONE',  ( -142.0084862216822614, 59.34995487985345619, -41.73440649756038567 ) ) ;
#53994 = CARTESIAN_POINT ( 'NONE',  ( -171.4943428135323131, 86.82484920477510570, -61.68648179989266822 ) ) ;
#53996 = ORIENTED_EDGE ( 'NONE', *, *, #59193, .F. ) ;
#53995 = CARTESIAN_POINT ( 'NONE',  ( -142.5211356634642073, 58.47296527616907014, -45.05442505613748949 ) ) ;
#53997 = CARTESIAN_POINT ( 'NONE',  ( 55.77012379229942240, 12.13428856597100491, 12.42136026870828047 ) ) ;
#53998 = VERTEX_POINT ( 'NONE', #21879 ) ;
#53999 = PLANE ( 'NONE',  #21153 ) ;
#54000 = DIRECTION ( 'NONE',  ( -0.000000000000000000, 1.000000000000000000, -0.000000000000000000 ) ) ;
#54001 = CARTESIAN_POINT ( 'NONE',  ( -20.93485882276955579, 13.66498028065538861, 0.000000000000000000 ) ) ;
#54002 = CARTESIAN_POINT ( 'NONE',  ( 79.38459371357852490, 17.07499996355400995, -14.47219513322666273 ) ) ;
#54003 = DIRECTION ( 'NONE',  ( 1.110515250991959028E-16, 1.000000000000000000, 1.110223024625156294E-16 ) ) ;
#54004 = CARTESIAN_POINT ( 'NONE',  ( 86.62931800182292363, 20.48449268398422163, -8.977013608448025650 ) ) ;
#54005 = FACE_BOUND ( 'NONE', #12940, .T. ) ;
#54006 = CARTESIAN_POINT ( 'NONE',  ( -101.3492134984965389, 32.31003911421601771, -61.90232122945574389 ) ) ;
#54007 = ORIENTED_EDGE ( 'NONE', *, *, #19208, .T. ) ;
#54008 = ORIENTED_EDGE ( 'NONE', *, *, #62963, .F. ) ;
#54009 = AXIS2_PLACEMENT_3D ( 'NONE', #58912, #38151, #54675 ) ;
#54010 = DIRECTION ( 'NONE',  ( 0.000000000000000000, 1.000000000000000000, -0.000000000000000000 ) ) ;
#54011 = DIRECTION ( 'NONE',  ( 1.000000000000000000, 0.000000000000000000, 0.000000000000000000 ) ) ;
#54012 = DIRECTION ( 'NONE',  ( 1.000000000000000000, 0.000000000000000000, 0.000000000000000000 ) ) ;
#54013 = DIRECTION ( 'NONE',  ( 0.000000000000000000, -1.000000000000000000, 0.000000000000000000 ) ) ;
#54014 = CARTESIAN_POINT ( 'NONE',  ( 105.8229724512851391, 27.98935528750254420, -76.33106803925247164 ) ) ;
#54015 = AXIS2_PLACEMENT_3D ( 'NONE', #11777, #33252, #54687 ) ;
#54016 = EDGE_CURVE ( 'NONE', #6148, #31811, #29595, .T. ) ;
#54017 = CARTESIAN_POINT ( 'NONE',  ( -77.02112161466365592, 22.77583432622784798, -62.13887678495888167 ) ) ;
#54018 = CARTESIAN_POINT ( 'NONE',  ( 26.11269837220812562, 31.11269837220800483, 85.00100000000000477 ) ) ;
#54019 = CARTESIAN_POINT ( 'NONE',  ( 46.23113030541875190, 10.41513832761375902, -40.00976335710233656 ) ) ;
#54020 = CARTESIAN_POINT ( 'NONE',  ( -15.55634918610396866, 36.11269837220808654, 2.000000000000001776 ) ) ;
#54021 = EDGE_LOOP ( 'NONE', ( #55460, #37335, #60376, #66930 ) ) ;
#54022 = CARTESIAN_POINT ( 'NONE',  ( -25.79929641484368830, 9.749255553662431240, 5.903164045998831710 ) ) ;
#54023 = ORIENTED_EDGE ( 'NONE', *, *, #63212, .F. ) ;
#54024 = VECTOR ( 'NONE', #6255, 1000.000000000000000 ) ;
#54025 = CIRCLE ( 'NONE', #1287, 27.00000000000000000 ) ;
#54026 = ADVANCED_FACE ( 'NONE', ( #30554 ), #20006, .F. ) ;
#54027 = CARTESIAN_POINT ( 'NONE',  ( -33.84080342750782222, 9.997552308299120227, 3.750042810399141668 ) ) ;
#54028 = FACE_OUTER_BOUND ( 'NONE', #45184, .T. ) ;
#54029 = CARTESIAN_POINT ( 'NONE',  ( 90.30840373526895348, 21.77864858272155146, 57.51652433617496030 ) ) ;
#54030 = CARTESIAN_POINT ( 'NONE',  ( 156.5977259323288138, 56.97512126940428345, -24.24178231028911057 ) ) ;
#54031 = DIRECTION ( 'NONE',  ( -0.000000000000000000, -0.000000000000000000, -1.000000000000000000 ) ) ;
#54032 = CARTESIAN_POINT ( 'NONE',  ( -98.67557579989350813, 32.10670856967970366, -75.95360591899348890 ) ) ;
#54033 = CIRCLE ( 'NONE', #59614, 24.99999999999985434 ) ;
#54034 = CARTESIAN_POINT ( 'NONE',  ( 125.0000000000000000, 0.000000000000000000, 10.00000000000000000 ) ) ;
#54035 = ORIENTED_EDGE ( 'NONE', *, *, #67362, .F. ) ;
#54036 = CARTESIAN_POINT ( 'NONE',  ( 0.000000000000000000, 19.13941707223176181, -5.803681084894614095 ) ) ;
#54037 = FACE_OUTER_BOUND ( 'NONE', #12521, .T. ) ;
#54038 = ORIENTED_EDGE ( 'NONE', *, *, #24486, .T. ) ;
#54039 = CARTESIAN_POINT ( 'NONE',  ( 58.47885130911549112, 12.69429933094348506, 58.16495201468348597 ) ) ;
#54040 = CARTESIAN_POINT ( 'NONE',  ( 12.68603346975295487, 7.427591953486040843, -63.03079970252639441 ) ) ;
#54041 = DIRECTION ( 'NONE',  ( 0.000000000000000000, -0.000000000000000000, -1.000000000000000000 ) ) ;
#54042 = EDGE_CURVE ( 'NONE', #41303, #61608, #19649, .T. ) ;
#54043 = DIRECTION ( 'NONE',  ( -0.000000000000000000, -0.000000000000000000, -1.000000000000000000 ) ) ;
#54044 = CARTESIAN_POINT ( 'NONE',  ( -4.504169684898444714, 6.697401007565301434, 44.34460521785229048 ) ) ;
#54045 = CARTESIAN_POINT ( 'NONE',  ( -105.8768181937898447, 34.64545164169047808, -62.76079459674738104 ) ) ;
#54046 = EDGE_CURVE ( 'NONE', #12092, #25560, #56950, .T. ) ;
#54047 = CARTESIAN_POINT ( 'NONE',  ( 79.20873702246476000, 18.07356264622685771, 89.75976143019885001 ) ) ;
#54048 = VERTEX_POINT ( 'NONE', #24602 ) ;
#54049 = CARTESIAN_POINT ( 'NONE',  ( 563.2335602428199763, 993.5958018146700397, 657.5068267248714164 ) ) ;
#54050 = EDGE_CURVE ( 'NONE', #50931, #2896, #20337, .T. ) ;
#54051 = DIRECTION ( 'NONE',  ( -0.000000000000000000, -0.000000000000000000, -1.000000000000000000 ) ) ;
#54052 = CARTESIAN_POINT ( 'NONE',  ( -128.7650348665117122, 48.41336321950709731, 18.20782630100844202 ) ) ;
#54053 = CARTESIAN_POINT ( 'NONE',  ( -170.2951623264597458, 85.51757001115475987, -35.25191629578037578 ) ) ;
#54054 = CARTESIAN_POINT ( 'NONE',  ( -125.8938041572051105, 47.69968343338781835, -34.91370389823391918 ) ) ;
#54055 = ORIENTED_EDGE ( 'NONE', *, *, #56725, .F. ) ;
#54056 = DIRECTION ( 'NONE',  ( 0.6234898018587431423, -0.7818314824680220321, 0.000000000000000000 ) ) ;
#54057 = CARTESIAN_POINT ( 'NONE',  ( -74.75133697335800775, -5.472689625387135770, 41.38025477438755928 ) ) ;
#54058 = CARTESIAN_POINT ( 'NONE',  ( -23.85457283326427813, -7.880174245944393974, 3.061616997868437868E-16 ) ) ;
#54059 = CARTESIAN_POINT ( 'NONE',  ( -157.0089340775362814, 70.81267942336693011, 91.81416744909685690 ) ) ;
#54060 = CARTESIAN_POINT ( 'NONE',  ( -39.29440389294403246, 17.09499999999999886, 4.000000000000000000 ) ) ;
#54061 = ADVANCED_FACE ( 'NONE', ( #14716 ), #24937, .T. ) ;
#54062 = EDGE_LOOP ( 'NONE', ( #41750, #43826, #30108, #24681 ) ) ;
#54063 = DIRECTION ( 'NONE',  ( 1.000000000000000000, 0.000000000000000000, 0.000000000000000000 ) ) ;
#54064 = CARTESIAN_POINT ( 'NONE',  ( 110.7164744784864041, 29.10110206241301967, -62.76698815611734972 ) ) ;
#54065 = DIRECTION ( 'NONE',  ( -1.000000000000000000, 0.000000000000000000, 0.000000000000000000 ) ) ;
#54066 = VECTOR ( 'NONE', #16188, 1000.000000000000000 ) ;
#54067 = EDGE_CURVE ( 'NONE', #31009, #40830, #62121, .T. ) ;
#54068 = EDGE_CURVE ( 'NONE', #49352, #62757, #47053, .T. ) ;
#54069 = EDGE_CURVE ( 'NONE', #42836, #33757, #49517, .T. ) ;
#54070 = VECTOR ( 'NONE', #23664, 1000.000000000000000 ) ;
#54071 = ORIENTED_EDGE ( 'NONE', *, *, #31011, .F. ) ;
#54072 = CARTESIAN_POINT ( 'NONE',  ( -64.61430802170482934, -7.070445451048283481, 170.0000000000000000 ) ) ;
#54073 = ORIENTED_EDGE ( 'NONE', *, *, #51826, .F. ) ;
#54074 = VECTOR ( 'NONE', #34922, 1000.000000000000114 ) ;
#54075 = AXIS2_PLACEMENT_3D ( 'NONE', #53798, #38331, #54141 ) ;
#54076 = EDGE_LOOP ( 'NONE', ( #46402, #65065, #5981, #59264 ) ) ;
#54077 = CARTESIAN_POINT ( 'NONE',  ( -119.6686548882513392, 42.52932972989362526, -91.89361949810667340 ) ) ;
#54078 = CYLINDRICAL_SURFACE ( 'NONE', #60775, 7.500000000000020428 ) ;
#54080 = ORIENTED_EDGE ( 'NONE', *, *, #34495, .F. ) ;
#54079 = CARTESIAN_POINT ( 'NONE',  ( 153.2208437558771550, 55.67531116261156399, 16.26249285195666161 ) ) ;
#54081 = CARTESIAN_POINT ( 'NONE',  ( -68.11501976657811497, -31.41506934893937952, 43.58025477438756212 ) ) ;
#54082 = CIRCLE ( 'NONE', #48449, 75.31295361348104223 ) ;
#54083 = DIRECTION ( 'NONE',  ( 0.000000000000000000, 0.000000000000000000, -1.000000000000000000 ) ) ;
#54084 = CARTESIAN_POINT ( 'NONE',  ( 39.40195752203892710, -170.0000000000000000, -23.77526687496409608 ) ) ;
#54085 = EDGE_LOOP ( 'NONE', ( #37741, #56818, #24620, #14089 ) ) ;
#54086 = CARTESIAN_POINT ( 'NONE',  ( -147.9238768789327025, 64.15721743195632598, -88.62461181704978230 ) ) ;
#54087 = CARTESIAN_POINT ( 'NONE',  ( -35.17600017528511813, 10.23461991275926586, -22.47999145424725498 ) ) ;
#54088 = CARTESIAN_POINT ( 'NONE',  ( -166.3175803736862122, 79.86140754556167565, 41.48986120324848059 ) ) ;
#54089 = CARTESIAN_POINT ( 'NONE',  ( 131.3924949472282719, 41.12442122814101708, 56.76750252905168281 ) ) ;
#54090 = VERTEX_POINT ( 'NONE', #15414 ) ;
#54091 = ORIENTED_EDGE ( 'NONE', *, *, #39362, .F. ) ;
#54092 = ORIENTED_EDGE ( 'NONE', *, *, #50105, .T. ) ;
#54093 = CARTESIAN_POINT ( 'NONE',  ( -11.01093400780220932, -22.58090174195397992, 0.000000000000000000 ) ) ;
#54094 = CARTESIAN_POINT ( 'NONE',  ( -30.00000000000000355, -30.00000000000000355, 15.00000000000000000 ) ) ;
#54095 = CARTESIAN_POINT ( 'NONE',  ( 63.01563776193091826, 12.67277567978498176, -77.56524142263344856 ) ) ;
#54096 = DIRECTION ( 'NONE',  ( 0.000000000000000000, 0.4999999999999998890, -0.8660254037844387076 ) ) ;
#54097 = CARTESIAN_POINT ( 'NONE',  ( 429.8372781065087338, 394.9999999999999432, 91.05029585798857283 ) ) ;
#54098 = FACE_OUTER_BOUND ( 'NONE', #38982, .T. ) ;
#54099 = CARTESIAN_POINT ( 'NONE',  ( 74.01791526339567895, -12.16185512414844716, 170.0000000000000000 ) ) ;
#54100 = VERTEX_POINT ( 'NONE', #610 ) ;
#54101 = EDGE_CURVE ( 'NONE', #15739, #56426, #43509, .T. ) ;
#54102 = DIRECTION ( 'NONE',  ( -1.000000000000000000, 0.000000000000000000, 0.000000000000000000 ) ) ;
#54103 = VERTEX_POINT ( 'NONE', #42485 ) ;
#54104 = FACE_OUTER_BOUND ( 'NONE', #31738, .T. ) ;
#54105 = CARTESIAN_POINT ( 'NONE',  ( 183.9986899696430669, 81.60141257362811018, 29.88476414464218323 ) ) ;
#54106 = CARTESIAN_POINT ( 'NONE',  ( 0.000000000000000000, 0.000000000000000000, 0.000000000000000000 ) ) ;
#54107 = CARTESIAN_POINT ( 'NONE',  ( -71.16584859396996876, 19.60484997908767113, 11.30861530554621730 ) ) ;
#54108 = DIRECTION ( 'NONE',  ( -0.000000000000000000, -0.000000000000000000, 1.000000000000000000 ) ) ;
#54109 = CARTESIAN_POINT ( 'NONE',  ( 23.03546163277112413, 7.848986635155157821, 39.46112786506829906 ) ) ;
#54110 = VECTOR ( 'NONE', #4105, 1000.000000000000000 ) ;
#54111 = LINE ( 'NONE', #5596, #52874 ) ;
#54112 = CARTESIAN_POINT ( 'NONE',  ( 7.484861546145933353, -64.56761454192826477, 170.0000000000000000 ) ) ;
#54113 = CARTESIAN_POINT ( 'NONE',  ( 162.6205203824432317, 63.07332653227187791, -65.01131320985699347 ) ) ;
#54114 = ORIENTED_EDGE ( 'NONE', *, *, #23699, .F. ) ;
#54115 = AXIS2_PLACEMENT_3D ( 'NONE', #44322, #65447, #49590 ) ;
#54116 = B_SPLINE_CURVE_WITH_KNOTS ( 'NONE', 3,
 ( #57926, #31205, #58596, #53311, #63550, #26603, #36821, #62519, #52637, #47350, #911, #27982, #32912, #38537, #1255, #60344, #59628, #16042, #33628, #22361, #32230, #11440, #21662, #64228, #55058, #53997, #65634, #59291, #59981, #17422, #53665, #37493, #54350, #6173, #5822, #28329, #27635, #5488, #49072, #43798, #65274, #6877, #16727 ),
 .UNSPECIFIED., .F., .F.,
 ( 4, 2, 2, 2, 2, 2, 2, 2, 2, 2, 2, 2, 1, 2, 2, 2, 2, 2, 2, 2, 2, 4 ),
 ( 0.02379577142314830140, 0.02527778373276530488, 0.02601878988757379968, 0.02675979604238229101, 0.02824180835199927714, 0.02972382066161625980, 0.03046482681642476154, 0.03120583297123326327, 0.03268784528085027369, 0.03416985759046728410, 0.03565186990008429452, 0.03639287605489279626, 0.03713388220970130493, 0.03787488836450979973, 0.03861589451931830147, 0.04009790682893531188, 0.04157991913855231536, 0.04306193144816932578, 0.04380293760297782057, 0.04454394375778632231, 0.04602595606740332579, 0.04750796837702032926 ),
 .UNSPECIFIED. ) ;
#54117 = DIRECTION ( 'NONE',  ( 1.000000000000000000, 0.000000000000000000, 0.000000000000000000 ) ) ;
#54118 = DIRECTION ( 'NONE',  ( -0.000000000000000000, 0.000000000000000000, -1.000000000000000000 ) ) ;
#54119 = ORIENTED_EDGE ( 'NONE', *, *, #58057, .F. ) ;
#54120 = ORIENTED_EDGE ( 'NONE', *, *, #68379, .F. ) ;
#54121 = EDGE_CURVE ( 'NONE', #14469, #13950, #37200, .T. ) ;
#54122 = CARTESIAN_POINT ( 'NONE',  ( -78.66644367742111399, 22.32174330031316956, 45.41820113967312977 ) ) ;
#54123 = ADVANCED_FACE ( 'NONE', ( #25973 ), #36872, .T. ) ;
#54124 = CARTESIAN_POINT ( 'NONE',  ( 109.9975424824652777, 172.0000000000000284, 418.0000000000000000 ) ) ;
#54125 = CARTESIAN_POINT ( 'NONE',  ( 40.38132770291768026, 9.553709436640062336, 44.86553172969242098 ) ) ;
#54126 = AXIS2_PLACEMENT_3D ( 'NONE', #14085, #57001, #8819 ) ;
#54127 = EDGE_CURVE ( 'NONE', #54421, #48274, #37548, .T. ) ;
#54128 = CARTESIAN_POINT ( 'NONE',  ( -23.99924996210628336, 8.487987924059023470, 65.54065325144799203 ) ) ;
#54129 = FACE_OUTER_BOUND ( 'NONE', #4770, .T. ) ;
#54130 = VECTOR ( 'NONE', #30244, 1000.000000000000000 ) ;
#54131 = EDGE_CURVE ( 'NONE', #58982, #42757, #4510, .T. ) ;
#54132 = ORIENTED_EDGE ( 'NONE', *, *, #43837, .T. ) ;
#54133 = ORIENTED_EDGE ( 'NONE', *, *, #25292, .F. ) ;
#54134 = DIRECTION ( 'NONE',  ( -0.000000000000000000, 0.000000000000000000, -1.000000000000000000 ) ) ;
#54135 = EDGE_LOOP ( 'NONE', ( #24429, #1238 ) ) ;
#54136 = PLANE ( 'NONE',  #22242 ) ;
#54137 = CARTESIAN_POINT ( 'NONE',  ( 186.3463695477168187, 85.57362603246809840, -92.05568032583515503 ) ) ;
#54138 = CARTESIAN_POINT ( 'NONE',  ( 26.99999999999999645, -27.00000000000000355, 0.000000000000000000 ) ) ;
#54139 = CARTESIAN_POINT ( 'NONE',  ( -4.506365319453815133, 7.705038994660848850, 57.73001332318100509 ) ) ;
#54140 = CARTESIAN_POINT ( 'NONE',  ( -63.33140416796831573, -16.18162651919485739, 43.58025477438756212 ) ) ;
#54141 = DIRECTION ( 'NONE',  ( 1.000000000000000000, 0.000000000000000000, -0.000000000000000000 ) ) ;
#54142 = LINE ( 'NONE', #35677, #63826 ) ;
#54143 = VERTEX_POINT ( 'NONE', #57979 ) ;
#54144 = ORIENTED_EDGE ( 'NONE', *, *, #22305, .F. ) ;
#54145 = CARTESIAN_POINT ( 'NONE',  ( -0.6527133886630325232, 8.860760056385744932, -0.4969600502617563254 ) ) ;
#54146 = LINE ( 'NONE', #37641, #20439 ) ;
#54147 = CARTESIAN_POINT ( 'NONE',  ( 35.00000000000000000, 4.286263797015736496E-15, 0.000000000000000000 ) ) ;
#54148 = CARTESIAN_POINT ( 'NONE',  ( 138.5721691894143532, 44.34516164557648210, -76.22048844638042908 ) ) ;
#54149 = CARTESIAN_POINT ( 'NONE',  ( 68.61679388097590504, 14.04192738700836607, 32.31919998833575391 ) ) ;
#54150 = EDGE_CURVE ( 'NONE', #66496, #9968, #26317, .T. ) ;
#54151 = EDGE_CURVE ( 'NONE', #16482, #9638, #15753, .T. ) ;
#54152 = ORIENTED_EDGE ( 'NONE', *, *, #27843, .T. ) ;
#54153 = ADVANCED_FACE ( 'NONE', ( #58646 ), #26655, .F. ) ;
#54154 = ADVANCED_BREP_SHAPE_REPRESENTATION ( '', ( #40699, #66832 ), #11806 ) ;
#54155 = CARTESIAN_POINT ( 'NONE',  ( 86.15410276028859471, 19.25894675708889991, 2.867536982015614910 ) ) ;
#54156 = ORIENTED_EDGE ( 'NONE', *, *, #35889, .T. ) ;
#54157 = CARTESIAN_POINT ( 'NONE',  ( -74.19961951691010427, 20.67022044985851181, 31.88851621870251307 ) ) ;
#54158 = VERTEX_POINT ( 'NONE', #254 ) ;
#54159 = CIRCLE ( 'NONE', #23878, 5.000000000000000000 ) ;
#54160 = EDGE_LOOP ( 'NONE', ( #5777, #5644, #24092, #49574 ) ) ;
#54161 = CARTESIAN_POINT ( 'NONE',  ( -67.03031041878421092, -33.66749151869542089, 170.0000000000000000 ) ) ;
#54162 = CARTESIAN_POINT ( 'NONE',  ( 91.11342358617753234, 21.00000175105273570, 4.350741119497574694 ) ) ;
#54163 = DIRECTION ( 'NONE',  ( 0.000000000000000000, -0.000000000000000000, -1.000000000000000000 ) ) ;
#54164 = AXIS2_PLACEMENT_3D ( 'NONE', #14347, #30517, #61820 ) ;
#54165 = ORIENTED_EDGE ( 'NONE', *, *, #28236, .F. ) ;
#54166 = CARTESIAN_POINT ( 'NONE',  ( -56.44201257846630426, 32.26641783793562723, 170.0000000000000000 ) ) ;
#54167 = B_SPLINE_CURVE_WITH_KNOTS ( 'NONE', 3,
 ( #63624, #58325, #48436, #37567 ),
 .UNSPECIFIED., .F., .F.,
 ( 4, 4 ),
 ( 9.900409499088329389E-07, 0.05658314289920116785 ),
 .UNSPECIFIED. ) ;
#54168 = AXIS2_PLACEMENT_3D ( 'NONE', #62179, #20305, #13999 ) ;
#54169 = LINE ( 'NONE', #27103, #35727 ) ;
#54170 = CARTESIAN_POINT ( 'NONE',  ( 151.7819978880463907, 53.35998893001570309, 32.01513195124016420 ) ) ;
#54171 = CARTESIAN_POINT ( 'NONE',  ( -180.3114074031036296, 97.09758726817787533, -44.36644437796192619 ) ) ;
#54172 = DIRECTION ( 'NONE',  ( 2.220446049250313081E-16, -0.000000000000000000, 1.000000000000000000 ) ) ;
#54173 = CARTESIAN_POINT ( 'NONE',  ( 10.55634918610406281, 15.55634918610400241, 85.00100000000000477 ) ) ;
#54174 = CARTESIAN_POINT ( 'NONE',  ( 444.9999999999999432, -35.00000000000000000, -2.000000000000000000 ) ) ;
#54175 = ORIENTED_EDGE ( 'NONE', *, *, #30646, .T. ) ;
#54176 = CARTESIAN_POINT ( 'NONE',  ( 136.1215428813736708, 43.99260314811115080, -77.53266360357038423 ) ) ;
#54177 = DIRECTION ( 'NONE',  ( -1.000000000000000000, 0.000000000000000000, 0.000000000000000000 ) ) ;
#54178 = ORIENTED_EDGE ( 'NONE', *, *, #21593, .F. ) ;
#54179 = AXIS2_PLACEMENT_3D ( 'NONE', #10835, #6953, #6250 ) ;
#54180 = FACE_BOUND ( 'NONE', #42569, .T. ) ;
#54181 = CARTESIAN_POINT ( 'NONE',  ( -6.126800896373019611, 6.786243985899685249, -77.07188336801345940 ) ) ;
#54182 = SURFACE_STYLE_FILL_AREA ( #33469 ) ;
#54183 = DIRECTION ( 'NONE',  ( 0.000000000000000000, -5.102127870520020458E-18, -1.000000000000000000 ) ) ;
#54184 = CARTESIAN_POINT ( 'NONE',  ( -124.1095621208148572, 46.52671329146387791, -35.07131596630200221 ) ) ;
#54185 = CARTESIAN_POINT ( 'NONE',  ( -81.24432217070636852, 24.40203426192926628, 18.12073039003383101 ) ) ;
#54186 = DIRECTION ( 'NONE',  ( -0.6427876096865403621, -0.7660444431189770143, 0.000000000000000000 ) ) ;
#54187 = CARTESIAN_POINT ( 'NONE',  ( -154.0718453320783681, 68.14976693162394383, 5.420520227110683820 ) ) ;
#54188 = FACE_OUTER_BOUND ( 'NONE', #31616, .T. ) ;
#54189 = CARTESIAN_POINT ( 'NONE',  ( 68.61679388097593346, 14.04192738700836784, 5.474649397872059176 ) ) ;
#54190 = CARTESIAN_POINT ( 'NONE',  ( 116.5096233816162226, 31.89062767870469273, 6.138510810235731974 ) ) ;
#54191 = CARTESIAN_POINT ( 'NONE',  ( 89.20981392318256553, 21.38519354635265657, -9.430786644822518383 ) ) ;
#54192 = VERTEX_POINT ( 'NONE', #42815 ) ;
#54193 = EDGE_CURVE ( 'NONE', #27319, #49666, #47403, .T. ) ;
#54194 = CARTESIAN_POINT ( 'NONE',  ( 133.8566784816069344, 41.42467568809808398, -89.71241211332301191 ) ) ;
#54195 = ORIENTED_EDGE ( 'NONE', *, *, #30224, .F. ) ;
#54196 = DIRECTION ( 'NONE',  ( 0.000000000000000000, 0.000000000000000000, -1.000000000000000000 ) ) ;
#54197 = LINE ( 'NONE', #64778, #17474 ) ;
#54198 = CARTESIAN_POINT ( 'NONE',  ( 117.6677778655470377, 33.59861415422441411, 89.68390048962857009 ) ) ;
#54199 = CARTESIAN_POINT ( 'NONE',  ( -147.3669217311067712, 63.69361261596462498, 57.87395473753091579 ) ) ;
#54200 = DIRECTION ( 'NONE',  ( -1.000000000000000000, 0.000000000000000000, 0.000000000000000000 ) ) ;
#54201 = CARTESIAN_POINT ( 'NONE',  ( -23.99957301099517082, 9.503061049698471763, -43.79968545520912926 ) ) ;
#54202 = CARTESIAN_POINT ( 'NONE',  ( -47.94536219817736367, 13.92422159065987408, -72.00662047797626997 ) ) ;
#54203 = B_SPLINE_CURVE_WITH_KNOTS ( 'NONE', 3,
 ( #54122, #28107, #59416, #23200, #66129, #64705, #65407, #49550, #59755, #16514, #33045, #1382, #65056, #12640, #65766, #5946, #7371, #1038, #27406, #11227, #22489, #32693, #28465, #55538, #48844, #690, #34103, #22137, #17197, #39030, #60474, #43585, #44646, #17916, #16855, #38669, #60114, #11935, #55187, #33407, #38312, #12288, #54480, #6307, #48493, #54836, #27759 ),
 .UNSPECIFIED., .F., .F.,
 ( 4, 2, 2, 2, 2, 2, 2, 2, 2, 2, 2, 2, 1, 2, 2, 2, 2, 2, 2, 2, 2, 2, 2, 4 ),
 ( 0.000000000000000000, 0.001520400357568945033, 0.002280600536353434571, 0.003040800715137924760, 0.004561201072706896897, 0.005321401251491367571, 0.006081601430275837376, 0.007602001787844763978, 0.008362201966629231181, 0.009122402145413698385, 0.01064280250298265361, 0.01140300268176713816, 0.01216320286055162618, 0.01292340303933611073, 0.01368360321812059875, 0.01520400357568958000, 0.01596420375447406975, 0.01672440393325855951, 0.01824480429082751820, 0.01976520464839648036, 0.02052540482718096318, 0.02128560500596544600, 0.02280600536353444285, 0.02432640572110343971 ),
 .UNSPECIFIED. ) ;
#54204 = CARTESIAN_POINT ( 'NONE',  ( 149.0250918491436778, 6.000000000000000000, -9.435653166495526989 ) ) ;
#54205 = LINE ( 'NONE', #12367, #29661 ) ;
#54206 = VERTEX_POINT ( 'NONE', #10817 ) ;
#54207 = EDGE_LOOP ( 'NONE', ( #43894, #31277, #42128, #5143, #27492, #1501, #36879, #54152, #2228 ) ) ;
#54208 = EDGE_CURVE ( 'NONE', #1836, #51958, #59610, .T. ) ;
#54209 = CARTESIAN_POINT ( 'NONE',  ( 32.89501968360929851, 8.663558833820820482, 68.02007762215981757 ) ) ;
#54210 = CARTESIAN_POINT ( 'NONE',  ( -168.0052514572427071, 83.06849406765624622, 70.65604521105746016 ) ) ;
#54211 = CARTESIAN_POINT ( 'NONE',  ( 442.3372781065085064, 390.0000000000001137, -141.4497041420117398 ) ) ;
#54212 = EDGE_CURVE ( 'NONE', #64129, #2060, #62134, .T. ) ;
#54213 = EDGE_CURVE ( 'NONE', #55507, #14375, #39640, .T. ) ;
#54214 = PRODUCT_DEFINITION_CONTEXT ( 'detailed design', #57460, 'design' ) ;
#54215 = AXIS2_PLACEMENT_3D ( 'NONE', #38553, #1273, #59998 ) ;
#54216 = CARTESIAN_POINT ( 'NONE',  ( -843.0889760620008246, -561.4220607509099636, 10.00000000000000000 ) ) ;
#54217 = ORIENTED_EDGE ( 'NONE', *, *, #4297, .T. ) ;
#54218 = EDGE_CURVE ( 'NONE', #45135, #46531, #11854, .T. ) ;
#54219 = CARTESIAN_POINT ( 'NONE',  ( 284.9998692468128638, 21.99997028336874294, -0.3318949079940898828 ) ) ;
#54220 = CARTESIAN_POINT ( 'NONE',  ( 181.9295958320008140, 80.90438706151871884, -24.34483382478239832 ) ) ;
#54221 = DIRECTION ( 'NONE',  ( -1.000000000000000000, 0.000000000000000000, 0.000000000000000000 ) ) ;
#54222 = CARTESIAN_POINT ( 'NONE',  ( 39.99999999999997868, 29.79383981485517197, -1.218703225458906021E-14 ) ) ;
#54223 = CARTESIAN_POINT ( 'NONE',  ( 46.64694836521739774, 9.462741877720626249, -18.23014210735218654 ) ) ;
#54224 = CARTESIAN_POINT ( 'NONE',  ( 210.6475357757681763, 114.8748261044496388, -21.55495887534324950 ) ) ;
#54225 = DIRECTION ( 'NONE',  ( -9.109522253334613014E-16, -1.000000000000000000, 3.889846672687432470E-31 ) ) ;
#54226 = DIRECTION ( 'NONE',  ( -0.3978785209734125861, -0.9174381082928753095, 0.000000000000000000 ) ) ;
#54227 = AXIS2_PLACEMENT_3D ( 'NONE', #64621, #41791, #63592 ) ;
#54228 = AXIS2_PLACEMENT_3D ( 'NONE', #59166, #6048, #63429 ) ;
#54229 = VERTEX_POINT ( 'NONE', #38240 ) ;
#54230 = CARTESIAN_POINT ( 'NONE',  ( -15.55634918610411077, -41.66904755831209428, 85.00100000000000477 ) ) ;
#54231 = CARTESIAN_POINT ( 'NONE',  ( 94.06416612695406343, 23.16920323269611970, -42.30311029455274507 ) ) ;
#54232 = AXIS2_PLACEMENT_3D ( 'NONE', #26876, #63478, #47624 ) ;
#54233 = CARTESIAN_POINT ( 'NONE',  ( -47.56466076048272384, 13.83435953640667826, 64.17104296208425751 ) ) ;
#54234 = CARTESIAN_POINT ( 'NONE',  ( -63.73419499958998813, 12.83646726144834993, 170.0000000000000000 ) ) ;
#54235 = DIRECTION ( 'NONE',  ( 0.000000000000000000, 0.000000000000000000, 1.000000000000000000 ) ) ;
#54236 = CARTESIAN_POINT ( 'NONE',  ( -26.00000000000002132, 0.000000000000000000, 55.00000000000001421 ) ) ;
#54237 = ORIENTED_EDGE ( 'NONE', *, *, #8961, .F. ) ;
#54238 = EDGE_CURVE ( 'NONE', #57335, #40013, #23475, .T. ) ;
#54239 = DIRECTION ( 'NONE',  ( -1.000000000000000000, 0.000000000000000000, 0.000000000000000000 ) ) ;
#54240 = DIRECTION ( 'NONE',  ( -1.000000000000000000, -0.000000000000000000, -0.000000000000000000 ) ) ;
#54241 = ORIENTED_EDGE ( 'NONE', *, *, #47561, .F. ) ;
#54242 = VERTEX_POINT ( 'NONE', #45256 ) ;
#54243 = CARTESIAN_POINT ( 'NONE',  ( 198.7765072002625288, 98.56267746775340299, 94.99999999999866418 ) ) ;
#54244 = FACE_OUTER_BOUND ( 'NONE', #12604, .T. ) ;
#54245 = CARTESIAN_POINT ( 'NONE',  ( 106.4107271020440209, 27.14892220304137993, 30.65973466290294525 ) ) ;
#54246 = ORIENTED_EDGE ( 'NONE', *, *, #44051, .T. ) ;
#54247 = FACE_OUTER_BOUND ( 'NONE', #36898, .T. ) ;
#54248 = CARTESIAN_POINT ( 'NONE',  ( -49.42000000000000171, -36.09918303830819752, 15.41169613715280562 ) ) ;
#54249 = CARTESIAN_POINT ( 'NONE',  ( 160.4986104110022609, 61.33701824525267199, 43.77471383263033289 ) ) ;
#54250 = CARTESIAN_POINT ( 'NONE',  ( 110.2429982417149432, 29.99119854320847267, 2.766663615273645682 ) ) ;
#54251 = CARTESIAN_POINT ( 'NONE',  ( 0.000000000000000000, 0.000000000000000000, 2.000000000000001776 ) ) ;
#54252 = CARTESIAN_POINT ( 'NONE',  ( -435.1627218934913799, 399.9999999999998295, 96.05029585798821756 ) ) ;
#54253 = CARTESIAN_POINT ( 'NONE',  ( -51.77779688167511551, 14.86590802019197000, -49.46793554282675132 ) ) ;
#54254 = AXIS2_PLACEMENT_3D ( 'NONE', #38495, #11758, #27239 ) ;
#54255 = CARTESIAN_POINT ( 'NONE',  ( 31.11269837220809364, 15.55634918610396866, 0.000000000000000000 ) ) ;
#54256 = CARTESIAN_POINT ( 'NONE',  ( 10.83521140779424208, 7.398743030771590234, 31.86172333737584950 ) ) ;
#54257 = DIRECTION ( 'NONE',  ( 0.000000000000000000, 0.000000000000000000, -1.000000000000000000 ) ) ;
#54258 = CARTESIAN_POINT ( 'NONE',  ( 79.14402072927414622, 17.00139091204388819, 91.48213081605835839 ) ) ;
#54260 = ORIENTED_EDGE ( 'NONE', *, *, #4760, .F. ) ;
#54259 = DIRECTION ( 'NONE',  ( 0.000000000000000000, 0.000000000000000000, -1.000000000000000000 ) ) ;
#54261 = ORIENTED_EDGE ( 'NONE', *, *, #20391, .T. ) ;
#54262 = VECTOR ( 'NONE', #51469, 1000.000000000000000 ) ;
#54263 = ORIENTED_EDGE ( 'NONE', *, *, #55811, .T. ) ;
#54264 = CIRCLE ( 'NONE', #43025, 243.4957430088094839 ) ;
#54265 = CARTESIAN_POINT ( 'NONE',  ( -11.78792974237933322, 7.181513757308651158, -22.44595994035757514 ) ) ;
#54266 = CARTESIAN_POINT ( 'NONE',  ( -55.05276343752909440, 14.68156374112637863, 45.31732777293115788 ) ) ;
#54267 = PLANE ( 'NONE',  #61483 ) ;
#54268 = DIRECTION ( 'NONE',  ( 1.000000000000000000, 0.000000000000000000, 0.000000000000000000 ) ) ;
#54270 = ADVANCED_FACE ( 'NONE', ( #12214 ), #33333, .F. ) ;
#54269 = VECTOR ( 'NONE', #25696, 1000.000000000000000 ) ;
#54271 = CARTESIAN_POINT ( 'NONE',  ( -33.38294402636584124, 10.93918551420889607, 71.82136885757543610 ) ) ;
#54272 = EDGE_CURVE ( 'NONE', #7128, #59178, #55463, .T. ) ;
#54273 = CIRCLE ( 'NONE', #55399, 4.999999999999997335 ) ;
#54274 = DIRECTION ( 'NONE',  ( 0.000000000000000000, 0.000000000000000000, 1.000000000000000000 ) ) ;
#54275 = CARTESIAN_POINT ( 'NONE',  ( 157.4703587214989113, 57.65129005721576760, -77.96873488960135035 ) ) ;
#54276 = CARTESIAN_POINT ( 'NONE',  ( 0.000000000000000000, 0.000000000000000000, 0.000000000000000000 ) ) ;
#54277 = EDGE_LOOP ( 'NONE', ( #33220, #56081, #19413, #60584 ) ) ;
#54278 = EDGE_CURVE ( 'NONE', #57346, #26420, #33682, .T. ) ;
#54279 = VECTOR ( 'NONE', #35676, 1000.000000000000000 ) ;
#54280 = DIRECTION ( 'NONE',  ( -0.000000000000000000, -1.000000000000000000, -0.000000000000000000 ) ) ;
#54281 = ORIENTED_EDGE ( 'NONE', *, *, #21271, .F. ) ;
#54282 = VERTEX_POINT ( 'NONE', #1309 ) ;
#54283 = CARTESIAN_POINT ( 'NONE',  ( 63.99027454648602031, 13.93445177372599098, -23.82830888214883558 ) ) ;
#54284 = PRESENTATION_STYLE_ASSIGNMENT (( #33567 ) ) ;
#54285 = AXIS2_PLACEMENT_3D ( 'NONE', #26118, #4328, #25790 ) ;
#54286 = CARTESIAN_POINT ( 'NONE',  ( -26.44231144410477086, 9.840790913154485509, 85.80307888686122908 ) ) ;
#54287 = LINE ( 'NONE', #22646, #40846 ) ;
#54288 = CARTESIAN_POINT ( 'NONE',  ( -109.3432140528234697, 36.51591785955881875, 13.74895797865885783 ) ) ;
#54289 = DIRECTION ( 'NONE',  ( -0.000000000000000000, -1.000000000000000000, -0.000000000000000000 ) ) ;
#54290 = CARTESIAN_POINT ( 'NONE',  ( 136.7507824285648610, 44.38599729999915411, -9.755793251951397238 ) ) ;
#54291 = ORIENTED_EDGE ( 'NONE', *, *, #36279, .T. ) ;
#54292 = ORIENTED_EDGE ( 'NONE', *, *, #39306, .F. ) ;
#54293 = ORIENTED_EDGE ( 'NONE', *, *, #22396, .F. ) ;
#54294 = FACE_OUTER_BOUND ( 'NONE', #57065, .T. ) ;
#54295 = CARTESIAN_POINT ( 'NONE',  ( -156.4966862384868591, 71.70877417666513054, -12.69550417867896286 ) ) ;
#54296 = CARTESIAN_POINT ( 'NONE',  ( 32.03384598935271299, 8.576372641735986235, -41.65668636982230311 ) ) ;
#54297 = EDGE_CURVE ( 'NONE', #62102, #44967, #5979, .T. ) ;
#54298 = EDGE_CURVE ( 'NONE', #8257, #14673, #52887, .T. ) ;
#54299 = CARTESIAN_POINT ( 'NONE',  ( -37.38262509017738466, 10.64263598035110192, 69.16181315953529918 ) ) ;
#54300 = DIRECTION ( 'NONE',  ( 0.000000000000000000, 0.000000000000000000, 1.000000000000000000 ) ) ;
#54301 = ORIENTED_EDGE ( 'NONE', *, *, #29375, .T. ) ;
#54302 = CARTESIAN_POINT ( 'NONE',  ( 188.0094179620990928, 87.39792407168449984, 60.76004803506884855 ) ) ;
#54303 = CARTESIAN_POINT ( 'NONE',  ( -149.5074843970971017, 64.17983161892347255, 72.56537183036277838 ) ) ;
#54304 = CARTESIAN_POINT ( 'NONE',  ( -2.172839205444464739, 7.595638683704372340, -47.87223819190520402 ) ) ;
#54305 = CARTESIAN_POINT ( 'NONE',  ( 102.7571040248401033, 25.57023079238896912, 10.79413422094299690 ) ) ;
#54306 = CARTESIAN_POINT ( 'NONE',  ( 0.000000000000000000, 70.00000000000000000, 0.000000000000000000 ) ) ;
#54307 = CARTESIAN_POINT ( 'NONE',  ( -84.54326985437107567, 24.64760594531649218, -37.92967292645255384 ) ) ;
#54308 = CARTESIAN_POINT ( 'NONE',  ( 22.29513692215318343, 6.796052026456515627, 60.59742216850811758 ) ) ;
#54309 = DIRECTION ( 'NONE',  ( -1.000000000000000000, 0.000000000000000000, 0.000000000000000000 ) ) ;
#54310 = CARTESIAN_POINT ( 'NONE',  ( 15.78827728214693416, 6.500811158483329244, -62.36349468914946925 ) ) ;
#54311 = B_SPLINE_CURVE_WITH_KNOTS ( 'NONE', 3,
 ( #25300, #56249, #8063, #8419, #13013, #7729, #29872, #40077, #51334, #3480, #61534, #13352, #40765, #24607, #50978, #46040, #24260, #9453, #48099, #4176, #64292, #5208, #52691, #69558, #59006, #47759, #20689, #26662, #30914, #52362, #32290, #15761, #15072, #63949, #21378, #36881, #42821, #37208, #53724, #25646, #4858, #16100, #47076, #41808, #63266, #58655 ),
 .UNSPECIFIED., .F., .F.,
 ( 4, 2, 2, 2, 2, 2, 2, 2, 2, 2, 2, 2, 2, 2, 2, 2, 2, 2, 2, 2, 2, 2, 4 ),
 ( 0.02404638330965504917, 0.02555608299537569239, 0.02631093283823601400, 0.02706578268109633562, 0.02857548236681698231, 0.02933033220967730392, 0.03008518205253762554, 0.03159488173825823754, 0.03310458142397884607, 0.03385943126683915033, 0.03461428110969945460, 0.03612398079542002843, 0.03687883063828029107, 0.03763368048114055370, 0.03838853032400082327, 0.03914338016686108590, 0.04065307985258157647, 0.04216277953830206704, 0.04367247922402255067, 0.04518217890974304124, 0.04593702875260328999, 0.04669187859546353181, 0.04820157828118398075 ),
 .UNSPECIFIED. ) ;
#54312 = B_SPLINE_CURVE_WITH_KNOTS ( 'NONE', 3,
 ( #24298, #61902, #30261, #62618, #51710, #19346, #28876, #13052, #45740, #50327, #23597, #39767, #29216, #66518, #46077, #8457, #67220, #67898, #34511, #55954, #50664, #24987, #45388, #40457, #8809, #8103, #66867, #67548, #18666, #13725, #29910, #51020, #19693, #41158, #61575, #40802, #62257, #14426, #56287, #29553, #56991, #58021, #58688, #69257, #9147 ),
 .UNSPECIFIED., .F., .F.,
 ( 4, 2, 2, 1, 2, 2, 2, 2, 2, 2, 2, 2, 2, 2, 2, 2, 2, 2, 2, 2, 2, 2, 4 ),
 ( 0.02346464386237016517, 0.02493212228186624663, 0.02566586149161428909, 0.02639960070136233156, 0.02713333991111037402, 0.02786707912085841649, 0.02933455754035451182, 0.03006829675010256817, 0.03080203595985062451, 0.03226951437934675454, 0.03300325358909481782, 0.03373699279884288804, 0.03520447121833901460, 0.03667194963783514117, 0.03740568884758318363, 0.03813942805733122610, 0.03960690647682735266, 0.04107438489632347922, 0.04254186331581959885, 0.04327560252556765519, 0.04400934173531571847, 0.04547682015481184503, 0.04694429857430796466 ),
 .UNSPECIFIED. ) ;
#54313 = ORIENTED_EDGE ( 'NONE', *, *, #59918, .F. ) ;
#54315 = DIRECTION ( 'NONE',  ( 0.000000000000000000, 0.000000000000000000, -1.000000000000000000 ) ) ;
#54314 = AXIS2_PLACEMENT_3D ( 'NONE', #21769, #11211, #32679 ) ;
#54316 = APPLICATION_PROTOCOL_DEFINITION ( 'draft international standard', 'automotive_design', 1998, #43056 ) ;
#54317 = CARTESIAN_POINT ( 'NONE',  ( -131.6508182719823594, 50.40277850441010798, -74.09140414498664029 ) ) ;
#54318 = CARTESIAN_POINT ( 'NONE',  ( -130.6002960060536680, 49.67125682092489569, -48.27322245354486796 ) ) ;
#54319 = DIRECTION ( 'NONE',  ( -1.000000000000000000, 0.000000000000000000, 0.000000000000000000 ) ) ;
#54320 = PLANE ( 'NONE',  #60213 ) ;
#54321 = ORIENTED_EDGE ( 'NONE', *, *, #11596, .T. ) ;
#54322 = VECTOR ( 'NONE', #19379, 1000.000000000000000 ) ;
#54323 = VERTEX_POINT ( 'NONE', #49475 ) ;
#54324 = VECTOR ( 'NONE', #41602, 1000.000000000000000 ) ;
#54325 = CARTESIAN_POINT ( 'NONE',  ( -133.1167005700037294, 51.43735670037489172, -94.02487124159708287 ) ) ;
#54326 = VECTOR ( 'NONE', #33850, 1000.000000000000000 ) ;
#54327 = DIRECTION ( 'NONE',  ( 1.000000000000000000, 0.000000000000000000, 0.000000000000000000 ) ) ;
#54328 = ORIENTED_EDGE ( 'NONE', *, *, #50213, .T. ) ;
#54329 = ORIENTED_EDGE ( 'NONE', *, *, #28997, .F. ) ;
#54330 = VECTOR ( 'NONE', #26333, 1000.000000000000000 ) ;
#54331 = CARTESIAN_POINT ( 'NONE',  ( 173.6020601204682805, 71.36108012062136652, -43.12795722065862947 ) ) ;
#54332 = DIRECTION ( 'NONE',  ( 0.1342332658176522420, 0.9909497617679351444, 0.000000000000000000 ) ) ;
#54333 = ORIENTED_EDGE ( 'NONE', *, *, #6991, .F. ) ;
#54334 = CARTESIAN_POINT ( 'NONE',  ( -417.6627218934913230, 397.0710678118655323, 78.55029585798810388 ) ) ;
#54335 = CARTESIAN_POINT ( 'NONE',  ( 136.7690435008551617, 44.39743995805025634, 56.93957293383409279 ) ) ;
#54336 = CARTESIAN_POINT ( 'NONE',  ( -73.10694748374054086, 20.28107308417882493, -47.67311660692905662 ) ) ;
#54337 = AXIS2_PLACEMENT_3D ( 'NONE', #7005, #59412, #27403 ) ;
#54338 = CARTESIAN_POINT ( 'NONE',  ( 80.69264259299148989, 17.48002198187963430, -92.40914142493147665 ) ) ;
#54339 = CARTESIAN_POINT ( 'NONE',  ( 19.78559780309666394, 6.660707902886499276, -90.30598456206999458 ) ) ;
#54340 = B_SPLINE_CURVE_WITH_KNOTS ( 'NONE', 3,
 ( #68942, #20768, #25025, #25718, #24682, #52089, #41195, #62656, #62301, #52762, #68612, #4588, #14112, #46459, #35575, #57371, #57034, #51748, #68280, #35921, #9184, #3554, #3909, #36261, #25378, #20419, #46813, #41883, #30992, #47484, #20084, #15152, #41539, #57718, #14798, #9531, #52439, #36610, #58063, #26057, #56678, #8497, #29949, #26740, #38322, #15835, #10201, #27417, #5615, #37279 ),
 .UNSPECIFIED., .F., .F.,
 ( 4, 2, 2, 2, 2, 2, 2, 2, 2, 2, 2, 2, 2, 2, 2, 2, 2, 2, 2, 2, 2, 2, 2, 2, 4 ),
 ( 0.03126542424884325155, 0.03330676804260264412, 0.03534811183636203669, 0.03738945563012142231, 0.03943079942388081488, 0.04045147132076052504, 0.04147214321764023520, 0.04249281511451994536, 0.04351348701139965552, 0.04555483080515909666, 0.04657550270203882070, 0.04759617459891854474, 0.04810651054735841370, 0.04861684649579828266, 0.04963751839267800670, 0.05065819028955773073, 0.05167886218643745477, 0.05269953408331717881, 0.05372020598019690285, 0.05474087787707662689, 0.05576154977395635093, 0.05780289356771586839, 0.05984423736147539280, 0.06188558115523491721, 0.06392692494899443467 ),
 .UNSPECIFIED. ) ;
#54341 = CARTESIAN_POINT ( 'NONE',  ( -49.43836229152576323, 14.28302414152159372, -20.86921515441098407 ) ) ;
#54342 = ORIENTED_EDGE ( 'NONE', *, *, #39922, .F. ) ;
#54343 = CARTESIAN_POINT ( 'NONE',  ( -121.5677746760273692, 43.71038933438990881, -9.424279492981348483 ) ) ;
#54344 = CARTESIAN_POINT ( 'NONE',  ( 46.66904755831212981, 15.55634918610394379, 2.000000000000001776 ) ) ;
#54345 =( REPRESENTATION_RELATIONSHIP ('NONE','NONE', #40274, #64096 ) REPRESENTATION_RELATIONSHIP_WITH_TRANSFORMATION ( #29779 )SHAPE_REPRESENTATION_RELATIONSHIP( ) );
#54346 = CARTESIAN_POINT ( 'NONE',  ( -142.3260422482980800, 59.60034523324941347, -40.07815075408650074 ) ) ;
#54347 = DIRECTION ( 'NONE',  ( -0.000000000000000000, -0.000000000000000000, -1.000000000000000000 ) ) ;
#54349 = ORIENTED_EDGE ( 'NONE', *, *, #50521, .F. ) ;
#54348 = CARTESIAN_POINT ( 'NONE',  ( 50.57199999999998852, 6.123233995736767268E-16, -5.000000000000000888 ) ) ;
#54350 = CARTESIAN_POINT ( 'NONE',  ( 58.08938767906774103, 12.61185010801509776, 16.14489018905632989 ) ) ;
#54351 = ORIENTED_EDGE ( 'NONE', *, *, #51153, .T. ) ;
#54352 = DIRECTION ( 'NONE',  ( -0.000000000000000000, 0.8660254037844387076, 0.4999999999999998890 ) ) ;
#54353 = DIRECTION ( 'NONE',  ( 0.000000000000000000, 0.000000000000000000, 1.000000000000000000 ) ) ;
#54354 = CARTESIAN_POINT ( 'NONE',  ( -26.83517958587656338, 59.60356471962913361, 41.38025477438755928 ) ) ;
#54355 = CARTESIAN_POINT ( 'NONE',  ( 188.4359598230020083, 86.36951380984521620, -18.39236985717185391 ) ) ;
#54356 = EDGE_CURVE ( 'NONE', #56697, #48044, #49830, .T. ) ;
#54357 = CARTESIAN_POINT ( 'NONE',  ( 86.62931800182293784, 19.42108912189600645, -8.977013608448025650 ) ) ;
#54358 = CARTESIAN_POINT ( 'NONE',  ( 86.62931800182293784, -170.0000000000000000, 64.05663816294301682 ) ) ;
#54360 = CARTESIAN_POINT ( 'NONE',  ( 199.7255144154429445, 99.76581417577200739, 4.229220098907731540 ) ) ;
#54359 = AXIS2_PLACEMENT_3D ( 'NONE', #44942, #13296, #3425 ) ;
#54361 = ADVANCED_FACE ( 'NONE', ( #44914 ), #61097, .T. ) ;
#54362 = CARTESIAN_POINT ( 'NONE',  ( -96.76159256735193992, 30.06445763698410900, 16.27712563862165851 ) ) ;
#54363 = DIRECTION ( 'NONE',  ( -1.000000000000000000, 0.000000000000000000, 0.000000000000000000 ) ) ;
#54364 = VERTEX_POINT ( 'NONE', #11493 ) ;
#54365 = ORIENTED_EDGE ( 'NONE', *, *, #3558, .T. ) ;
#54366 = EDGE_CURVE ( 'NONE', #65444, #454, #6228, .T. ) ;
#54367 = PLANE ( 'NONE',  #4603 ) ;
#54368 = CARTESIAN_POINT ( 'NONE',  ( 9.416603677636258496, 6.380307115728824030, 33.55093279848803434 ) ) ;
#54369 = DIRECTION ( 'NONE',  ( 0.000000000000000000, 0.000000000000000000, 1.000000000000000000 ) ) ;
#54370 = CARTESIAN_POINT ( 'NONE',  ( -5.000000000000026645, -10.55634918610403439, 2.000000000000001776 ) ) ;
#54371 = VECTOR ( 'NONE', #4927, 1000.000000000000000 ) ;
#54372 = CARTESIAN_POINT ( 'NONE',  ( 205.5049354810105910, 109.1776577097390657, -51.32593103262160383 ) ) ;
#54373 = CARTESIAN_POINT ( 'NONE',  ( -72.21947956767110099, 21.03570528348186031, -73.30056851817380448 ) ) ;
#54374 = CARTESIAN_POINT ( 'NONE',  ( 9.068001488962039502, 57.63052748569040062, 27.58472315868180402 ) ) ;
#54375 = AXIS2_PLACEMENT_3D ( 'NONE', #34536, #23280, #17995 ) ;
#54376 = CARTESIAN_POINT ( 'NONE',  ( 45.04506994399701370, 10.22854084020123899, -48.08472337634788119 ) ) ;
#54377 = CARTESIAN_POINT ( 'NONE',  ( 211.8476521439973794, 116.6941316755177382, 65.83984939228595579 ) ) ;
#54378 = ORIENTED_EDGE ( 'NONE', *, *, #57298, .F. ) ;
#54380 = CARTESIAN_POINT ( 'NONE',  ( -102.7456062648101209, 33.01749955571781214, -23.17002667451225406 ) ) ;
#54379 = AXIS2_PLACEMENT_3D ( 'NONE', #14224, #7909, #35687 ) ;
#54381 = EDGE_LOOP ( 'NONE', ( #14359, #56015 ) ) ;
#54382 = CARTESIAN_POINT ( 'NONE',  ( -14.19447842053094178, 7.389800932646227061, -38.94998986089500193 ) ) ;
#54383 = AXIS2_PLACEMENT_3D ( 'NONE', #66501, #34135, #44682 ) ;
#54384 = DIRECTION ( 'NONE',  ( 0.000000000000000000, 0.000000000000000000, 1.000000000000000000 ) ) ;
#54385 = CARTESIAN_POINT ( 'NONE',  ( 90.30732934992394689, 21.77797012484621320, 70.61059424602628098 ) ) ;
#54386 = EDGE_CURVE ( 'NONE', #17804, #16476, #58751, .T. ) ;
#54387 = FACE_OUTER_BOUND ( 'NONE', #180, .T. ) ;
#54388 = DIRECTION ( 'NONE',  ( 0.000000000000000000, 0.000000000000000000, -1.000000000000000000 ) ) ;
#54389 = CARTESIAN_POINT ( 'NONE',  ( 254.4165763529819344, 225.8585178651493948, 128.9999999999999716 ) ) ;
#54390 = CARTESIAN_POINT ( 'NONE',  ( 116.5796390945666019, 33.05011449662006129, -93.07866499088535761 ) ) ;
#54391 = CARTESIAN_POINT ( 'NONE',  ( 210.8249406480391883, 115.1412791740558106, 94.73500360378400842 ) ) ;
#54392 = CARTESIAN_POINT ( 'NONE',  ( 412.3372781065086201, 399.9999999999998863, 113.5502958579881891 ) ) ;
#54393 = VERTEX_POINT ( 'NONE', #3731 ) ;
#54394 = DIRECTION ( 'NONE',  ( -0.000000000000000000, -0.000000000000000000, 1.000000000000000000 ) ) ;
#54395 = DIRECTION ( 'NONE',  ( -0.000000000000000000, -0.000000000000000000, -1.000000000000000000 ) ) ;
#54396 = CARTESIAN_POINT ( 'NONE',  ( -26.87327614295024958, 8.886070347947290671, 16.84225167926756939 ) ) ;
#54397 = CARTESIAN_POINT ( 'NONE',  ( 42.71680114082827373, 9.880016734137543111, -63.21884616217572983 ) ) ;
#54398 = CARTESIAN_POINT ( 'NONE',  ( -0.5158933718595605233, 6.525180340836108428, 39.31287253911112600 ) ) ;
#54399 = CARTESIAN_POINT ( 'NONE',  ( 110.2429982417149574, 29.99119854320844425, -62.76698815611734972 ) ) ;
#54400 = CARTESIAN_POINT ( 'NONE',  ( 93.83003346581507742, 23.08044164087233341, 88.77615774936755599 ) ) ;
#54401 = VERTEX_POINT ( 'NONE', #29776 ) ;
#54402 = DIRECTION ( 'NONE',  ( 9.992007221626795406E-15, -1.000000000000000000, -4.056584128438397956E-15 ) ) ;
#54403 = CARTESIAN_POINT ( 'NONE',  ( -49.42000000000000171, -36.09918303830819752, 15.41169613715280562 ) ) ;
#54404 = CARTESIAN_POINT ( 'NONE',  ( -125.8938041572051389, 46.49392987655491538, 18.77539728269342945 ) ) ;
#54405 = CARTESIAN_POINT ( 'NONE',  ( -165.6208371326873703, 80.58821715390999429, -42.50979365522336195 ) ) ;
#54406 = CARTESIAN_POINT ( 'NONE',  ( -180.3485529394662024, 95.55077600385843084, 89.97650250217222379 ) ) ;
#54407 = ORIENTED_EDGE ( 'NONE', *, *, #53882, .T. ) ;
#54408 = CARTESIAN_POINT ( 'NONE',  ( -118.4622862908118890, 41.79153065058247307, -41.36719475118654543 ) ) ;
#54409 = FACE_OUTER_BOUND ( 'NONE', #49085, .T. ) ;
#54410 = CARTESIAN_POINT ( 'NONE',  ( 133.8566784816069060, 41.42467568809810530, -51.02331093239568816 ) ) ;
#54411 = FACE_OUTER_BOUND ( 'NONE', #18974, .T. ) ;
#54412 = AXIS2_PLACEMENT_3D ( 'NONE', #44159, #43117, #22369 ) ;
#54413 = FACE_OUTER_BOUND ( 'NONE', #20898, .T. ) ;
#54414 = VERTEX_POINT ( 'NONE', #3393 ) ;
#54415 = CARTESIAN_POINT ( 'NONE',  ( 0.000000000000000000, 0.000000000000000000, 2.000000000000001776 ) ) ;
#54416 = CARTESIAN_POINT ( 'NONE',  ( 86.15454111412294935, 20.32174891186167187, 2.867536982015618019 ) ) ;
#54417 = CARTESIAN_POINT ( 'NONE',  ( -17.90772993695011550, -72.84144224619156205, 170.0000000000000000 ) ) ;
#54418 = CARTESIAN_POINT ( 'NONE',  ( 181.0840389613909736, 78.60582251573003987, -78.06960825634331513 ) ) ;
#54419 = AXIS2_PLACEMENT_3D ( 'NONE', #50372, #38775, #7104 ) ;
#54421 = VERTEX_POINT ( 'NONE', #9025 ) ;
#54420 = CARTESIAN_POINT ( 'NONE',  ( 113.8724110608469431, 31.71510301790681652, 3.685887770946741693 ) ) ;
#54422 = ADVANCED_FACE ( 'NONE', ( #18880 ), #51586, .T. ) ;
#54423 = AXIS2_PLACEMENT_3D ( 'NONE', #3128, #12990, #44980 ) ;
#54424 = PLANE ( 'NONE',  #55308 ) ;
#54425 = VECTOR ( 'NONE', #54477, 1000.000000000000114 ) ;
#54426 = ORIENTED_EDGE ( 'NONE', *, *, #45337, .T. ) ;
#54427 = ORIENTED_EDGE ( 'NONE', *, *, #11096, .F. ) ;
#54428 = CARTESIAN_POINT ( 'NONE',  ( -121.5528704565120819, 43.70117646488017016, -89.97093067013521761 ) ) ;
#54429 = VECTOR ( 'NONE', #12495, 1000.000000000000000 ) ;
#54430 = CARTESIAN_POINT ( 'NONE',  ( 141.9165763529819344, -52.00000000000000711, 129.0000000000000000 ) ) ;
#54432 = EDGE_LOOP ( 'NONE', ( #18163, #63492, #22135, #56830, #42657, #67159 ) ) ;
#54431 = CARTESIAN_POINT ( 'NONE',  ( -23.03840347525647658, 9.707315041312055470, 0.000000000000000000 ) ) ;
#54433 = CARTESIAN_POINT ( 'NONE',  ( 160.5141379054754225, 60.05651755415394888, 43.77875689395856540 ) ) ;
#54434 = CARTESIAN_POINT ( 'NONE',  ( 1.667562369267789890, -64.99262834925670518, 170.0000000000000000 ) ) ;
#54435 = DIRECTION ( 'NONE',  ( 1.000000000000000000, 0.000000000000000000, 0.000000000000000000 ) ) ;
#54436 = ORIENTED_EDGE ( 'NONE', *, *, #20313, .T. ) ;
#54437 = CARTESIAN_POINT ( 'NONE',  ( -142.2711026674345760, 59.55689780112353304, -93.96688110664084093 ) ) ;
#54438 = EDGE_CURVE ( 'NONE', #6453, #35701, #61776, .T. ) ;
#54439 = DIRECTION ( 'NONE',  ( -1.156482317317871478E-16, -4.943042645790591857E-17, -1.000000000000000000 ) ) ;
#54440 = CARTESIAN_POINT ( 'NONE',  ( 152.0785009218370760, 53.57704863418404528, -92.08473246085713981 ) ) ;
#54441 = CARTESIAN_POINT ( 'NONE',  ( -38.93878980550034186, 10.94326053663841769, -69.16458801474382767 ) ) ;
#54442 = ORIENTED_EDGE ( 'NONE', *, *, #62514, .F. ) ;
#54443 = ORIENTED_EDGE ( 'NONE', *, *, #39883, .F. ) ;
#54444 = VERTEX_POINT ( 'NONE', #30134 ) ;
#54445 = EDGE_CURVE ( 'NONE', #5653, #50582, #57552, .T. ) ;
#54446 = LINE ( 'NONE', #42857, #5881 ) ;
#54447 = ADVANCED_FACE ( 'NONE', ( #61444 ), #35402, .F. ) ;
#54448 = LINE ( 'NONE', #33015, #56759 ) ;
#54449 = CARTESIAN_POINT ( 'NONE',  ( 2.700000000000004619, 3.024877593893962577E-15, 24.69999999999999929 ) ) ;
#54450 = CARTESIAN_POINT ( 'NONE',  ( -37.79601571721867259, 10.72155118426296561, -38.82969307849655394 ) ) ;
#54451 = CARTESIAN_POINT ( 'NONE',  ( -97.10826110816122991, 30.23021954617678020, 86.26777175360041383 ) ) ;
#54452 = CARTESIAN_POINT ( 'NONE',  ( 0.000000000000000000, 0.000000000000000000, 161.3522585083728700 ) ) ;
#54453 = CARTESIAN_POINT ( 'NONE',  ( 213.7147529443549843, 18.00000000000002132, 277.7621479143228385 ) ) ;
#54454 = DIRECTION ( 'NONE',  ( -0.7660444431189771253, 0.6427876096865404731, 0.000000000000000000 ) ) ;
#54455 = CARTESIAN_POINT ( 'NONE',  ( 79.38459371357852490, 17.07499996355401350, 66.06145663816440106 ) ) ;
#54456 = ORIENTED_EDGE ( 'NONE', *, *, #32879, .T. ) ;
#54457 = CARTESIAN_POINT ( 'NONE',  ( 0.000000000000000000, 0.000000000000000000, 170.0000000000000000 ) ) ;
#54458 = ORIENTED_EDGE ( 'NONE', *, *, #53580, .T. ) ;
#54459 = LINE ( 'NONE', #44264, #47542 ) ;
#54460 = CARTESIAN_POINT ( 'NONE',  ( 209.9944361927103955, 113.8994774711241433, -75.98551876403080030 ) ) ;
#54461 = ADVANCED_FACE ( 'NONE', ( #46290 ), #2705, .T. ) ;
#54462 = FACE_BOUND ( 'NONE', #25930, .T. ) ;
#54464 = FILL_AREA_STYLE_COLOUR ( '', #47188 ) ;
#54463 = VECTOR ( 'NONE', #49168, 1000.000000000000000 ) ;
#54465 = CARTESIAN_POINT ( 'NONE',  ( -32.91766192354460685, 9.838705478717917785, -89.15043209282478642 ) ) ;
#54466 = DIRECTION ( 'NONE',  ( 0.000000000000000000, 0.000000000000000000, 1.000000000000000000 ) ) ;
#54467 = EDGE_CURVE ( 'NONE', #40644, #9181, #8222, .T. ) ;
#54468 = CARTESIAN_POINT ( 'NONE',  ( -4.856322230924655483E-17, 0.3912769056150321445, -8.000000000000000000 ) ) ;
#54469 = EDGE_CURVE ( 'NONE', #59450, #25590, #24396, .T. ) ;
#54471 = CARTESIAN_POINT ( 'NONE',  ( 159.6614743841974757, 60.66237087206235401, -77.65552351392290120 ) ) ;
#54470 = AXIS2_PLACEMENT_3D ( 'NONE', #22288, #38466, #45131 ) ;
#54472 = VECTOR ( 'NONE', #15331, 1000.000000000000000 ) ;
#54473 = ORIENTED_EDGE ( 'NONE', *, *, #29645, .F. ) ;
#54474 = CARTESIAN_POINT ( 'NONE',  ( 41.66904755831212981, 15.55634918610394379, 2.000000000000000000 ) ) ;
#54475 = DIRECTION ( 'NONE',  ( 0.000000000000000000, 0.000000000000000000, 1.000000000000000000 ) ) ;
#54476 = VERTEX_POINT ( 'NONE', #16356 ) ;
#54477 = DIRECTION ( 'NONE',  ( 0.9839295885986321100, -0.1785568947986229116, 0.000000000000000000 ) ) ;
#54478 = CARTESIAN_POINT ( 'NONE',  ( 48.79594074893261535, 16.97828781540491505, 26.66469104408687585 ) ) ;
#54479 = ORIENTED_EDGE ( 'NONE', *, *, #30736, .F. ) ;
#54480 = CARTESIAN_POINT ( 'NONE',  ( -81.01337222286373674, 23.22902179892322749, 30.77879346308872144 ) ) ;
#54481 = AXIS2_PLACEMENT_3D ( 'NONE', #32559, #41735, #32220 ) ;
#54482 = DIRECTION ( 'NONE',  ( 0.000000000000000000, -1.000000000000000000, 0.000000000000000000 ) ) ;
#54483 = CARTESIAN_POINT ( 'NONE',  ( 39.40195752203891999, 9.424259417798149130, 44.91383430596327742 ) ) ;
#54484 = CARTESIAN_POINT ( 'NONE',  ( -23.93965512371324067, 8.480096402797087762, 64.05595943103627121 ) ) ;
#54485 = VECTOR ( 'NONE', #26600, 1000.000000000000000 ) ;
#54486 = CARTESIAN_POINT ( 'NONE',  ( 127.4953815656694758, 37.71366486045443622, -12.67436558192646601 ) ) ;
#54487 = ORIENTED_EDGE ( 'NONE', *, *, #56523, .F. ) ;
#54488 = ORIENTED_EDGE ( 'NONE', *, *, #23576, .F. ) ;
#54489 = DIRECTION ( 'NONE',  ( -0.000000000000000000, -0.000000000000000000, -1.000000000000000000 ) ) ;
#54490 = VERTEX_POINT ( 'NONE', #4765 ) ;
#54491 = FACE_OUTER_BOUND ( 'NONE', #25970, .T. ) ;
#54492 = CARTESIAN_POINT ( 'NONE',  ( 0.000000000000000000, 0.000000000000000000, 170.0000000000000000 ) ) ;
#54493 = CARTESIAN_POINT ( 'NONE',  ( 55.51597771111713797, 11.05737652677075999, 64.65722201551544401 ) ) ;
#54494 = CARTESIAN_POINT ( 'NONE',  ( -1.862553927312063706, 7.582910205528083480, 59.88481149980647444 ) ) ;
#54495 = VERTEX_POINT ( 'NONE', #9711 ) ;
#54496 = CARTESIAN_POINT ( 'NONE',  ( -119.1795380581000359, 42.22910606512926535, -72.61016301487133262 ) ) ;
#54497 = ORIENTED_EDGE ( 'NONE', *, *, #38611, .T. ) ;
#54498 = EDGE_LOOP ( 'NONE', ( #59704, #8871, #59502, #41029 ) ) ;
#54499 = CARTESIAN_POINT ( 'NONE',  ( -2.644994884459115347, 7.710515798486364147, -0.08224679563971236396 ) ) ;
#54500 = DIRECTION ( 'NONE',  ( 0.000000000000000000, 0.000000000000000000, -1.000000000000000000 ) ) ;
#54501 = DIRECTION ( 'NONE',  ( 1.000000000000000000, 0.000000000000000000, 0.000000000000000000 ) ) ;
#54502 = CARTESIAN_POINT ( 'NONE',  ( 135.6842057900327632, 42.53841116629842389, -63.07930687841992068 ) ) ;
#54503 = DIRECTION ( 'NONE',  ( -0.000000000000000000, -0.000000000000000000, -1.000000000000000000 ) ) ;
#54504 = ORIENTED_EDGE ( 'NONE', *, *, #28078, .F. ) ;
#54505 = EDGE_CURVE ( 'NONE', #47103, #31912, #42055, .T. ) ;
#54506 = CARTESIAN_POINT ( 'NONE',  ( 83.60262962804348774, 18.41036205028016326, 3.501146626846444398 ) ) ;
#54507 = ORIENTED_EDGE ( 'NONE', *, *, #59468, .F. ) ;
#54508 = CARTESIAN_POINT ( 'NONE',  ( -71.41745561414263932, 19.69148172991714318, 39.90720259758258237 ) ) ;
#54509 = ORIENTED_EDGE ( 'NONE', *, *, #8756, .F. ) ;
#54510 = EDGE_CURVE ( 'NONE', #52460, #32375, #52604, .T. ) ;
#54511 = AXIS2_PLACEMENT_3D ( 'NONE', #38193, #20723, #65638 ) ;
#54512 = DIRECTION ( 'NONE',  ( 0.000000000000000000, 0.000000000000000000, -1.000000000000000000 ) ) ;
#54513 = AXIS2_PLACEMENT_3D ( 'NONE', #5592, #10874, #27046 ) ;
#54514 = ORIENTED_EDGE ( 'NONE', *, *, #34141, .T. ) ;
#54515 = CARTESIAN_POINT ( 'NONE',  ( 4.000000000000011546, -6.928203230275505220, 0.000000000000000000 ) ) ;
#54516 = DIRECTION ( 'NONE',  ( 0.000000000000000000, 0.000000000000000000, -1.000000000000000000 ) ) ;
#54517 = CARTESIAN_POINT ( 'NONE',  ( -72.29721455218883364, -19.95276341750119897, 0.000000000000000000 ) ) ;
#54518 = AXIS2_PLACEMENT_3D ( 'NONE', #8488, #45417, #55272 ) ;
#54519 = AXIS2_PLACEMENT_3D ( 'NONE', #37044, #33158, #15929 ) ;
#54520 = ORIENTED_EDGE ( 'NONE', *, *, #65020, .F. ) ;
#54521 = AXIS2_PLACEMENT_3D ( 'NONE', #58309, #15751, #24936 ) ;
#54522 = LINE ( 'NONE', #6352, #66019 ) ;
#54523 = ADVANCED_FACE ( 'NONE', ( #63514 ), #63863, .T. ) ;
#54524 = VECTOR ( 'NONE', #57498, 1000.000000000000000 ) ;
#54525 = ADVANCED_FACE ( 'NONE', ( #58913 ), #43075, .T. ) ;
#54526 = CARTESIAN_POINT ( 'NONE',  ( 73.43826238111391547, 0.000000000000000000, 26.24939009510892518 ) ) ;
#54527 = CARTESIAN_POINT ( 'NONE',  ( 33.93974911725172916, 8.773765372885550917, 32.26854139689001499 ) ) ;
#54528 = AXIS2_PLACEMENT_3D ( 'NONE', #45465, #19778, #24720 ) ;
#54529 = CARTESIAN_POINT ( 'NONE',  ( -52.13778968636736977, -39.42540649522066332, 43.58025477438756212 ) ) ;
#54530 = CARTESIAN_POINT ( 'NONE',  ( -133.1093894320205493, 51.43221067881452768, -17.68593715264120192 ) ) ;
#54531 = CARTESIAN_POINT ( 'NONE',  ( -58.33959211651037435, 29.48226216511319464, 43.58025477438756212 ) ) ;
#54532 = LINE ( 'NONE', #42604, #41753 ) ;
#54534 = ORIENTED_EDGE ( 'NONE', *, *, #36949, .F. ) ;
#54533 = EDGE_CURVE ( 'NONE', #5941, #16163, #52094, .T. ) ;
#54535 = CARTESIAN_POINT ( 'NONE',  ( 137.6104751318277124, 44.92718313329109492, -76.86516922214269698 ) ) ;
#54536 = DIRECTION ( 'NONE',  ( 0.000000000000000000, 1.000000000000000000, -0.000000000000000000 ) ) ;
#54537 = ORIENTED_EDGE ( 'NONE', *, *, #27376, .F. ) ;
#54538 = EDGE_CURVE ( 'NONE', #1914, #29362, #11071, .T. ) ;
#54539 = FACE_BOUND ( 'NONE', #33443, .T. ) ;
#54540 = CARTESIAN_POINT ( 'NONE',  ( -1.083610669212420330, 6.545642299653470886, -66.43984342559842560 ) ) ;
#54541 = CARTESIAN_POINT ( 'NONE',  ( -180.2243452982809231, 96.99029284948635166, 67.59096301620702718 ) ) ;
#54542 = CARTESIAN_POINT ( 'NONE',  ( 75.00000000000000000, -1.250000000000021094, 170.0000000000000000 ) ) ;
#54543 = FACE_OUTER_BOUND ( 'NONE', #63287, .T. ) ;
#54544 = CARTESIAN_POINT ( 'NONE',  ( -85.95621526752228192, 26.32462117888281128, 9.292053853339920622 ) ) ;
#54545 = CARTESIAN_POINT ( 'NONE',  ( 132.9440032680862771, 40.87616997986732059, 2.718024143144065707 ) ) ;
#54546 = CARTESIAN_POINT ( 'NONE',  ( 113.9746407525165779, 21.78913134333903301, -3.050900938606327273 ) ) ;
#54547 = CARTESIAN_POINT ( 'NONE',  ( -71.71116731091892404, 19.79303856213887869, -93.48959018091433393 ) ) ;
#54548 = CARTESIAN_POINT ( 'NONE',  ( -12.39770133248888584, 8.241491894828993026, 31.65004457334004329 ) ) ;
#54549 = CARTESIAN_POINT ( 'NONE',  ( 164.9534461562627143, 63.71129898458563190, 9.487489937330947143 ) ) ;
#54550 = CARTESIAN_POINT ( 'NONE',  ( 93.87650740736113164, 23.09802612281733758, -18.47339464351970761 ) ) ;
#54551 = EDGE_LOOP ( 'NONE', ( #34464, #17736, #11388, #7185 ) ) ;
#54552 = CARTESIAN_POINT ( 'NONE',  ( 0.000000000000000000, 0.000000000000000000, 0.000000000000000000 ) ) ;
#54553 = ORIENTED_EDGE ( 'NONE', *, *, #56944, .T. ) ;
#54554 = LINE ( 'NONE', #12358, #34066 ) ;
#54555 = CARTESIAN_POINT ( 'NONE',  ( 83.37782009939533623, 19.39546426214656094, -63.40324210487996481 ) ) ;
#54556 = CARTESIAN_POINT ( 'NONE',  ( 103.8353834748950533, 27.12366330047747454, 94.71338854545251706 ) ) ;
#54557 = DIRECTION ( 'NONE',  ( 1.020422603260505347E-14, -1.000000000000000000, -5.551115123125782702E-17 ) ) ;
#54558 = LINE ( 'NONE', #27840, #60308 ) ;
#54559 = EDGE_CURVE ( 'NONE', #23453, #7404, #1703, .T. ) ;
#54560 = ADVANCED_FACE ( 'NONE', ( #17036 ), #1568, .F. ) ;
#54561 = CARTESIAN_POINT ( 'NONE',  ( -24.71604178686819253, 9.599501655372941755, -46.15064928016835211 ) ) ;
#54562 = PRODUCT_DEFINITION_SHAPE ( 'NONE', 'NONE',  #69618 ) ;
#54563 = CARTESIAN_POINT ( 'NONE',  ( -50.52615126106341137, 14.55080735582892792, -75.56057009363912869 ) ) ;
#54564 = CARTESIAN_POINT ( 'NONE',  ( -72.32580847922558576, 21.07301141147191359, -92.29252585439962786 ) ) ;
#54565 = EDGE_CURVE ( 'NONE', #59604, #44250, #44834, .T. ) ;
#54566 = CARTESIAN_POINT ( 'NONE',  ( -125.8938041572051389, 47.69968343338778283, -23.06915330777029638 ) ) ;
#54567 = ORIENTED_EDGE ( 'NONE', *, *, #66343, .F. ) ;
#54568 = ORIENTED_EDGE ( 'NONE', *, *, #2053, .F. ) ;
#54569 = CARTESIAN_POINT ( 'NONE',  ( 34.82939798935584719, 8.870855050008906062, 70.22358934348724802 ) ) ;
#54570 = CARTESIAN_POINT ( 'NONE',  ( 179.4279766878530040, 76.94722012158231905, 56.32619385280453628 ) ) ;
#54571 = AXIS2_PLACEMENT_3D ( 'NONE', #65199, #53925, #59900 ) ;
#54572 = DIRECTION ( 'NONE',  ( 0.000000000000000000, 0.000000000000000000, 1.000000000000000000 ) ) ;
#54573 = CARTESIAN_POINT ( 'NONE',  ( -172.3127615181936108, 87.73358064377640630, -22.83500978608775256 ) ) ;
#54574 = VECTOR ( 'NONE', #55885, 999.9999999999998863 ) ;
#54575 = CARTESIAN_POINT ( 'NONE',  ( -439.4229916354185548, 395.0000000000065370, -133.9497041420121377 ) ) ;
#54576 = EDGE_LOOP ( 'NONE', ( #17046, #43698, #23221, #36795, #43212, #55315, #5741, #37217, #13620 ) ) ;
#54577 = CARTESIAN_POINT ( 'NONE',  ( 91.12448333640237763, 22.07449368110503229, 4.344509129112214652 ) ) ;
#54578 = AXIS2_PLACEMENT_3D ( 'NONE', #6927, #60394, #1649 ) ;
#54579 = VECTOR ( 'NONE', #10656, 1000.000000000000000 ) ;
#54580 = CARTESIAN_POINT ( 'NONE',  ( -11.57931195747592135, 7.164335452024272577, 70.97150444363501265 ) ) ;
#54581 = CARTESIAN_POINT ( 'NONE',  ( -82.32750425780474757, 23.74963782027935011, -9.207586315752052997 ) ) ;
#54582 = DIRECTION ( 'NONE',  ( -0.000000000000000000, 1.000000000000000000, -0.000000000000000000 ) ) ;
#54583 = CARTESIAN_POINT ( 'NONE',  ( 45.02738683369922512, 9.207938468499236251, -21.24168803743694411 ) ) ;
#54584 = CARTESIAN_POINT ( 'NONE',  ( 210.0292194063021896, 113.9511645670926328, -11.70118341294292286 ) ) ;
#54585 = FACE_BOUND ( 'NONE', #7233, .T. ) ;
#54586 = AXIS2_PLACEMENT_3D ( 'NONE', #12920, #67091, #44912 ) ;
#54587 = CARTESIAN_POINT ( 'NONE',  ( -62.53989795537026453, 16.81768094534200841, -42.21107432078621002 ) ) ;
#54588 = AXIS2_PLACEMENT_3D ( 'NONE', #66263, #16645, #1517 ) ;
#54589 = CIRCLE ( 'NONE', #33273, 4.171999999999999709 ) ;
#54590 = ORIENTED_EDGE ( 'NONE', *, *, #16803, .T. ) ;
#54591 = CARTESIAN_POINT ( 'NONE',  ( -439.4229916354182706, 388.0000000000064801, -123.9497041420119530 ) ) ;
#54592 = CARTESIAN_POINT ( 'NONE',  ( 93.87650740736111743, 23.09802612281734113, -45.31794523398337304 ) ) ;
#54593 = CARTESIAN_POINT ( 'NONE',  ( -51.34542473642582650, 14.75635007918829444, 58.13766928157564706 ) ) ;
#54594 = DIRECTION ( 'NONE',  ( -0.000000000000000000, -0.000000000000000000, -1.000000000000000000 ) ) ;
#54595 = CARTESIAN_POINT ( 'NONE',  ( 206.3053863259449940, 110.3084416756849464, 70.92284527924854842 ) ) ;
#54596 = DIRECTION ( 'NONE',  ( 0.000000000000000000, 0.000000000000000000, 1.000000000000000000 ) ) ;
#54597 = VERTEX_POINT ( 'NONE', #12835 ) ;
#54598 = DIRECTION ( 'NONE',  ( -0.000000000000000000, 1.000000000000000000, 0.000000000000000000 ) ) ;
#54599 = DIRECTION ( 'NONE',  ( -4.565061778886334783E-18, -1.000000000000000000, 0.000000000000000000 ) ) ;
#54600 = ORIENTED_EDGE ( 'NONE', *, *, #45524, .T. ) ;
#54601 = ORIENTED_EDGE ( 'NONE', *, *, #42234, .T. ) ;
#54602 = EDGE_CURVE ( 'NONE', #5602, #23803, #6032, .T. ) ;
#54603 = DIRECTION ( 'NONE',  ( 1.000000000000000000, 0.000000000000000000, 0.000000000000000000 ) ) ;
#54604 = CARTESIAN_POINT ( 'NONE',  ( -63.00000000000000000, 0.000000000000000000, 170.0000000000000000 ) ) ;
#54605 = CARTESIAN_POINT ( 'NONE',  ( 103.1653143050726271, 25.74301230421575681, 39.64379936348838385 ) ) ;
#54606 = ORIENTED_EDGE ( 'NONE', *, *, #35200, .T. ) ;
#54607 = ORIENTED_EDGE ( 'NONE', *, *, #47311, .T. ) ;
#54608 = CARTESIAN_POINT ( 'NONE',  ( 15.55634918610406103, 20.55634918610400064, 0.000000000000000000 ) ) ;
#54609 = CARTESIAN_POINT ( 'NONE',  ( 163.2911130186310515, 63.63047778106599139, 41.64567797802362037 ) ) ;
#54610 = DIRECTION ( 'NONE',  ( 0.000000000000000000, 0.000000000000000000, -1.000000000000000000 ) ) ;
#54611 = CARTESIAN_POINT ( 'NONE',  ( 70.26936813788618963, 15.51386666370915179, 8.498182904468185583 ) ) ;
#54612 = PLANE ( 'NONE',  #56773 ) ;
#54613 = ADVANCED_FACE ( 'NONE', ( #6504 ), #34290, .F. ) ;
#54614 = PRODUCT_DEFINITION_SHAPE ( 'NONE', 'NONE',  #28900 ) ;
#54615 = CARTESIAN_POINT ( 'NONE',  ( 104.3759779378692514, 27.35691041569134185, -11.87929481196654002 ) ) ;
#54616 = AXIS2_PLACEMENT_3D ( 'NONE', #22898, #23605, #55960 ) ;
#54617 = DIRECTION ( 'NONE',  ( 1.000000000000000000, 4.565061778886334783E-18, 0.000000000000000000 ) ) ;
#54618 = FACE_OUTER_BOUND ( 'NONE', #39713, .T. ) ;
#54619 = ADVANCED_FACE ( 'NONE', ( #6140 ), #43768, .T. ) ;
#54620 = CARTESIAN_POINT ( 'NONE',  ( -156.3880368899749840, 71.60874093180113675, -93.00681123627661862 ) ) ;
#54621 = CARTESIAN_POINT ( 'NONE',  ( 311.9975424824652350, 20.00000000000003197, 380.0000000000001137 ) ) ;
#54622 = EDGE_CURVE ( 'NONE', #63051, #9029, #27727, .T. ) ;
#54623 = CARTESIAN_POINT ( 'NONE',  ( 82.33420414567002865, 17.99921649865971673, 84.71689430370859952 ) ) ;
#54624 = AXIS2_PLACEMENT_3D ( 'NONE', #44989, #3137, #61852 ) ;
#54626 = VERTEX_POINT ( 'NONE', #45522 ) ;
#54625 = PLANE ( 'NONE',  #54588 ) ;
#54627 = ORIENTED_EDGE ( 'NONE', *, *, #69173, .F. ) ;
#54628 = AXIS2_PLACEMENT_3D ( 'NONE', #9270, #3999, #25467 ) ;
#54629 = ORIENTED_EDGE ( 'NONE', *, *, #16686, .T. ) ;
#54630 = CARTESIAN_POINT ( 'NONE',  ( -10.23402954931276554, 7.059791383763804440, -8.966552176226290527 ) ) ;
#54631 = DIRECTION ( 'NONE',  ( 0.000000000000000000, 0.000000000000000000, 1.000000000000000000 ) ) ;
#54632 = CARTESIAN_POINT ( 'NONE',  ( 412.3372781065085633, 179.4906275429376024, -144.4497041420117682 ) ) ;
#54633 = FACE_OUTER_BOUND ( 'NONE', #66208, .T. ) ;
#54634 = CARTESIAN_POINT ( 'NONE',  ( 134.3159642998340075, 41.70198410084974938, 56.35489142945900198 ) ) ;
#54635 = CARTESIAN_POINT ( 'NONE',  ( -58.97243502469714826, 16.81420332340175605, -36.31741409159577927 ) ) ;
#54636 = CARTESIAN_POINT ( 'NONE',  ( -14.92860730136983882, 8.468845235798738713, -18.49331991024065758 ) ) ;
#54637 = FACE_OUTER_BOUND ( 'NONE', #56300, .T. ) ;
#54638 = CARTESIAN_POINT ( 'NONE',  ( 3.245026581591060388, 33.26789593292490110, 6.893342931642332694 ) ) ;
#54639 = ORIENTED_EDGE ( 'NONE', *, *, #34088, .F. ) ;
#54640 = VECTOR ( 'NONE', #44009, 1000.000000000000000 ) ;
#54641 = DIRECTION ( 'NONE',  ( -0.3090169943749446757, -0.9510565162951544194, 0.000000000000000000 ) ) ;
#54642 = ORIENTED_EDGE ( 'NONE', *, *, #52551, .F. ) ;
#54643 = ORIENTED_EDGE ( 'NONE', *, *, #56724, .F. ) ;
#54644 = CARTESIAN_POINT ( 'NONE',  ( -142.0729208125266325, 59.40063722436774185, 12.51388629237925265 ) ) ;
#54645 = CARTESIAN_POINT ( 'NONE',  ( 36.85262215550149278, -53.56030941157680303, 0.000000000000000000 ) ) ;
#54646 = DIRECTION ( 'NONE',  ( -1.000000000000000000, 0.000000000000000000, 0.000000000000000000 ) ) ;
#54647 = CARTESIAN_POINT ( 'NONE',  ( -97.88309373898363219, 30.60238467438962218, -48.60923466570785223 ) ) ;
#54648 = EDGE_CURVE ( 'NONE', #20901, #66152, #13181, .T. ) ;
#54649 = CARTESIAN_POINT ( 'NONE',  ( 26.69682282325795697, -59.27986298182186431, 43.58025477438756923 ) ) ;
#54650 = CYLINDRICAL_SURFACE ( 'NONE', #62914, 7.500000000000013323 ) ;
#54651 = EDGE_CURVE ( 'NONE', #60669, #61883, #67004, .T. ) ;
#54652 = CARTESIAN_POINT ( 'NONE',  ( 140.4769819293527178, 46.76840769395177944, -20.21251253278985871 ) ) ;
#54653 = ORIENTED_EDGE ( 'NONE', *, *, #58572, .F. ) ;
#54654 = ORIENTED_EDGE ( 'NONE', *, *, #48961, .T. ) ;
#54655 = ORIENTED_EDGE ( 'NONE', *, *, #16969, .F. ) ;
#54656 = CARTESIAN_POINT ( 'NONE',  ( -12.39413342787890926, 7.231444436041488011, 16.73898743515862009 ) ) ;
#54657 = CARTESIAN_POINT ( 'NONE',  ( 38.42020198992004509, 8.283430712587435352, -77.41584236862877333 ) ) ;
#54658 = CARTESIAN_POINT ( 'NONE',  ( -16.43619359402630664, 18.99971924381106092, 0.000000000000000000 ) ) ;
#54659 = CARTESIAN_POINT ( 'NONE',  ( -38.69408084385327840, 10.89529537250242619, 66.52660731830836482 ) ) ;
#54660 = DIRECTION ( 'NONE',  ( 0.000000000000000000, 0.000000000000000000, -1.000000000000000000 ) ) ;
#54661 = EDGE_LOOP ( 'NONE', ( #63217, #36402, #29271, #4762 ) ) ;
#54662 = CARTESIAN_POINT ( 'NONE',  ( -7.825402957745083654, 6.891034867348166060, -50.41807073194384259 ) ) ;
#54663 = DIRECTION ( 'NONE',  ( -0.000000000000000000, 1.000000000000000000, -0.000000000000000000 ) ) ;
#54664 = DIRECTION ( 'NONE',  ( -1.307628076647265482E-16, -5.414661928692507974E-17, -1.000000000000000000 ) ) ;
#54665 = CARTESIAN_POINT ( 'NONE',  ( -1.095583923122880332, 7.553030873957009561, -39.59844992052428836 ) ) ;
#54666 = CARTESIAN_POINT ( 'NONE',  ( 109.3079614081140818, 28.45126415661783170, 17.72277496343515324 ) ) ;
#54667 = CARTESIAN_POINT ( 'NONE',  ( -166.5704851812740230, 80.12110537694668722, 7.814510292449148743 ) ) ;
#54668 = CARTESIAN_POINT ( 'NONE',  ( -82.32931163805224628, 23.75065981441939655, -49.16463154184398121 ) ) ;
#54669 = FACE_BOUND ( 'NONE', #6550, .T. ) ;
#54670 = DIRECTION ( 'NONE',  ( -1.000000000000000000, 0.000000000000000000, 0.000000000000000000 ) ) ;
#54671 = CARTESIAN_POINT ( 'NONE',  ( 11.21387192505585872, 6.397095920409659797, -75.82701624946969332 ) ) ;
#54672 = CIRCLE ( 'NONE', #62523, 5.000000000000004441 ) ;
#54673 = ORIENTED_EDGE ( 'NONE', *, *, #41535, .F. ) ;
#54674 = VECTOR ( 'NONE', #19206, 1000.000000000000000 ) ;
#54675 = DIRECTION ( 'NONE',  ( 0.000000000000000000, 0.000000000000000000, -1.000000000000000000 ) ) ;
#54676 = CARTESIAN_POINT ( 'NONE',  ( -65.36598343705435354, 0.000000000000000000, 41.38025477438755928 ) ) ;
#54677 = CARTESIAN_POINT ( 'NONE',  ( -131.6133495896317243, 50.37677745548730712, -37.55590930492478208 ) ) ;
#54678 = CARTESIAN_POINT ( 'NONE',  ( 44.86216938219159545, 9.182565662897470560, -75.11176578098715595 ) ) ;
#54679 = LINE ( 'NONE', #6507, #35573 ) ;
#54680 = ORIENTED_EDGE ( 'NONE', *, *, #39883, .T. ) ;
#54681 = AXIS2_PLACEMENT_3D ( 'NONE', #22595, #23649, #65520 ) ;
#54682 = PRODUCT_DEFINITION ( 'UNKNOWN', '', #69200, #52839 ) ;
#54683 = VECTOR ( 'NONE', #33579, 1000.000000000000000 ) ;
#54684 = ORIENTED_EDGE ( 'NONE', *, *, #9538, .F. ) ;
#54685 = CARTESIAN_POINT ( 'NONE',  ( 15.78827728214693416, -170.0000000000000000, 18.17015708224157322 ) ) ;
#54686 = EDGE_CURVE ( 'NONE', #53714, #45779, #56422, .T. ) ;
#54687 = DIRECTION ( 'NONE',  ( -0.3930250316539148359, -0.9195277725514544587, 0.000000000000000000 ) ) ;
#54688 = ORIENTED_EDGE ( 'NONE', *, *, #1850, .F. ) ;
#54689 = ORIENTED_EDGE ( 'NONE', *, *, #26575, .T. ) ;
#54690 = EDGE_CURVE ( 'NONE', #66166, #33134, #18793, .T. ) ;
#54691 = CARTESIAN_POINT ( 'NONE',  ( 173.9288990958749821, 71.66475105971927917, -41.40298165088110238 ) ) ;
#54692 = PLANE ( 'NONE',  #33565 ) ;
#54693 = ORIENTED_EDGE ( 'NONE', *, *, #54829, .F. ) ;
#54694 = CARTESIAN_POINT ( 'NONE',  ( 4.165045035620147829, 64.88046627338042072, 41.38025477438755928 ) ) ;
#54695 = CARTESIAN_POINT ( 'NONE',  ( -76.78936026062119424, 21.61552955137052123, -49.88070520349071302 ) ) ;
#54696 = DIRECTION ( 'NONE',  ( -1.000000000000000000, 0.000000000000000000, 0.000000000000000000 ) ) ;
#54697 = CARTESIAN_POINT ( 'NONE',  ( 22.57527834893889107, 6.812418720475017508, -93.40615590320534523 ) ) ;
#54698 = CARTESIAN_POINT ( 'NONE',  ( -53.13788504024111603, 15.21566150156364650, -23.13923814719157335 ) ) ;
#54699 = EDGE_CURVE ( 'NONE', #53834, #3914, #29693, .T. ) ;
#54700 = ORIENTED_EDGE ( 'NONE', *, *, #68617, .T. ) ;
#54701 = CARTESIAN_POINT ( 'NONE',  ( -122.3745688183166180, 44.21964839958061333, -8.929199399706153173 ) ) ;
#54702 = CYLINDRICAL_SURFACE ( 'NONE', #5519, 9.999999999999994671 ) ;
#54703 = EDGE_CURVE ( 'NONE', #31208, #63543, #68948, .T. ) ;
#54704 = CARTESIAN_POINT ( 'NONE',  ( -143.8756912989386763, 60.83492035645721074, -37.35355894080970529 ) ) ;
#54705 = EDGE_CURVE ( 'NONE', #32490, #34184, #68000, .T. ) ;
#54706 = CYLINDRICAL_SURFACE ( 'NONE', #14040, 65.00000000000000000 ) ;
#54708 = VERTEX_POINT ( 'NONE', #9274 ) ;
#54707 = CARTESIAN_POINT ( 'NONE',  ( -128.7316684282232870, 48.39061963499592878, 84.86076366594872411 ) ) ;
#54709 = DIRECTION ( 'NONE',  ( -1.000000000000000000, 1.232595164407830946E-32, 7.703719777548943412E-34 ) ) ;
#54710 = ORIENTED_EDGE ( 'NONE', *, *, #33673, .F. ) ;
#54711 = CARTESIAN_POINT ( 'NONE',  ( -133.3958821919893012, 51.63629593114585248, 37.60575035420465184 ) ) ;
#54712 = VECTOR ( 'NONE', #46738, 1000.000000000000000 ) ;
#54713 = CYLINDRICAL_SURFACE ( 'NONE', #14242, 65.36598343705435354 ) ;
#54714 = CARTESIAN_POINT ( 'NONE',  ( 38.31361498191044035, 1.250000000000018652, 13.32819299319724493 ) ) ;
#54715 = DIRECTION ( 'NONE',  ( 1.000000000000000000, 0.000000000000000000, 0.000000000000000000 ) ) ;
#54716 = CARTESIAN_POINT ( 'NONE',  ( 85.67452303415197434, 19.09699411916382417, -9.022822218913626457 ) ) ;
#54717 = CIRCLE ( 'NONE', #61470, 20.00000000000000000 ) ;
#54718 = DIRECTION ( 'NONE',  ( 0.000000000000000000, 0.000000000000000000, 1.000000000000000000 ) ) ;
#54719 = FACE_OUTER_BOUND ( 'NONE', #19063, .T. ) ;
#54720 = CARTESIAN_POINT ( 'NONE',  ( 0.000000000000000000, 0.000000000000000000, 40.00000000000003553 ) ) ;
#54721 = CARTESIAN_POINT ( 'NONE',  ( -156.1706799718432421, 70.04375536285918713, -92.55028558477887657 ) ) ;
#54722 = EDGE_LOOP ( 'NONE', ( #16136, #10276, #24912, #8688 ) ) ;
#54723 = ORIENTED_EDGE ( 'NONE', *, *, #50744, .T. ) ;
#54724 = AXIS2_PLACEMENT_3D ( 'NONE', #57968, #38585, #12821 ) ;
#54725 = CARTESIAN_POINT ( 'NONE',  ( -29.47687737404459085, 68.96458294135867106, 0.000000000000000000 ) ) ;
#54726 = CARTESIAN_POINT ( 'NONE',  ( 13.84120792123769306, 6.445822122644894847, 30.25530662355467726 ) ) ;
#54727 = DIRECTION ( 'NONE',  ( 0.000000000000000000, 1.000000000000000000, 0.000000000000000000 ) ) ;
#54728 = LINE ( 'NONE', #39267, #56508 ) ;
#54729 = AXIS2_PLACEMENT_3D ( 'NONE', #32991, #65716, #33357 ) ;
#54730 = CARTESIAN_POINT ( 'NONE',  ( 210.6592759200688079, 116.7161312026394597, -39.26769195576843430 ) ) ;
#54731 = CARTESIAN_POINT ( 'NONE',  ( -71.17846906053300415, 20.67346400882179225, -69.95449947810095637 ) ) ;
#54732 = VECTOR ( 'NONE', #16561, 1000.000000000000000 ) ;
#54733 = CARTESIAN_POINT ( 'NONE',  ( 0.000000000000000000, 0.000000000000000000, 43.58025477438756212 ) ) ;
#54734 = CARTESIAN_POINT ( 'NONE',  ( -23.99924996210628336, 8.487987924059027023, -41.83754911040676916 ) ) ;
#54735 = CARTESIAN_POINT ( 'NONE',  ( -190.6985136298601731, 109.1272424661242582, -19.71767969763411799 ) ) ;
#54736 = ORIENTED_EDGE ( 'NONE', *, *, #32310, .T. ) ;
#54737 = DIRECTION ( 'NONE',  ( 0.000000000000000000, 0.000000000000000000, 1.000000000000000000 ) ) ;
#54738 = ORIENTED_EDGE ( 'NONE', *, *, #17953, .F. ) ;
#54739 = DIRECTION ( 'NONE',  ( 0.000000000000000000, 1.000000000000000000, 0.000000000000000000 ) ) ;
#54740 = CARTESIAN_POINT ( 'NONE',  ( -15.55634918610408945, -31.11269837220804035, 2.000000000000001776 ) ) ;
#54741 = CARTESIAN_POINT ( 'NONE',  ( -81.90266786693713641, 23.58030232261292269, 71.54568514678170743 ) ) ;
#54742 = CARTESIAN_POINT ( 'NONE',  ( 126.6266894765173419, 38.37986986668737899, 39.07338674164753201 ) ) ;
#54743 = CARTESIAN_POINT ( 'NONE',  ( 32.15284246740099405, 8.588257691344878708, 12.50862876416052138 ) ) ;
#54744 = CARTESIAN_POINT ( 'NONE',  ( 22.18075376363927020, -11.79626863379931656, 3.061616997868437868E-16 ) ) ;
#54745 = CARTESIAN_POINT ( 'NONE',  ( 0.000000000000000000, 0.000000000000000000, 40.00000000000003553 ) ) ;
#54746 = LINE ( 'NONE', #23104, #24475 ) ;
#54747 = CARTESIAN_POINT ( 'NONE',  ( 204.4450048848729011, 105.9958458039796341, 82.88260271150369363 ) ) ;
#54748 = CARTESIAN_POINT ( 'NONE',  ( 0.000000000000000000, 192.0000000000000000, 378.0000000000000000 ) ) ;
#54749 = ORIENTED_EDGE ( 'NONE', *, *, #30834, .T. ) ;
#54750 = CARTESIAN_POINT ( 'NONE',  ( 59.72647370436681769, 12.96353798836696569, 70.90221448876295085 ) ) ;
#54751 = CARTESIAN_POINT ( 'NONE',  ( 13.36262230781615479, 7.441298897118794109, -62.74979327901514381 ) ) ;
#54752 = CARTESIAN_POINT ( 'NONE',  ( -13.29455179262032871, 8.319166883236663423, 5.633120552283173765 ) ) ;
#54753 = CARTESIAN_POINT ( 'NONE',  ( 283.3057637310466248, -21.67663200833031922, -3.765392563550209459 ) ) ;
#54754 = DIRECTION ( 'NONE',  ( -3.344045254895050726E-17, -1.000000000000000000, 0.000000000000000000 ) ) ;
#54755 = VERTEX_POINT ( 'NONE', #69396 ) ;
#54756 = CARTESIAN_POINT ( 'NONE',  ( 620.5071894358275131, 928.5915846175167871, 538.2366127225690207 ) ) ;
#54757 = DIRECTION ( 'NONE',  ( 0.000000000000000000, 1.000000000000000000, -0.000000000000000000 ) ) ;
#54758 = CARTESIAN_POINT ( 'NONE',  ( -132.9109786433856755, 51.29129389542019624, 13.93605864163157726 ) ) ;
#54759 = DIRECTION ( 'NONE',  ( -0.000000000000000000, 1.000000000000000000, -0.000000000000000000 ) ) ;
#54760 = EDGE_CURVE ( 'NONE', #11797, #18819, #36708, .T. ) ;
#54761 = CONTEXT_DEPENDENT_SHAPE_REPRESENTATION ( #67849, #20448 ) ;
#54762 = CARTESIAN_POINT ( 'NONE',  ( -133.3316503378477478, 52.82738260200861902, -43.51700776321061426 ) ) ;
#54763 = ORIENTED_EDGE ( 'NONE', *, *, #51474, .F. ) ;
#54764 = CARTESIAN_POINT ( 'NONE',  ( -118.6157340058430094, 41.88485941274768010, -40.58329878568739701 ) ) ;
#54765 = CARTESIAN_POINT ( 'NONE',  ( -4.070918861171931802, 6.675509947362630925, -9.576274108367087479 ) ) ;
#54766 = CIRCLE ( 'NONE', #64922, 1.500000000000001332 ) ;
#54767 = DIRECTION ( 'NONE',  ( -0.000000000000000000, -1.000000000000000000, -0.000000000000000000 ) ) ;
#54768 = EDGE_CURVE ( 'NONE', #43885, #20839, #25470, .T. ) ;
#54769 = CARTESIAN_POINT ( 'NONE',  ( -2.869721780807578781, 7.625909776230886727, -64.11188747930218312 ) ) ;
#54770 = CIRCLE ( 'NONE', #55902, 10.00000000000000355 ) ;
#54771 = ADVANCED_FACE ( 'NONE', ( #5024 ), #15593, .F. ) ;
#54772 =( REPRESENTATION_RELATIONSHIP ('NONE','NONE', #40274, #45625 ) REPRESENTATION_RELATIONSHIP_WITH_TRANSFORMATION ( #53027 )SHAPE_REPRESENTATION_RELATIONSHIP( ) );
#54773 = CARTESIAN_POINT ( 'NONE',  ( 0.000000000000000000, 0.000000000000000000, 43.58025477438756212 ) ) ;
#54774 = ORIENTED_EDGE ( 'NONE', *, *, #42590, .F. ) ;
#54775 = CARTESIAN_POINT ( 'NONE',  ( -59.57462349605619067, 16.98779896904799358, 4.969145654779915766 ) ) ;
#54776 = CARTESIAN_POINT ( 'NONE',  ( 203.1420903260745945, 104.2307086582027154, -36.44445549019010855 ) ) ;
#54777 = AXIS2_PLACEMENT_3D ( 'NONE', #12134, #6847, #54319 ) ;
#54778 = EDGE_CURVE ( 'NONE', #50048, #21528, #47241, .T. ) ;
#54779 = CARTESIAN_POINT ( 'NONE',  ( -97.49665543375859045, 31.53324358035376918, 43.81673036652279052 ) ) ;
#54780 = CARTESIAN_POINT ( 'NONE',  ( 23.03578842369135771, 6.840884649289439956, -44.96429564819586489 ) ) ;
#54781 = VECTOR ( 'NONE', #4620, 1000.000000000000227 ) ;
#54783 = EDGE_LOOP ( 'NONE', ( #10849, #4647, #45244, #19084 ) ) ;
#54782 = CARTESIAN_POINT ( 'NONE',  ( 117.7417271423230147, 33.63613196344608269, 10.80182121036862419 ) ) ;
#54784 = DIRECTION ( 'NONE',  ( 1.000000000000000000, 0.000000000000000000, -0.000000000000000000 ) ) ;
#54785 = VERTEX_POINT ( 'NONE', #58480 ) ;
#54786 = EDGE_LOOP ( 'NONE', ( #60479, #67946, #46968, #37106 ) ) ;
#54787 = VECTOR ( 'NONE', #11997, 1000.000000000000227 ) ;
#54788 = CARTESIAN_POINT ( 'NONE',  ( -75.64857587248467041, 21.19501514561450506, -8.900704809817050034 ) ) ;
#54789 = EDGE_CURVE ( 'NONE', #14795, #30095, #68698, .T. ) ;
#54790 = CYLINDRICAL_SURFACE ( 'NONE', #41655, 7.500000000000020428 ) ;
#54792 = ORIENTED_EDGE ( 'NONE', *, *, #47937, .F. ) ;
#54791 = CARTESIAN_POINT ( 'NONE',  ( -13.77312480593389488, 8.361845410302544579, -74.33815112409169501 ) ) ;
#54793 = CARTESIAN_POINT ( 'NONE',  ( 162.1014732644455307, 61.34312237409763213, 42.82812415200849898 ) ) ;
#54794 = DIRECTION ( 'NONE',  ( -0.9561276726666709802, 0.000000000000000000, -0.2929502919626733037 ) ) ;
#54795 = CARTESIAN_POINT ( 'NONE',  ( 35.54014968547473785, 66.04466488925542933, 43.58025477438756212 ) ) ;
#54796 = VERTEX_POINT ( 'NONE', #37043 ) ;
#54797 = CARTESIAN_POINT ( 'NONE',  ( -145.2564783699978079, 61.95220470181592987, -89.80724196599325637 ) ) ;
#54798 = CARTESIAN_POINT ( 'NONE',  ( -38.54881010929333485, 10.86689971295294477, -13.53486305356366515 ) ) ;
#54799 = B_SPLINE_CURVE_WITH_KNOTS ( 'NONE', 3,
 ( #52370, #47086, #18631, #15768, #64655, #26332, #4865, #47770, #57994, #55037, #36889, #63956, #63274, #27007, #42159, #36545, #37566, #58666, #69226, #21056, #31953, #37917, #59361, #31601, #42828, #43177, #16461, #21727, #272, #25991, #20699, #42502, #15083, #37215, #28310, #12146, #10832, #53731, #10484, #53383, #5214, #26673, #48435, #48108 ),
 .UNSPECIFIED., .F., .F.,
 ( 4, 2, 2, 2, 2, 2, 2, 2, 2, 2, 2, 2, 2, 2, 2, 2, 2, 2, 2, 2, 2, 4 ),
 ( 7.757919228897728493E-18, 0.003360573201437767454, 0.004200716501797173430, 0.005040859802156579840, 0.006721146402875345822, 0.007561289703234706262, 0.008401433003594062365, 0.009241576303953422805, 0.01008171960431278324, 0.01176200620503151974, 0.01260214950539088018, 0.01344229280575023888, 0.01428243610610959932, 0.01512257940646895803, 0.01680286600718770146, 0.01764300930754707578, 0.01848315260790645009, 0.02016343920862517791, 0.02184372580934390573, 0.02352401241006263355, 0.02520429901078136137, 0.02688458561150008919 ),
 .UNSPECIFIED. ) ;
#54800 = CARTESIAN_POINT ( 'NONE',  ( -176.3856149167965555, 92.38076834121982017, 45.08818581386256596 ) ) ;
#54801 = DIRECTION ( 'NONE',  ( -0.000000000000000000, 1.000000000000000000, -0.000000000000000000 ) ) ;
#54802 = CARTESIAN_POINT ( 'NONE',  ( 22.90619343622340764, 7.840927939412484449, 61.94537535831524622 ) ) ;
#54803 = ORIENTED_EDGE ( 'NONE', *, *, #62281, .T. ) ;
#54804 = ORIENTED_EDGE ( 'NONE', *, *, #22449, .T. ) ;
#54805 = ORIENTED_EDGE ( 'NONE', *, *, #26324, .T. ) ;
#54806 = CARTESIAN_POINT ( 'NONE',  ( 35.39413431650373099, 0.000000000000000000, -5.000000000000000000 ) ) ;
#54807 = DIRECTION ( 'NONE',  ( -0.7071067811865474617, 9.422489238170280455E-15, 0.7071067811865475727 ) ) ;
#54808 = FILL_AREA_STYLE ('',( #58694 ) ) ;
#54809 = CARTESIAN_POINT ( 'NONE',  ( -34.74312654625182972, 10.15703162223800682, -49.55465837260248918 ) ) ;
#54810 = CARTESIAN_POINT ( 'NONE',  ( 0.000000000000000000, 0.000000000000000000, 85.00000000000000000 ) ) ;
#54811 = FACE_OUTER_BOUND ( 'NONE', #62509, .T. ) ;
#54812 = DIRECTION ( 'NONE',  ( 1.000000000000000000, 0.000000000000000000, 0.000000000000000000 ) ) ;
#54813 = CARTESIAN_POINT ( 'NONE',  ( -61.84115830117593759, 17.65779703603521256, 94.71171141969601592 ) ) ;
#54814 = CARTESIAN_POINT ( 'NONE',  ( 79.38020582286196714, 17.07365509555548755, 62.06798524717918752 ) ) ;
#54815 = EDGE_LOOP ( 'NONE', ( #10090, #49534, #50251, #33847 ) ) ;
#54816 = VECTOR ( 'NONE', #42897, 1000.000000000000000 ) ;
#54817 = LINE ( 'NONE', #38652, #64437 ) ;
#54818 = SURFACE_STYLE_FILL_AREA ( #65392 ) ;
#54819 = ORIENTED_EDGE ( 'NONE', *, *, #64391, .F. ) ;
#54820 = CARTESIAN_POINT ( 'NONE',  ( 185.1647878987785987, 82.82967084668430857, 30.50037864223945405 ) ) ;
#54821 = LINE ( 'NONE', #6643, #18641 ) ;
#54822 = AXIS2_PLACEMENT_3D ( 'NONE', #68375, #26748, #14215 ) ;
#54823 = CARTESIAN_POINT ( 'NONE',  ( -71.37402418445427088, 19.67651958824262692, 9.303105102284899175 ) ) ;
#54824 = CARTESIAN_POINT ( 'NONE',  ( -118.8392474096542202, 43.20060570451234128, 62.36526549987367929 ) ) ;
#54825 = CARTESIAN_POINT ( 'NONE',  ( -48.57297291660696459, 13.03920345822339044, 7.163779599053963665 ) ) ;
#54826 = CARTESIAN_POINT ( 'NONE',  ( -40.99999999999999289, 0.000000000000000000, 55.00000000000001421 ) ) ;
#54827 = FACE_OUTER_BOUND ( 'NONE', #11692, .T. ) ;
#54828 = ORIENTED_EDGE ( 'NONE', *, *, #69547, .F. ) ;
#54829 = EDGE_CURVE ( 'NONE', #6792, #60434, #26145, .T. ) ;
#54830 = CYLINDRICAL_SURFACE ( 'NONE', #39797, 7.500000000000013323 ) ;
#54831 = DIRECTION ( 'NONE',  ( 1.000000000000000000, 0.000000000000000000, 0.000000000000000000 ) ) ;
#54832 = EDGE_LOOP ( 'NONE', ( #62255, #67781, #39672, #9977 ) ) ;
#54833 = CYLINDRICAL_SURFACE ( 'NONE', #45459, 7.500000000000020428 ) ;
#54834 = FACE_OUTER_BOUND ( 'NONE', #7425, .T. ) ;
#54835 = EDGE_LOOP ( 'NONE', ( #42998, #24975, #7058, #42225 ) ) ;
#54836 = CARTESIAN_POINT ( 'NONE',  ( -79.14127775978546708, 22.50259208414363599, 30.41820113967310490 ) ) ;
#54837 = CARTESIAN_POINT ( 'NONE',  ( -24.32776401346968953, 9.546905915310571089, -67.22867289442208971 ) ) ;
#54838 = CARTESIAN_POINT ( 'NONE',  ( 45.04020069093783007, 10.22779424730543063, 42.38369278573359367 ) ) ;
#54839 = DIRECTION ( 'NONE',  ( -0.000000000000000000, 1.000000000000000000, -0.000000000000000000 ) ) ;
#54840 = VECTOR ( 'NONE', #66363, 1000.000000000000000 ) ;
#54841 = VERTEX_POINT ( 'NONE', #42660 ) ;
#54842 = ORIENTED_EDGE ( 'NONE', *, *, #20313, .F. ) ;
#54843 = CARTESIAN_POINT ( 'NONE',  ( -65.36598343705435354, 0.000000000000000000, 41.38025477438755928 ) ) ;
#54844 = ORIENTED_EDGE ( 'NONE', *, *, #33829, .T. ) ;
#54845 = CARTESIAN_POINT ( 'NONE',  ( 32.29578462738145817, 8.602609172809795979, -13.86424321593882070 ) ) ;
#54846 = DIRECTION ( 'NONE',  ( 1.000000000000000000, -1.421085471520200372E-14, 0.000000000000000000 ) ) ;
#54847 = CARTESIAN_POINT ( 'NONE',  ( -17.50000000000002842, -18.06806526123148160, -2.000000000000000000 ) ) ;
#54848 = CARTESIAN_POINT ( 'NONE',  ( -0.7211439451572413395, 7.539282923622935506, 66.87669417409435368 ) ) ;
#54849 = DIRECTION ( 'NONE',  ( 0.000000000000000000, 0.000000000000000000, 1.000000000000000000 ) ) ;
#54850 = EDGE_CURVE ( 'NONE', #16148, #23177, #20510, .T. ) ;
#54851 = LINE ( 'NONE', #1054, #14679 ) ;
#54852 = ORIENTED_EDGE ( 'NONE', *, *, #62489, .T. ) ;
#54853 = CARTESIAN_POINT ( 'NONE',  ( -119.2982054035571196, 42.30181775808006961, -72.83786828249223788 ) ) ;
#54854 = ORIENTED_EDGE ( 'NONE', *, *, #34901, .F. ) ;
#54855 = ORIENTED_EDGE ( 'NONE', *, *, #13214, .T. ) ;
#54856 = CARTESIAN_POINT ( 'NONE',  ( 164.9709596662455624, 63.72607097915132357, -16.51597377340664252 ) ) ;
#54857 = FACE_OUTER_BOUND ( 'NONE', #45089, .T. ) ;
#54858 = LINE ( 'NONE', #22168, #17231 ) ;
#54859 = CARTESIAN_POINT ( 'NONE',  ( 136.9654665832768217, 44.52067472585214603, 16.99517226826078797 ) ) ;
#54860 = EDGE_CURVE ( 'NONE', #35681, #60290, #53196, .T. ) ;
#54861 = CARTESIAN_POINT ( 'NONE',  ( -55.15976438495155776, 34.41253982194033512, 41.38025477438755928 ) ) ;
#54862 = EDGE_LOOP ( 'NONE', ( #6638, #29764, #39484, #22906 ) ) ;
#54863 = DIRECTION ( 'NONE',  ( 0.000000000000000000, 0.000000000000000000, 1.000000000000000000 ) ) ;
#54864 = ORIENTED_EDGE ( 'NONE', *, *, #4360, .T. ) ;
#54866 = DIRECTION ( 'NONE',  ( 0.000000000000000000, 0.000000000000000000, -1.000000000000000000 ) ) ;
#54865 = AXIS2_PLACEMENT_3D ( 'NONE', #54230, #16952, #38420 ) ;
#54867 = ORIENTED_EDGE ( 'NONE', *, *, #65296, .T. ) ;
#54868 = CARTESIAN_POINT ( 'NONE',  ( 127.5843554582764057, 37.76388480628244793, -93.07977588763110077 ) ) ;
#54869 = EDGE_CURVE ( 'NONE', #51453, #17220, #19504, .T. ) ;
#54870 = CONICAL_SURFACE ( 'NONE', #39184, 65.00000000000000000, 0.7853981633974497223 ) ;
#54871 = ORIENTED_EDGE ( 'NONE', *, *, #66115, .F. ) ;
#54872 = LINE ( 'NONE', #7405, #11694 ) ;
#54873 = ADVANCED_FACE ( 'NONE', ( #32114, #36354 ), #53547, .F. ) ;
#54874 = CARTESIAN_POINT ( 'NONE',  ( 2.112947028648761272, 24.91054906769654664, 0.000000000000000000 ) ) ;
#54875 = AXIS2_PLACEMENT_3D ( 'NONE', #32331, #43901, #63986 ) ;
#54876 = DIRECTION ( 'NONE',  ( 0.000000000000000000, 0.000000000000000000, 1.000000000000000000 ) ) ;
#54877 = VERTEX_POINT ( 'NONE', #64461 ) ;
#54878 = DIRECTION ( 'NONE',  ( 0.000000000000000000, 0.000000000000000000, 1.000000000000000000 ) ) ;
#54879 = CARTESIAN_POINT ( 'NONE',  ( 422.4999999999999432, 207.5000000000000284, 20.00000000000000000 ) ) ;
#54880 = CARTESIAN_POINT ( 'NONE',  ( 32.66883187925818532, 8.640402022338106391, 34.07364008131894195 ) ) ;
#54881 = CARTESIAN_POINT ( 'NONE',  ( -174.7817412490652202, 90.52199442492063497, -49.53788585594068650 ) ) ;
#54882 = CARTESIAN_POINT ( 'NONE',  ( 0.000000000000000000, 100.0000000000000000, 0.000000000000000000 ) ) ;
#54883 = DIRECTION ( 'NONE',  ( 0.000000000000000000, 0.000000000000000000, 1.000000000000000000 ) ) ;
#54884 = LINE ( 'NONE', #6707, #18165 ) ;
#54885 = ORIENTED_EDGE ( 'NONE', *, *, #41385, .T. ) ;
#54886 = DIRECTION ( 'NONE',  ( 1.000000000000000000, 0.000000000000000000, 0.000000000000000000 ) ) ;
#54887 = CARTESIAN_POINT ( 'NONE',  ( -147.1538409485623049, 63.51600817366544049, -76.28201582439264428 ) ) ;
#54888 = ORIENTED_EDGE ( 'NONE', *, *, #17807, .T. ) ;
#54889 = FACE_BOUND ( 'NONE', #45580, .T. ) ;
#54890 = CARTESIAN_POINT ( 'NONE',  ( -7.330690860789854213, 6.858814156830895570, -62.26262132240749025 ) ) ;
#54891 = CARTESIAN_POINT ( 'NONE',  ( -180.5234362879040191, 97.35934147644944403, 66.41375281865778391 ) ) ;
#54892 = FACE_OUTER_BOUND ( 'NONE', #19441, .T. ) ;
#54893 = CARTESIAN_POINT ( 'NONE',  ( -122.3759299995709853, 45.41285412136511468, -49.05442115285750759 ) ) ;
#54894 = CARTESIAN_POINT ( 'NONE',  ( -0.3252226420479328306, 7.525368746738511305, 37.12884226405564903 ) ) ;
#54895 = CARTESIAN_POINT ( 'NONE',  ( -11.84006471019700335, 7.185574865082572593, -90.25816456928032494 ) ) ;
#54896 = CARTESIAN_POINT ( 'NONE',  ( 113.0554507864566318, 21.63937313260594664, 3.971423903130212985 ) ) ;
#54897 = CARTESIAN_POINT ( 'NONE',  ( -119.1605144823340652, 43.39823405392967715, -72.57201457058890526 ) ) ;
#54898 = CARTESIAN_POINT ( 'NONE',  ( -14.84903512415885452, 8.461292896365067762, 40.25741089538951201 ) ) ;
#54899 = CARTESIAN_POINT ( 'NONE',  ( 164.0298848570286907, 62.93631132702877551, 13.74007122767754652 ) ) ;
#54900 = LINE ( 'NONE', #19974, #6165 ) ;
#54901 = VERTEX_POINT ( 'NONE', #16272 ) ;
#54902 = CARTESIAN_POINT ( 'NONE',  ( -35.99414836699283882, 11.40630460607619590, 4.893268811183970612 ) ) ;
#54903 = ORIENTED_EDGE ( 'NONE', *, *, #15008, .F. ) ;
#54904 = FACE_OUTER_BOUND ( 'NONE', #19576, .T. ) ;
#54905 = DIRECTION ( 'NONE',  ( -1.000000000000000000, 0.000000000000000000, 0.000000000000000000 ) ) ;
#54906 = CARTESIAN_POINT ( 'NONE',  ( 113.3877257111496846, 31.48076025743010931, 83.98386345913559126 ) ) ;
#54907 = CARTESIAN_POINT ( 'NONE',  ( 100.0000000000000284, 5.000000000000000000, 21.42428528562851753 ) ) ;
#54908 = DIRECTION ( 'NONE',  ( 0.000000000000000000, 0.000000000000000000, -1.000000000000000000 ) ) ;
#54909 = FACE_OUTER_BOUND ( 'NONE', #17319, .T. ) ;
#54910 = CARTESIAN_POINT ( 'NONE',  ( 0.08224679563971232232, 6.145890662064651622, -5.355005115540898863 ) ) ;
#54911 = EDGE_CURVE ( 'NONE', #44954, #40902, #20141, .T. ) ;
#54912 = CYLINDRICAL_SURFACE ( 'NONE', #61131, 5.000000000000000888 ) ;
#54913 = CARTESIAN_POINT ( 'NONE',  ( -4.238248324054826099, 66.51046413633903853, 34.48241823979277143 ) ) ;
#54914 = ORIENTED_EDGE ( 'NONE', *, *, #12242, .T. ) ;
#54915 = ORIENTED_EDGE ( 'NONE', *, *, #19934, .T. ) ;
#54916 = CARTESIAN_POINT ( 'NONE',  ( 35.44311777160621091, 8.940232499250161169, 70.63318520892174490 ) ) ;
#54917 = CARTESIAN_POINT ( 'NONE',  ( 55.65793654284683356, -50.28674377798225947, 43.58025477438756212 ) ) ;
#54918 = FACE_OUTER_BOUND ( 'NONE', #58586, .T. ) ;
#54919 = EDGE_CURVE ( 'NONE', #15010, #41004, #6417, .T. ) ;
#54920 =( NAMED_UNIT ( * ) SI_UNIT ( $, .STERADIAN. ) SOLID_ANGLE_UNIT ( ) );
#54921 = CARTESIAN_POINT ( 'NONE',  ( 0.000000000000000000, 65.13282190615278466, -5.000000000000000000 ) ) ;
#54922 = B_SPLINE_CURVE_WITH_KNOTS ( 'NONE', 3,
 ( #39422, #65468, #55244, #22547 ),
 .UNSPECIFIED., .F., .F.,
 ( 4, 4 ),
 ( 9.900409499066787224E-07, 0.05658314289920114010 ),
 .UNSPECIFIED. ) ;
#54923 = CIRCLE ( 'NONE', #38209, 185.0000000000000000 ) ;
#54924 = CIRCLE ( 'NONE', #41485, 498.0000000000000000 ) ;
#54925 = CARTESIAN_POINT ( 'NONE',  ( -39.29440389294403246, -17.09499999999999886, 4.000000000000000000 ) ) ;
#54926 = ORIENTED_EDGE ( 'NONE', *, *, #65993, .F. ) ;
#54927 = AXIS2_PLACEMENT_3D ( 'NONE', #66834, #44297, #13354 ) ;
#54928 = CARTESIAN_POINT ( 'NONE',  ( 105.8229724512851817, 27.98935528750253710, -49.48651744878882397 ) ) ;
#54929 = CARTESIAN_POINT ( 'NONE',  ( 23.24047374271772881, 7.861801299833791390, -42.03981132063025683 ) ) ;
#54930 = CARTESIAN_POINT ( 'NONE',  ( -86.09999398724997377, 25.29376521564880420, -14.74247839810679572 ) ) ;
#54931 = DIRECTION ( 'NONE',  ( -1.000000000000000000, 0.000000000000000000, 0.000000000000000000 ) ) ;
#54932 = DIRECTION ( 'NONE',  ( 0.9362348706397417564, -0.3513748240813305279, 0.000000000000000000 ) ) ;
#54933 = CARTESIAN_POINT ( 'NONE',  ( 211.5175447467296408, 116.1901475271413915, -13.84624472280481200 ) ) ;
#54934 = FACE_BOUND ( 'NONE', #55750, .T. ) ;
#54935 = EDGE_CURVE ( 'NONE', #29393, #26090, #33515, .T. ) ;
#54936 = CARTESIAN_POINT ( 'NONE',  ( -61.75629144857964548, 16.58190704077737720, -39.34366674388692786 ) ) ;
#54937 = EDGE_CURVE ( 'NONE', #55648, #65743, #1486, .T. ) ;
#54938 = EDGE_CURVE ( 'NONE', #3736, #63617, #9422, .T. ) ;
#54939 = VERTEX_POINT ( 'NONE', #795 ) ;
#54940 = CARTESIAN_POINT ( 'NONE',  ( 154.4165763529819628, -26.99999999999998224, 138.9999999999999716 ) ) ;
#54941 = DIRECTION ( 'NONE',  ( -0.000000000000000000, -0.000000000000000000, 1.000000000000000000 ) ) ;
#54942 = CARTESIAN_POINT ( 'NONE',  ( -52.68206656346372796, 15.09776187114413482, 71.78146491162712550 ) ) ;
#54943 = CARTESIAN_POINT ( 'NONE',  ( -23.14886993799584047, 9.760512885996790899, 3.061616997868437868E-16 ) ) ;
#54944 = EDGE_CURVE ( 'NONE', #44265, #43935, #4885, .T. ) ;
#54945 = CARTESIAN_POINT ( 'NONE',  ( 154.4429418375333114, 55.33424769452795999, 3.188201469828449319 ) ) ;
#54946 = FACE_OUTER_BOUND ( 'NONE', #37050, .T. ) ;
#54947 = ORIENTED_EDGE ( 'NONE', *, *, #56614, .F. ) ;
#54948 = CARTESIAN_POINT ( 'NONE',  ( 57.08336938683662964, 11.37442068895388836, 15.08384692392094450 ) ) ;
#54949 = DIRECTION ( 'NONE',  ( 1.000000000000000000, 0.000000000000000000, 0.000000000000000000 ) ) ;
#54950 = VERTEX_POINT ( 'NONE', #28569 ) ;
#54951 = ORIENTED_EDGE ( 'NONE', *, *, #5859, .F. ) ;
#54952 = DIRECTION ( 'NONE',  ( 1.000000000000000000, 0.000000000000000000, 0.000000000000000000 ) ) ;
#54953 = CARTESIAN_POINT ( 'NONE',  ( -47.92160639629907593, -33.27200008537087683, 27.58472315868179692 ) ) ;
#54954 = CARTESIAN_POINT ( 'NONE',  ( 107.0471828278921009, 27.43080724084234134, 43.91305964950614538 ) ) ;
#54956 = ORIENTED_EDGE ( 'NONE', *, *, #46561, .F. ) ;
#54955 = EDGE_CURVE ( 'NONE', #22638, #22983, #1141, .T. ) ;
#54957 = EDGE_LOOP ( 'NONE', ( #31021, #20341, #38295, #24315 ) ) ;
#54958 = DIRECTION ( 'NONE',  ( 0.000000000000000000, 0.000000000000000000, 1.000000000000000000 ) ) ;
#54959 = AXIS2_PLACEMENT_3D ( 'NONE', #2399, #66086, #44247 ) ;
#54960 = EDGE_CURVE ( 'NONE', #58410, #16538, #22592, .T. ) ;
#54962 = EDGE_CURVE ( 'NONE', #21605, #35550, #55291, .T. ) ;
#54961 = CARTESIAN_POINT ( 'NONE',  ( 159.2258951716709987, 60.31399909112332125, 29.60431511090013856 ) ) ;
#54963 = ADVANCED_FACE ( 'NONE', ( #34897 ), #56005, .F. ) ;
#54964 = DIRECTION ( 'NONE',  ( 1.000000000000000000, 0.000000000000000000, 0.000000000000000000 ) ) ;
#54965 = CARTESIAN_POINT ( 'NONE',  ( 70.11969827741711470, 15.47408882293424703, 12.92314886639808869 ) ) ;
#54966 = LINE ( 'NONE', #64836, #36535 ) ;
#54967 = CARTESIAN_POINT ( 'NONE',  ( -50.52615126106343268, 14.55080735582893325, -48.71601950317546681 ) ) ;
#54968 = CARTESIAN_POINT ( 'NONE',  ( -48.23389383802711450, 13.99288361739331066, 7.839931237048672230 ) ) ;
#54969 = CARTESIAN_POINT ( 'NONE',  ( -132.4896623150434039, 52.22616402022728721, -11.98991211083652075 ) ) ;
#54970 = DIRECTION ( 'NONE',  ( -1.000000000000000000, 0.000000000000000000, 0.000000000000000000 ) ) ;
#54971 = LINE ( 'NONE', #59543, #16938 ) ;
#54972 = CARTESIAN_POINT ( 'NONE',  ( 85.04740456388582004, 18.88715044253751429, 83.56261749178500509 ) ) ;
#54974 = VERTEX_POINT ( 'NONE', #67267 ) ;
#54973 = LINE ( 'NONE', #28242, #6285 ) ;
#54975 = VERTEX_POINT ( 'NONE', #2881 ) ;
#54976 = AXIS2_PLACEMENT_3D ( 'NONE', #36360, #20868, #5032 ) ;
#54977 = ORIENTED_EDGE ( 'NONE', *, *, #48424, .F. ) ;
#54978 = DIRECTION ( 'NONE',  ( 0.000000000000000000, 0.000000000000000000, -1.000000000000000000 ) ) ;
#54979 = CARTESIAN_POINT ( 'NONE',  ( -167.9514378334966977, 83.01160612846800291, 86.56910000124806004 ) ) ;
#54980 = CARTESIAN_POINT ( 'NONE',  ( 5.799999999999999822, 8.000000000000000000, 0.000000000000000000 ) ) ;
#54981 = CARTESIAN_POINT ( 'NONE',  ( 109.7724924842966203, 28.66436020578543875, -9.077886975190001095 ) ) ;
#54982 = CARTESIAN_POINT ( 'NONE',  ( -62.49137879463569334, 17.85440472148626867, -41.72647759500893727 ) ) ;
#54983 = DIRECTION ( 'NONE',  ( -0.000000000000000000, 0.000000000000000000, -1.000000000000000000 ) ) ;
#54984 = CARTESIAN_POINT ( 'NONE',  ( -71.17819443284074055, 19.60909329639479637, -68.96902843604570421 ) ) ;
#54985 = LINE ( 'NONE', #49699, #57805 ) ;
#54986 = EDGE_LOOP ( 'NONE', ( #16341, #33012, #7874, #4471 ) ) ;
#54987 = DIRECTION ( 'NONE',  ( 0.2225209339563042066, 0.9749279121818259508, 0.000000000000000000 ) ) ;
#54988 = ORIENTED_EDGE ( 'NONE', *, *, #5568, .F. ) ;
#54989 = ORIENTED_EDGE ( 'NONE', *, *, #61876, .F. ) ;
#54990 = CARTESIAN_POINT ( 'NONE',  ( -24.40147488398704567, -5.437648709335880071, 0.000000000000000000 ) ) ;
#54991 = CARTESIAN_POINT ( 'NONE',  ( 117.4727955442972984, 32.37277428084794906, 92.82555064614152229 ) ) ;
#54992 = VECTOR ( 'NONE', #31890, 1000.000000000000000 ) ;
#54993 = CARTESIAN_POINT ( 'NONE',  ( 117.7442255600443275, 33.63739995216997869, -17.07680329598102276 ) ) ;
#54994 = LINE ( 'NONE', #1910, #18053 ) ;
#54995 = CYLINDRICAL_SURFACE ( 'NONE', #30371, 7.500000000000013323 ) ;
#54996 = DIRECTION ( 'NONE',  ( 0.000000000000000000, 1.000000000000000000, -0.000000000000000000 ) ) ;
#54997 = ORIENTED_EDGE ( 'NONE', *, *, #3031, .T. ) ;
#54998 = VERTEX_POINT ( 'NONE', #40505 ) ;
#54999 = ORIENTED_EDGE ( 'NONE', *, *, #40419, .T. ) ;
#55000 = EDGE_CURVE ( 'NONE', #62166, #34582, #67821, .T. ) ;
#55001 = LINE ( 'NONE', #39534, #29357 ) ;
#55002 = CARTESIAN_POINT ( 'NONE',  ( 0.000000000000000000, 0.000000000000000000, 0.000000000000000000 ) ) ;
#55003 = CARTESIAN_POINT ( 'NONE',  ( 32.90878072717891456, 7.653588083204843073, -66.20281501231022503 ) ) ;
#55004 = CARTESIAN_POINT ( 'NONE',  ( 57.39674746172460118, 11.43903079040059012, -11.38430605732729006 ) ) ;
#55005 = UNCERTAINTY_MEASURE_WITH_UNIT (LENGTH_MEASURE( 1.000000000000000082E-05 ), #55200, 'distance_accuracy_value', 'NONE');
#55006 = CARTESIAN_POINT ( 'NONE',  ( -53.14475157111025538, 14.17819596930906201, 30.56003773838011739 ) ) ;
#55007 = AXIS2_PLACEMENT_3D ( 'NONE', #47041, #57607, #24907 ) ;
#55008 = DIRECTION ( 'NONE',  ( -0.000000000000000000, 1.000000000000000000, 1.224646799147353207E-16 ) ) ;
#55009 = ORIENTED_EDGE ( 'NONE', *, *, #24586, .T. ) ;
#55010 = CARTESIAN_POINT ( 'NONE',  ( 187.6511924654682275, 87.00187850361884045, 60.02042712270064584 ) ) ;
#55011 = CARTESIAN_POINT ( 'NONE',  ( 177.7960900018544805, 75.34533826015463376, -63.82509446584703738 ) ) ;
#55012 =( LENGTH_UNIT ( ) NAMED_UNIT ( * ) SI_UNIT ( .MILLI., .METRE. ) );
#55013 = CYLINDRICAL_SURFACE ( 'NONE', #35132, 10.00000000000000178 ) ;
#55014 = SURFACE_SIDE_STYLE ('',( #23022 ) ) ;
#55015 = CARTESIAN_POINT ( 'NONE',  ( -166.5686015187717999, 80.11916873959168583, 15.13637275916411973 ) ) ;
#55016 = CARTESIAN_POINT ( 'NONE',  ( -79.14127775978546708, 22.50259208414362533, -50.11545063171792691 ) ) ;
#55017 = CARTESIAN_POINT ( 'NONE',  ( 183.2136430849847955, 0.000000000000000000, -41.68900338898720292 ) ) ;
#55018 = EDGE_CURVE ( 'NONE', #8019, #23880, #45366, .T. ) ;
#55019 = DIRECTION ( 'NONE',  ( -0.9195277725514544587, 0.3930250316539147803, 0.000000000000000000 ) ) ;
#55020 = EDGE_CURVE ( 'NONE', #14714, #62926, #24690, .T. ) ;
#55021 = EDGE_CURVE ( 'NONE', #15204, #26008, #19053, .T. ) ;
#55022 = EDGE_CURVE ( 'NONE', #39395, #51882, #34205, .T. ) ;
#55023 = EDGE_LOOP ( 'NONE', ( #12911, #6031, #3765, #2567 ) ) ;
#55024 = CARTESIAN_POINT ( 'NONE',  ( -8.000000000000001776, 0.000000000000000000, 0.000000000000000000 ) ) ;
#55025 = CARTESIAN_POINT ( 'NONE',  ( 0.000000000000000000, 0.000000000000000000, 380.0000000000000000 ) ) ;
#55026 = DIRECTION ( 'NONE',  ( -0.000000000000000000, -1.000000000000000000, -0.000000000000000000 ) ) ;
#55027 = CARTESIAN_POINT ( 'NONE',  ( 46.13856685535756696, 9.381502944822535994, -66.63088862529708933 ) ) ;
#55028 = VECTOR ( 'NONE', #21897, 1000.000000000000000 ) ;
#55029 = DIRECTION ( 'NONE',  ( -0.000000000000000000, 1.000000000000000000, -0.000000000000000000 ) ) ;
#55030 = VERTEX_POINT ( 'NONE', #29603 ) ;
#55031 = ORIENTED_EDGE ( 'NONE', *, *, #14460, .T. ) ;
#55032 = CARTESIAN_POINT ( 'NONE',  ( 0.000000000000000000, 1.502314598737159031E-15, -8.000000000000000000 ) ) ;
#55033 = CARTESIAN_POINT ( 'NONE',  ( 179.8066339122161708, 77.32395502108371943, 83.10161394449548311 ) ) ;
#55034 = ORIENTED_EDGE ( 'NONE', *, *, #9122, .T. ) ;
#55035 = ORIENTED_EDGE ( 'NONE', *, *, #18118, .F. ) ;
#55036 = CARTESIAN_POINT ( 'NONE',  ( 175.3815143714021474, 73.02838262206999786, -38.84691806896955057 ) ) ;
#55037 = CARTESIAN_POINT ( 'NONE',  ( 162.6205203824432317, 63.07332653227189212, 15.52233856153403124 ) ) ;
#55038 = DIRECTION ( 'NONE',  ( -0.7071067811865475727, -0.7071067811865475727, -0.000000000000000000 ) ) ;
#55039 = EDGE_LOOP ( 'NONE', ( #50309, #4201, #3356, #32133 ) ) ;
#55040 = CARTESIAN_POINT ( 'NONE',  ( 117.3246714514015565, 33.42485879931864901, 61.43420873138611427 ) ) ;
#55041 = CARTESIAN_POINT ( 'NONE',  ( 138.5943620234098717, 45.55242290395135285, 58.02036038869290735 ) ) ;
#55042 = CARTESIAN_POINT ( 'NONE',  ( -72.20490592113146988, 19.96451062593609649, -38.77557629329852062 ) ) ;
#55043 = CIRCLE ( 'NONE', #37074, 4.999999999999997335 ) ;
#55044 = EDGE_CURVE ( 'NONE', #46155, #20027, #23645, .T. ) ;
#55046 = EDGE_CURVE ( 'NONE', #11058, #37117, #55641, .T. ) ;
#55045 = FACE_OUTER_BOUND ( 'NONE', #65247, .T. ) ;
#55047 = CARTESIAN_POINT ( 'NONE',  ( 88.30010642107259855, 19.99780058782973668, -36.00606560305973147 ) ) ;
#55048 = CARTESIAN_POINT ( 'NONE',  ( -54.57263979903869711, 15.59415114099631872, -23.37177340799620495 ) ) ;
#55049 = EDGE_CURVE ( 'NONE', #24494, #48193, #35234, .T. ) ;
#55050 = ADVANCED_BREP_SHAPE_REPRESENTATION ( '', ( #62812, #66832 ), #11761 ) ;
#55051 = ORIENTED_EDGE ( 'NONE', *, *, #51372, .F. ) ;
#55052 = CARTESIAN_POINT ( 'NONE',  ( -125.8938041572051389, 46.49392987655490828, -8.069153307770243089 ) ) ;
#55053 = CARTESIAN_POINT ( 'NONE',  ( -71.17984086584779391, 20.67393782512343137, 11.58859701068692871 ) ) ;
#55054 = CARTESIAN_POINT ( 'NONE',  ( 42.03492317486905705, 8.766487167902370814, -50.14667375286791895 ) ) ;
#55055 = LINE ( 'NONE', #6874, #27525 ) ;
#55057 = ORIENTED_EDGE ( 'NONE', *, *, #6049, .T. ) ;
#55056 = CARTESIAN_POINT ( 'NONE',  ( -119.4574925226536237, 42.39917684031088640, 87.90653636692998418 ) ) ;
#55058 = CARTESIAN_POINT ( 'NONE',  ( 55.64941047419414133, 12.11006143146460978, 11.94197868491970915 ) ) ;
#55059 = AXIS2_PLACEMENT_3D ( 'NONE', #69446, #21261, #5432 ) ;
#55060 = ORIENTED_EDGE ( 'NONE', *, *, #59061, .T. ) ;
#55061 = CARTESIAN_POINT ( 'NONE',  ( -149.5074843970971017, 64.17983161892348676, 57.56537183036274996 ) ) ;
#55062 = DIRECTION ( 'NONE',  ( 0.000000000000000000, 0.000000000000000000, 1.000000000000000000 ) ) ;
#55063 = LINE ( 'NONE', #24469, #51184 ) ;
#55064 = CARTESIAN_POINT ( 'NONE',  ( 181.9295719569815049, 79.46350097013164770, -24.34495040295407620 ) ) ;
#55065 = CARTESIAN_POINT ( 'NONE',  ( 140.2332932573541768, 45.41010019581507606, -12.69871729523817727 ) ) ;
#55066 = CARTESIAN_POINT ( 'NONE',  ( -21.27554331372999741, 61.43430442924864820, 170.0000000000000000 ) ) ;
#55067 = CARTESIAN_POINT ( 'NONE',  ( 92.51858280840787074, 21.51505926344916730, -74.83681589150050684 ) ) ;
#55068 = CARTESIAN_POINT ( 'NONE',  ( -29.34031752350706412, 9.255998326330892922, -89.29320561667297795 ) ) ;
#55069 = CARTESIAN_POINT ( 'NONE',  ( -54.08816720029309977, 15.46531105893042302, 45.27054875321893945 ) ) ;
#55070 = ORIENTED_EDGE ( 'NONE', *, *, #68976, .F. ) ;
#55071 = ORIENTED_EDGE ( 'NONE', *, *, #986, .F. ) ;
#55072 = DIRECTION ( 'NONE',  ( -1.000000000000000000, 0.000000000000000000, 0.000000000000000000 ) ) ;
#55073 = CARTESIAN_POINT ( 'NONE',  ( 197.2200752504831769, 96.62072041958363400, -16.31714441260212212 ) ) ;
#55074 = LINE ( 'NONE', #28351, #11002 ) ;
#55075 = CARTESIAN_POINT ( 'NONE',  ( -190.0468231512975308, 108.2116162189844459, 61.86802075691926461 ) ) ;
#55076 = VECTOR ( 'NONE', #50131, 1000.000000000000000 ) ;
#55077 = CARTESIAN_POINT ( 'NONE',  ( 211.3757499519976761, 117.8130818709823586, -40.40091158434037055 ) ) ;
#55078 = CARTESIAN_POINT ( 'NONE',  ( 0.000000000000000000, 0.000000000000000000, -0.5251556536572842271 ) ) ;
#55079 = LINE ( 'NONE', #39270, #66350 ) ;
#55080 = CARTESIAN_POINT ( 'NONE',  ( -29.02794087136069123, 9.207646203414331154, -35.69869208938506944 ) ) ;
#55081 = DIRECTION ( 'NONE',  ( 1.000000000000000000, 0.000000000000000000, 0.000000000000000000 ) ) ;
#55082 = ORIENTED_EDGE ( 'NONE', *, *, #19586, .F. ) ;
#55083 = CARTESIAN_POINT ( 'NONE',  ( -10.00000000000000178, -31.50328976398030534, -9.999999999999998224 ) ) ;
#55084 = ORIENTED_EDGE ( 'NONE', *, *, #11642, .T. ) ;
#55085 = CARTESIAN_POINT ( 'NONE',  ( 86.62931800182293784, 19.42108912189598158, 2.867536982015618019 ) ) ;
#55086 = EDGE_CURVE ( 'NONE', #32665, #2286, #20878, .T. ) ;
#55087 =( NAMED_UNIT ( * ) SI_UNIT ( $, .STERADIAN. ) SOLID_ANGLE_UNIT ( ) );
#55088 = CARTESIAN_POINT ( 'NONE',  ( -8.000000000000000000, 0.000000000000000000, -9.500000000000000000 ) ) ;
#55089 = CARTESIAN_POINT ( 'NONE',  ( 131.3924949472282719, 41.12442122814098866, 29.92295193858798186 ) ) ;
#55090 = CARTESIAN_POINT ( 'NONE',  ( 2.005731055991735623, 188.0000000000000000, 0.000000000000000000 ) ) ;
#55091 = PLANE ( 'NONE',  #19949 ) ;
#55092 = VECTOR ( 'NONE', #67470, 1000.000000000000114 ) ;
#55093 = CARTESIAN_POINT ( 'NONE',  ( -95.52093927227217307, 30.58993121475388577, -12.40980231041914195 ) ) ;
#55094 = LINE ( 'NONE', #66035, #44649 ) ;
#55095 = CARTESIAN_POINT ( 'NONE',  ( 210.9858733471680239, 115.3838960844459933, 86.29496074341011536 ) ) ;
#55096 = DIRECTION ( 'NONE',  ( -0.000000000000000000, -0.000000000000000000, -1.000000000000000000 ) ) ;
#55097 = ORIENTED_EDGE ( 'NONE', *, *, #37465, .F. ) ;
#55098 = LINE ( 'NONE', #43498, #2595 ) ;
#55099 = CARTESIAN_POINT ( 'NONE',  ( 13.24564585880136036, -63.65041531508826012, 170.0000000000000000 ) ) ;
#55100 = CARTESIAN_POINT ( 'NONE',  ( -11.79249160485393588, 8.191429102467035150, 17.14070543632877275 ) ) ;
#55101 = EDGE_CURVE ( 'NONE', #42689, #28520, #47158, .T. ) ;
#55102 = CARTESIAN_POINT ( 'NONE',  ( 280.0000000000000000, -21.42428528562853529, -4.999999999999990230 ) ) ;
#55103 = DIRECTION ( 'NONE',  ( 0.6579387259397136978, -0.7530714660036099684, 0.000000000000000000 ) ) ;
#55104 = EDGE_CURVE ( 'NONE', #55930, #19164, #5295, .T. ) ;
#55105 = CARTESIAN_POINT ( 'NONE',  ( -94.95309908913763763, 29.21194990959874360, -94.53409306187226946 ) ) ;
#55106 = ADVANCED_FACE ( 'NONE', ( #63352 ), #68622, .F. ) ;
#55107 = EDGE_CURVE ( 'NONE', #68773, #62204, #8311, .T. ) ;
#55108 = ORIENTED_EDGE ( 'NONE', *, *, #3365, .F. ) ;
#55109 = DIRECTION ( 'NONE',  ( -0.4127148655274873734, 0.9108602745606090290, 7.802725385365067200E-15 ) ) ;
#55110 = VECTOR ( 'NONE', #5939, 1000.000000000000000 ) ;
#55111 = CARTESIAN_POINT ( 'NONE',  ( 112.3013380801406385, 400.0000000000077307, 96.05029585798746439 ) ) ;
#55112 = CARTESIAN_POINT ( 'NONE',  ( -131.1078488676299116, 50.02394948559178545, 16.67182174600359801 ) ) ;
#55113 = CARTESIAN_POINT ( 'NONE',  ( -166.5742238910466426, 81.57147158222491612, -45.88140790838662042 ) ) ;
#55114 = CONTEXT_DEPENDENT_SHAPE_REPRESENTATION ( #6292, #647 ) ;
#55115 = CARTESIAN_POINT ( 'NONE',  ( -172.2786706323828696, 86.19570483525345139, 84.55397788683201554 ) ) ;
#55116 = VERTEX_POINT ( 'NONE', #6332 ) ;
#55117 = CARTESIAN_POINT ( 'NONE',  ( -122.8118341587044853, 44.49743491855736721, -49.26647034107312351 ) ) ;
#55118 = CARTESIAN_POINT ( 'NONE',  ( -20.55634918610396866, 31.11269837220809009, 0.000000000000000000 ) ) ;
#55119 = CARTESIAN_POINT ( 'NONE',  ( -149.0782809666403637, 63.81577337591402710, -22.96827994102829962 ) ) ;
#55120 = CARTESIAN_POINT ( 'NONE',  ( -1.328627985309862591, 7.561890325089885678, -73.51797458872181323 ) ) ;
#55121 = CARTESIAN_POINT ( 'NONE',  ( -125.8938041572051105, 46.49392987655492959, 3.775397282693376599 ) ) ;
#55122 = EDGE_LOOP ( 'NONE', ( #27603, #51918, #28481 ) ) ;
#55123 = CARTESIAN_POINT ( 'NONE',  ( 164.5345649067969021, 64.67444685591088671, -94.78372339538049118 ) ) ;
#55124 = CARTESIAN_POINT ( 'NONE',  ( 10.55634918610403084, 4.999999999999969802, 2.000000000000001776 ) ) ;
#55125 = CARTESIAN_POINT ( 'NONE',  ( -102.2801239173131052, 33.91021738430207932, 30.51907450641510522 ) ) ;
#55126 = CARTESIAN_POINT ( 'NONE',  ( 19.54475376904848005, 6.649964688461123430, -36.52285208494490121 ) ) ;
#55128 = VERTEX_POINT ( 'NONE', #53805 ) ;
#55127 = CARTESIAN_POINT ( 'NONE',  ( -55.53469534616550618, 14.81076603075803888, 3.472777182467473356 ) ) ;
#55129 = EDGE_CURVE ( 'NONE', #27252, #33243, #47602, .T. ) ;
#55130 = CARTESIAN_POINT ( 'NONE',  ( 185.0000000000000000, 0.000000000000000000, -2.500000000000002220 ) ) ;
#55131 = ORIENTED_EDGE ( 'NONE', *, *, #29785, .F. ) ;
#55132 = VERTEX_POINT ( 'NONE', #43609 ) ;
#55133 = CARTESIAN_POINT ( 'NONE',  ( 176.6238742729555327, 75.60943990211369226, 30.76015344212299851 ) ) ;
#55134 = DIRECTION ( 'NONE',  ( -0.000000000000000000, 1.000000000000000000, -0.000000000000000000 ) ) ;
#55136 = ORIENTED_EDGE ( 'NONE', *, *, #49210, .T. ) ;
#55135 = CARTESIAN_POINT ( 'NONE',  ( -14.56151485655250255, 8.434196591921343966, -73.09670765900315814 ) ) ;
#55137 = CARTESIAN_POINT ( 'NONE',  ( 159.2319614735955895, 59.03334608081210177, 29.60582811906876799 ) ) ;
#55138 = AXIS2_PLACEMENT_3D ( 'NONE', #12803, #7533, #50769 ) ;
#55139 = DIRECTION ( 'NONE',  ( 0.04486483035051862939, -0.9989930665413143673, 0.000000000000000000 ) ) ;
#55140 = FACE_OUTER_BOUND ( 'NONE', #36183, .T. ) ;
#55141 = ORIENTED_EDGE ( 'NONE', *, *, #8130, .F. ) ;
#55142 = CIRCLE ( 'NONE', #36084, 65.00000000000000000 ) ;
#55143 = CARTESIAN_POINT ( 'NONE',  ( -143.3273709291075875, 60.39554735433492993, -91.72452606276587517 ) ) ;
#55144 = AXIS2_PLACEMENT_3D ( 'NONE', #4029, #25501, #46937 ) ;
#55145 = CARTESIAN_POINT ( 'NONE',  ( -36.37371824399144060, 10.45334302951138206, -21.64224812475993431 ) ) ;
#55146 = DIRECTION ( 'NONE',  ( 1.000000000000000000, 0.000000000000000000, 0.000000000000000000 ) ) ;
#55147 = CARTESIAN_POINT ( 'NONE',  ( -133.2787743207940991, 52.78950725740546090, 12.61127779455901710 ) ) ;
#55148 = CARTESIAN_POINT ( 'NONE',  ( -102.2801239173131194, 33.91021738430207932, -61.85912785543958847 ) ) ;
#55149 = EDGE_LOOP ( 'NONE', ( #52583, #21388, #67791, #38564 ) ) ;
#55150 = VERTEX_POINT ( 'NONE', #714 ) ;
#55151 = ORIENTED_EDGE ( 'NONE', *, *, #54101, .F. ) ;
#55152 = AXIS2_PLACEMENT_3D ( 'NONE', #1272, #54010, #5839 ) ;
#55153 = CARTESIAN_POINT ( 'NONE',  ( 208.3164187557410116, 111.4385528447316318, -90.93565301021618552 ) ) ;
#55154 = DIRECTION ( 'NONE',  ( 0.000000000000000000, 0.000000000000000000, 1.000000000000000000 ) ) ;
#55155 = ADVANCED_FACE ( 'NONE', ( #1062 ), #49227, .F. ) ;
#55156 = FACE_OUTER_BOUND ( 'NONE', #59435, .T. ) ;
#55157 = CARTESIAN_POINT ( 'NONE',  ( -37.92511097250854846, 10.74631978746601213, -39.04328897955974753 ) ) ;
#55158 = CARTESIAN_POINT ( 'NONE',  ( -103.7931824998358792, 33.55607161175042563, 84.35638170082560805 ) ) ;
#55159 = CARTESIAN_POINT ( 'NONE',  ( -144.2188519266539970, 59.82027639618910797, 32.89713914446858922 ) ) ;
#55160 = EDGE_CURVE ( 'NONE', #43438, #2040, #60142, .T. ) ;
#55161 = CARTESIAN_POINT ( 'NONE',  ( -133.3392045760936355, 51.59583146030204404, 63.91024170815089178 ) ) ;
#55162 = CARTESIAN_POINT ( 'NONE',  ( -73.80418150970712077, 21.59712875466423299, -21.50274857840328124 ) ) ;
#55164 = ORIENTED_EDGE ( 'NONE', *, *, #63938, .T. ) ;
#55163 = EDGE_CURVE ( 'NONE', #69223, #21790, #7032, .T. ) ;
#55165 = DIRECTION ( 'NONE',  ( 0.000000000000000000, 0.000000000000000000, -1.000000000000000000 ) ) ;
#55166 = EDGE_LOOP ( 'NONE', ( #43284, #56325, #12639, #47173 ) ) ;
#55167 = LINE ( 'NONE', #28088, #18400 ) ;
#55168 = EDGE_CURVE ( 'NONE', #1149, #31022, #54858, .T. ) ;
#55169 = CARTESIAN_POINT ( 'NONE',  ( 63.01563776193091826, -170.0000000000000000, 37.31296093922129131 ) ) ;
#55170 = VERTEX_POINT ( 'NONE', #54147 ) ;
#55171 = DIRECTION ( 'NONE',  ( 0.000000000000000000, 0.000000000000000000, 1.000000000000000000 ) ) ;
#55172 = DIRECTION ( 'NONE',  ( -0.000000000000000000, -0.000000000000000000, 1.000000000000000000 ) ) ;
#55173 = CARTESIAN_POINT ( 'NONE',  ( -417.6627218934915504, 399.9999999999957367, 78.55029585799222502 ) ) ;
#55174 = CARTESIAN_POINT ( 'NONE',  ( 38.90894112122322923, 8.345444037631242651, 18.06928371549960488 ) ) ;
#55175 = EDGE_CURVE ( 'NONE', #36960, #28100, #38697, .T. ) ;
#55176 = CARTESIAN_POINT ( 'NONE',  ( -49.14234466229832776, 13.17605306081206251, 6.349177895488338663 ) ) ;
#55177 = CARTESIAN_POINT ( 'NONE',  ( 149.9838583332408177, 52.05699766415859386, -44.15268191325389324 ) ) ;
#55178 = CARTESIAN_POINT ( 'NONE',  ( 158.3516718297675823, 59.61984652322049527, -77.92999794994581464 ) ) ;
#55179 = VERTEX_POINT ( 'NONE', #17588 ) ;
#55180 = CARTESIAN_POINT ( 'NONE',  ( -109.1685085742250294, 36.41998174028086765, -93.20135381603594737 ) ) ;
#55181 = DIRECTION ( 'NONE',  ( -0.000000000000000000, -1.000000000000000000, -0.000000000000000000 ) ) ;
#55182 = ORIENTED_EDGE ( 'NONE', *, *, #15413, .F. ) ;
#55183 = DIRECTION ( 'NONE',  ( 0.9909497617679352555, -0.1342332658176522420, 0.000000000000000000 ) ) ;
#55184 = DIRECTION ( 'NONE',  ( -1.000000000000000000, 0.000000000000000000, 0.000000000000000000 ) ) ;
#55185 = CARTESIAN_POINT ( 'NONE',  ( 6.000000000000000000, 23.07878402833891229, -5.000000000000000000 ) ) ;
#55186 = EDGE_LOOP ( 'NONE', ( #183, #34170 ) ) ;
#55187 = CARTESIAN_POINT ( 'NONE',  ( -82.53770812813168334, 23.83403279300014077, 31.49003151132006550 ) ) ;
#55188 = CARTESIAN_POINT ( 'NONE',  ( -8.320652113663527416, 6.923290556636831461, -62.26262132240749025 ) ) ;
#55189 = CARTESIAN_POINT ( 'NONE',  ( 46.89016064832838993, 10.52130577388959587, 36.92564426630246288 ) ) ;
#55190 = ADVANCED_FACE ( 'NONE', ( #16541 ), #32723, .T. ) ;
#55191 = ADVANCED_FACE ( 'NONE', ( #16877 ), #59438, .F. ) ;
#55192 = ORIENTED_EDGE ( 'NONE', *, *, #49851, .F. ) ;
#55193 = VECTOR ( 'NONE', #5791, 1000.000000000000000 ) ;
#55194 = VERTEX_POINT ( 'NONE', #33774 ) ;
#55195 = CARTESIAN_POINT ( 'NONE',  ( -51.84164840787185113, 39.21024726209461875, 40.00000000000003553 ) ) ;
#55196 = ORIENTED_EDGE ( 'NONE', *, *, #70, .F. ) ;
#55197 = CARTESIAN_POINT ( 'NONE',  ( 31.96192885395476679, 8.569232728322420556, -15.29726466815624697 ) ) ;
#55198 = CARTESIAN_POINT ( 'NONE',  ( 188.9999999999999432, -2.000000000000000000, 380.0000000000000000 ) ) ;
#55199 = AXIS2_PLACEMENT_3D ( 'NONE', #58931, #16379, #26251 ) ;
#55200 =( LENGTH_UNIT ( ) NAMED_UNIT ( * ) SI_UNIT ( .MILLI., .METRE. ) );
#55201 = CARTESIAN_POINT ( 'NONE',  ( 137.2367873612328424, 44.69120782157546756, 83.99673694943189162 ) ) ;
#55202 = PRODUCT_DEFINITION_SHAPE ( 'NONE', 'NONE',  #43080 ) ;
#55203 = CARTESIAN_POINT ( 'NONE',  ( 200.5149448373513508, 102.4289237596961044, -91.27880272729396438 ) ) ;
#55204 = AXIS2_PLACEMENT_3D ( 'NONE', #20046, #36569, #31296 ) ;
#55206 = VECTOR ( 'NONE', #38131, 1000.000000000000000 ) ;
#55205 = DIRECTION ( 'NONE',  ( -0.000000000000000000, -0.000000000000000000, 1.000000000000000000 ) ) ;
#55207 = ORIENTED_EDGE ( 'NONE', *, *, #42701, .F. ) ;
#55208 = CARTESIAN_POINT ( 'NONE',  ( 8.000000000000001776, 0.000000000000000000, 0.000000000000000000 ) ) ;
#55209 = ORIENTED_EDGE ( 'NONE', *, *, #27891, .T. ) ;
#55210 = VERTEX_POINT ( 'NONE', #17223 ) ;
#55211 = CARTESIAN_POINT ( 'NONE',  ( 163.7607557204680404, 62.71181783708028235, -12.66404714983320368 ) ) ;
#55212 = DIRECTION ( 'NONE',  ( 1.110223024625156294E-16, 3.697785493223491743E-32, -1.000000000000000000 ) ) ;
#55213 = CARTESIAN_POINT ( 'NONE',  ( -61.41100614348627573, -43.07262267896732766, 170.0000000000000000 ) ) ;
#55214 = CARTESIAN_POINT ( 'NONE',  ( 141.2811136745703777, 46.09188267874204570, -71.46311027019235951 ) ) ;
#55215 = DIRECTION ( 'NONE',  ( 0.000000000000000000, 1.232595164407830672E-32, -1.000000000000000000 ) ) ;
#55216 = CONICAL_SURFACE ( 'NONE', #6917, 74.95140232871122521, 0.8777644062502172329 ) ;
#55217 = ORIENTED_EDGE ( 'NONE', *, *, #39925, .T. ) ;
#55218 = ORIENTED_EDGE ( 'NONE', *, *, #67027, .F. ) ;
#55219 = FACE_OUTER_BOUND ( 'NONE', #17205, .T. ) ;
#55220 = VERTEX_POINT ( 'NONE', #6683 ) ;
#55221 = CARTESIAN_POINT ( 'NONE',  ( -29.87147652227455552, 100.0000000000000000, 133.5802547743875550 ) ) ;
#55222 = VERTEX_POINT ( 'NONE', #37995 ) ;
#55223 = CARTESIAN_POINT ( 'NONE',  ( -149.5074843970971301, 64.17983161892345834, -76.65738112195568021 ) ) ;
#55224 = CARTESIAN_POINT ( 'NONE',  ( 93.92910382125421620, 22.04227458821882379, 12.10717395489050929 ) ) ;
#55225 = CYLINDRICAL_SURFACE ( 'NONE', #19352, 200.0000000000000000 ) ;
#55226 = VERTEX_POINT ( 'NONE', #28486 ) ;
#55227 = CARTESIAN_POINT ( 'NONE',  ( 15.55634918610400241, -15.55634918610406103, 0.000000000000000000 ) ) ;
#55228 = LINE ( 'NONE', #24288, #42489 ) ;
#55229 = CARTESIAN_POINT ( 'NONE',  ( 196.9999999999999716, 3.000000000000030198, -50.00000000000000000 ) ) ;
#55230 = CARTESIAN_POINT ( 'NONE',  ( 64.94098077424391136, 14.16208887966257457, 30.04812862234404491 ) ) ;
#55231 = CARTESIAN_POINT ( 'NONE',  ( -133.2698123908828620, 51.54642138335022139, -14.18505733217823561 ) ) ;
#55232 = DIRECTION ( 'NONE',  ( 0.000000000000000000, 0.000000000000000000, -1.000000000000000000 ) ) ;
#55233 = CARTESIAN_POINT ( 'NONE',  ( 130.7531879853686405, 39.58149302537893277, -63.52440237893536334 ) ) ;
#55234 = ORIENTED_EDGE ( 'NONE', *, *, #26747, .F. ) ;
#55235 = CARTESIAN_POINT ( 'NONE',  ( -31.11269837220809364, -15.55634918610397754, 85.00100000000000477 ) ) ;
#55236 = LINE ( 'NONE', #38022, #29900 ) ;
#55237 = ORIENTED_EDGE ( 'NONE', *, *, #23355, .T. ) ;
#55238 = VECTOR ( 'NONE', #35232, 1000.000000000000114 ) ;
#55239 = DIRECTION ( 'NONE',  ( -0.8160245890732938934, -0.5780171883497599028, 0.000000000000000000 ) ) ;
#55240 = CYLINDRICAL_SURFACE ( 'NONE', #62381, 7.500000000000013323 ) ;
#55241 = CARTESIAN_POINT ( 'NONE',  ( -37.93379515072632557, 11.77251734620211643, 33.93346572377289050 ) ) ;
#55243 = CARTESIAN_POINT ( 'NONE',  ( -144.2038301586456726, 61.09856042007388055, -20.79348971481011432 ) ) ;
#55242 = CONICAL_SURFACE ( 'NONE', #66524, 4.999999999999997335, 0.7853981633974482790 ) ;
#55244 = CARTESIAN_POINT ( 'NONE',  ( 32.24915246298996863, 20.72408643103235448, 13.32819299319724493 ) ) ;
#55245 = CARTESIAN_POINT ( 'NONE',  ( -90.99999999999998579, 0.000000000000000000, -2.818925648462311528E-14 ) ) ;
#55246 = DIRECTION ( 'NONE',  ( -0.000000000000000000, -0.000000000000000000, -1.000000000000000000 ) ) ;
#55247 = CARTESIAN_POINT ( 'NONE',  ( -47.61380558691494969, 12.81230778489788058, -68.57384386193655246 ) ) ;
#55248 = DIRECTION ( 'NONE',  ( 0.000000000000000000, 0.000000000000000000, 1.000000000000000000 ) ) ;
#55249 = ADVANCED_FACE ( 'NONE', ( #28130 ), #43252, .F. ) ;
#55251 = CARTESIAN_POINT ( 'NONE',  ( 312.3372781065084496, 394.9999999999999432, -21.44970414201177888 ) ) ;
#55250 = CIRCLE ( 'NONE', #207, 5.000000000000004441 ) ;
#55252 = PRESENTATION_LAYER_ASSIGNMENT (  '', '', ( #24951 ) ) ;
#55253 = CARTESIAN_POINT ( 'NONE',  ( 164.3702714028688945, 63.22112480708620552, 13.01656737544070452 ) ) ;
#55254 = CARTESIAN_POINT ( 'NONE',  ( 46.68054346512387554, 10.48734223171576829, -95.00000000000133582 ) ) ;
#55255 = VERTEX_POINT ( 'NONE', #55213 ) ;
#55256 = CARTESIAN_POINT ( 'NONE',  ( -99.10904156412040322, 32.31949011661295401, -35.70134815719908516 ) ) ;
#55258 = VERTEX_POINT ( 'NONE', #42908 ) ;
#55257 = ADVANCED_FACE ( 'NONE', ( #39053 ), #66778, .F. ) ;
#55259 = DIRECTION ( 'NONE',  ( 1.000000000000000000, 0.000000000000000000, 0.000000000000000000 ) ) ;
#55260 = VECTOR ( 'NONE', #47433, 1000.000000000000000 ) ;
#55261 = LINE ( 'NONE', #38389, #2880 ) ;
#55262 = CARTESIAN_POINT ( 'NONE',  ( 40.38414441725701209, 8.538832720399533116, 71.71009557933999190 ) ) ;
#55263 = DIRECTION ( 'NONE',  ( 0.000000000000000000, 0.000000000000000000, 1.000000000000000000 ) ) ;
#55264 = ADVANCED_FACE ( 'NONE', ( #64373 ), #59092, .T. ) ;
#55265 = CARTESIAN_POINT ( 'NONE',  ( -44.26023579658871654, -48.10138582123836670, 43.58025477438756212 ) ) ;
#55266 = CLOSED_SHELL ( 'NONE', ( #29312, #38016, #51089, #16684, #24074, #7818, #60592, #31908, #25105, #7491, #3037, #38518, #55772, #10334, #57949, #69266, #27970, #56239, #59449, #2068, #66892, #4071, #58734, #63502, #14532, #16961, #54447, #8131, #65341 ) ) ;
#55267 = DIRECTION ( 'NONE',  ( 1.000000000000000000, 0.000000000000000000, 0.000000000000000000 ) ) ;
#55268 = CARTESIAN_POINT ( 'NONE',  ( 0.000000000000000000, 0.000000000000000000, -25.03750572909317285 ) ) ;
#55269 = LINE ( 'NONE', #17996, #21756 ) ;
#55270 = ORIENTED_EDGE ( 'NONE', *, *, #57210, .T. ) ;
#55271 = ORIENTED_EDGE ( 'NONE', *, *, #46142, .T. ) ;
#55272 = DIRECTION ( 'NONE',  ( 0.000000000000000000, 0.000000000000000000, 1.000000000000000000 ) ) ;
#55273 = CARTESIAN_POINT ( 'NONE',  ( 173.9288990958749537, 71.66475105971926496, 65.97522071097360197 ) ) ;
#55274 = FACE_OUTER_BOUND ( 'NONE', #29830, .T. ) ;
#55275 = SURFACE_STYLE_FILL_AREA ( #10277 ) ;
#55276 = DIRECTION ( 'NONE',  ( -0.000000000000000000, 1.000000000000000000, -0.000000000000000000 ) ) ;
#55277 = EDGE_CURVE ( 'NONE', #54950, #43248, #40428, .T. ) ;
#55278 = DIRECTION ( 'NONE',  ( -0.000000000000000000, -1.000000000000000000, -0.000000000000000000 ) ) ;
#55279 = ORIENTED_EDGE ( 'NONE', *, *, #58368, .F. ) ;
#55280 = CARTESIAN_POINT ( 'NONE',  ( 105.7953515382196201, 27.97683113100023533, -37.36414706739255109 ) ) ;
#55281 = CARTESIAN_POINT ( 'NONE',  ( 23.04797191264875522, 7.849755664016355716, -44.96511804298085480 ) ) ;
#55282 = CARTESIAN_POINT ( 'NONE',  ( 15.55634918610400241, -15.55634918610406103, 2.000000000000001776 ) ) ;
#55283 = CARTESIAN_POINT ( 'NONE',  ( -55.05276343752910151, -170.0000000000000000, 37.81732777293115078 ) ) ;
#55284 = LINE ( 'NONE', #65505, #510 ) ;
#55285 = FACE_BOUND ( 'NONE', #58959, .T. ) ;
#55286 = CARTESIAN_POINT ( 'NONE',  ( 159.6614743841975042, 60.66237087206236822, 56.56722943839550055 ) ) ;
#55287 = ORIENTED_EDGE ( 'NONE', *, *, #15651, .T. ) ;
#55288 = CARTESIAN_POINT ( 'NONE',  ( 11.30618213853385967, 74.15344055032308290, 73.58025477438755502 ) ) ;
#55289 = CARTESIAN_POINT ( 'NONE',  ( -29.68020330876228030, 70.00000000000000000, 4.368699068434031219 ) ) ;
#55290 = AXIS2_PLACEMENT_3D ( 'NONE', #45710, #44308, #55561 ) ;
#55291 = LINE ( 'NONE', #5711, #29650 ) ;
#55292 = FACE_OUTER_BOUND ( 'NONE', #9905, .T. ) ;
#55293 = CARTESIAN_POINT ( 'NONE',  ( -49.77357484059193382, 41.82599373102802787, 43.58025477438756923 ) ) ;
#55294 = CARTESIAN_POINT ( 'NONE',  ( -5.354491962338131295, 6.146186931204402626, -0.06809871960542626668 ) ) ;
#55295 = AXIS2_PLACEMENT_3D ( 'NONE', #46323, #57239, #15012 ) ;
#55296 = VERTEX_POINT ( 'NONE', #28846 ) ;
#55297 = B_SPLINE_CURVE_WITH_KNOTS ( 'NONE', 3,
 ( #36169, #41103, #15403, #47393, #14019, #25629, #47063, #51659, #57966, #19640, #9096, #68850, #63249, #36513, #15059, #24928, #46361, #62562, #4839, #31247, #14374, #52677, #30545, #25280, #4502, #42131, #63594, #36862, #58303, #46718, #57629, #16772, #11846, #54396, #32615, #63933, #11150, #31929, #59337, #6218, #16082, #27674, #43499 ),
 .UNSPECIFIED., .F., .F.,
 ( 4, 2, 2, 2, 2, 2, 2, 2, 2, 2, 2, 2, 1, 2, 2, 2, 2, 2, 2, 2, 2, 4 ),
 ( 0.02362927190606132349, 0.02510248541563189772, 0.02583909217041719178, 0.02657569892520248236, 0.02804891243477306700, 0.02952212594434364817, 0.03025873269912893876, 0.03099533945391423281, 0.03246855296348481745, 0.03394176647305539862, 0.03541497998262597979, 0.03615158673741127038, 0.03688819349219656096, 0.03762480024698185155, 0.03836140700176714213, 0.03983462051133771636, 0.04130783402090829060, 0.04278104753047886483, 0.04351765428526414847, 0.04425426104004943906, 0.04572747454962002023, 0.04720068805919060140 ),
 .UNSPECIFIED. ) ;
#55298 = DIRECTION ( 'NONE',  ( 0.000000000000000000, 0.000000000000000000, -1.000000000000000000 ) ) ;
#55299 = DIRECTION ( 'NONE',  ( 0.000000000000000000, -1.000000000000000000, 0.000000000000000000 ) ) ;
#55300 = ORIENTED_EDGE ( 'NONE', *, *, #26790, .T. ) ;
#55301 = AXIS2_PLACEMENT_3D ( 'NONE', #63631, #4874, #57663 ) ;
#55302 = PLANE ( 'NONE',  #34018 ) ;
#55303 = ORIENTED_EDGE ( 'NONE', *, *, #45213, .T. ) ;
#55304 = CARTESIAN_POINT ( 'NONE',  ( -61.29635759142584561, -21.66977272663583776, 170.0000000000000000 ) ) ;
#55305 = CARTESIAN_POINT ( 'NONE',  ( -59.57462349605615515, 16.98779896904799358, -21.87540493568376831 ) ) ;
#55306 = CARTESIAN_POINT ( 'NONE',  ( 93.72687053612526142, 23.04134601640627622, -72.64113259414895651 ) ) ;
#55307 = ORIENTED_EDGE ( 'NONE', *, *, #26790, .F. ) ;
#55308 = AXIS2_PLACEMENT_3D ( 'NONE', #11878, #49494, #60420 ) ;
#55309 = EDGE_LOOP ( 'NONE', ( #34848, #16786, #69359, #42171 ) ) ;
#55310 = CARTESIAN_POINT ( 'NONE',  ( 41.33434189587761409, 9.684413566891869607, 71.50931503011094037 ) ) ;
#55311 = CARTESIAN_POINT ( 'NONE',  ( 99.99999999999997158, 6.000000000000000000, -46.99999999999997158 ) ) ;
#55312 = CARTESIAN_POINT ( 'NONE',  ( 104.7227067006896561, 27.50728936118537149, 5.166247656402080501 ) ) ;
#55313 = CARTESIAN_POINT ( 'NONE',  ( 63.01563776193091826, 13.70579113808096849, 17.96841034875761878 ) ) ;
#55314 = LINE ( 'NONE', #5729, #63493 ) ;
#55315 = ORIENTED_EDGE ( 'NONE', *, *, #43559, .F. ) ;
#55316 = EDGE_CURVE ( 'NONE', #22488, #55692, #47779, .T. ) ;
#55317 = CARTESIAN_POINT ( 'NONE',  ( -48.34500911884041585, 14.01939034823941554, 14.33699677132702099 ) ) ;
#55318 = CARTESIAN_POINT ( 'NONE',  ( -132.8257891167039304, 52.46553896898735303, -12.69414959889051886 ) ) ;
#55319 = CARTESIAN_POINT ( 'NONE',  ( -151.5161158480891856, 67.23556208791072208, -88.76439689521589571 ) ) ;
#55320 = CARTESIAN_POINT ( 'NONE',  ( 115.7561705820729117, 31.51689401996056361, -21.68569513149070715 ) ) ;
#55321 = CARTESIAN_POINT ( 'NONE',  ( -55.05276343752910151, -170.0000000000000000, -50.21632399845989170 ) ) ;
#55323 = VERTEX_POINT ( 'NONE', #67518 ) ;
#55322 = CARTESIAN_POINT ( 'NONE',  ( -3.806566064960824935E-15, 7.321656987762869662, -3.318518101603011417 ) ) ;
#55324 = VERTEX_POINT ( 'NONE', #55562 ) ;
#55325 = ORIENTED_EDGE ( 'NONE', *, *, #21210, .T. ) ;
#55326 = CARTESIAN_POINT ( 'NONE',  ( -9.763294602873862971, 7.024900256480052896, -8.824033836334688630 ) ) ;
#55327 = DIRECTION ( 'NONE',  ( -1.000000000000000000, 0.000000000000000000, 0.000000000000000000 ) ) ;
#55328 = CARTESIAN_POINT ( 'NONE',  ( -47.80896875121165834, 12.85816703949531004, -13.91236320614654964 ) ) ;
#55329 = CARTESIAN_POINT ( 'NONE',  ( 103.5839822277949906, 25.92130892112108853, -13.11793987809817885 ) ) ;
#55330 = EDGE_CURVE ( 'NONE', #12323, #8257, #28549, .T. ) ;
#55331 = CARTESIAN_POINT ( 'NONE',  ( -35.17718245314462422, 11.25729435722175609, 71.06764365538327866 ) ) ;
#55332 = EDGE_CURVE ( 'NONE', #50410, #57368, #1765, .T. ) ;
#55333 = CARTESIAN_POINT ( 'NONE',  ( 157.4703587214989398, -170.0000000000000000, 56.25401806271706562 ) ) ;
#55334 = DIRECTION ( 'NONE',  ( -0.000000000000000000, -0.000000000000000000, 1.000000000000000000 ) ) ;
#55335 = CARTESIAN_POINT ( 'NONE',  ( -8.807541152391516803, 6.956521193351524524, 45.06700915991218181 ) ) ;
#55336 = EDGE_LOOP ( 'NONE', ( #25759, #3323, #6862, #13804 ) ) ;
#55337 = FACE_BOUND ( 'NONE', #4785, .T. ) ;
#55338 = ORIENTED_EDGE ( 'NONE', *, *, #48479, .T. ) ;
#55339 = ORIENTED_EDGE ( 'NONE', *, *, #62746, .F. ) ;
#55340 = DIRECTION ( 'NONE',  ( -1.000000000000000000, 0.000000000000000000, 0.000000000000000000 ) ) ;
#55341 = CIRCLE ( 'NONE', #50836, 242.4895526022646379 ) ;
#55342 = CARTESIAN_POINT ( 'NONE',  ( -172.3038663181179970, 87.72015621195187407, 45.82169460664105998 ) ) ;
#55343 = ADVANCED_FACE ( 'NONE', ( #17938 ), #39391, .T. ) ;
#55344 = CARTESIAN_POINT ( 'NONE',  ( 311.9975424824652350, -23.68493792952219934, 521.0102483033961107 ) ) ;
#55345 = COLOUR_RGB ( '',0.7921568627450980005, 0.8196078431372548767, 0.9333333333333333481 ) ;
#55346 = CARTESIAN_POINT ( 'NONE',  ( -103.2129897037410728, 33.25684593987699600, 18.63071618642112881 ) ) ;
#55347 = CARTESIAN_POINT ( 'NONE',  ( 183.2136430849847955, 0.000000000000000000, -41.68900338898720292 ) ) ;
#55348 = CARTESIAN_POINT ( 'NONE',  ( -25.10237775011640338, 1.004202417053489116, 3.061616997868437868E-16 ) ) ;
#55349 = ORIENTED_EDGE ( 'NONE', *, *, #57243, .T. ) ;
#55350 = ORIENTED_EDGE ( 'NONE', *, *, #2155, .T. ) ;
#55351 = VERTEX_POINT ( 'NONE', #45004 ) ;
#55352 = VECTOR ( 'NONE', #24154, 1000.000000000000227 ) ;
#55353 = CARTESIAN_POINT ( 'NONE',  ( -7.486743542470047252, 64.58150799671128084, 43.58025477438756923 ) ) ;
#55354 = DIRECTION ( 'NONE',  ( 0.000000000000000000, 0.7071067811865474617, -0.7071067811865474617 ) ) ;
#55355 = DIRECTION ( 'NONE',  ( 1.000000000000000000, 1.850550996349095901E-16, 1.228197773518735191E-20 ) ) ;
#55356 = VECTOR ( 'NONE', #34761, 1000.000000000000000 ) ;
#55357 = CARTESIAN_POINT ( 'NONE',  ( 55.61382797299288683, 11.07686102552914953, -17.61099702755072371 ) ) ;
#55358 = EDGE_CURVE ( 'NONE', #38637, #17049, #66491, .T. ) ;
#55359 = AXIS2_PLACEMENT_3D ( 'NONE', #23438, #60357, #12178 ) ;
#55360 = CARTESIAN_POINT ( 'NONE',  ( -49.62489392740899774, 13.29305723289026275, 32.63583538682032525 ) ) ;
#55361 = ADVANCED_FACE ( 'NONE', ( #21989 ), #32547, .T. ) ;
#55362 = LINE ( 'NONE', #28281, #48597 ) ;
#55363 = ADVANCED_FACE ( 'NONE', ( #3839 ), #62589, .F. ) ;
#55364 = VERTEX_POINT ( 'NONE', #63273 ) ;
#55365 = FACE_OUTER_BOUND ( 'NONE', #50384, .T. ) ;
#55366 = CARTESIAN_POINT ( 'NONE',  ( 197.6329787101073805, 98.74106466892197886, -73.20637281266709806 ) ) ;
#55367 = CARTESIAN_POINT ( 'NONE',  ( -3.862560291631544906, 7.672660553664872651, -49.29031988421443344 ) ) ;
#55368 = CARTESIAN_POINT ( 'NONE',  ( 103.0026233023292974, 25.67408295205787994, 8.243349890369009003 ) ) ;
#55369 = CARTESIAN_POINT ( 'NONE',  ( -165.6754884515988522, 79.20562145685592270, -95.00000000000133582 ) ) ;
#55370 = DIRECTION ( 'NONE',  ( -0.000000000000000000, -0.000000000000000000, -1.000000000000000000 ) ) ;
#55371 = FACE_BOUND ( 'NONE', #58758, .T. ) ;
#55372 = DIRECTION ( 'NONE',  ( -1.000000000000000000, 0.000000000000000000, 0.000000000000000000 ) ) ;
#55373 = ORIENTED_EDGE ( 'NONE', *, *, #58825, .T. ) ;
#55374 = LINE ( 'NONE', #7198, #27114 ) ;
#55375 = CARTESIAN_POINT ( 'NONE',  ( -133.3926783185151521, 51.63401075114363437, -68.95695763348717833 ) ) ;
#55376 = CARTESIAN_POINT ( 'NONE',  ( 8.000000000000007105, 249.8719672152120381, 94.99999999999866418 ) ) ;
#55377 = FACE_OUTER_BOUND ( 'NONE', #51661, .T. ) ;
#55378 = DIRECTION ( 'NONE',  ( -1.000000000000000000, 0.000000000000000000, 0.000000000000000000 ) ) ;
#55379 = EDGE_LOOP ( 'NONE', ( #45145, #26287, #20440, #21478 ) ) ;
#55380 = CARTESIAN_POINT ( 'NONE',  ( 8.000000000000007105, 249.8719672152120381, 94.99999999999866418 ) ) ;
#55381 = CARTESIAN_POINT ( 'NONE',  ( 175.3026482967971162, 72.95361582193056904, 85.70764415495648336 ) ) ;
#55382 = ORIENTED_EDGE ( 'NONE', *, *, #9367, .T. ) ;
#55383 = ORIENTED_EDGE ( 'NONE', *, *, #29638, .T. ) ;
#55384 = CARTESIAN_POINT ( 'NONE',  ( 175.5406524085945819, 73.17873692326776336, -48.80246454543877377 ) ) ;
#55385 = CARTESIAN_POINT ( 'NONE',  ( 150.9013375937531407, 53.96275732797612079, 40.53801543753266401 ) ) ;
#55386 = DIRECTION ( 'NONE',  ( 0.000000000000000000, 0.000000000000000000, 1.000000000000000000 ) ) ;
#55387 = ORIENTED_EDGE ( 'NONE', *, *, #44878, .T. ) ;
#55388 = DIRECTION ( 'NONE',  ( -0.000000000000000000, -0.000000000000000000, -1.000000000000000000 ) ) ;
#55389 = CARTESIAN_POINT ( 'NONE',  ( -178.5790738944854184, 93.41591512785082330, 16.62680291879139105 ) ) ;
#55390 = CARTESIAN_POINT ( 'NONE',  ( -76.31381168750411348, 21.43908608416557371, -35.47797508748302420 ) ) ;
#55391 = CIRCLE ( 'NONE', #59847, 160.5210298272983778 ) ;
#55392 = LINE ( 'NONE', #7221, #45949 ) ;
#55393 = CARTESIAN_POINT ( 'NONE',  ( 19.05389411040262004, 6.625946609665808396, -89.90362069605247086 ) ) ;
#55394 = CIRCLE ( 'NONE', #35166, 24.99999999999985434 ) ;
#55395 = CARTESIAN_POINT ( 'NONE',  ( -51.77779688167514394, 14.86590802019197355, -22.62338495236307878 ) ) ;
#55396 = EDGE_CURVE ( 'NONE', #55490, #23613, #36195, .T. ) ;
#55397 = CIRCLE ( 'NONE', #43030, 245.3095347406803342 ) ;
#55398 = VERTEX_POINT ( 'NONE', #62929 ) ;
#55399 = AXIS2_PLACEMENT_3D ( 'NONE', #44379, #17301, #27157 ) ;
#55401 = EDGE_CURVE ( 'NONE', #51654, #47113, #44423, .T. ) ;
#55400 = LINE ( 'NONE', #13205, #49144 ) ;
#55402 = VECTOR ( 'NONE', #26743, 1000.000000000000000 ) ;
#55403 = DIRECTION ( 'NONE',  ( 1.000000000000000000, 0.000000000000000000, -1.261617073437677999E-16 ) ) ;
#55404 = DIRECTION ( 'NONE',  ( -0.01289363347198224825, 0.000000000000000000, -0.9999168736529503443 ) ) ;
#55405 = DIRECTION ( 'NONE',  ( -0.000000000000000000, 1.000000000000000000, -0.000000000000000000 ) ) ;
#55407 = ORIENTED_EDGE ( 'NONE', *, *, #68976, .T. ) ;
#55406 = CARTESIAN_POINT ( 'NONE',  ( 56.67004931728209982, 12.31690113431407951, 94.99999999999866418 ) ) ;
#55408 = CARTESIAN_POINT ( 'NONE',  ( 81.04675113612954362, 17.59091904316106891, -38.28904491945431943 ) ) ;
#55409 = AXIS2_PLACEMENT_3D ( 'NONE', #585, #22036, #7618 ) ;
#55410 = ORIENTED_EDGE ( 'NONE', *, *, #17127, .T. ) ;
#55411 = CYLINDRICAL_SURFACE ( 'NONE', #39141, 7.500000000000020428 ) ;
#55412 = CARTESIAN_POINT ( 'NONE',  ( 209.3223706822284100, 172.0000000000000284, 31.44247402469554942 ) ) ;
#55413 = CARTESIAN_POINT ( 'NONE',  ( 0.000000000000000000, 0.000000000000000000, 5.000000000000000000 ) ) ;
#55414 = ADVANCED_FACE ( 'NONE', ( #65254 ), #7575, .F. ) ;
#55415 = CARTESIAN_POINT ( 'NONE',  ( 93.08073375333744082, 22.79826000593201840, 33.37906321384794950 ) ) ;
#55416 = EDGE_CURVE ( 'NONE', #37187, #48528, #17770, .T. ) ;
#55417 = CARTESIAN_POINT ( 'NONE',  ( -122.8118341587044853, 44.49743491855734590, 58.11173202078160216 ) ) ;
#55418 = CARTESIAN_POINT ( 'NONE',  ( 0.000000000000000000, 0.000000000000000000, 43.58025477438756212 ) ) ;
#55419 = DIRECTION ( 'NONE',  ( -1.000000000000000000, 0.000000000000000000, 0.000000000000000000 ) ) ;
#55420 = CARTESIAN_POINT ( 'NONE',  ( -156.7398303041269116, 70.56491326691592292, -93.95181625296153527 ) ) ;
#55421 = ORIENTED_EDGE ( 'NONE', *, *, #62514, .T. ) ;
#55422 = ORIENTED_EDGE ( 'NONE', *, *, #55423, .T. ) ;
#55423 = EDGE_CURVE ( 'NONE', #54490, #33627, #29029, .T. ) ;
#55424 = CARTESIAN_POINT ( 'NONE',  ( 46.90141780929663895, 9.503798448769780194, 36.90919837786481850 ) ) ;
#55425 = CARTESIAN_POINT ( 'NONE',  ( 0.000000000000000000, 0.000000000000000000, 380.0000000000000000 ) ) ;
#55426 = CARTESIAN_POINT ( 'NONE',  ( 157.9130201331580565, 57.99550255803045928, 56.25401806271705851 ) ) ;
#55427 = DIRECTION ( 'NONE',  ( -0.000000000000000000, 1.000000000000000000, 0.000000000000000000 ) ) ;
#55428 = LINE ( 'NONE', #1989, #4124 ) ;
#55429 = CARTESIAN_POINT ( 'NONE',  ( 10.78925482157233340, 22.68765681156020264, 3.061616997868437868E-16 ) ) ;
#55430 = CARTESIAN_POINT ( 'NONE',  ( 0.4964154566687932202, 8.859816792613651515, -0.6543471694412406059 ) ) ;
#55431 = CARTESIAN_POINT ( 'NONE',  ( -27.48703802937313512, 8.975952825337596863, -36.43818875052794226 ) ) ;
#55432 = CARTESIAN_POINT ( 'NONE',  ( 164.4615316623335275, 63.29763980349834185, -73.19771330824563904 ) ) ;
#55433 = ORIENTED_EDGE ( 'NONE', *, *, #63842, .T. ) ;
#55434 = ORIENTED_EDGE ( 'NONE', *, *, #10386, .F. ) ;
#55435 = DIRECTION ( 'NONE',  ( 0.000000000000000000, 0.000000000000000000, 1.000000000000000000 ) ) ;
#55436 = CARTESIAN_POINT ( 'NONE',  ( -79.30552041445847067, 22.56523793503362896, 84.10971841195282650 ) ) ;
#55437 = CARTESIAN_POINT ( 'NONE',  ( -86.15275984831843914, 25.31588180512571995, 65.28274353219886450 ) ) ;
#55438 = LINE ( 'NONE', #7271, #29798 ) ;
#55439 = CARTESIAN_POINT ( 'NONE',  ( 445.3372781065085633, 177.8591479523844612, -111.4497041420119388 ) ) ;
#55440 = DIRECTION ( 'NONE',  ( 0.000000000000000000, 0.000000000000000000, 1.000000000000000000 ) ) ;
#55441 = CARTESIAN_POINT ( 'NONE',  ( -94.77890319529971919, 30.24118571794803145, -16.17010367493866596 ) ) ;
#55442 = ADVANCED_FACE ( 'NONE', ( #50122 ), #44842, .F. ) ;
#55443 = EDGE_CURVE ( 'NONE', #57346, #32720, #49751, .T. ) ;
#55444 = VECTOR ( 'NONE', #2251, 1000.000000000000114 ) ;
#55445 = B_SPLINE_CURVE_WITH_KNOTS ( 'NONE', 3,
 ( #58392, #53793, #5616, #21794, #339, #4935, #11582, #26402 ),
 .UNSPECIFIED., .F., .F.,
 ( 4, 2, 2, 4 ),
 ( 0.02285338878549945940, 0.02519297481083175236, 0.02636276782349789710, 0.02753256083616404531 ),
 .UNSPECIFIED. ) ;
#55446 = CARTESIAN_POINT ( 'NONE',  ( 62.04382205963241148, 13.48099884269679549, 44.76576134482495206 ) ) ;
#55447 = CARTESIAN_POINT ( 'NONE',  ( 36.82834578791594993, 8.088597268192994960, 84.05056018580073385 ) ) ;
#55448 = DIRECTION ( 'NONE',  ( 0.000000000000000000, 1.000000000000000000, 0.000000000000000000 ) ) ;
#55449 = ORIENTED_EDGE ( 'NONE', *, *, #55160, .T. ) ;
#55450 = DIRECTION ( 'NONE',  ( -0.000000000000000000, -0.000000000000000000, -1.000000000000000000 ) ) ;
#55451 = DIRECTION ( 'NONE',  ( 1.000000000000000000, 0.000000000000000000, 0.000000000000000000 ) ) ;
#55453 = ADVANCED_FACE ( 'NONE', ( #60672 ), #2291, .T. ) ;
#55452 = LINE ( 'NONE', #7635, #18499 ) ;
#55454 = CONICAL_SURFACE ( 'NONE', #49869, 8.000000000000000000, 1.047197551196600296 ) ;
#55455 = FACE_OUTER_BOUND ( 'NONE', #27794, .T. ) ;
#55456 = CARTESIAN_POINT ( 'NONE',  ( -105.8879439778144729, 34.65133284149107595, -75.95163754952972113 ) ) ;
#55457 = AXIS2_PLACEMENT_3D ( 'NONE', #55025, #49393, #527 ) ;
#55458 = CARTESIAN_POINT ( 'NONE',  ( -96.30817042286538765, 29.84904329666579059, -91.64453525374615595 ) ) ;
#55459 = CIRCLE ( 'NONE', #25151, 2.999999999999999112 ) ;
#55460 = ORIENTED_EDGE ( 'NONE', *, *, #4456, .T. ) ;
#55462 = VECTOR ( 'NONE', #11306, 1000.000000000000000 ) ;
#55461 = DIRECTION ( 'NONE',  ( 9.256411411948308756E-15, -4.223941262780577246E-15, 1.000000000000000000 ) ) ;
#55463 = LINE ( 'NONE', #66046, #31805 ) ;
#55464 = CARTESIAN_POINT ( 'NONE',  ( -38.69449158134469968, 11.92067517118074527, -44.77975842212855184 ) ) ;
#55465 = CARTESIAN_POINT ( 'NONE',  ( 5.799999999999999822, 4.618802153517001408, -8.000000000000000000 ) ) ;
#55466 = CONTEXT_DEPENDENT_SHAPE_REPRESENTATION ( #12573, #19894 ) ;
#55467 = CARTESIAN_POINT ( 'NONE',  ( -166.1022426123342655, 79.64087030515175059, 94.67701969901513337 ) ) ;
#55468 = ORIENTED_EDGE ( 'NONE', *, *, #27009, .T. ) ;
#55469 = CARTESIAN_POINT ( 'NONE',  ( -118.8504142000305421, 42.02789424825281372, -39.82313612425161864 ) ) ;
#55470 = LINE ( 'NONE', #17486, #37470 ) ;
#55471 = CARTESIAN_POINT ( 'NONE',  ( -144.7571537022064376, 60.25265659240449168, -21.27708794859261943 ) ) ;
#55472 = CARTESIAN_POINT ( 'NONE',  ( -5.888165822225384538, 7.780336669456523246, -62.51295767058608277 ) ) ;
#55473 = SHAPE_REPRESENTATION ( 'y3+', ( #66832 ), #2840 ) ;
#55474 = DIRECTION ( 'NONE',  ( 0.000000000000000000, 0.000000000000000000, 1.000000000000000000 ) ) ;
#55475 = ORIENTED_EDGE ( 'NONE', *, *, #15387, .F. ) ;
#55476 = CARTESIAN_POINT ( 'NONE',  ( 157.4703587214989113, 58.92748579479259519, -89.81328548006499091 ) ) ;
#55477 = CARTESIAN_POINT ( 'NONE',  ( 86.14890207173844772, 20.31981596387579714, 17.86753698201564688 ) ) ;
#55478 = CARTESIAN_POINT ( 'NONE',  ( -442.6627218934913230, 399.9999999999997726, 108.5502958579881891 ) ) ;
#55479 = CARTESIAN_POINT ( 'NONE',  ( 20.36314374176838271, 6.689939636827348934, -48.98252730634334995 ) ) ;
#55481 = ORIENTED_EDGE ( 'NONE', *, *, #3440, .F. ) ;
#55480 = CARTESIAN_POINT ( 'NONE',  ( 0.000000000000000000, 0.000000000000000000, -0.5776712190230133270 ) ) ;
#55482 = CARTESIAN_POINT ( 'NONE',  ( 55.76298701799387914, 11.10663440745151576, 39.28782614698545927 ) ) ;
#55483 = ORIENTED_EDGE ( 'NONE', *, *, #38118, .T. ) ;
#55484 = ORIENTED_EDGE ( 'NONE', *, *, #24503, .F. ) ;
#55486 = EDGE_CURVE ( 'NONE', #33294, #37589, #17047, .T. ) ;
#55485 = CARTESIAN_POINT ( 'NONE',  ( -123.8527606835264550, 45.16425545704599642, -88.87375819088765638 ) ) ;
#55487 = CARTESIAN_POINT ( 'NONE',  ( -36.49774120431530378, 11.49988540678358895, -90.95249728063662076 ) ) ;
#55488 = COLOUR_RGB ( '',0.7921568627450980005, 0.8196078431372548767, 0.9333333333333333481 ) ;
#55490 = VERTEX_POINT ( 'NONE', #12848 ) ;
#55489 = CARTESIAN_POINT ( 'NONE',  ( -14.33060720034882962, 8.412649192293178757, -73.52734388806258892 ) ) ;
#55491 = LINE ( 'NONE', #13626, #62270 ) ;
#55492 = DIRECTION ( 'NONE',  ( 0.000000000000000000, 1.000000000000000000, -0.000000000000000000 ) ) ;
#55493 = FACE_BOUND ( 'NONE', #20376, .T. ) ;
#55494 = VECTOR ( 'NONE', #7270, 1000.000000000000000 ) ;
#55495 = ORIENTED_EDGE ( 'NONE', *, *, #1847, .F. ) ;
#55496 = CARTESIAN_POINT ( 'NONE',  ( 176.4131312624861891, 75.40601160939048953, -91.53289336470793103 ) ) ;
#55497 = EDGE_CURVE ( 'NONE', #58864, #36637, #49390, .T. ) ;
#55498 = AXIS2_PLACEMENT_3D ( 'NONE', #65430, #27085, #37642 ) ;
#55499 = LINE ( 'NONE', #22799, #63431 ) ;
#55500 = DIRECTION ( 'NONE',  ( -1.000000000000000000, 0.000000000000000000, 0.000000000000000000 ) ) ;
#55501 = AXIS2_PLACEMENT_3D ( 'NONE', #14404, #62226, #23912 ) ;
#55502 = CARTESIAN_POINT ( 'NONE',  ( -447.6627218934913799, 369.9999999999998295, -141.4497041420117966 ) ) ;
#55503 = ADVANCED_FACE ( 'NONE', ( #24444 ), #51516, .T. ) ;
#55504 = CARTESIAN_POINT ( 'NONE',  ( 21.75198946226450758, 7.772524967554916842, 59.78508500779173573 ) ) ;
#55505 = ORIENTED_EDGE ( 'NONE', *, *, #3110, .F. ) ;
#55506 = EDGE_CURVE ( 'NONE', #53998, #27278, #13193, .T. ) ;
#55507 = VERTEX_POINT ( 'NONE', #67014 ) ;
#55508 = ORIENTED_EDGE ( 'NONE', *, *, #42505, .F. ) ;
#55509 = CARTESIAN_POINT ( 'NONE',  ( 6.400000000000000355, 4.618802153517001408, -8.000000000000000000 ) ) ;
#55510 = CARTESIAN_POINT ( 'NONE',  ( 65.13282190615461786, 1.839221433318906476E-12, -9.999999999999998224 ) ) ;
#55511 = FILL_AREA_STYLE ('',( #44959 ) ) ;
#55512 = CARTESIAN_POINT ( 'NONE',  ( -33.84080342750782222, 9.997552308299095358, -49.93905837052822250 ) ) ;
#55513 = CARTESIAN_POINT ( 'NONE',  ( -97.57502601200189929, 30.45419729933975361, 85.85939687630843764 ) ) ;
#55514 = CARTESIAN_POINT ( 'NONE',  ( -145.5261806899006558, 60.87473129144525075, 31.86056720367915673 ) ) ;
#55515 = CARTESIAN_POINT ( 'NONE',  ( -132.2352756077771119, 50.81350938245626736, 60.95178715509886302 ) ) ;
#55516 = CARTESIAN_POINT ( 'NONE',  ( -76.10382222627278281, 22.43453174720079346, -8.718168199828413734 ) ) ;
#55517 = ORIENTED_EDGE ( 'NONE', *, *, #24805, .F. ) ;
#55518 = CARTESIAN_POINT ( 'NONE',  ( 79.14129363775928994, 17.00055658855362850, 63.56359600498407048 ) ) ;
#55519 = ORIENTED_EDGE ( 'NONE', *, *, #68652, .T. ) ;
#55520 = CARTESIAN_POINT ( 'NONE',  ( 32.14349651933087415, 7.576119504381656711, 35.46268199549083988 ) ) ;
#55521 = CYLINDRICAL_SURFACE ( 'NONE', #20589, 65.00000000000000000 ) ;
#55522 = FACE_OUTER_BOUND ( 'NONE', #66699, .T. ) ;
#55523 = FACE_OUTER_BOUND ( 'NONE', #20116, .T. ) ;
#55524 = DIRECTION ( 'NONE',  ( 1.000000000000000000, 1.387778780781445922E-16, 0.000000000000000000 ) ) ;
#55525 = CARTESIAN_POINT ( 'NONE',  ( -119.5404913382139824, 43.63271406506959949, 60.97046577758045771 ) ) ;
#55526 = CARTESIAN_POINT ( 'NONE',  ( -52.45215874217871033, 13.99961488531757858, 3.933950466555594883 ) ) ;
#55527 = CARTESIAN_POINT ( 'NONE',  ( 153.4268936273268196, 54.57409659828383042, -49.94518735799756826 ) ) ;
#55528 = CARTESIAN_POINT ( 'NONE',  ( 450.2085304802404266, 188.0000000000000000, -247.8920266495912870 ) ) ;
#55529 = ORIENTED_EDGE ( 'NONE', *, *, #10309, .F. ) ;
#55530 = CARTESIAN_POINT ( 'NONE',  ( -103.9519010518735911, 33.63790860794365045, -88.88018785531716048 ) ) ;
#55531 = CARTESIAN_POINT ( 'NONE',  ( -153.7005182577090068, 67.81869626254727734, -9.233257554413990320 ) ) ;
#55532 = VERTEX_POINT ( 'NONE', #8947 ) ;
#55533 = DIRECTION ( 'NONE',  ( 0.000000000000000000, 0.000000000000000000, 1.000000000000000000 ) ) ;
#55534 = CARTESIAN_POINT ( 'NONE',  ( -35.00000000000002842, -35.00000000000000000, 0.000000000000000000 ) ) ;
#55536 = ADVANCED_FACE ( 'NONE', ( #46921 ), #36433, .T. ) ;
#55535 = PLANE ( 'NONE',  #44292 ) ;
#55537 = EDGE_LOOP ( 'NONE', ( #37075, #3343, #20638, #7278 ) ) ;
#55538 = CARTESIAN_POINT ( 'NONE',  ( -86.15275984831842493, 25.31588180512566666, 38.43819294173514578 ) ) ;
#55539 = CARTESIAN_POINT ( 'NONE',  ( 149.9714610887121466, 53.28792066194169763, -70.77614368036395831 ) ) ;
#55540 = CARTESIAN_POINT ( 'NONE',  ( 41.80869235728135891, 9.750404582811610155, 30.29359847640873227 ) ) ;
#55541 = CARTESIAN_POINT ( 'NONE',  ( 140.5781926063689298, 45.63383190293699698, -46.86065139210757025 ) ) ;
#55542 = VECTOR ( 'NONE', #18562, 1000.000000000000000 ) ;
#55543 = ORIENTED_EDGE ( 'NONE', *, *, #63973, .T. ) ;
#55544 =( NAMED_UNIT ( * ) PLANE_ANGLE_UNIT ( ) SI_UNIT ( $, .RADIAN. ) );
#55545 = CARTESIAN_POINT ( 'NONE',  ( 15.55634918610403261, 4.999999999999969802, 85.00100000000000477 ) ) ;
#55546 = VERTEX_POINT ( 'NONE', #62758 ) ;
#55547 = CARTESIAN_POINT ( 'NONE',  ( 38.42095780754792145, 9.297684251045556181, -8.823390837636260642 ) ) ;
#55548 = DIRECTION ( 'NONE',  ( 0.000000000000000000, 0.000000000000000000, 1.000000000000000000 ) ) ;
#55549 = VECTOR ( 'NONE', #43590, 1000.000000000000114 ) ;
#55550 = CARTESIAN_POINT ( 'NONE',  ( -1.327237339234996538, 7.561837009978232160, 14.52392135664211636 ) ) ;
#55551 = LINE ( 'NONE', #65781, #43091 ) ;
#55552 = CIRCLE ( 'NONE', #23025, 30.00000000000000000 ) ;
#55553 = DIRECTION ( 'NONE',  ( 0.000000000000000000, 0.000000000000000000, 1.000000000000000000 ) ) ;
#55554 = CIRCLE ( 'NONE', #49925, 25.00000000000296296 ) ;
#55555 = FACE_OUTER_BOUND ( 'NONE', #4514, .T. ) ;
#55556 = EDGE_LOOP ( 'NONE', ( #28720, #56893, #18980, #6469 ) ) ;
#55557 = AXIS2_PLACEMENT_3D ( 'NONE', #62764, #42339, #63453 ) ;
#55558 = DIRECTION ( 'NONE',  ( 0.000000000000000000, 1.000000000000000000, 0.000000000000000000 ) ) ;
#55559 = EDGE_LOOP ( 'NONE', ( #21136, #16620 ) ) ;
#55560 = CARTESIAN_POINT ( 'NONE',  ( 164.9697211531230039, 63.72502658717166213, -17.07644040156450416 ) ) ;
#55561 = DIRECTION ( 'NONE',  ( -0.3978785209734125861, -0.9174381082928753095, 0.000000000000000000 ) ) ;
#55562 = CARTESIAN_POINT ( 'NONE',  ( 211.7634543339367781, 118.4123239814494610, -95.00000000000133582 ) ) ;
#55563 = CARTESIAN_POINT ( 'NONE',  ( 139.7928618793172859, 45.12615179300590285, -65.77714084613532464 ) ) ;
#55564 = CARTESIAN_POINT ( 'NONE',  ( 60.82895951008336510, 30.68107831874607072, 170.0000000000000000 ) ) ;
#55565 = PRODUCT_DEFINITION ( 'UNKNOWN', '', #32152, #9955 ) ;
#55566 = VERTEX_POINT ( 'NONE', #19846 ) ;
#55567 = B_SPLINE_CURVE_WITH_KNOTS ( 'NONE', 3,
 ( #10171, #6274, #5580, #42530, #27033, #54093 ),
 .UNSPECIFIED., .F., .F.,
 ( 4, 2, 4 ),
 ( 1.095770181117380865E-06, 0.03239442681617711595, 0.06478775786217311206 ),
 .UNSPECIFIED. ) ;
#55568 = ADVANCED_FACE ( 'NONE', ( #62409, #30063 ), #2628, .F. ) ;
#55569 = ORIENTED_EDGE ( 'NONE', *, *, #38589, .T. ) ;
#55570 = CYLINDRICAL_SURFACE ( 'NONE', #35118, 7.500000000000013323 ) ;
#55571 = VERTEX_POINT ( 'NONE', #24781 ) ;
#55573 = ADVANCED_FACE ( 'NONE', ( #14564 ), #68383, .T. ) ;
#55572 = DIRECTION ( 'NONE',  ( 0.000000000000000000, 0.000000000000000000, 1.000000000000000000 ) ) ;
#55574 = CARTESIAN_POINT ( 'NONE',  ( 442.3372781065085633, 367.0710678118653050, 108.5502958579886439 ) ) ;
#55575 = EDGE_LOOP ( 'NONE', ( #10836, #24737, #20781, #7513 ) ) ;
#55576 = LINE ( 'NONE', #54161, #12830 ) ;
#55577 = CARTESIAN_POINT ( 'NONE',  ( 93.09528872995973359, 21.72934119836186184, 14.19978795179650710 ) ) ;
#55578 = CARTESIAN_POINT ( 'NONE',  ( 164.8471526211111495, 63.62172173173271972, -42.24226993237041938 ) ) ;
#55579 = VERTEX_POINT ( 'NONE', #20184 ) ;
#55580 = DIRECTION ( 'NONE',  ( 1.000000000000000000, -0.000000000000000000, -0.000000000000000000 ) ) ;
#55581 = CARTESIAN_POINT ( 'NONE',  ( 56.17775956989186881, 12.21653819234432703, 87.90252147785352577 ) ) ;
#55582 = CARTESIAN_POINT ( 'NONE',  ( 196.9999999999999716, 0.000000000000000000, 0.000000000000000000 ) ) ;
#55583 = AXIS2_PLACEMENT_3D ( 'NONE', #31808, #26187, #53241 ) ;
#55584 = CARTESIAN_POINT ( 'NONE',  ( -180.6215424137752166, 97.48070480470860844, -41.90601408175744069 ) ) ;
#55585 = CARTESIAN_POINT ( 'NONE',  ( -126.3458714439411921, 46.79154809309481777, -23.06915330777030348 ) ) ;
#55586 = CARTESIAN_POINT ( 'NONE',  ( 154.0401952541423327, 55.03227529428313147, 70.42760438175315585 ) ) ;
#55587 = EDGE_CURVE ( 'NONE', #28455, #32766, #56093, .T. ) ;
#55588 = FACE_BOUND ( 'NONE', #771, .T. ) ;
#55589 = ORIENTED_EDGE ( 'NONE', *, *, #25969, .F. ) ;
#55590 = CARTESIAN_POINT ( 'NONE',  ( 139.7883986595928434, 46.32091287009614433, -74.96433037504790775 ) ) ;
#55592 = EDGE_CURVE ( 'NONE', #12059, #32583, #51168, .T. ) ;
#55591 = DIRECTION ( 'NONE',  ( -0.000000000000000000, -0.000000000000000000, 1.000000000000000000 ) ) ;
#55593 = ORIENTED_EDGE ( 'NONE', *, *, #52497, .T. ) ;
#55594 = AXIS2_PLACEMENT_3D ( 'NONE', #36061, #3018, #40989 ) ;
#55595 = CARTESIAN_POINT ( 'NONE',  ( -149.7268278745401346, 65.68859631971237434, -49.81283053149198992 ) ) ;
#55596 = CARTESIAN_POINT ( 'NONE',  ( 209.6698611676811481, 115.2210955123518517, -11.34831209349323267 ) ) ;
#55597 = CIRCLE ( 'NONE', #37768, 65.36598343705435354 ) ;
#55598 = AXIS2_PLACEMENT_3D ( 'NONE', #54306, #15663, #37111 ) ;
#55599 = CARTESIAN_POINT ( 'NONE',  ( -31.92572261726339633, 10.69135962481465185, 30.21645440618915046 ) ) ;
#55600 = CARTESIAN_POINT ( 'NONE',  ( -171.4867114763004849, 85.32693843184998173, -49.54345430716655585 ) ) ;
#55601 = CARTESIAN_POINT ( 'NONE',  ( -7.330587818645181386, 7.867004275019547244, 45.11558103944723541 ) ) ;
#55602 = CARTESIAN_POINT ( 'NONE',  ( -422.6627218934914367, 0.000000000000000000, -141.4497041420118535 ) ) ;
#55603 = CARTESIAN_POINT ( 'NONE',  ( 31.11269837220812562, 31.11269837220800483, 2.000000000000001776 ) ) ;
#55604 = CARTESIAN_POINT ( 'NONE',  ( -0.5178428571329629637, 7.532057582089302983, -14.36748065752867909 ) ) ;
#55605 = FACE_OUTER_BOUND ( 'NONE', #46331, .T. ) ;
#55606 = CARTESIAN_POINT ( 'NONE',  ( 114.6890011751075917, 30.99337387307411973, 16.32607591214094356 ) ) ;
#55607 = CARTESIAN_POINT ( 'NONE',  ( -55.05276343752910151, 15.72344139423345588, -88.90542517938717992 ) ) ;
#55608 = ORIENTED_EDGE ( 'NONE', *, *, #26236, .T. ) ;
#55610 = AXIS2_PLACEMENT_3D ( 'NONE', #58181, #827, #63810 ) ;
#55609 = CARTESIAN_POINT ( 'NONE',  ( -97.49665543375861887, 31.53324358035377983, -36.71692140486827327 ) ) ;
#55611 = ORIENTED_EDGE ( 'NONE', *, *, #33006, .T. ) ;
#55612 = CARTESIAN_POINT ( 'NONE',  ( 110.2429982417149432, 28.88204397445228722, -62.76698815611734972 ) ) ;
#55613 = CARTESIAN_POINT ( 'NONE',  ( 46.12611922993085756, 10.39838587005582227, -19.60643483645174356 ) ) ;
#55614 = CARTESIAN_POINT ( 'NONE',  ( 46.85206196242843646, 9.495795933269468136, 63.26480904775041836 ) ) ;
#55615 = DIRECTION ( 'NONE',  ( 1.000000000000000000, 0.000000000000000000, 0.000000000000000000 ) ) ;
#55616 = CARTESIAN_POINT ( 'NONE',  ( 0.000000000000000000, 70.00000000000000000, 0.000000000000000000 ) ) ;
#55617 = LINE ( 'NONE', #60549, #9723 ) ;
#55618 = CARTESIAN_POINT ( 'NONE',  ( 62.60807349995172189, 13.61084778855394184, -89.40979201309710334 ) ) ;
#55619 = CARTESIAN_POINT ( 'NONE',  ( -2.374459999240554620, 25.00999262126967437, 3.061616997868437868E-16 ) ) ;
#55620 = VERTEX_POINT ( 'NONE', #13534 ) ;
#55621 = ORIENTED_EDGE ( 'NONE', *, *, #48949, .T. ) ;
#55622 = LINE ( 'NONE', #34878, #59003 ) ;
#55623 = CARTESIAN_POINT ( 'NONE',  ( -16.04603980063842883, -64.68484481756375715, 34.48241795236666007 ) ) ;
#55624 = LINE ( 'NONE', #2517, #46904 ) ;
#55625 = CARTESIAN_POINT ( 'NONE',  ( -168.7329347389696181, 83.83901812802760389, 59.06544427237531636 ) ) ;
#55626 = DIRECTION ( 'NONE',  ( 0.000000000000000000, 0.000000000000000000, 1.000000000000000000 ) ) ;
#55627 = DIRECTION ( 'NONE',  ( 0.000000000000000000, -0.7071067811865474617, -0.7071067811865474617 ) ) ;
#55628 = EDGE_LOOP ( 'NONE', ( #2978, #37198, #66146, #40917 ) ) ;
#55629 = CARTESIAN_POINT ( 'NONE',  ( 93.72687053612523300, 23.04134601640628333, 7.892519177242094841 ) ) ;
#55630 = FACE_OUTER_BOUND ( 'NONE', #54862, .T. ) ;
#55631 = CARTESIAN_POINT ( 'NONE',  ( 11.82929895397812814, 7.412564870773603154, 57.98450507560617950 ) ) ;
#55632 = B_SPLINE_CURVE_WITH_KNOTS ( 'NONE', 3,
 ( #4966, #26, #37312, #69335, #15186, #42265, #47515, #59111, #21158, #48540, #68974, #43276, #32401, #48890, #58766, #375, #64055, #10928, #64397, #16209, #42601, #63724, #31704, #26775, #15534, #31368, #27449, #10579, #11271, #32052, #53826, #32740, #36986, #54170, #5992, #36647, #38014, #52797, #21826, #58424, #64752, #16558, #48201, #50656, #60516, #43626, #2476 ),
 .UNSPECIFIED., .F., .F.,
 ( 4, 2, 2, 2, 2, 2, 2, 2, 2, 2, 2, 1, 2, 2, 2, 2, 2, 2, 2, 2, 2, 2, 2, 4 ),
 ( 0.000000000000000000, 0.003297771944419079955, 0.004122214930523814165, 0.004946657916628548375, 0.006595543888838025469, 0.007419986874942737128, 0.008244429861047451388, 0.009068872847152163047, 0.009893315833256876440, 0.01154220180546630149, 0.01236664479157101315, 0.01319108777767572481, 0.01401553076378043820, 0.01483997374988514986, 0.01566441673598986326, 0.01648885972209457318, 0.01813774569430401384, 0.01896218868040875152, 0.01978663166651348920, 0.02061107465261822688, 0.02143551763872296456, 0.02308440361093244339, 0.02473328958314192222, 0.02638217555535139758 ),
 .UNSPECIFIED. ) ;
#55633 = DIRECTION ( 'NONE',  ( 0.000000000000000000, 0.000000000000000000, 1.000000000000000000 ) ) ;
#55634 = DIRECTION ( 'NONE',  ( 0.000000000000000000, 0.000000000000000000, 1.000000000000000000 ) ) ;
#55635 = FACE_BOUND ( 'NONE', #53678, .T. ) ;
#55636 = VECTOR ( 'NONE', #27809, 1000.000000000000000 ) ;
#55637 = ORIENTED_EDGE ( 'NONE', *, *, #48418, .F. ) ;
#55638 = DIRECTION ( 'NONE',  ( 1.000000000000000000, 0.000000000000000000, 0.000000000000000000 ) ) ;
#55639 = DIRECTION ( 'NONE',  ( -0.000000000000000000, -0.000000000000000000, -1.000000000000000000 ) ) ;
#55640 = VECTOR ( 'NONE', #3533, 1000.000000000000000 ) ;
#55641 = LINE ( 'NONE', #7814, #13883 ) ;
#55642 = CYLINDRICAL_SURFACE ( 'NONE', #660, 21.50000000000000000 ) ;
#55643 = CARTESIAN_POINT ( 'NONE',  ( 155.7277429502854602, 56.30804678861343149, 2.756809054777331625 ) ) ;
#55644 = CARTESIAN_POINT ( 'NONE',  ( 82.95057496836383848, 18.19812356106674400, -63.61242132756339629 ) ) ;
#55645 = EDGE_CURVE ( 'NONE', #51139, #27226, #15090, .T. ) ;
#55646 = CONICAL_SURFACE ( 'NONE', #33213, 8.000000000000000000, 1.047197551196600296 ) ;
#55647 = AXIS2_PLACEMENT_3D ( 'NONE', #48093, #21715, #22068 ) ;
#55648 = VERTEX_POINT ( 'NONE', #30396 ) ;
#55649 = CARTESIAN_POINT ( 'NONE',  ( 57.39674746172462960, 11.43903079040059190, 15.46024453313638247 ) ) ;
#55650 = AXIS2_PLACEMENT_3D ( 'NONE', #41323, #4032, #25503 ) ;
#55651 = CARTESIAN_POINT ( 'NONE',  ( 201.9721407532275066, 104.3507814346147740, -36.82671456535588561 ) ) ;
#55652 = EDGE_CURVE ( 'NONE', #10057, #43150, #33067, .T. ) ;
#55653 = ORIENTED_EDGE ( 'NONE', *, *, #65595, .F. ) ;
#55654 = FACE_BOUND ( 'NONE', #3390, .T. ) ;
#55655 = EDGE_LOOP ( 'NONE', ( #67523, #43040, #65939, #43743 ) ) ;
#55656 = VECTOR ( 'NONE', #14592, 1000.000000000000000 ) ;
#55657 = CARTESIAN_POINT ( 'NONE',  ( 0.4964154566687932202, -8.859816792613647962, 0.6543471694412412720 ) ) ;
#55658 = LINE ( 'NONE', #7489, #57960 ) ;
#55659 = ADVANCED_FACE ( 'NONE', ( #34989 ), #3660, .F. ) ;
#55660 = FACE_OUTER_BOUND ( 'NONE', #3101, .T. ) ;
#55661 = ORIENTED_EDGE ( 'NONE', *, *, #56622, .T. ) ;
#55662 = EDGE_CURVE ( 'NONE', #20172, #56288, #38687, .T. ) ;
#55663 = ORIENTED_EDGE ( 'NONE', *, *, #43023, .F. ) ;
#55664 = DIRECTION ( 'NONE',  ( 0.000000000000000000, 0.000000000000000000, 1.000000000000000000 ) ) ;
#55665 = CARTESIAN_POINT ( 'NONE',  ( 163.1313205310724470, 63.49733392291054201, 41.83532195775659090 ) ) ;
#55666 = CARTESIAN_POINT ( 'NONE',  ( -150.3850953947692801, 66.25368649589884740, -61.69593361462676739 ) ) ;
#55667 = CARTESIAN_POINT ( 'NONE',  ( 66.07923263163411320, 14.44036440558000223, 3.618334148579396725 ) ) ;
#55668 = LINE ( 'NONE', #9130, #69096 ) ;
#55669 = ORIENTED_EDGE ( 'NONE', *, *, #61052, .F. ) ;
#55670 = LINE ( 'NONE', #39500, #28948 ) ;
#55671 = CARTESIAN_POINT ( 'NONE',  ( -55.05276343752909440, 15.72344139423348430, 18.47277718246750311 ) ) ;
#55672 = CARTESIAN_POINT ( 'NONE',  ( -127.6894679065405143, 48.89973668460848444, -8.273314918213934277 ) ) ;
#55674 = EDGE_CURVE ( 'NONE', #49213, #68160, #9285, .T. ) ;
#55673 = CARTESIAN_POINT ( 'NONE',  ( -156.0562654606047488, 71.30334311561915683, -92.33834972157848142 ) ) ;
#55675 = CARTESIAN_POINT ( 'NONE',  ( 112.1164716692773027, 29.75790342121397813, -9.300245223945209361 ) ) ;
#55676 = MECHANICAL_DESIGN_GEOMETRIC_PRESENTATION_REPRESENTATION (  '', ( #13521 ), #42508 ) ;
#55677 = CARTESIAN_POINT ( 'NONE',  ( 94.10318957145940999, 22.10801446288250105, 91.83129037648295423 ) ) ;
#55679 = VERTEX_POINT ( 'NONE', #4014 ) ;
#55678 = CARTESIAN_POINT ( 'NONE',  ( 313.9975424824652350, 170.0000000000000284, 536.6193948016162949 ) ) ;
#55680 = ORIENTED_EDGE ( 'NONE', *, *, #14306, .F. ) ;
#55681 = ORIENTED_EDGE ( 'NONE', *, *, #13430, .T. ) ;
#55682 = CARTESIAN_POINT ( 'NONE',  ( 42.71504753277076816, 8.863481902720399930, 17.30229059452629414 ) ) ;
#55683 = DIRECTION ( 'NONE',  ( -0.000000000000000000, 1.000000000000000000, -0.000000000000000000 ) ) ;
#55684 = DIRECTION ( 'NONE',  ( 0.000000000000000000, -1.000000000000000000, 0.000000000000000000 ) ) ;
#55685 = CARTESIAN_POINT ( 'NONE',  ( 0.000000000000000000, 0.000000000000000000, 40.00000000000003553 ) ) ;
#55686 = CARTESIAN_POINT ( 'NONE',  ( 181.0840389613909736, -170.0000000000000000, -43.72505766587962484 ) ) ;
#55687 = CARTESIAN_POINT ( 'NONE',  ( 209.0197447343145711, 114.2532834725572002, 84.26074548200141123 ) ) ;
#55688 = B_SPLINE_CURVE_WITH_KNOTS ( 'NONE', 3,
 ( #69496, #63888, #53994, #59625, #15698, #21314, #58593, #64577, #5819, #32567, #31880, #16390, #43452, #5141, #16039, #6169, #37490, #58940, #32227, #53662, #48716, #5485, #26939, #48366, #197, #21659, #64931, #37843, #34319, #39587, #28687, #27979, #17790, #33277, #1252, #39929, #65631, #56109, #50486, #66685, #44515, #17418, #22705, #61387, #45203, #61039 ),
 .UNSPECIFIED., .F., .F.,
 ( 4, 2, 2, 2, 2, 2, 2, 2, 2, 2, 2, 2, 2, 2, 2, 2, 2, 2, 2, 2, 2, 2, 4 ),
 ( 0.000000000000000000, 0.003635178948345886823, 0.005452768422518803129, 0.007270357896691719002, 0.008179152633778141376, 0.009087947370864565486, 0.01090553684503748136, 0.01181433158212392975, 0.01272312631921037988, 0.01363192105629682828, 0.01454071579338327667, 0.01544951053046972854, 0.01635830526755617867, 0.01726710000464262706, 0.01817589474172907546, 0.01908468947881552386, 0.01999348421590197225, 0.02090227895298842412, 0.02181107369007487251, 0.02362866316424780053, 0.02544625263842072507, 0.02726384211259365309, 0.02908143158676657763 ),
 .UNSPECIFIED. ) ;
#55689 = CARTESIAN_POINT ( 'NONE',  ( -65.36598343705435354, 0.000000000000000000, 41.38025477438755928 ) ) ;
#55690 = CARTESIAN_POINT ( 'NONE',  ( -10.00000000000000178, 35.26862320190615208, -9.999999999999998224 ) ) ;
#55691 = CARTESIAN_POINT ( 'NONE',  ( -11.78792974237933144, 7.181513757308655599, 31.24314124056975928 ) ) ;
#55692 = VERTEX_POINT ( 'NONE', #50812 ) ;
#55693 = AXIS2_PLACEMENT_3D ( 'NONE', #11722, #38463, #5748 ) ;
#55694 = LINE ( 'NONE', #33900, #18312 ) ;
#55695 = ORIENTED_EDGE ( 'NONE', *, *, #44240, .T. ) ;
#55696 = ORIENTED_EDGE ( 'NONE', *, *, #16445, .F. ) ;
#55697 = CARTESIAN_POINT ( 'NONE',  ( -17.36794314067741496, 70.00000000000000000, 24.46128678263259815 ) ) ;
#55698 = AXIS2_PLACEMENT_3D ( 'NONE', #63236, #36502, #53347 ) ;
#55699 = CARTESIAN_POINT ( 'NONE',  ( -55.05276343752909440, 14.68156374112638041, -35.21632399845986328 ) ) ;
#55700 = CARTESIAN_POINT ( 'NONE',  ( -38.17834711144558213, 11.81993749040892006, 94.71300855358852289 ) ) ;
#55701 = CARTESIAN_POINT ( 'NONE',  ( 117.6853163455685234, 33.60747889659833021, -15.51686428253033334 ) ) ;
#55702 = AXIS2_PLACEMENT_3D ( 'NONE', #164, #31499, #10042 ) ;
#55703 = VECTOR ( 'NONE', #44755, 1000.000000000000000 ) ;
#55704 = DIRECTION ( 'NONE',  ( -0.000000000000000000, -1.000000000000000000, -0.000000000000000000 ) ) ;
#55705 = DIRECTION ( 'NONE',  ( 1.000000000000000000, -0.000000000000000000, -0.000000000000000000 ) ) ;
#55706 = CARTESIAN_POINT ( 'NONE',  ( 140.9141742510256847, 47.05414327990550305, -19.26942019242481052 ) ) ;
#55707 = ORIENTED_EDGE ( 'NONE', *, *, #41782, .T. ) ;
#55708 = EDGE_LOOP ( 'NONE', ( #28787, #14705, #42137, #45233 ) ) ;
#55709 = CIRCLE ( 'NONE', #16383, 8.000000000000000000 ) ;
#55710 = EDGE_LOOP ( 'NONE', ( #63491, #57684, #31824, #23358 ) ) ;
#55711 = LINE ( 'NONE', #11389, #47315 ) ;
#55712 = VECTOR ( 'NONE', #12789, 1000.000000000000000 ) ;
#55713 = CARTESIAN_POINT ( 'NONE',  ( 0.06809871960542812630, 6.146186931204408843, 5.354491962338127742 ) ) ;
#55714 = CARTESIAN_POINT ( 'NONE',  ( -14.27739063142107589, 30.22315691998191056, 6.893342933292202268 ) ) ;
#55715 = CARTESIAN_POINT ( 'NONE',  ( 55.51547041749725508, 11.05727559334829735, -16.61830272299990696 ) ) ;
#55716 = APPLICATION_CONTEXT ( 'automotive_design' ) ;
#55717 = UNCERTAINTY_MEASURE_WITH_UNIT (LENGTH_MEASURE( 1.000000000000000082E-05 ), #18093, 'distance_accuracy_value', 'NONE');
#55718 = CARTESIAN_POINT ( 'NONE',  ( -52.45215874217871033, 13.99961488531755727, 30.77850105701925187 ) ) ;
#55719 = CARTESIAN_POINT ( 'NONE',  ( 202.7506655727288489, 105.3943386412348957, 70.80670385009113943 ) ) ;
#55720 = ORIENTED_EDGE ( 'NONE', *, *, #21156, .F. ) ;
#55721 = DIRECTION ( 'NONE',  ( -0.000000000000000000, -0.000000000000000000, -1.000000000000000000 ) ) ;
#55722 = DIRECTION ( 'NONE',  ( 0.000000000000000000, 6.123233995736870806E-17, -1.000000000000000000 ) ) ;
#55723 = DIRECTION ( 'NONE',  ( -4.565061778886334783E-18, 1.000000000000000000, 0.000000000000000000 ) ) ;
#55724 = DIRECTION ( 'NONE',  ( -0.3113469631412870142, 0.9502963056556088528, 3.155443620884047222E-30 ) ) ;
#55725 = B_SPLINE_CURVE_WITH_KNOTS ( 'NONE', 3,
 ( #23669, #23335, #22977, #49683, #29289, #13462, #44420, #50052, #34921, #56363, #44779, #66256, #22620, #34592, #2562, #50742, #12770, #12422, #61301, #38809, #18046, #66944, #28602, #60949, #44060, #34232, #50403, #12073, #1881, #17703, #55318, #39162, #54969, #40196, #18737, #65904, #60255, #2220, #1166, #45113, #66596, #33541, #7139, #18385, #55672, #30332, #41570, #8881 ),
 .UNSPECIFIED., .F., .F.,
 ( 4, 2, 2, 2, 2, 2, 2, 2, 2, 2, 2, 2, 2, 2, 2, 2, 2, 2, 2, 2, 2, 2, 2, 4 ),
 ( 0.02554216173022672010, 0.02715505844859231535, 0.02796150680777513900, 0.02876795516695796265, 0.03038085188532356137, 0.03199374860368915663, 0.03360664532205475535, 0.03441309368123755819, 0.03521954204042036102, 0.03602599039960316385, 0.03683243875878596668, 0.03844533547715157235, 0.03925178383633436824, 0.04005823219551716413, 0.04086468055469996696, 0.04167112891388276286, 0.04247757727306555875, 0.04328402563224835464, 0.04489692235061398806, 0.04650981906897962148, 0.04731626742816243125, 0.04812271578734524796, 0.04973561250571081893, 0.05134850922407639684 ),
 .UNSPECIFIED. ) ;
#55726 = EDGE_CURVE ( 'NONE', #39251, #168, #15895, .T. ) ;
#55727 = CARTESIAN_POINT ( 'NONE',  ( -180.4643341113398094, 95.69224917234934935, -40.65656990911850244 ) ) ;
#55728 = CARTESIAN_POINT ( 'NONE',  ( 103.8093541423578898, 26.01745837747064982, 6.379909146910426543 ) ) ;
#55729 = CARTESIAN_POINT ( 'NONE',  ( -169.1041038606267364, 82.76530082651281361, 5.127983675400830776 ) ) ;
#55730 = DIRECTION ( 'NONE',  ( -1.000000000000000000, 0.000000000000000000, 0.000000000000000000 ) ) ;
#55731 = FACE_BOUND ( 'NONE', #51239, .T. ) ;
#55732 = CARTESIAN_POINT ( 'NONE',  ( -189.4135091951039271, 107.3303746924218274, 93.77231123529229251 ) ) ;
#55733 = CARTESIAN_POINT ( 'NONE',  ( -1.319107422865894108, 6.554467368239800251, 60.69727779971288584 ) ) ;
#55734 = ORIENTED_EDGE ( 'NONE', *, *, #40356, .F. ) ;
#55735 = DIRECTION ( 'NONE',  ( -0.000000000000000000, -1.000000000000000000, -0.000000000000000000 ) ) ;
#55736 = CARTESIAN_POINT ( 'NONE',  ( -125.8938041572051105, 46.49392987655492959, -61.75825448869760237 ) ) ;
#55737 = CARTESIAN_POINT ( 'NONE',  ( -64.97888516016278970, 7.103257987405393159, 41.38025477438755928 ) ) ;
#55738 = CARTESIAN_POINT ( 'NONE',  ( 26.69682282325795697, -59.27986298182186431, 0.000000000000000000 ) ) ;
#55739 = CARTESIAN_POINT ( 'NONE',  ( 412.0000000000000000, 0.000000000000000000, 378.0000000000000000 ) ) ;
#55740 = EDGE_LOOP ( 'NONE', ( #54514, #61222, #14311, #58412 ) ) ;
#55741 = FACE_OUTER_BOUND ( 'NONE', #17218, .T. ) ;
#55742 = DIRECTION ( 'NONE',  ( 1.000000000000000000, 0.000000000000000000, 0.000000000000000000 ) ) ;
#55743 = EDGE_CURVE ( 'NONE', #53205, #63094, #31775, .T. ) ;
#55744 = VERTEX_POINT ( 'NONE', #15941 ) ;
#55745 = CIRCLE ( 'NONE', #27659, 65.00000000000000000 ) ;
#55746 = ORIENTED_EDGE ( 'NONE', *, *, #57967, .T. ) ;
#55747 = CARTESIAN_POINT ( 'NONE',  ( 173.5843421840238250, 71.34465141434347402, -43.42181600850904744 ) ) ;
#55748 = CARTESIAN_POINT ( 'NONE',  ( 154.4435090467314069, 56.59612921827834242, 43.77540956279869278 ) ) ;
#55749 = DIRECTION ( 'NONE',  ( -1.000000000000000000, 0.000000000000000000, 0.000000000000000000 ) ) ;
#55750 = EDGE_LOOP ( 'NONE', ( #66936, #35142 ) ) ;
#55751 = DIRECTION ( 'NONE',  ( -1.000000000000000000, -0.000000000000000000, -0.000000000000000000 ) ) ;
#55752 = VECTOR ( 'NONE', #18593, 1000.000000000000000 ) ;
#55753 = LINE ( 'NONE', #2296, #56968 ) ;
#55754 = CARTESIAN_POINT ( 'NONE',  ( -0.5780275525703886252, 6.527356703336898214, 8.825157539075730639 ) ) ;
#55755 = ADVANCED_FACE ( 'NONE', ( #37738 ), #451, .T. ) ;
#55756 = CARTESIAN_POINT ( 'NONE',  ( -80.31482177285907653, 24.03632224640838189, 30.59770256097123919 ) ) ;
#55757 = VECTOR ( 'NONE', #39644, 1000.000000000000227 ) ;
#55758 = CARTESIAN_POINT ( 'NONE',  ( -27.70115495247213033, 10.02455692117576547, -9.452150211312456918 ) ) ;
#55759 = CARTESIAN_POINT ( 'NONE',  ( -52.00092620775821217, 14.92276858858357969, -22.72708555046020251 ) ) ;
#55760 = PRODUCT_DEFINITION_FORMATION_WITH_SPECIFIED_SOURCE ( 'ANY', '', #30563, .NOT_KNOWN. ) ;
#55761 = CIRCLE ( 'NONE', #19817, 20.00000000000000000 ) ;
#55762 = EDGE_LOOP ( 'NONE', ( #35782, #20371, #25218, #45009, #57758, #17501, #61103, #67254 ) ) ;
#55763 = CARTESIAN_POINT ( 'NONE',  ( 117.3281529665581786, 32.29994712002882551, -40.90972925606320842 ) ) ;
#55764 = VECTOR ( 'NONE', #69183, 1000.000000000000114 ) ;
#55765 = DIRECTION ( 'NONE',  ( -1.000000000000000000, 0.000000000000000000, 0.000000000000000000 ) ) ;
#55766 = EDGE_CURVE ( 'NONE', #33414, #61115, #16286, .T. ) ;
#55767 = CARTESIAN_POINT ( 'NONE',  ( 46.70715146412977958, 9.472433765546995232, -44.83575853474970074 ) ) ;
#55768 = LINE ( 'NONE', #1965, #39899 ) ;
#55770 = ORIENTED_EDGE ( 'NONE', *, *, #56278, .F. ) ;
#55769 = CARTESIAN_POINT ( 'NONE',  ( -120.8809492823584435, 43.28069332005611614, 86.22209529451693300 ) ) ;
#55771 = CARTESIAN_POINT ( 'NONE',  ( 81.03898448521320574, 17.58847173596444335, -48.34590843317131004 ) ) ;
#55772 = ADVANCED_FACE ( 'NONE', ( #38436 ), #59525, .T. ) ;
#55773 = EDGE_CURVE ( 'NONE', #61844, #51807, #26338, .T. ) ;
#55774 = EDGE_LOOP ( 'NONE', ( #31884, #33610, #39430, #15820 ) ) ;
#55775 = B_SPLINE_CURVE_WITH_KNOTS ( 'NONE', 3,
 ( #2468, #7752, #56978, #62605, #23922, #51005, #35864, #14412, #24278, #67201, #23580, #3502, #66504, #28860, #50310, #13373, #40784, #50646, #61887, #56269, #29534, #46062, #18294, #67531, #19331, #45374, #2814, #62241, #66852, #18643, #35518, #45724, #8795, #2128, #40103, #67883, #41138, #20364, #63968, #62939, #58679, #37227, #42172, #47782 ),
 .UNSPECIFIED., .F., .F.,
 ( 4, 2, 2, 2, 2, 2, 2, 2, 2, 2, 2, 2, 2, 2, 2, 2, 2, 2, 2, 2, 2, 4 ),
 ( 0.000000000000000000, 0.003360573201437790872, 0.004200716501797208992, 0.005040859802156626678, 0.006721146402875383119, 0.007561289703234740957, 0.008401433003594098795, 0.009241576303953457500, 0.01008171960431281620, 0.01176200620503154576, 0.01260214950539091140, 0.01344229280575027705, 0.01428243610610964269, 0.01512257940646901180, 0.01680286600718775003, 0.01764300930754711741, 0.01848315260790648826, 0.02016343920862520914, 0.02184372580934392655, 0.02352401241006264743, 0.02520429901078136484, 0.02688458561150008225 ),
 .UNSPECIFIED. ) ;
#55776 = LINE ( 'NONE', #62077, #46961 ) ;
#55777 = CARTESIAN_POINT ( 'NONE',  ( 81.74250361646207352, 18.86685472882137304, 42.92257895484420516 ) ) ;
#55778 = DIRECTION ( 'NONE',  ( -6.405132834375898112E-16, 1.000000000000000000, 1.281026566875181792E-15 ) ) ;
#55779 = CARTESIAN_POINT ( 'NONE',  ( 57.25833571151937207, -48.36523237396138342, 41.38025477438755928 ) ) ;
#55780 = CARTESIAN_POINT ( 'NONE',  ( 139.6203063421347395, 45.01495791936838486, -21.50363658416259582 ) ) ;
#55781 = CARTESIAN_POINT ( 'NONE',  ( 43.14565945994674223, 9.942782559600559011, 4.065828422660362484 ) ) ;
#55782 = CARTESIAN_POINT ( 'NONE',  ( 18.65373113224114832, 7.616233774882145369, -89.76416870551544491 ) ) ;
#55783 = DIRECTION ( 'NONE',  ( -0.000000000000000000, -0.000000000000000000, -1.000000000000000000 ) ) ;
#55784 = ORIENTED_EDGE ( 'NONE', *, *, #35419, .T. ) ;
#55785 = ORIENTED_EDGE ( 'NONE', *, *, #40753, .F. ) ;
#55786 = CARTESIAN_POINT ( 'NONE',  ( 109.7724924842965777, 28.66436020578542809, 71.45576479620103783 ) ) ;
#55787 = CARTESIAN_POINT ( 'NONE',  ( 164.8886903222557407, 63.65672212134879260, 62.61455516568165081 ) ) ;
#55788 = DIRECTION ( 'NONE',  ( 0.000000000000000000, 0.000000000000000000, -1.000000000000000000 ) ) ;
#55789 = DIRECTION ( 'NONE',  ( 0.7530714660036099684, 0.6579387259397136978, 0.000000000000000000 ) ) ;
#55790 = CARTESIAN_POINT ( 'NONE',  ( 30.47484983475695586, 59.26962220273969706, 34.48241823991043020 ) ) ;
#55791 = CARTESIAN_POINT ( 'NONE',  ( -108.9452487746634120, 36.29752968355630571, 61.38692384849660755 ) ) ;
#55792 = CYLINDRICAL_SURFACE ( 'NONE', #62037, 7.500000000000013323 ) ;
#55793 = LINE ( 'NONE', #66708, #22830 ) ;
#55794 = ORIENTED_EDGE ( 'NONE', *, *, #2401, .T. ) ;
#55795 = PRODUCT_DEFINITION_SHAPE ( 'NONE', 'NONE',  #46499 ) ;
#55796 = EDGE_LOOP ( 'NONE', ( #66090, #63867, #22411, #3706 ) ) ;
#55797 = VERTEX_POINT ( 'NONE', #54243 ) ;
#55798 = AXIS2_PLACEMENT_3D ( 'NONE', #46335, #51969, #29825 ) ;
#55799 = CARTESIAN_POINT ( 'NONE',  ( 262.2186286510350328, 0.000000000000000000, 236.5504542314483274 ) ) ;
#55800 = CYLINDRICAL_SURFACE ( 'NONE', #31895, 7.500000000000020428 ) ;
#55801 = CARTESIAN_POINT ( 'NONE',  ( -84.54326985437108988, 24.64760594531652771, 69.44852943540219314 ) ) ;
#55802 = CARTESIAN_POINT ( 'NONE',  ( 6.123233995736766282E-16, 50.00000000000000000, 5.000000000000000000 ) ) ;
#55803 = CARTESIAN_POINT ( 'NONE',  ( -33.37998494234739155, 1.749200548590775117, 6.893342931535256568 ) ) ;
#55804 = AXIS2_PLACEMENT_3D ( 'NONE', #3816, #47066, #47396 ) ;
#55805 = LINE ( 'NONE', #17825, #57005 ) ;
#55806 = CARTESIAN_POINT ( 'NONE',  ( -95.20053778133913625, 30.43887292928078381, -18.19781731286621707 ) ) ;
#55807 = VECTOR ( 'NONE', #31235, 1000.000000000000000 ) ;
#55808 = CARTESIAN_POINT ( 'NONE',  ( 37.00112095025831138, 8.109340230899352520, 71.36796680436268048 ) ) ;
#55809 = LINE ( 'NONE', #67078, #66381 ) ;
#55810 = CARTESIAN_POINT ( 'NONE',  ( 44.98017955506416854, 25.41829140422818156, 26.66469104408689006 ) ) ;
#55812 = ORIENTED_EDGE ( 'NONE', *, *, #11980, .F. ) ;
#55811 = EDGE_CURVE ( 'NONE', #11580, #25024, #65611, .T. ) ;
#55813 = FACE_OUTER_BOUND ( 'NONE', #56384, .T. ) ;
#55814 = CARTESIAN_POINT ( 'NONE',  ( -0.5751131641471393108, 6.527254166626919485, -40.98318541392706038 ) ) ;
#55815 = FACE_OUTER_BOUND ( 'NONE', #53231, .T. ) ;
#55816 = CARTESIAN_POINT ( 'NONE',  ( -7.825402957745085430, 7.899365992529246761, 18.27103044898354511 ) ) ;
#55817 = CARTESIAN_POINT ( 'NONE',  ( -147.3614567344830277, 62.37986555269947786, 18.57643577236105870 ) ) ;
#55818 = LINE ( 'NONE', #2014, #26477 ) ;
#55819 = CARTESIAN_POINT ( 'NONE',  ( 201.9869293910475392, 102.6997661182766990, 70.55695970202656042 ) ) ;
#55820 = CARTESIAN_POINT ( 'NONE',  ( 126.6266894765172850, 38.37986986668738609, -14.61571443927980418 ) ) ;
#55821 = ADVANCED_FACE ( 'NONE', ( #23319 ), #28582, .T. ) ;
#55822 = AXIS2_PLACEMENT_3D ( 'NONE', #24286, #29206, #45379 ) ;
#55823 = ORIENTED_EDGE ( 'NONE', *, *, #11261, .F. ) ;
#55824 = DIRECTION ( 'NONE',  ( 9.830670564645161641E-15, -3.582068857269162787E-15, 0.9999999999999997780 ) ) ;
#55825 = DIRECTION ( 'NONE',  ( 0.8584487936018728726, -0.5128992774058949156, 0.000000000000000000 ) ) ;
#55826 = CARTESIAN_POINT ( 'NONE',  ( -31.43908319763709969, 10.61114334766715928, -50.31719736520186359 ) ) ;
#55827 = DIRECTION ( 'NONE',  ( -0.7071067811865476838, -1.110223024625156294E-16, -0.7071067811865474617 ) ) ;
#55828 = CARTESIAN_POINT ( 'NONE',  ( 213.7150814747576817, 0.000000000000000000, 277.7615984639418798 ) ) ;
#55829 = ORIENTED_EDGE ( 'NONE', *, *, #31364, .T. ) ;
#55830 = CARTESIAN_POINT ( 'NONE',  ( -120.4586945679390766, 43.01762219615312688, -37.22256326113324576 ) ) ;
#55831 = EDGE_CURVE ( 'NONE', #33798, #19006, #44243, .T. ) ;
#55832 = CARTESIAN_POINT ( 'NONE',  ( -142.0062637385110236, 58.06920992247432167, -14.91780738418984420 ) ) ;
#55833 = CARTESIAN_POINT ( 'NONE',  ( -7.330587818645182274, 7.867004275019543691, -62.26262132240751157 ) ) ;
#55834 = EDGE_CURVE ( 'NONE', #32488, #33166, #34215, .T. ) ;
#55835 = CARTESIAN_POINT ( 'NONE',  ( 164.2838686904782151, 64.46257747810135186, 93.81936057118011263 ) ) ;
#55836 = EDGE_CURVE ( 'NONE', #28100, #62198, #66261, .T. ) ;
#55837 = EDGE_LOOP ( 'NONE', ( #21041, #59965, #61168, #57312 ) ) ;
#55838 = CARTESIAN_POINT ( 'NONE',  ( 161.3396229061448821, 62.02013338058599601, -90.87705086538740318 ) ) ;
#55839 = DIRECTION ( 'NONE',  ( -0.000000000000000000, -0.000000000000000000, 1.000000000000000000 ) ) ;
#55840 = FACE_OUTER_BOUND ( 'NONE', #35594, .T. ) ;
#55841 = EDGE_CURVE ( 'NONE', #33379, #8644, #22602, .T. ) ;
#55842 = CARTESIAN_POINT ( 'NONE',  ( 16.28371206594635723, 6.516665886438624433, -35.51894409868580738 ) ) ;
#55844 = VERTEX_POINT ( 'NONE', #6431 ) ;
#55843 = CARTESIAN_POINT ( 'NONE',  ( 117.7442255600443275, 33.63739995216996448, 9.767747294482646225 ) ) ;
#55845 = CARTESIAN_POINT ( 'NONE',  ( 56.53635105806416306, 11.26263375223564367, 33.52739349540972569 ) ) ;
#55846 = ORIENTED_EDGE ( 'NONE', *, *, #58933, .T. ) ;
#55847 = EDGE_LOOP ( 'NONE', ( #19188, #40874, #17057, #27804 ) ) ;
#55848 = VECTOR ( 'NONE', #59833, 1000.000000000000000 ) ;
#55849 = CARTESIAN_POINT ( 'NONE',  ( 173.5844030397476274, 72.71952271766126330, 36.50363886079529863 ) ) ;
#55850 = EDGE_CURVE ( 'NONE', #64355, #49951, #39479, .T. ) ;
#55851 = CARTESIAN_POINT ( 'NONE',  ( 16.28371206594634657, 6.516665886438621769, -62.36349468914946215 ) ) ;
#55852 = CIRCLE ( 'NONE', #59185, 25.12245591505646303 ) ;
#55854 = EDGE_LOOP ( 'NONE', ( #51227, #22213, #17142, #5912 ) ) ;
#55853 = CARTESIAN_POINT ( 'NONE',  ( -13.92109095214679648, 8.375243258322925044, -74.13901166531486808 ) ) ;
#55855 = DIRECTION ( 'NONE',  ( -0.000000000000000000, -0.000000000000000000, 1.000000000000000000 ) ) ;
#55856 = CARTESIAN_POINT ( 'NONE',  ( -23.93895920923072396, 9.495000752338446759, 37.47437177380988516 ) ) ;
#55857 = EDGE_CURVE ( 'NONE', #16162, #51932, #66241, .T. ) ;
#55858 = EDGE_CURVE ( 'NONE', #6300, #28769, #44046, .T. ) ;
#55859 = CARTESIAN_POINT ( 'NONE',  ( -76.32456871438915869, 22.51591205926308703, -49.75660205866648056 ) ) ;
#55860 = AXIS2_PLACEMENT_3D ( 'NONE', #51948, #12946, #3762 ) ;
#55861 = EDGE_LOOP ( 'NONE', ( #35523, #62497, #51269, #64558 ) ) ;
#55862 = VECTOR ( 'NONE', #67565, 999.9999999999998863 ) ;
#55863 = CARTESIAN_POINT ( 'NONE',  ( 210.5008983495072243, 116.4753531594350733, -65.91294173661489708 ) ) ;
#55864 = AXIS2_PLACEMENT_3D ( 'NONE', #5747, #15966, #48994 ) ;
#55865 = DIRECTION ( 'NONE',  ( 0.7071067811865487940, 0.000000000000000000, 0.7071067811865462405 ) ) ;
#55866 = CARTESIAN_POINT ( 'NONE',  ( 154.9796718954650601, 55.73967834827486456, -90.22953998753959581 ) ) ;
#55867 = CARTESIAN_POINT ( 'NONE',  ( -7.825402957745085430, -170.0000000000000000, -23.57352014148015584 ) ) ;
#55868 = CARTESIAN_POINT ( 'NONE',  ( 21.43750346857337519, 7.754771113113076986, 69.31663613037677862 ) ) ;
#55869 = VERTEX_POINT ( 'NONE', #33528 ) ;
#55870 = VERTEX_POINT ( 'NONE', #17322 ) ;
#55871 = ORIENTED_EDGE ( 'NONE', *, *, #50276, .F. ) ;
#55872 = CARTESIAN_POINT ( 'NONE',  ( -63.58578643762691485, 7.787012983210697559E-15, 41.41421356237313489 ) ) ;
#55873 = FACE_OUTER_BOUND ( 'NONE', #22456, .T. ) ;
#55874 = CARTESIAN_POINT ( 'NONE',  ( -37.07086358537071646, 10.58360809068249964, -37.84001496053501512 ) ) ;
#55875 = DIRECTION ( 'NONE',  ( 0.000000000000000000, 0.4999999999999998890, -0.8660254037844387076 ) ) ;
#55876 = DIRECTION ( 'NONE',  ( -1.000000000000000000, -0.000000000000000000, -0.000000000000000000 ) ) ;
#55877 = DIRECTION ( 'NONE',  ( -0.9009688679024155933, -0.4338837391175656699, 0.000000000000000000 ) ) ;
#55878 = CARTESIAN_POINT ( 'NONE',  ( -71.57660578921959882, 20.81129687646279436, -13.27386354321084383 ) ) ;
#55879 = ORIENTED_EDGE ( 'NONE', *, *, #49858, .T. ) ;
#55880 = CARTESIAN_POINT ( 'NONE',  ( 85.67138972405898301, 19.09593469918313957, 56.60270476246709137 ) ) ;
#55881 = ORIENTED_EDGE ( 'NONE', *, *, #37008, .F. ) ;
#55882 = CARTESIAN_POINT ( 'NONE',  ( 35.65685430025423841, 7.951642554322390311, 43.93025521648888798 ) ) ;
#55883 = PLANE ( 'NONE',  #49814 ) ;
#55884 = DIRECTION ( 'NONE',  ( 1.387778780781445922E-16, -1.000000000000000000, -1.232595164407830946E-32 ) ) ;
#55885 = DIRECTION ( 'NONE',  ( 0.9362348706397369824, 0.3513748240813435175, 0.000000000000000000 ) ) ;
#55886 = CARTESIAN_POINT ( 'NONE',  ( -125.8938041572051389, 47.69968343338778283, -23.06915330777029638 ) ) ;
#55887 = CARTESIAN_POINT ( 'NONE',  ( -51.77439426130688815, 13.82695438436703128, 17.72271401957979364 ) ) ;
#55888 = DIRECTION ( 'NONE',  ( 0.000000000000000000, 0.000000000000000000, -1.000000000000000000 ) ) ;
#55889 = ORIENTED_EDGE ( 'NONE', *, *, #5396, .F. ) ;
#55890 = VECTOR ( 'NONE', #35850, 1000.000000000000000 ) ;
#55891 = CARTESIAN_POINT ( 'NONE',  ( -783.0172411895269988, -622.0000000000060254, 0.000000000000000000 ) ) ;
#55892 = DIRECTION ( 'NONE',  ( 1.000000000000000000, 0.000000000000000000, 0.000000000000000000 ) ) ;
#55893 = ORIENTED_EDGE ( 'NONE', *, *, #27843, .F. ) ;
#55894 = CARTESIAN_POINT ( 'NONE',  ( -30.62628708973388569, 68.47330165179126027, 170.0000000000000000 ) ) ;
#55895 = CARTESIAN_POINT ( 'NONE',  ( -61.53550548562874667, 17.56596194025584978, 68.46545811016181915 ) ) ;
#55896 = CARTESIAN_POINT ( 'NONE',  ( -452.6627218934862071, 370.0000000000064233, -141.4497041420121661 ) ) ;
#55897 = ORIENTED_EDGE ( 'NONE', *, *, #16653, .F. ) ;
#55898 = CARTESIAN_POINT ( 'NONE',  ( 24.34427655538957680, -5.688250960945929080, 0.000000000000000000 ) ) ;
#55899 = CARTESIAN_POINT ( 'NONE',  ( 151.1827182658834374, 54.16800928478855326, -74.58909220960448749 ) ) ;
#55900 = CARTESIAN_POINT ( 'NONE',  ( -33.83558513595454542, 9.996963989836507025, 44.82747360581453933 ) ) ;
#55901 =( BOUNDED_CURVE ( )  B_SPLINE_CURVE ( 3, ( #27164, #64116, #22247, #11331 ),
 .UNSPECIFIED., .F., .F. ) 
 B_SPLINE_CURVE_WITH_KNOTS ( ( 4, 4 ),
 ( 2.398060303794313342, 2.801953471882904001 ),
 .UNSPECIFIED. ) 
 CURVE ( )  GEOMETRIC_REPRESENTATION_ITEM ( )  RATIONAL_B_SPLINE_CURVE ( ( 1.000000000000000000, 0.9864519964717846090, 0.9864519964717846090, 1.000000000000000000 ) ) 
 REPRESENTATION_ITEM ( '' )  );
#55902 = AXIS2_PLACEMENT_3D ( 'NONE', #60387, #65317, #17103 ) ;
#55903 = CARTESIAN_POINT ( 'NONE',  ( -30.46060138092287772, 9.432375387772214737, 72.01313598860062370 ) ) ;
#55904 = EDGE_CURVE ( 'NONE', #11779, #45015, #20758, .T. ) ;
#55905 = VECTOR ( 'NONE', #36695, 1000.000000000000000 ) ;
#55906 = ORIENTED_EDGE ( 'NONE', *, *, #23118, .T. ) ;
#55907 = CARTESIAN_POINT ( 'NONE',  ( 644.1895565744057421, 939.3221711212305536, 766.5068267248707343 ) ) ;
#55908 = CARTESIAN_POINT ( 'NONE',  ( -124.3250225421925990, 45.46958056770281331, 45.45752980411683097 ) ) ;
#55909 = ORIENTED_EDGE ( 'NONE', *, *, #28424, .F. ) ;
#55910 = LINE ( 'NONE', #29512, #35716 ) ;
#55911 = DIRECTION ( 'NONE',  ( -1.000000000000000000, 0.000000000000000000, 0.000000000000000000 ) ) ;
#55912 = DIRECTION ( 'NONE',  ( 0.000000000000000000, 1.000000000000000000, -0.000000000000000000 ) ) ;
#55913 = CARTESIAN_POINT ( 'NONE',  ( 128.2049106864180601, 39.27214849547761588, 85.72287850017508504 ) ) ;
#55914 = AXIS2_PLACEMENT_3D ( 'NONE', #54166, #38357, #5989 ) ;
#55915 = EDGE_CURVE ( 'NONE', #37097, #7708, #1497, .T. ) ;
#55916 = CARTESIAN_POINT ( 'NONE',  ( -5.000000000000026645, -15.55634918610403616, 85.00100000000000477 ) ) ;
#55917 = CARTESIAN_POINT ( 'NONE',  ( 427.4999999999999432, -18.06806526123148160, 378.0000000000000000 ) ) ;
#55918 = AXIS2_PLACEMENT_3D ( 'NONE', #21168, #6370, #11633 ) ;
#55919 = CARTESIAN_POINT ( 'NONE',  ( -121.2008155373973608, 43.48033530165983507, -75.12874222293449122 ) ) ;
#55920 = EDGE_CURVE ( 'NONE', #48281, #52460, #65890, .T. ) ;
#55921 = ORIENTED_EDGE ( 'NONE', *, *, #26667, .F. ) ;
#55922 = CARTESIAN_POINT ( 'NONE',  ( 160.9241720448059425, 60.38677655937337363, -10.10604509194042500 ) ) ;
#55923 = CARTESIAN_POINT ( 'NONE',  ( 0.000000000000000000, 0.000000000000000000, 40.00000000000003553 ) ) ;
#55924 = CARTESIAN_POINT ( 'NONE',  ( 64.93495251696904802, 13.12601614965099728, 56.90318657735401331 ) ) ;
#55925 = CARTESIAN_POINT ( 'NONE',  ( 140.4897729434290454, 45.57634363643753517, -66.82868248181939919 ) ) ;
#55926 = DIRECTION ( 'NONE',  ( -0.000000000000000000, -0.000000000000000000, 1.000000000000000000 ) ) ;
#55927 = ORIENTED_EDGE ( 'NONE', *, *, #47177, .T. ) ;
#55928 = CARTESIAN_POINT ( 'NONE',  ( 161.7031777507226877, 62.31724004902782355, -10.57123460863781261 ) ) ;
#55929 = CARTESIAN_POINT ( 'NONE',  ( 14.08699529666005823, 6.452200550165255066, 44.82328613664139993 ) ) ;
#55930 = VERTEX_POINT ( 'NONE', #12405 ) ;
#55931 = CARTESIAN_POINT ( 'NONE',  ( -125.8938041572051105, 47.69968343338781835, 45.61994787315711619 ) ) ;
#55932 = CARTESIAN_POINT ( 'NONE',  ( 129.2374845572065851, 38.70429341380298638, -91.29071524815627470 ) ) ;
#55933 = ORIENTED_EDGE ( 'NONE', *, *, #69325, .F. ) ;
#55934 = CARTESIAN_POINT ( 'NONE',  ( -148.4259959918497600, 63.26767374754766138, -61.73259096974960869 ) ) ;
#55935 = DIRECTION ( 'NONE',  ( 1.000000000000000000, 0.000000000000000000, 0.000000000000000000 ) ) ;
#55936 = DIRECTION ( 'NONE',  ( 1.000000000000000000, 0.000000000000000000, -0.000000000000000000 ) ) ;
#55937 = ADVANCED_FACE ( 'NONE', ( #65172 ), #33862, .T. ) ;
#55938 = CARTESIAN_POINT ( 'NONE',  ( 164.9709596662455340, 63.72607097915130936, -43.36052436387029729 ) ) ;
#55939 = EDGE_LOOP ( 'NONE', ( #54723, #59790 ) ) ;
#55940 = CIRCLE ( 'NONE', #60406, 5.000000000000004441 ) ;
#55941 = EDGE_CURVE ( 'NONE', #42689, #14285, #38571, .T. ) ;
#55942 = CARTESIAN_POINT ( 'NONE',  ( -39.09764951710990744, -70.01774562958885895, 73.58025477438756923 ) ) ;
#55943 = CARTESIAN_POINT ( 'NONE',  ( 69.72022767004882837, 15.36837594864515388, 94.43018735991657309 ) ) ;
#55944 = AXIS2_PLACEMENT_3D ( 'NONE', #60648, #45861, #67332 ) ;
#55945 = CARTESIAN_POINT ( 'NONE',  ( 34.83823433017388282, 8.871835168107979896, 31.44169914746493788 ) ) ;
#55946 = DIRECTION ( 'NONE',  ( -0.5773502691896255090, 0.5773502691896258421, 0.5773502691896258421 ) ) ;
#55947 = CARTESIAN_POINT ( 'NONE',  ( -125.8938041572051389, 46.49392987655490828, -8.069153307770243089 ) ) ;
#55948 = CARTESIAN_POINT ( 'NONE',  ( 34.13137819193417499, 8.793608427416353734, -91.40789414581379901 ) ) ;
#55949 = CARTESIAN_POINT ( 'NONE',  ( 130.7260704202054455, 39.56565398554879920, -77.19931493661745492 ) ) ;
#55950 = B_SPLINE_CURVE_WITH_KNOTS ( 'NONE', 3,
 ( #59377, #5905, #54086, #16813, #28416, #59031, #54797, #32659, #49868, #649, #23154, #11889, #55143, #44241, #22448, #54437, #5573, #65017 ),
 .UNSPECIFIED., .F., .F.,
 ( 4, 2, 2, 2, 2, 2, 2, 2, 4 ),
 ( 0.01277287546153429119, 0.01590198764852522595, 0.01746654374202068205, 0.01903109983551613815, 0.01981337788226390437, 0.02059565592901167058, 0.02216021202250712668, 0.02372476811600258279, 0.02528932420949803542 ),
 .UNSPECIFIED. ) ;
#55951 = EDGE_LOOP ( 'NONE', ( #11442, #51584, #57888, #43693 ) ) ;
#55952 = LINE ( 'NONE', #13724, #18616 ) ;
#55953 = AXIS2_PLACEMENT_3D ( 'NONE', #25557, #46990, #10050 ) ;
#55954 = CARTESIAN_POINT ( 'NONE',  ( -14.92860730136983705, 8.468845235798745819, 62.04033186115039911 ) ) ;
#55955 = ORIENTED_EDGE ( 'NONE', *, *, #23656, .T. ) ;
#55956 = DIRECTION ( 'NONE',  ( -0.000000000000000000, -0.000000000000000000, -1.000000000000000000 ) ) ;
#55957 = VECTOR ( 'NONE', #7931, 1000.000000000000000 ) ;
#55958 = CARTESIAN_POINT ( 'NONE',  ( -2.113472939310175658, 74.92159864268209901, 41.38025477438755928 ) ) ;
#55959 = DIRECTION ( 'NONE',  ( 0.000000000000000000, -0.000000000000000000, 1.000000000000000000 ) ) ;
#55960 = DIRECTION ( 'NONE',  ( 0.000000000000000000, 0.000000000000000000, 1.000000000000000000 ) ) ;
#55961 = CARTESIAN_POINT ( 'NONE',  ( -22.06416059020174103, -12.01293505575318044, 3.061616997868437868E-16 ) ) ;
#55962 = CARTESIAN_POINT ( 'NONE',  ( -49.45858366215606594, 13.25262207532078662, -74.56246164764421280 ) ) ;
#55963 = CARTESIAN_POINT ( 'NONE',  ( 31.11269837220800127, -26.11269837220812562, 0.000000000000000000 ) ) ;
#55964 = CARTESIAN_POINT ( 'NONE',  ( -10.92576759990585700, 8.121994053275061631, 44.44912068652092785 ) ) ;
#55965 = DIRECTION ( 'NONE',  ( -0.000000000000000000, -0.000000000000000000, -1.000000000000000000 ) ) ;
#55966 = ORIENTED_EDGE ( 'NONE', *, *, #8844, .T. ) ;
#55967 = VECTOR ( 'NONE', #25174, 1000.000000000000000 ) ;
#55968 = CARTESIAN_POINT ( 'NONE',  ( -95.04371414958063724, 30.36527049547254720, -44.55352501167941881 ) ) ;
#55969 = EDGE_LOOP ( 'NONE', ( #43594, #51189, #27960, #19347, #18209 ) ) ;
#55970 = CARTESIAN_POINT ( 'NONE',  ( 109.3047266816502088, 28.44977739115300253, -77.72287105795275863 ) ) ;
#55971 = CARTESIAN_POINT ( 'NONE',  ( 46.84154678921882464, 10.51341196666389521, -17.25711569787797828 ) ) ;
#55972 = CARTESIAN_POINT ( 'NONE',  ( 46.90141780929663895, 9.503798448769778417, 63.75374896832851590 ) ) ;
#55973 = CARTESIAN_POINT ( 'NONE',  ( -25.87147652227456263, 70.00000000000000000, 77.58025477438755502 ) ) ;
#55974 = CARTESIAN_POINT ( 'NONE',  ( -15.16549112504216268, 7.480664377850763103, 92.87927133262334678 ) ) ;
#55975 = B_SPLINE_CURVE_WITH_KNOTS ( 'NONE', 3,
 ( #16515, #11228, #691, #32694, #11571, #6308, #27760, #66130, #22840, #13675, #65768, #60475, #23550, #1741, #2098, #55899, #23890, #60814, #7012, #29503, #12289, #28466, #18613, #8407, #55539, #24249, #7718, #12641, #18958, #50967, #61174, #34461, #29166, #50615, #7372, #2433, #44988, #50274, #45336, #45692, #29857, #40067, #61522, #56586, #1383, #44281, #2779, #66818, #39371, #13341 ),
 .UNSPECIFIED., .F., .F.,
 ( 4, 2, 2, 2, 2, 2, 2, 2, 2, 2, 2, 2, 2, 2, 2, 2, 2, 2, 2, 2, 2, 2, 2, 2, 4 ),
 ( 0.02688458561150013429, 0.02770990876165297517, 0.02853523191180581606, 0.03018587821211148742, 0.03183652451241715531, 0.03266184766256999272, 0.03348717081272283708, 0.03513781711302847027, 0.03678846341333410347, 0.03761378656348691313, 0.03843910971363971585, 0.03926443286379251857, 0.04008975601394532129, 0.04174040231425089204, 0.04256572546440369476, 0.04339104861455649748, 0.04421637176470930020, 0.04504169491486210292, 0.04586701806501490564, 0.04669234121516771530, 0.04834298751547328604, 0.04916831066562603325, 0.04999363381577878046, 0.05164428011608426794, 0.05329492641638975542 ),
 .UNSPECIFIED. ) ;
#55976 = CARTESIAN_POINT ( 'NONE',  ( -34.75846525698938194, -54.92585086258257121, 170.0000000000000000 ) ) ;
#55977 = DIRECTION ( 'NONE',  ( -0.000000000000000000, 1.000000000000000000, -0.000000000000000000 ) ) ;
#55978 = LINE ( 'NONE', #25012, #30773 ) ;
#55979 = ORIENTED_EDGE ( 'NONE', *, *, #65946, .T. ) ;
#55980 = ORIENTED_EDGE ( 'NONE', *, *, #46510, .T. ) ;
#55981 = EDGE_CURVE ( 'NONE', #61751, #19234, #40518, .T. ) ;
#55982 = PLANE ( 'NONE',  #25341 ) ;
#55983 = FACE_OUTER_BOUND ( 'NONE', #35797, .T. ) ;
#55984 = LINE ( 'NONE', #7796, #66002 ) ;
#55985 = CARTESIAN_POINT ( 'NONE',  ( 0.7145311798163210826, 4.618802153517001408, -8.000000000000000000 ) ) ;
#55986 = EDGE_CURVE ( 'NONE', #45254, #59777, #2547, .T. ) ;
#55987 = CARTESIAN_POINT ( 'NONE',  ( -435.1627218934888788, 400.0000000000064801, -128.9497041420092387 ) ) ;
#55988 = CARTESIAN_POINT ( 'NONE',  ( 57.57684776206768618, 12.50442334002048561, -21.54617277829715505 ) ) ;
#55989 = ORIENTED_EDGE ( 'NONE', *, *, #30337, .T. ) ;
#55990 = CARTESIAN_POINT ( 'NONE',  ( 89.87840278991586729, 21.62393877508910123, 3.603499079925511328 ) ) ;
#55991 = CARTESIAN_POINT ( 'NONE',  ( 21.43750346857337874, 7.754771113113079650, -38.06156623147796125 ) ) ;
#55992 = CARTESIAN_POINT ( 'NONE',  ( 13.37708032728285623, 7.441924986912758833, 57.25317478596774379 ) ) ;
#55993 = FACE_OUTER_BOUND ( 'NONE', #11420, .T. ) ;
#55995 = LINE ( 'NONE', #12735, #42090 ) ;
#55994 = B_SPLINE_CURVE_WITH_KNOTS ( 'NONE', 3,
 ( #7386, #33069, #50627, #66487, #43947, #60137, #18279, #65425, #17217, #38692, #55919, #60491, #33427, #65073, #16872, #54853, #54496, #6677, #49572, #22854, #44303, #17582, #24262, #24953, #46736, #56961, #30920, #29518, #40768, #9459, #67864, #36190, #52365, #41472, #23905, #50984, #3483, #9112, #56601, #3833, #20018, #57649, #46384, #2800, #45355, #46044 ),
 .UNSPECIFIED., .F., .F.,
 ( 4, 2, 2, 2, 2, 2, 2, 2, 2, 2, 2, 2, 2, 2, 2, 2, 2, 2, 2, 2, 2, 2, 4 ),
 ( 0.02584318557310393699, 0.02743529570732774342, 0.02823135077443962929, 0.02902740584155151862, 0.03061951597577525913, 0.03221162610999900311, 0.03380373624422274015, 0.03459979131133462255, 0.03539584637844649800, 0.03619190144555838040, 0.03698795651267025586, 0.03858006664689401372, 0.03937612171400586836, 0.04017217678111772994, 0.04096823184822958458, 0.04176428691534143922, 0.04335639704956512075, 0.04494850718378880228, 0.04654061731801248381, 0.04813272745223615839, 0.04892878251934799916, 0.04972483758645983298, 0.05131694772068345900 ),
 .UNSPECIFIED. ) ;
#55996 = FACE_BOUND ( 'NONE', #49754, .T. ) ;
#55997 = EDGE_CURVE ( 'NONE', #33133, #24611, #8869, .T. ) ;
#55998 = VECTOR ( 'NONE', #5207, 1000.000000000000000 ) ;
#55999 = EDGE_CURVE ( 'NONE', #41255, #17804, #56702, .T. ) ;
#56000 = ORIENTED_EDGE ( 'NONE', *, *, #45983, .F. ) ;
#56001 = VECTOR ( 'NONE', #14398, 1000.000000000000000 ) ;
#56002 = ADVANCED_FACE ( 'NONE', ( #27756 ), #54833, .F. ) ;
#56003 = CARTESIAN_POINT ( 'NONE',  ( -447.6627218934916073, 369.9999999999953957, 108.5502958579925377 ) ) ;
#56004 = CARTESIAN_POINT ( 'NONE',  ( 88.53025347111699261, 21.14438024052373066, -50.59242619532921736 ) ) ;
#56005 = PLANE ( 'NONE',  #31858 ) ;
#56006 = DIRECTION ( 'NONE',  ( 0.000000000000000000, 0.000000000000000000, -1.000000000000000000 ) ) ;
#56007 = CARTESIAN_POINT ( 'NONE',  ( 207.8398359204632868, 112.5208221429021478, 56.73900988323001826 ) ) ;
#56008 = CARTESIAN_POINT ( 'NONE',  ( 410.0000000000000000, 0.000000000000000000, 2.000000000000000000 ) ) ;
#56009 = CIRCLE ( 'NONE', #58249, 242.4895526022646379 ) ;
#56010 = EDGE_LOOP ( 'NONE', ( #50182, #4877, #11973, #48301 ) ) ;
#56011 = DIRECTION ( 'NONE',  ( -1.000000000000000000, 0.000000000000000000, 0.000000000000000000 ) ) ;
#56012 = CARTESIAN_POINT ( 'NONE',  ( 197.4121679705847612, 98.46451029407252520, -45.61355052951746814 ) ) ;
#56013 = EDGE_LOOP ( 'NONE', ( #52458, #30820, #51315, #36192 ) ) ;
#56014 = CARTESIAN_POINT ( 'NONE',  ( 63.01563776193091826, -170.0000000000000000, -8.876140241706055534 ) ) ;
#56015 = ORIENTED_EDGE ( 'NONE', *, *, #814, .F. ) ;
#56016 = CARTESIAN_POINT ( 'NONE',  ( -84.22570405563702423, 24.51726571826274181, -64.40185529543865073 ) ) ;
#56017 = CARTESIAN_POINT ( 'NONE',  ( -46.66904755831210139, 5.000000000000066613, 0.000000000000000000 ) ) ;
#56018 = CARTESIAN_POINT ( 'NONE',  ( 90.30840373526891085, 21.77864858272155146, -76.70622861614346277 ) ) ;
#56019 = ORIENTED_EDGE ( 'NONE', *, *, #2481, .T. ) ;
#56020 = VERTEX_POINT ( 'NONE', #49198 ) ;
#56021 = CARTESIAN_POINT ( 'NONE',  ( 46.65860211212412878, 10.48377752989033951, 66.21745745935314176 ) ) ;
#56022 = PLANE ( 'NONE',  #1158 ) ;
#56023 = CARTESIAN_POINT ( 'NONE',  ( 22.89234820949993576, 6.832052815347870123, 8.252930022751796102 ) ) ;
#56024 = ORIENTED_EDGE ( 'NONE', *, *, #21156, .T. ) ;
#56025 = EDGE_CURVE ( 'NONE', #49164, #24416, #7007, .T. ) ;
#56026 = CARTESIAN_POINT ( 'NONE',  ( -125.8938041572051105, 46.49392987655492959, -61.75825448869760237 ) ) ;
#56027 = CARTESIAN_POINT ( 'NONE',  ( 62.52762183777209515, 13.59210632617625159, -35.72069083216972984 ) ) ;
#56028 = CARTESIAN_POINT ( 'NONE',  ( 0.000000000000000000, 0.000000000000000000, 170.0000000000000000 ) ) ;
#56029 = CARTESIAN_POINT ( 'NONE',  ( 117.4830770399668012, 32.37795270233553424, -14.55398040625970957 ) ) ;
#56030 = CARTESIAN_POINT ( 'NONE',  ( 90.96235852665459731, 20.94448655708621487, 84.74411175189248979 ) ) ;
#56032 = ORIENTED_EDGE ( 'NONE', *, *, #54760, .F. ) ;
#56031 = CARTESIAN_POINT ( 'NONE',  ( -168.9893587165131521, 84.11247246121824617, -89.62666367685146440 ) ) ;
#56033 = ORIENTED_EDGE ( 'NONE', *, *, #6454, .F. ) ;
#56034 = ORIENTED_EDGE ( 'NONE', *, *, #67745, .T. ) ;
#56035 = CARTESIAN_POINT ( 'NONE',  ( 0.4969600502617472215, -4.995646404165269949, 7.347286611336972584 ) ) ;
#56036 = CARTESIAN_POINT ( 'NONE',  ( -180.2731542922991252, 97.04988144230624414, 94.37081299702376214 ) ) ;
#56037 = CARTESIAN_POINT ( 'NONE',  ( -49.45858366215605884, 13.25262207532078307, -20.87336046671682155 ) ) ;
#56038 = DIRECTION ( 'NONE',  ( -0.000000000000000000, -0.000000000000000000, 1.000000000000000000 ) ) ;
#56039 = DIRECTION ( 'NONE',  ( -1.000000000000000000, 0.000000000000000000, 0.000000000000000000 ) ) ;
#56040 = CARTESIAN_POINT ( 'NONE',  ( 197.8192566318489298, 98.97502303561493875, 87.37853646849281120 ) ) ;
#56041 = CARTESIAN_POINT ( 'NONE',  ( 10.55634918610411432, 46.66904755831205875, 0.000000000000000000 ) ) ;
#56042 = CARTESIAN_POINT ( 'NONE',  ( -4.164416015344991173, -64.86646004871191451, 40.00000000000003553 ) ) ;
#56043 = CARTESIAN_POINT ( 'NONE',  ( 9.249622075198342230, 0.000000000000000000, 3.800590936420744193 ) ) ;
#56044 = VERTEX_POINT ( 'NONE', #28460 ) ;
#56045 = CARTESIAN_POINT ( 'NONE',  ( 12.04188192036245297, 7.416006018508748632, -22.67628800238064457 ) ) ;
#56046 = ORIENTED_EDGE ( 'NONE', *, *, #45079, .F. ) ;
#56047 = VERTEX_POINT ( 'NONE', #39366 ) ;
#56048 = CARTESIAN_POINT ( 'NONE',  ( -146.5230751932348596, 62.99205605665031271, 4.481088983380310253 ) ) ;
#56049 = CARTESIAN_POINT ( 'NONE',  ( 184.0001683447903815, 83.06228184427187955, -77.49291610268716113 ) ) ;
#56050 = CARTESIAN_POINT ( 'NONE',  ( -167.4844853368928455, 82.52074065752739784, 33.36765669216441665 ) ) ;
#56051 = CARTESIAN_POINT ( 'NONE',  ( 0.4973051450695318842, -3.866309095700718235, 8.000000000000000000 ) ) ;
#56052 = EDGE_CURVE ( 'NONE', #7827, #37858, #44277, .T. ) ;
#56053 = VECTOR ( 'NONE', #55553, 1000.000000000000000 ) ;
#56054 = ADVANCED_FACE ( 'NONE', ( #33748 ), #52192, .T. ) ;
#56055 = DIRECTION ( 'NONE',  ( 0.000000000000000000, 0.000000000000000000, -1.000000000000000000 ) ) ;
#56056 = FACE_OUTER_BOUND ( 'NONE', #27363, .T. ) ;
#56057 = CARTESIAN_POINT ( 'NONE',  ( 133.8566784816069060, 41.42467568809810530, -51.02331093239568816 ) ) ;
#56058 = ORIENTED_EDGE ( 'NONE', *, *, #59329, .F. ) ;
#56059 = VERTEX_POINT ( 'NONE', #11565 ) ;
#56060 = EDGE_CURVE ( 'NONE', #57871, #5356, #34099, .T. ) ;
#56061 = CARTESIAN_POINT ( 'NONE',  ( 188.5677332624426299, 88.01870958063736339, 89.96319809774311693 ) ) ;
#56062 = CARTESIAN_POINT ( 'NONE',  ( -33.15588667008874779, -4.239136283579393982, 6.893342931535249463 ) ) ;
#56063 = DIRECTION ( 'NONE',  ( -0.000000000000000000, 1.000000000000000000, -0.000000000000000000 ) ) ;
#56064 = EDGE_CURVE ( 'NONE', #35550, #56478, #65762, .T. ) ;
#56065 = LINE ( 'NONE', #38487, #44238 ) ;
#56066 = EDGE_CURVE ( 'NONE', #44487, #31187, #23394, .T. ) ;
#56067 = CARTESIAN_POINT ( 'NONE',  ( -54.09522495088361183, 14.42642983673693813, 30.36297380349473229 ) ) ;
#56068 = PLANE ( 'NONE',  #62087 ) ;
#56069 = VERTEX_POINT ( 'NONE', #28104 ) ;
#56070 = CARTESIAN_POINT ( 'NONE',  ( 45.78444578632068840, -59.41672343742509810, 170.0000000000000000 ) ) ;
#56071 = CARTESIAN_POINT ( 'NONE',  ( -59.58556642339448217, 16.99097764963620705, -63.56561058464538405 ) ) ;
#56072 = CARTESIAN_POINT ( 'NONE',  ( 203.1423857108908919, 105.9238244286950135, -78.01806626934511257 ) ) ;
#56073 = CARTESIAN_POINT ( 'NONE',  ( 275.5096892522198573, -21.88944388124440010, 2.223599993928938812 ) ) ;
#56074 = FACE_OUTER_BOUND ( 'NONE', #57963, .T. ) ;
#56075 = CARTESIAN_POINT ( 'NONE',  ( -166.2028657618940883, 79.74389853943290518, 14.38770061196751726 ) ) ;
#56076 = CARTESIAN_POINT ( 'NONE',  ( -80.55742067659896577, 23.05042616197511762, -49.88874770082764343 ) ) ;
#56077 = FACE_BOUND ( 'NONE', #43483, .T. ) ;
#56078 = DIRECTION ( 'NONE',  ( 0.000000000000000000, 1.000000000000000000, 0.000000000000000000 ) ) ;
#56079 = EDGE_CURVE ( 'NONE', #28546, #4522, #44642, .T. ) ;
#56080 = CARTESIAN_POINT ( 'NONE',  ( -0.8055628312658249524, 6.535476276302840226, 61.80831115705540668 ) ) ;
#56081 = ORIENTED_EDGE ( 'NONE', *, *, #9480, .T. ) ;
#56082 = ADVANCED_FACE ( 'NONE', ( #33404 ), #60471, .F. ) ;
#56083 = CARTESIAN_POINT ( 'NONE',  ( 277.7821011353898939, 21.53668059256674638, -4.493084242282730401 ) ) ;
#56084 = CARTESIAN_POINT ( 'NONE',  ( 151.8005253678162774, 54.62151558044534738, 58.81795113802257902 ) ) ;
#56085 = CARTESIAN_POINT ( 'NONE',  ( 444.9999999999999432, -35.00000000000000000, 0.000000000000000000 ) ) ;
#56086 = CARTESIAN_POINT ( 'NONE',  ( 5.799999999999999822, 4.618802153517001408, -8.000000000000000000 ) ) ;
#56087 = DIRECTION ( 'NONE',  ( -0.000000000000000000, -0.000000000000000000, -1.000000000000000000 ) ) ;
#56088 = ORIENTED_EDGE ( 'NONE', *, *, #30839, .F. ) ;
#56089 = CARTESIAN_POINT ( 'NONE',  ( 10.00000000000000178, 35.26862320190615208, -9.999999999999998224 ) ) ;
#56090 = PLANE ( 'NONE',  #46159 ) ;
#56091 = VERTEX_POINT ( 'NONE', #22836 ) ;
#56092 = ORIENTED_EDGE ( 'NONE', *, *, #25680, .T. ) ;
#56093 = LINE ( 'NONE', #19489, #45416 ) ;
#56094 = CARTESIAN_POINT ( 'NONE',  ( -173.1211646369891355, 87.12891641440857882, -61.55650775521367279 ) ) ;
#56095 = CARTESIAN_POINT ( 'NONE',  ( -55.15976438495157197, 34.41253982194030669, 170.0000000000000000 ) ) ;
#56096 = ORIENTED_EDGE ( 'NONE', *, *, #39086, .F. ) ;
#56097 = DIRECTION ( 'NONE',  ( 0.000000000000000000, 0.000000000000000000, 1.000000000000000000 ) ) ;
#56098 = AXIS2_PLACEMENT_3D ( 'NONE', #52540, #53560, #57826 ) ;
#56099 = DIRECTION ( 'NONE',  ( 1.000000000000000000, 1.387778780781445676E-16, -1.110223024625156294E-16 ) ) ;
#56100 = CARTESIAN_POINT ( 'NONE',  ( 42.02161712141799654, -16.09918303830818687, 30.00000000000000000 ) ) ;
#56101 = DIRECTION ( 'NONE',  ( 0.5508969814520944253, 0.8345732537213078617, 0.000000000000000000 ) ) ;
#56102 = AXIS2_PLACEMENT_3D ( 'NONE', #55380, #28664, #50117 ) ;
#56103 = CARTESIAN_POINT ( 'NONE',  ( 150.3320035166323976, 52.30731334295649049, 88.26711376708068713 ) ) ;
#56104 = CARTESIAN_POINT ( 'NONE',  ( 140.8984307802396359, 45.84194788389001474, 7.533282231769419468 ) ) ;
#56105 = ORIENTED_EDGE ( 'NONE', *, *, #32851, .T. ) ;
#56106 = FACE_OUTER_BOUND ( 'NONE', #576, .T. ) ;
#56107 = CARTESIAN_POINT ( 'NONE',  ( -71.17846906053298994, 20.67346400882179935, 10.57915229329010565 ) ) ;
#56108 = CARTESIAN_POINT ( 'NONE',  ( 45.49006904354232717, 9.279592366778887325, -47.50676418804506085 ) ) ;
#56109 = CARTESIAN_POINT ( 'NONE',  ( -168.7329347389696181, 83.83901812802758968, -75.15730867994311382 ) ) ;
#56111 = ORIENTED_EDGE ( 'NONE', *, *, #716, .F. ) ;
#56110 = CARTESIAN_POINT ( 'NONE',  ( -118.4102557275056142, 41.75991974097812687, 92.41143590757182835 ) ) ;
#56112 = CARTESIAN_POINT ( 'NONE',  ( 39.99999999999999289, 29.79383981485516486, 30.00000000000001066 ) ) ;
#56113 = EDGE_LOOP ( 'NONE', ( #2216, #51846, #69043, #19050 ) ) ;
#56114 = CARTESIAN_POINT ( 'NONE',  ( 0.000000000000000000, 242.0000000000000000, 0.000000000000000000 ) ) ;
#56115 = B_SPLINE_CURVE_WITH_KNOTS ( 'NONE', 3,
 ( #4428, #58915, #37458, #47323, #20594, #46644, #37123, #26572, #31850, #36793, #14974, #63865, #62835, #42057, #15674, #5111, #14637, #63516, #58565, #48010, #36101, #51922, #58234, #52942, #57554, #25893, #41719, #9713, #63178, #9361, #64198, #10381, #30826, #68119, #4767, #16007, #31507, #26230, #25212, #10729, #47667, #3733, #68779, #53283 ),
 .UNSPECIFIED., .F., .F.,
 ( 4, 2, 2, 2, 2, 2, 2, 2, 2, 2, 2, 2, 2, 2, 2, 2, 2, 2, 2, 2, 2, 4 ),
 ( 0.02477387709520258510, 0.02633314402883775787, 0.02711277749565534079, 0.02789241096247292370, 0.02945167789610812423, 0.03023131136292571408, 0.03101094482974330047, 0.03257021176337848711, 0.03334984523019606656, 0.03412947869701364600, 0.03568874563064879796, 0.03646837909746637740, 0.03724801256428394991, 0.03802764603110152242, 0.03880727949791910186, 0.04036654643155426075, 0.04192581336518942658, 0.04348508029882458548, 0.04504434723245974437, 0.04660361416609490326, 0.04816288109973006215, 0.04972214803336522798 ),
 .UNSPECIFIED. ) ;
#56116 = CARTESIAN_POINT ( 'NONE',  ( 79.37778929114108450, 18.12554302172301490, 39.19102792528236279 ) ) ;
#56117 = DIRECTION ( 'NONE',  ( -1.000000000000000000, -0.000000000000000000, -0.000000000000000000 ) ) ;
#56118 = DIRECTION ( 'NONE',  ( -1.000000000000000000, 0.000000000000000000, 0.000000000000000000 ) ) ;
#56119 = CYLINDRICAL_SURFACE ( 'NONE', #19711, 27.00000000000000000 ) ;
#56120 = CARTESIAN_POINT ( 'NONE',  ( -15.47041015649658213, 73.39774458108210808, 43.58025477438756212 ) ) ;
#56121 = CARTESIAN_POINT ( 'NONE',  ( -178.5848962563134421, 94.99295350784009884, -10.20532857645564917 ) ) ;
#56122 = CARTESIAN_POINT ( 'NONE',  ( -155.2912910578197057, 69.24479901948498650, -37.53156387900870783 ) ) ;
#56123 = ORIENTED_EDGE ( 'NONE', *, *, #56214, .T. ) ;
#56124 = ORIENTED_EDGE ( 'NONE', *, *, #54101, .T. ) ;
#56125 = CARTESIAN_POINT ( 'NONE',  ( 106.0171289417043994, 26.97542621030654075, 70.15651320696453297 ) ) ;
#56126 = CARTESIAN_POINT ( 'NONE',  ( 324.1677456657756125, 188.0000000000000000, -123.1183350412580779 ) ) ;
#56127 = VECTOR ( 'NONE', #64332, 1000.000000000000114 ) ;
#56128 = CARTESIAN_POINT ( 'NONE',  ( -30.60309003827877916, -68.41902945196855512, 41.38025477438755928 ) ) ;
#56129 = DIRECTION ( 'NONE',  ( -0.6910626489868685329, 0.7227948638273878901, 0.000000000000000000 ) ) ;
#56130 = CARTESIAN_POINT ( 'NONE',  ( 188.2950202724320832, 86.21411212788224532, -45.80789658381507223 ) ) ;
#56131 = CARTESIAN_POINT ( 'NONE',  ( -102.2801239173131052, 32.78103895658057354, 57.36362509687880618 ) ) ;
#56132 = DIRECTION ( 'NONE',  ( 0.000000000000000000, -0.000000000000000000, -1.000000000000000000 ) ) ;
#56133 = DIRECTION ( 'NONE',  ( 0.000000000000000000, 0.000000000000000000, 1.000000000000000000 ) ) ;
#56134 = VERTEX_POINT ( 'NONE', #38310 ) ;
#56135 = ORIENTED_EDGE ( 'NONE', *, *, #2875, .F. ) ;
#56136 = EDGE_CURVE ( 'NONE', #67695, #68560, #49547, .T. ) ;
#56137 = ORIENTED_EDGE ( 'NONE', *, *, #33436, .T. ) ;
#56138 = CARTESIAN_POINT ( 'NONE',  ( 86.62931800182293784, -170.0000000000000000, -70.16611478937539914 ) ) ;
#56139 = CARTESIAN_POINT ( 'NONE',  ( 2.699999999999990408, 0.000000000000000000, 0.000000000000000000 ) ) ;
#56140 = LINE ( 'NONE', #33659, #24027 ) ;
#56141 = CARTESIAN_POINT ( 'NONE',  ( 128.0882145863933488, 39.20607399008168414, 32.19109523275562168 ) ) ;
#56142 = CARTESIAN_POINT ( 'NONE',  ( 309.8720357909272707, 170.0000000000000284, 256.6193948016162381 ) ) ;
#56143 = CARTESIAN_POINT ( 'NONE',  ( 15.55634918610396511, -46.66904755831214402, 2.000000000000001776 ) ) ;
#56144 = EDGE_CURVE ( 'NONE', #2120, #48269, #61169, .T. ) ;
#56145 = CARTESIAN_POINT ( 'NONE',  ( -100.4347360276019288, 32.97716872911836816, -22.95435981532398984 ) ) ;
#56146 = CARTESIAN_POINT ( 'NONE',  ( 59.08202327466401726, 12.82375733818950536, 43.70333317471333601 ) ) ;
#56147 = CARTESIAN_POINT ( 'NONE',  ( 32.31938840494672149, 7.593698200002521936, 88.61355331186805984 ) ) ;
#56148 =( NAMED_UNIT ( * ) PLANE_ANGLE_UNIT ( ) SI_UNIT ( $, .RADIAN. ) );
#56149 = EDGE_LOOP ( 'NONE', ( #65647, #13365, #61084, #14228 ) ) ;
#56150 = CARTESIAN_POINT ( 'NONE',  ( -5.416136198635860488, 6.745992685878682948, -50.02480415146536785 ) ) ;
#56151 = CARTESIAN_POINT ( 'NONE',  ( 10.55634918610400419, -15.55634918610406103, 85.00100000000000477 ) ) ;
#56152 = DIRECTION ( 'NONE',  ( 1.000000000000000000, 0.000000000000000000, 0.000000000000000000 ) ) ;
#56153 = CARTESIAN_POINT ( 'NONE',  ( -149.0732005398557760, 63.81212100765654327, 18.86682848876648322 ) ) ;
#56154 = CARTESIAN_POINT ( 'NONE',  ( 284.4935831913008997, -21.89011901571377194, 2.216886222927867856 ) ) ;
#56155 = CARTESIAN_POINT ( 'NONE',  ( 197.1974290009104891, 96.59277840252781289, 63.22824731097590245 ) ) ;
#56156 = CARTESIAN_POINT ( 'NONE',  ( 126.4318266066172214, 38.27072266789467392, -17.77050837306448727 ) ) ;
#56157 = EDGE_CURVE ( 'NONE', #8745, #7128, #34456, .T. ) ;
#56158 = ORIENTED_EDGE ( 'NONE', *, *, #57029, .F. ) ;
#56159 = APPLICATION_PROTOCOL_DEFINITION ( 'draft international standard', 'automotive_design', 1998, #57460 ) ;
#56160 = CIRCLE ( 'NONE', #46063, 25.00000000000000711 ) ;
#56161 = CARTESIAN_POINT ( 'NONE',  ( 130.3035708464390154, 40.48418876551453849, -36.90095733877659967 ) ) ;
#56162 = CARTESIAN_POINT ( 'NONE',  ( -37.07436112751821611, 11.60822760208522553, -37.84398108377252612 ) ) ;
#56163 = CARTESIAN_POINT ( 'NONE',  ( 188.9999999999999432, 190.0000000000000000, -2.000000000000000888 ) ) ;
#56164 = ITEM_DEFINED_TRANSFORMATION ( 'NONE', 'NONE', #42247,  #66832 ) ;
#56165 = LINE ( 'NONE', #17845, #55757 ) ;
#56166 = EDGE_LOOP ( 'NONE', ( #27281, #9239 ) ) ;
#56167 = CARTESIAN_POINT ( 'NONE',  ( 130.3281282802763315, 40.49854652972190650, 3.530804043226662969 ) ) ;
#56168 = DIRECTION ( 'NONE',  ( -0.000000000000000000, 1.000000000000000000, -0.000000000000000000 ) ) ;
#56169 = CARTESIAN_POINT ( 'NONE',  ( 202.7540649946182612, 105.3989460363904556, 2.608031559926723197 ) ) ;
#56170 = B_SPLINE_CURVE_WITH_KNOTS ( 'NONE', 3,
 ( #7452, #58543, #5089, #60555, #66211, #44015, #38761, #27494, #31828, #48932, #22926, #34189, #50358, #774, #6742, #28551, #55273, #43664, #18000, #39448, #59842, #2174, #60900, #12721, #23629, #65492, #45065, #1828, #22573, #22227, #66551, #28189, #16937, #65852, #49997, #17651, #60203, #12024, #49639, #53260, #54570, #23287, #6397, #65143 ),
 .UNSPECIFIED., .F., .F.,
 ( 4, 2, 2, 2, 2, 2, 2, 2, 2, 2, 2, 2, 2, 2, 2, 2, 2, 2, 2, 2, 2, 4 ),
 ( 1.387778780781445676E-17, 0.003518733725596352984, 0.004398417156995421823, 0.005278100588394489361, 0.007037467451192665202, 0.007917150882591726668, 0.008796834313990788135, 0.01055620117678895444, 0.01231556803958712074, 0.01319525147098622384, 0.01407493490238532520, 0.01495461833378442830, 0.01583430176518352966, 0.01671398519658263276, 0.01759366862798173933, 0.01935303549077990737, 0.02111240235357807887, 0.02199208578497713687, 0.02287176921637619487, 0.02463113607917434902, 0.02639050294197250318, 0.02814986980477065734 ),
 .UNSPECIFIED. ) ;
#56171 = CARTESIAN_POINT ( 'NONE',  ( 149.9779033028198683, 53.29256572657026680, 90.09284245516512613 ) ) ;
#56172 = ORIENTED_EDGE ( 'NONE', *, *, #47087, .F. ) ;
#56173 = CARTESIAN_POINT ( 'NONE',  ( -57.65574514524056582, 16.43983577669857254, 3.934844714199217997 ) ) ;
#56174 = CARTESIAN_POINT ( 'NONE',  ( 203.1511228994173166, 104.2426341584998823, -51.21072795959794632 ) ) ;
#56175 = CARTESIAN_POINT ( 'NONE',  ( 0.000000000000000000, -7.806255641895631925E-15, -15.99999999999998579 ) ) ;
#56176 = VECTOR ( 'NONE', #55705, 1000.000000000000000 ) ;
#56177 = CARTESIAN_POINT ( 'NONE',  ( 21.44031696305385282, 6.747195267824409370, -38.06475470450458687 ) ) ;
#56178 = CARTESIAN_POINT ( 'NONE',  ( 86.14852828165528820, 19.25704475759651402, 17.86753698201565754 ) ) ;
#56180 = ORIENTED_EDGE ( 'NONE', *, *, #36509, .F. ) ;
#56179 = DIRECTION ( 'NONE',  ( -1.000000000000000000, -0.000000000000000000, -0.000000000000000000 ) ) ;
#56181 = DIRECTION ( 'NONE',  ( -1.000000000000000000, -0.000000000000000000, -0.000000000000000000 ) ) ;
#56182 = VERTEX_POINT ( 'NONE', #2428 ) ;
#56183 = ORIENTED_EDGE ( 'NONE', *, *, #14775, .F. ) ;
#56184 = CARTESIAN_POINT ( 'NONE',  ( -169.1116812882276008, 84.24296059722695418, 17.83128106548857872 ) ) ;
#56185 = CARTESIAN_POINT ( 'NONE',  ( 22.80839748737787787, 6.826915557457463812, -72.51456902026779971 ) ) ;
#56187 = ORIENTED_EDGE ( 'NONE', *, *, #26141, .F. ) ;
#56186 = CARTESIAN_POINT ( 'NONE',  ( -11.57950265606958062, 8.174070387114797498, -63.26516250596657187 ) ) ;
#56188 = CARTESIAN_POINT ( 'NONE',  ( -95.04384172745170645, 30.36531739257813101, 93.78841958355275210 ) ) ;
#56189 = CARTESIAN_POINT ( 'NONE',  ( -24.71604178686819253, 9.599501655372943532, 34.38300249122266905 ) ) ;
#56190 = AXIS2_PLACEMENT_3D ( 'NONE', #35072, #68468, #67440 ) ;
#56191 = CARTESIAN_POINT ( 'NONE',  ( -73.80418150970714919, 21.59712875466422943, -48.34729916886697509 ) ) ;
#56192 = EDGE_LOOP ( 'NONE', ( #39638, #53849, #53339, #39230 ) ) ;
#56193 = EDGE_CURVE ( 'NONE', #69067, #2052, #16851, .T. ) ;
#56194 = CARTESIAN_POINT ( 'NONE',  ( 212.1734186221015932, 119.0499290057855291, -69.97830959964204567 ) ) ;
#56195 = EDGE_CURVE ( 'NONE', #29969, #63871, #43923, .T. ) ;
#56196 = CARTESIAN_POINT ( 'NONE',  ( 141.3036441389950539, 47.31002705502927341, 35.97038062019882432 ) ) ;
#56197 = CARTESIAN_POINT ( 'NONE',  ( 544.6745185807129701, 188.0000000000000000, 34.73878747406611467 ) ) ;
#56198 = FACE_OUTER_BOUND ( 'NONE', #31334, .T. ) ;
#56199 = CARTESIAN_POINT ( 'NONE',  ( 70.26936813788618963, 15.51386666370915357, -72.03546886692284090 ) ) ;
#56200 = ORIENTED_EDGE ( 'NONE', *, *, #28250, .F. ) ;
#56201 = VERTEX_POINT ( 'NONE', #17194 ) ;
#56202 = VERTEX_POINT ( 'NONE', #11932 ) ;
#56203 = VECTOR ( 'NONE', #52581, 1000.000000000000000 ) ;
#56204 = LINE ( 'NONE', #34427, #57572 ) ;
#56205 = CARTESIAN_POINT ( 'NONE',  ( 0.000000000000000000, 0.000000000000000000, -4.999999999999997335 ) ) ;
#56206 = CARTESIAN_POINT ( 'NONE',  ( 429.8372781065086201, 388.0000000000109708, 96.05029585798438063 ) ) ;
#56207 = DIRECTION ( 'NONE',  ( 0.000000000000000000, 0.000000000000000000, -1.000000000000000000 ) ) ;
#56208 = PLANE ( 'NONE',  #10081 ) ;
#56209 = EDGE_CURVE ( 'NONE', #56892, #66979, #14318, .T. ) ;
#56210 = CARTESIAN_POINT ( 'NONE',  ( 22.93737758745385946, -9.943676855698914352, 0.000000000000000000 ) ) ;
#56211 = DIRECTION ( 'NONE',  ( -0.000000000000000000, 1.000000000000000000, -0.000000000000000000 ) ) ;
#56212 = VERTEX_POINT ( 'NONE', #46662 ) ;
#56213 = CARTESIAN_POINT ( 'NONE',  ( -109.7811201291769549, 37.90784085457602970, 38.24940268311721780 ) ) ;
#56214 = EDGE_CURVE ( 'NONE', #59078, #25903, #13963, .T. ) ;
#56215 = ORIENTED_EDGE ( 'NONE', *, *, #67271, .T. ) ;
#56216 = CARTESIAN_POINT ( 'NONE',  ( 37.47081272996201307, 8.166145978397521432, 44.66509977773299767 ) ) ;
#56217 = DIRECTION ( 'NONE',  ( 0.000000000000000000, 1.000000000000000000, 0.000000000000000000 ) ) ;
#56218 = ORIENTED_EDGE ( 'NONE', *, *, #49262, .T. ) ;
#56219 = DIRECTION ( 'NONE',  ( 1.000000000000000000, 0.000000000000000000, 0.000000000000000000 ) ) ;
#56220 = CARTESIAN_POINT ( 'NONE',  ( 50.97490815085634352, 0.000000000000000000, -14.43565316649549679 ) ) ;
#56221 =( NAMED_UNIT ( * ) SI_UNIT ( $, .STERADIAN. ) SOLID_ANGLE_UNIT ( ) );
#56222 = FACE_OUTER_BOUND ( 'NONE', #18722, .T. ) ;
#56223 = CARTESIAN_POINT ( 'NONE',  ( -49.43915770973591606, 13.24768844696975378, 15.97056682900100810 ) ) ;
#56224 = EDGE_CURVE ( 'NONE', #10473, #49852, #35075, .T. ) ;
#56225 = VECTOR ( 'NONE', #10114, 1000.000000000000000 ) ;
#56226 = CARTESIAN_POINT ( 'NONE',  ( 154.0293889979056416, 55.02370422818216866, -50.30463981601170786 ) ) ;
#56227 = VERTEX_POINT ( 'NONE', #51265 ) ;
#56228 = LINE ( 'NONE', #12282, #6130 ) ;
#56229 = CARTESIAN_POINT ( 'NONE',  ( -154.0775378574014098, 68.15437918458557931, -9.502335120361516729 ) ) ;
#56230 = EDGE_LOOP ( 'NONE', ( #64161, #1679 ) ) ;
#56231 = CARTESIAN_POINT ( 'NONE',  ( -58.32860549785896609, 15.58423118879329294, 31.06615926810922801 ) ) ;
#56232 = CARTESIAN_POINT ( 'NONE',  ( -57.42826130032238297, 16.37596353166457419, 57.54390146367184400 ) ) ;
#56233 = DIRECTION ( 'NONE',  ( -0.000000000000000000, 1.000000000000000000, -0.000000000000000000 ) ) ;
#56234 = VERTEX_POINT ( 'NONE', #18901 ) ;
#56235 = CARTESIAN_POINT ( 'NONE',  ( -59.09450113343203270, -27.07101652673575032, 170.0000000000000000 ) ) ;
#56236 = DIRECTION ( 'NONE',  ( 0.000000000000000000, 0.000000000000000000, -1.000000000000000000 ) ) ;
#56237 = CARTESIAN_POINT ( 'NONE',  ( -96.78198318406111866, 30.07417864442862054, -20.79432951231798299 ) ) ;
#56238 = CARTESIAN_POINT ( 'NONE',  ( 138.5721691894142680, 44.34516164557648210, -49.37593785591674589 ) ) ;
#56239 = ADVANCED_FACE ( 'NONE', ( #45634 ), #39840, .T. ) ;
#56240 = VERTEX_POINT ( 'NONE', #9042 ) ;
#56241 = CARTESIAN_POINT ( 'NONE',  ( -452.6627218934913799, 0.000000000000000000, -111.4497041420118251 ) ) ;
#56242 = EDGE_CURVE ( 'NONE', #6148, #21697, #51942, .T. ) ;
#56243 = EDGE_CURVE ( 'NONE', #36104, #20970, #68138, .T. ) ;
#56244 = EDGE_CURVE ( 'NONE', #29654, #37239, #15141, .T. ) ;
#56245 = CARTESIAN_POINT ( 'NONE',  ( -125.8938041572051105, 46.49392987655495091, 45.61994787315711619 ) ) ;
#56246 = ORIENTED_EDGE ( 'NONE', *, *, #14382, .T. ) ;
#56247 = DIRECTION ( 'NONE',  ( -0.3754023374827052950, 0.9268613172740186590, -0.001087912492708085609 ) ) ;
#56248 = CARTESIAN_POINT ( 'NONE',  ( 188.2133404574783242, 86.12414067617878288, 12.31026140296448013 ) ) ;
#56249 = CARTESIAN_POINT ( 'NONE',  ( 87.10668362745094839, 19.58396519288863402, 56.55663816294299551 ) ) ;
#56250 = CARTESIAN_POINT ( 'NONE',  ( 0.000000000000000000, 0.000000000000000000, 41.38025477438755928 ) ) ;
#56251 = LINE ( 'NONE', #45352, #2498 ) ;
#56252 = DIRECTION ( 'NONE',  ( -0.000000000000000000, -0.000000000000000000, 1.000000000000000000 ) ) ;
#56253 = ORIENTED_EDGE ( 'NONE', *, *, #30434, .F. ) ;
#56254 = CARTESIAN_POINT ( 'NONE',  ( 157.4703587214989113, 57.65129005721576050, -9.279633708673953763 ) ) ;
#56255 = DIRECTION ( 'NONE',  ( -1.000000000000000000, 0.000000000000000000, 0.000000000000000000 ) ) ;
#56256 = CARTESIAN_POINT ( 'NONE',  ( 63.50528314073028469, 12.78634332146813435, 71.65751152968502424 ) ) ;
#56257 = CARTESIAN_POINT ( 'NONE',  ( 41.66904755831210849, -9.150666335777657423E-14, 2.000000000000001776 ) ) ;
#56258 = FACE_OUTER_BOUND ( 'NONE', #67126, .T. ) ;
#56259 = VECTOR ( 'NONE', #17021, 1000.000000000000000 ) ;
#56260 = VECTOR ( 'NONE', #47840, 1000.000000000000000 ) ;
#56261 = ORIENTED_EDGE ( 'NONE', *, *, #60699, .T. ) ;
#56262 = DIRECTION ( 'NONE',  ( -0.000000000000000000, -0.000000000000000000, -1.000000000000000000 ) ) ;
#56263 = AXIS2_PLACEMENT_3D ( 'NONE', #43016, #54257, #22979 ) ;
#56264 = CARTESIAN_POINT ( 'NONE',  ( 9.288975942802419894, 6.379608420846960115, 41.26562237599018346 ) ) ;
#56265 = VERTEX_POINT ( 'NONE', #29801 ) ;
#56266 = CARTESIAN_POINT ( 'NONE',  ( 69.83617901654358207, 15.39919709983075968, 61.02833969872266096 ) ) ;
#56267 = CARTESIAN_POINT ( 'NONE',  ( 127.3115382175395780, 37.60999379334474213, 94.42761284291371737 ) ) ;
#56268 = VERTEX_POINT ( 'NONE', #24873 ) ;
#56269 = CARTESIAN_POINT ( 'NONE',  ( 164.8433205901839642, 64.93586312665803462, -42.22151823635311274 ) ) ;
#56270 = DIRECTION ( 'NONE',  ( -0.000000000000000000, -0.000000000000000000, -1.000000000000000000 ) ) ;
#56271 = AXIS2_PLACEMENT_3D ( 'NONE', #9922, #51793, #68987 ) ;
#56272 = DIRECTION ( 'NONE',  ( 0.000000000000000000, 0.000000000000000000, -1.000000000000000000 ) ) ;
#56273 = DIRECTION ( 'NONE',  ( -0.3930250316539148359, -0.9195277725514544587, 0.000000000000000000 ) ) ;
#56274 = ORIENTED_EDGE ( 'NONE', *, *, #57470, .F. ) ;
#56275 = EDGE_CURVE ( 'NONE', #43209, #11718, #62853, .T. ) ;
#56276 = CARTESIAN_POINT ( 'NONE',  ( -99.99439884168255332, 32.75762661251356889, 18.33352629368685527 ) ) ;
#56277 = CARTESIAN_POINT ( 'NONE',  ( 59.84433950768821830, 12.98867007234732540, 84.17292290978423352 ) ) ;
#56278 = EDGE_CURVE ( 'NONE', #7321, #38915, #12895, .T. ) ;
#56279 = FACE_OUTER_BOUND ( 'NONE', #4953, .T. ) ;
#56280 = PLANE ( 'NONE',  #36464 ) ;
#56281 = CARTESIAN_POINT ( 'NONE',  ( -167.6413528428655866, 81.22881971256911982, 33.17534743252404894 ) ) ;
#56282 = DIRECTION ( 'NONE',  ( 0.3978782902816504485, 0.9174375763581197329, -0.001076851285082543923 ) ) ;
#56283 = CARTESIAN_POINT ( 'NONE',  ( 126.6576865394845868, 37.24426596493988484, -68.24804092954708779 ) ) ;
#56284 = B_SPLINE_CURVE_WITH_KNOTS ( 'NONE', 3,
 ( #2410, #50246, #45665, #67143, #45307, #3107, #1711, #55514, #24569, #13647, #17891, #44962, #55159, #39005, #65739, #60449, #18932, #12970, #40381, #35102, #56557, #23521, #7342, #2067, #66447, #18234, #39689, #61147, #34435, #7691, #42111, #31225, #9417, #41427, #62178, #51972, #68170, #25939, #15035, #35454, #3445, #51637, #62881, #14351, #9763, #52656, #30875, #46339 ),
 .UNSPECIFIED., .F., .F.,
 ( 4, 2, 2, 2, 2, 2, 2, 2, 2, 2, 2, 2, 2, 2, 2, 2, 2, 2, 2, 2, 2, 2, 2, 4 ),
 ( 0.02746511744866864460, 0.02914922134997103079, 0.03083332525127341350, 0.03251742915257578581, 0.03335948110322694421, 0.03420153305387810261, 0.03504358500452926101, 0.03588563695518041247, 0.03756974085648268069, 0.03841179280713380439, 0.03925384475778492810, 0.04009589670843605180, 0.04093794865908717551, 0.04262205256038943679, 0.04430615646169169808, 0.04514820841234285648, 0.04599026036299401488, 0.04767436426429631779, 0.04935846816559862071, 0.05020052011624975830, 0.05104257206690090282, 0.05272667596820317104, 0.05356872791885429475, 0.05441077986950541845 ),
 .UNSPECIFIED. ) ;
#56285 = VERTEX_POINT ( 'NONE', #8701 ) ;
#56286 = CARTESIAN_POINT ( 'NONE',  ( -99.99439884168261017, 32.75762661251357599, 72.02262747461425363 ) ) ;
#56287 = CARTESIAN_POINT ( 'NONE',  ( -11.14668121284975832, 8.139398342256729535, 71.18912459828850103 ) ) ;
#56288 = VERTEX_POINT ( 'NONE', #3075 ) ;
#56289 = CARTESIAN_POINT ( 'NONE',  ( -153.6994314938755792, 69.16570456337669270, -36.07705819171143702 ) ) ;
#56290 = CYLINDRICAL_SURFACE ( 'NONE', #26422, 7.500000000000020428 ) ;
#56291 = CARTESIAN_POINT ( 'NONE',  ( -5.412684891282530053, 7.753215344827980360, 30.49725765081104001 ) ) ;
#56292 = DIRECTION ( 'NONE',  ( -1.000000000000000000, -1.850550996349095901E-16, -1.228197773518735191E-20 ) ) ;
#56293 = DIRECTION ( 'NONE',  ( 2.312964634635743450E-16, -0.000000000000000000, 1.000000000000000000 ) ) ;
#56294 = EDGE_CURVE ( 'NONE', #67008, #20980, #7994, .T. ) ;
#56295 = CARTESIAN_POINT ( 'NONE',  ( 10.55634918610409656, 31.11269837220803325, 85.00100000000000477 ) ) ;
#56296 = EDGE_CURVE ( 'NONE', #30795, #38817, #2723, .T. ) ;
#56297 = CARTESIAN_POINT ( 'NONE',  ( 173.8575673535406452, 71.59843387604338716, 7.936245129884297533 ) ) ;
#56299 = EDGE_CURVE ( 'NONE', #22995, #42825, #24539, .T. ) ;
#56298 = CARTESIAN_POINT ( 'NONE',  ( -62.53989795537025032, 16.81768094534200841, 11.47802686014114038 ) ) ;
#56300 = EDGE_LOOP ( 'NONE', ( #61490, #63185, #53286, #53851 ) ) ;
#56301 = LINE ( 'NONE', #51033, #18353 ) ;
#56302 = ORIENTED_EDGE ( 'NONE', *, *, #21499, .F. ) ;
#56303 = CARTESIAN_POINT ( 'NONE',  ( 103.1653143050726129, 25.74301230421574616, -67.73440299836630629 ) ) ;
#56304 = EDGE_CURVE ( 'NONE', #19283, #66816, #29752, .T. ) ;
#56305 = CARTESIAN_POINT ( 'NONE',  ( 45.89268866913130296, 10.36133864615985800, -12.50948627268672375 ) ) ;
#56306 = CARTESIAN_POINT ( 'NONE',  ( 61.62594073580542897, 21.79346734965000820, 43.58025477438756212 ) ) ;
#56307 = DIRECTION ( 'NONE',  ( -1.000000000000000000, 0.000000000000000000, 0.000000000000000000 ) ) ;
#56308 = CARTESIAN_POINT ( 'NONE',  ( 54.16778967912048159, -21.66464655980577803, 27.58472315868180402 ) ) ;
#56309 = CIRCLE ( 'NONE', #64176, 65.00000000000000000 ) ;
#56310 = CARTESIAN_POINT ( 'NONE',  ( 2.999999999999995559, 0.000000000000000000, 0.000000000000000000 ) ) ;
#56311 = CIRCLE ( 'NONE', #12528, 65.00000000000000000 ) ;
#56312 = DIRECTION ( 'NONE',  ( -1.000000000000000000, 0.000000000000000000, 0.000000000000000000 ) ) ;
#56313 = CARTESIAN_POINT ( 'NONE',  ( -166.7049310409072405, 80.25944422923579680, 69.05890086907660930 ) ) ;
#56314 = ORIENTED_EDGE ( 'NONE', *, *, #276, .T. ) ;
#56315 = ORIENTED_EDGE ( 'NONE', *, *, #59864, .F. ) ;
#56316 = FACE_BOUND ( 'NONE', #13063, .T. ) ;
#56317 = DIRECTION ( 'NONE',  ( -1.000000000000000000, 0.000000000000000000, 0.000000000000000000 ) ) ;
#56319 = CARTESIAN_POINT ( 'NONE',  ( 42.62674880747476180, 8.849563476334237677, -89.98647070695761840 ) ) ;
#56318 = VECTOR ( 'NONE', #19343, 1000.000000000000000 ) ;
#56320 = VECTOR ( 'NONE', #6398, 1000.000000000000000 ) ;
#56321 = DIRECTION ( 'NONE',  ( 0.000000000000000000, 0.000000000000000000, 1.000000000000000000 ) ) ;
#56322 = LINE ( 'NONE', #51407, #66722 ) ;
#56323 = CONICAL_SURFACE ( 'NONE', #65315, 74.95140232871122521, 0.8777644062502172329 ) ;
#56324 = CARTESIAN_POINT ( 'NONE',  ( 59.73312635112158375, 12.96464920523511388, -23.13701263744227532 ) ) ;
#56325 = ORIENTED_EDGE ( 'NONE', *, *, #35751, .F. ) ;
#56326 = EDGE_CURVE ( 'NONE', #17465, #11802, #9520, .T. ) ;
#56327 = EDGE_CURVE ( 'NONE', #62331, #24824, #40687, .T. ) ;
#56328 = CARTESIAN_POINT ( 'NONE',  ( 45.80999061969644970, 9.329701754959341287, 94.99999999999866418 ) ) ;
#56329 = FACE_OUTER_BOUND ( 'NONE', #1566, .T. ) ;
#56330 = CARTESIAN_POINT ( 'NONE',  ( -79.14127775978548129, 22.50259208414360756, -23.27090004125422595 ) ) ;
#56331 = CARTESIAN_POINT ( 'NONE',  ( 0.000000000000000000, 0.000000000000000000, 26.24939009510892518 ) ) ;
#56332 = DIRECTION ( 'NONE',  ( 0.000000000000000000, 0.000000000000000000, 1.000000000000000000 ) ) ;
#56333 = EDGE_CURVE ( 'NONE', #4891, #53557, #57573, .T. ) ;
#56334 = ORIENTED_EDGE ( 'NONE', *, *, #22947, .T. ) ;
#56335 = ORIENTED_EDGE ( 'NONE', *, *, #67051, .F. ) ;
#56336 = DIRECTION ( 'NONE',  ( -0.000000000000000000, -0.000000000000000000, 1.000000000000000000 ) ) ;
#56337 = CARTESIAN_POINT ( 'NONE',  ( 100.0000000000000284, -5.000000000000000000, 18.50000000000000000 ) ) ;
#56338 = CARTESIAN_POINT ( 'NONE',  ( 42.02161712141799654, -16.09918303830818687, 0.000000000000000000 ) ) ;
#56339 = DIRECTION ( 'NONE',  ( -0.000000000000000000, -0.000000000000000000, -1.000000000000000000 ) ) ;
#56340 = CARTESIAN_POINT ( 'NONE',  ( 63.49940197359693883, 12.78497925206076147, 29.81296093922127000 ) ) ;
#56341 = CARTESIAN_POINT ( 'NONE',  ( 79.14129363775931836, 17.00055658855363205, -70.65915694733433838 ) ) ;
#56342 = EDGE_LOOP ( 'NONE', ( #28507, #32327, #33271, #21059 ) ) ;
#56343 = DIRECTION ( 'NONE',  ( 0.000000000000000000, 0.000000000000000000, -1.000000000000000000 ) ) ;
#56344 = CARTESIAN_POINT ( 'NONE',  ( 197.3756653044963514, 98.41886189307118116, -45.45805580265201939 ) ) ;
#56345 = ORIENTED_EDGE ( 'NONE', *, *, #36079, .F. ) ;
#56346 = CARTESIAN_POINT ( 'NONE',  ( 450.2085304802404266, 2.000000000000000000, -247.8920266495912870 ) ) ;
#56347 = VERTEX_POINT ( 'NONE', #3413 ) ;
#56348 = CARTESIAN_POINT ( 'NONE',  ( -81.90020664963803654, 23.57971581008656869, -76.23134889676580883 ) ) ;
#56349 = CARTESIAN_POINT ( 'NONE',  ( -62.29496909743951960, 17.79481128341706508, -13.90640243752122807 ) ) ;
#56350 = CARTESIAN_POINT ( 'NONE',  ( 88.53025347111696419, 21.14438024052372356, -77.43697678579287924 ) ) ;
#56351 = ORIENTED_EDGE ( 'NONE', *, *, #21971, .F. ) ;
#56352 = AXIS2_PLACEMENT_3D ( 'NONE', #18712, #1484, #56688 ) ;
#56353 = VERTEX_POINT ( 'NONE', #30843 ) ;
#56354 = CARTESIAN_POINT ( 'NONE',  ( 14.08699529666006178, 6.452200550165256843, -35.71036563474962833 ) ) ;
#56355 = CARTESIAN_POINT ( 'NONE',  ( -103.3308778225766815, 34.44988434361755480, -88.77464374387059820 ) ) ;
#56356 = CARTESIAN_POINT ( 'NONE',  ( 22.81270948571149404, 6.827178363529886163, 13.30984265512818077 ) ) ;
#56357 = VECTOR ( 'NONE', #69489, 999.9999999999998863 ) ;
#56358 = ORIENTED_EDGE ( 'NONE', *, *, #41309, .T. ) ;
#56359 = PRODUCT ( 'back cover', 'back cover', '', ( #9023 ) ) ;
#56360 = CARTESIAN_POINT ( 'NONE',  ( 0.000000000000000000, 0.000000000000000000, 0.000000000000000000 ) ) ;
#56361 = EDGE_CURVE ( 'NONE', #47170, #27210, #20276, .T. ) ;
#56362 = DIRECTION ( 'NONE',  ( -1.000000000000000000, 0.000000000000000000, 0.000000000000000000 ) ) ;
#56363 = CARTESIAN_POINT ( 'NONE',  ( -130.1938957973835329, 50.61368074696266461, -21.73168917496282404 ) ) ;
#56364 = CARTESIAN_POINT ( 'NONE',  ( 117.7447573007802788, 32.50990724960316669, -16.08767966913922010 ) ) ;
#56365 = CARTESIAN_POINT ( 'NONE',  ( 80.73462811483980772, 18.54763808182591589, -47.98554289559778141 ) ) ;
#56367 = ORIENTED_EDGE ( 'NONE', *, *, #53745, .T. ) ;
#56366 = CARTESIAN_POINT ( 'NONE',  ( -173.1211646369891355, 87.12891641440857882, -76.55650775521370122 ) ) ;
#56368 = ORIENTED_EDGE ( 'NONE', *, *, #61156, .F. ) ;
#56369 = AXIS2_PLACEMENT_3D ( 'NONE', #9818, #16113, #30580 ) ;
#56370 = ORIENTED_EDGE ( 'NONE', *, *, #10728, .F. ) ;
#56371 = CARTESIAN_POINT ( 'NONE',  ( 46.85206196242844356, 9.495795933269485900, 9.575707866823087500 ) ) ;
#56372 = CARTESIAN_POINT ( 'NONE',  ( -15.45727656667583005, -73.34020256436187424, 41.38025477438755928 ) ) ;
#56373 = CARTESIAN_POINT ( 'NONE',  ( -50.52927270563905182, 13.51486287463704627, -21.87426322953785629 ) ) ;
#56374 = DIRECTION ( 'NONE',  ( 1.000000000000000000, 0.000000000000000000, -0.000000000000000000 ) ) ;
#56375 = CARTESIAN_POINT ( 'NONE',  ( 197.1980152960109365, 96.59350208824301376, 10.20049193452572744 ) ) ;
#56376 = CARTESIAN_POINT ( 'NONE',  ( -26.37870220071948069, 8.815136099259133218, -90.95400284204914954 ) ) ;
#56377 = EDGE_CURVE ( 'NONE', #23906, #39203, #55554, .T. ) ;
#56378 = CARTESIAN_POINT ( 'NONE',  ( 211.5400400709320650, 118.0665875834716019, 93.47395779939256499 ) ) ;
#56379 = CARTESIAN_POINT ( 'NONE',  ( 207.8398359204632868, 112.5208221429021194, 29.89445929276630665 ) ) ;
#56380 = CARTESIAN_POINT ( 'NONE',  ( -79.61235761536670452, 23.76245710489568452, 57.30737474656424979 ) ) ;
#56381 = CARTESIAN_POINT ( 'NONE',  ( -9.771516655894554759, 7.025139475821124968, 30.35594508498904531 ) ) ;
#56382 = ORIENTED_EDGE ( 'NONE', *, *, #36756, .F. ) ;
#56383 = CARTESIAN_POINT ( 'NONE',  ( 10.82760985890677752, 7.398654328676805392, -10.52802355588776351 ) ) ;
#56384 = EDGE_LOOP ( 'NONE', ( #25215, #9344, #5134, #42100 ) ) ;
#56385 = EDGE_CURVE ( 'NONE', #37545, #65974, #48792, .T. ) ;
#56387 = ORIENTED_EDGE ( 'NONE', *, *, #2306, .T. ) ;
#56386 = B_SPLINE_CURVE_WITH_KNOTS ( 'NONE', 3,
 ( #30958, #19351, #62262, #9152, #30607, #4221, #58357, #52060, #46778, #52403, #9843, #68581, #35541, #24992, #46424, #41164, #40807, #68909, #31304, #67902, #20382, #14081, #4556, #56995, #20053, #52731, #19700, #14433, #30266, #53068, #51715, #35884, #41506, #3873, #62958, #41850, #63310, #25342, #68248, #47449 ),
 .UNSPECIFIED., .F., .F.,
 ( 4, 2, 2, 2, 2, 2, 2, 2, 2, 2, 2, 2, 2, 2, 2, 2, 2, 2, 2, 4 ),
 ( 0.02472759712254455483, 0.02626001169882808198, 0.02779242627511161259, 0.02932484085139513974, 0.03009104813953689117, 0.03085725542767863566, 0.03238967000396208301, 0.03315587729210382750, 0.03392208458024557199, 0.03545449915652904710, 0.03698691373281252220, 0.03851932830909599731, 0.04005174288537947241, 0.04158415746166294058, 0.04311657203794641569, 0.04464898661422989079, 0.04541519390237163528, 0.04618140119051337977, 0.04771381576679688263, 0.04924623034308039937 ),
 .UNSPECIFIED. ) ;
#56388 = ADVANCED_FACE ( 'NONE', ( #15691 ), #14996, .F. ) ;
#56389 = CARTESIAN_POINT ( 'NONE',  ( -142.8492950481059438, 60.01492924994605715, 7.913576728738202171 ) ) ;
#56390 = CARTESIAN_POINT ( 'NONE',  ( 185.5457097283155008, 84.70846743303874860, -64.52296994192434454 ) ) ;
#56391 = CARTESIAN_POINT ( 'NONE',  ( -168.7314919967217577, 83.83749564070829763, 44.42116658107412519 ) ) ;
#56392 = DIRECTION ( 'NONE',  ( -0.000000000000000000, 1.000000000000000000, -0.000000000000000000 ) ) ;
#56393 = EDGE_CURVE ( 'NONE', #67708, #26725, #10067, .T. ) ;
#56394 = CARTESIAN_POINT ( 'NONE',  ( -23.98747857548121232, 9.501432345103351551, 11.85715207713718122 ) ) ;
#56395 = FACE_OUTER_BOUND ( 'NONE', #28031, .T. ) ;
#56396 = DIRECTION ( 'NONE',  ( -1.000000000000000000, 0.000000000000000000, 0.000000000000000000 ) ) ;
#56397 = CARTESIAN_POINT ( 'NONE',  ( 127.1040286383415605, 37.49395136275128948, -46.79722293648432441 ) ) ;
#56398 = EDGE_LOOP ( 'NONE', ( #46052, #21804, #35446, #11471 ) ) ;
#56399 = ORIENTED_EDGE ( 'NONE', *, *, #65193, .T. ) ;
#56400 = CARTESIAN_POINT ( 'NONE',  ( 46.66904755831210139, -9.150666335777657423E-14, 85.00100000000000477 ) ) ;
#56401 = DIRECTION ( 'NONE',  ( -1.850169831522831466E-16, 1.000000000000000000, 1.110223024625156294E-16 ) ) ;
#56402 = DIRECTION ( 'NONE',  ( -0.000000000000000000, -0.000000000000000000, -1.000000000000000000 ) ) ;
#56403 = CARTESIAN_POINT ( 'NONE',  ( -28.35330809568272059, 9.105138953156460602, -62.82163295736274478 ) ) ;
#56404 = UNCERTAINTY_MEASURE_WITH_UNIT (LENGTH_MEASURE( 1.000000000000000082E-05 ), #66641, 'distance_accuracy_value', 'NONE');
#56405 = CIRCLE ( 'NONE', #14817, 10.00000000000000178 ) ;
#56406 = CARTESIAN_POINT ( 'NONE',  ( 8.288451200428832877, 6.376395059685423305, 11.16205334907189162 ) ) ;
#56407 = VERTEX_POINT ( 'NONE', #57913 ) ;
#56408 = CARTESIAN_POINT ( 'NONE',  ( 283.7642062731435431, 21.75126402171896345, -3.307110067226755490 ) ) ;
#56409 = CARTESIAN_POINT ( 'NONE',  ( -57.65574514524056582, 16.43983577669855833, -76.59880705719182004 ) ) ;
#56410 = CARTESIAN_POINT ( 'NONE',  ( 200.8383807319520713, 102.8517715783672912, -77.11560942651001938 ) ) ;
#56411 = CARTESIAN_POINT ( 'NONE',  ( 276.0271074675582099, -21.78879721737672881, -3.053546265906994517 ) ) ;
#56412 = DIRECTION ( 'NONE',  ( 0.000000000000000000, -1.000000000000000000, 0.000000000000000000 ) ) ;
#56413 = CARTESIAN_POINT ( 'NONE',  ( -24.03640295269301674, 9.507963273819775907, 63.33170168683827228 ) ) ;
#56414 = FACE_OUTER_BOUND ( 'NONE', #38051, .T. ) ;
#56415 = ADVANCED_FACE ( 'NONE', ( #58251 ), #16380, .F. ) ;
#56416 = CARTESIAN_POINT ( 'NONE',  ( -47.55235941796721733, 12.79790236059689867, 64.89954721557026573 ) ) ;
#56417 = VECTOR ( 'NONE', #34075, 1000.000000000000000 ) ;
#56418 = CARTESIAN_POINT ( 'NONE',  ( -99.60580143997752600, 31.44299022783583197, -89.19348776790582178 ) ) ;
#56419 = ORIENTED_EDGE ( 'NONE', *, *, #46306, .T. ) ;
#56420 = CARTESIAN_POINT ( 'NONE',  ( 279.3411025683419666, 21.43200632497276104, -4.967238636669200069 ) ) ;
#56421 = VECTOR ( 'NONE', #6073, 1000.000000000000000 ) ;
#56422 = LINE ( 'NONE', #62749, #7156 ) ;
#56423 = DIRECTION ( 'NONE',  ( -0.000000000000000000, 1.000000000000000000, -0.000000000000000000 ) ) ;
#56424 = CARTESIAN_POINT ( 'NONE',  ( 61.91366885787816443, -28.42865614898931881, 0.000000000000000000 ) ) ;
#56425 = CARTESIAN_POINT ( 'NONE',  ( -0.4403665414075291773, 7.529347476604110412, 89.95601636005106627 ) ) ;
#56426 = VERTEX_POINT ( 'NONE', #69142 ) ;
#56427 = CYLINDRICAL_SURFACE ( 'NONE', #5569, 7.500000000000013323 ) ;
#56428 = DIRECTION ( 'NONE',  ( 0.9195277725514489076, 0.3930250316539278810, 5.102127870520022769E-18 ) ) ;
#56429 = ORIENTED_EDGE ( 'NONE', *, *, #4914, .T. ) ;
#56430 = ORIENTED_EDGE ( 'NONE', *, *, #23031, .F. ) ;
#56431 = DIRECTION ( 'NONE',  ( -0.000000000000000000, 1.000000000000000000, -0.000000000000000000 ) ) ;
#56432 = CARTESIAN_POINT ( 'NONE',  ( -5.767955557622883589E-14, -31.11269837220806878, 85.00100000000000477 ) ) ;
#56433 = DIRECTION ( 'NONE',  ( -0.000000000000000000, -0.000000000000000000, -1.000000000000000000 ) ) ;
#56434 = ORIENTED_EDGE ( 'NONE', *, *, #8425, .F. ) ;
#56435 = CARTESIAN_POINT ( 'NONE',  ( 2.051824250824025420, -73.54888393769144272, 133.5802547743875550 ) ) ;
#56436 = CARTESIAN_POINT ( 'NONE',  ( -173.9656771507954431, 88.06879734510549440, 18.97714401617737323 ) ) ;
#56437 = CARTESIAN_POINT ( 'NONE',  ( -4.513903087372272083, 6.697902023160579255, 4.037233194458375252 ) ) ;
#56438 = CARTESIAN_POINT ( 'NONE',  ( 56.52205390515079841, 12.28646189164059166, -39.43576307262695479 ) ) ;
#56439 = CARTESIAN_POINT ( 'NONE',  ( -86.06525741550311182, 26.37048289224653885, 39.17186844186085892 ) ) ;
#56440 = CARTESIAN_POINT ( 'NONE',  ( -24.03640295269300964, 9.507963273819775907, -17.20195008455281993 ) ) ;
#56441 = CARTESIAN_POINT ( 'NONE',  ( 141.3403471770512851, 46.13063628128485760, 9.603197491847479839 ) ) ;
#56442 = EDGE_CURVE ( 'NONE', #53458, #23927, #31527, .T. ) ;
#56443 = EDGE_CURVE ( 'NONE', #2227, #66603, #26252, .T. ) ;
#56444 = ORIENTED_EDGE ( 'NONE', *, *, #15088, .F. ) ;
#56445 = CARTESIAN_POINT ( 'NONE',  ( 115.0692128464502417, 31.17922615202198600, -37.66088901092161478 ) ) ;
#56446 = EDGE_CURVE ( 'NONE', #925, #10198, #68797, .T. ) ;
#56447 = CARTESIAN_POINT ( 'NONE',  ( -76.32456871438914447, 22.51591205926308703, 3.932499122260883606 ) ) ;
#56448 = DIRECTION ( 'NONE',  ( -1.000000000000000000, -1.001918829714556097E-14, 9.899279560275163638E-15 ) ) ;
#56449 = CARTESIAN_POINT ( 'NONE',  ( 3.000000000000028866, 2.999999999999969802, 0.000000000000000000 ) ) ;
#56451 = ORIENTED_EDGE ( 'NONE', *, *, #63766, .T. ) ;
#56450 = CARTESIAN_POINT ( 'NONE',  ( 0.000000000000000000, 0.000000000000000000, 0.000000000000000000 ) ) ;
#56452 = CARTESIAN_POINT ( 'NONE',  ( 84.73231936899557581, 18.78199960571076943, -50.59343781656497896 ) ) ;
#56453 = AXIS2_PLACEMENT_3D ( 'NONE', #17, #64385, #54866 ) ;
#56454 = VERTEX_POINT ( 'NONE', #37836 ) ;
#56455 = AXIS2_PLACEMENT_3D ( 'NONE', #53746, #22445, #11887 ) ;
#56456 = FACE_OUTER_BOUND ( 'NONE', #35480, .T. ) ;
#56457 = DIRECTION ( 'NONE',  ( 0.000000000000000000, 0.000000000000000000, 1.000000000000000000 ) ) ;
#56458 = CARTESIAN_POINT ( 'NONE',  ( -442.6627218934913230, 394.9999999999998295, -123.9497041420119530 ) ) ;
#56459 = CARTESIAN_POINT ( 'NONE',  ( -20.55634918610396866, 31.11269837220809009, 85.00100000000000477 ) ) ;
#56460 = CIRCLE ( 'NONE', #50894, 21.99999999999997158 ) ;
#56461 = CARTESIAN_POINT ( 'NONE',  ( -123.4531143159639157, 44.90777521523903459, 57.86905838940393210 ) ) ;
#56462 = CARTESIAN_POINT ( 'NONE',  ( -81.89510452344293867, 24.66033552777455284, -22.55706376423087178 ) ) ;
#56463 = CARTESIAN_POINT ( 'NONE',  ( -180.5801285865471471, 97.42945596116095430, -16.16651611906625163 ) ) ;
#56464 = AXIS2_PLACEMENT_3D ( 'NONE', #22932, #39807, #17656 ) ;
#56465 = CARTESIAN_POINT ( 'NONE',  ( -47.94960849910474110, 13.92522873833625141, 40.27489391830895471 ) ) ;
#56466 = ORIENTED_EDGE ( 'NONE', *, *, #61076, .T. ) ;
#56467 = ADVANCED_FACE ( 'NONE', ( #20969 ), #64216, .F. ) ;
#56468 = ORIENTED_EDGE ( 'NONE', *, *, #65294, .F. ) ;
#56469 = EDGE_CURVE ( 'NONE', #41104, #42670, #53300, .T. ) ;
#56470 = EDGE_CURVE ( 'NONE', #29725, #20901, #37572, .T. ) ;
#56471 = CARTESIAN_POINT ( 'NONE',  ( 110.2429982417149432, 28.88204397445228722, 71.45576479620103783 ) ) ;
#56472 = AXIS2_PLACEMENT_3D ( 'NONE', #60278, #59559, #38115 ) ;
#56473 = CARTESIAN_POINT ( 'NONE',  ( 164.7250737226290198, 63.51898362052162383, 65.67648673783554614 ) ) ;
#56474 = CARTESIAN_POINT ( 'NONE',  ( -189.9554299271397326, 108.0836897899587967, 68.49611169383959464 ) ) ;
#56475 = FACE_OUTER_BOUND ( 'NONE', #34985, .T. ) ;
#56476 = DIRECTION ( 'NONE',  ( 6.405132834375898112E-16, -1.000000000000000000, 1.396592535537253184E-14 ) ) ;
#56477 = CARTESIAN_POINT ( 'NONE',  ( -142.3939495481492372, 59.65374914730258382, 94.38145074191702122 ) ) ;
#56478 = VERTEX_POINT ( 'NONE', #42421 ) ;
#56479 = ORIENTED_EDGE ( 'NONE', *, *, #66650, .T. ) ;
#56480 = ORIENTED_EDGE ( 'NONE', *, *, #45610, .F. ) ;
#56481 = CARTESIAN_POINT ( 'NONE',  ( 31.11269837220806522, -6.375108774214766072E-14, 2.000000000000001776 ) ) ;
#56482 = CARTESIAN_POINT ( 'NONE',  ( -71.15978761293872878, 19.60276553435116753, 91.52478201086924514 ) ) ;
#56483 = CARTESIAN_POINT ( 'NONE',  ( 174.3239633726426803, 72.03325965189267777, -94.13525938529653558 ) ) ;
#56484 = CARTESIAN_POINT ( 'NONE',  ( 66.29961816943398389, 13.45804302849870204, -49.98079997445120881 ) ) ;
#56485 = DIRECTION ( 'NONE',  ( 0.000000000000000000, 0.000000000000000000, 1.000000000000000000 ) ) ;
#56486 = CARTESIAN_POINT ( 'NONE',  ( -57.43883374585513479, 16.37892664338858495, 44.93176015419845726 ) ) ;
#56487 = LINE ( 'NONE', #51223, #11265 ) ;
#56488 = CARTESIAN_POINT ( 'NONE',  ( 63.01563776193090405, 13.70579113808097738, 44.81296093922130552 ) ) ;
#56489 = CARTESIAN_POINT ( 'NONE',  ( 38.09561781553523474, 8.243036803495508380, 83.71016925063842962 ) ) ;
#56490 = CARTESIAN_POINT ( 'NONE',  ( 450.2085304802404266, 188.0000000000000000, -247.8920266495912870 ) ) ;
#56491 = ORIENTED_EDGE ( 'NONE', *, *, #56193, .T. ) ;
#56492 = CARTESIAN_POINT ( 'NONE',  ( 33.08880980852370612, -4.734317562933250123, 6.893342931793783102 ) ) ;
#56493 = CARTESIAN_POINT ( 'NONE',  ( 133.8566784816069344, 42.60093787723652525, -77.86786152285937135 ) ) ;
#56494 = CARTESIAN_POINT ( 'NONE',  ( -189.9554299271397895, 108.0836897899587825, -38.88209066801512392 ) ) ;
#56495 = CARTESIAN_POINT ( 'NONE',  ( 15.55634918610396511, -41.66904755831214402, 0.000000000000000000 ) ) ;
#56496 = LINE ( 'NONE', #32193, #5126 ) ;
#56497 = CARTESIAN_POINT ( 'NONE',  ( 199.7278513351971299, 99.76879341361768638, 69.18835753365968344 ) ) ;
#56498 = VECTOR ( 'NONE', #60732, 1000.000000000000000 ) ;
#56499 = ORIENTED_EDGE ( 'NONE', *, *, #36220, .T. ) ;
#56500 = PRESENTATION_LAYER_ASSIGNMENT (  '', '', ( #58740 ) ) ;
#56501 = DIRECTION ( 'NONE',  ( 0.9108602745606092510, 0.4127148655274866518, -6.586019698969276444E-15 ) ) ;
#56502 = CARTESIAN_POINT ( 'NONE',  ( 126.3554864210862121, 38.22801630372146775, -43.29534180877571004 ) ) ;
#56503 = CARTESIAN_POINT ( 'NONE',  ( -35.38962320578853138, 11.29584325137385470, -36.43726333423634145 ) ) ;
#56504 = CARTESIAN_POINT ( 'NONE',  ( 149.0250918491436494, 6.000000000000000000, -36.68900338898720292 ) ) ;
#56505 = LINE ( 'NONE', #7290, #56870 ) ;
#56506 = ORIENTED_EDGE ( 'NONE', *, *, #65680, .F. ) ;
#56507 = CYLINDRICAL_SURFACE ( 'NONE', #13321, 21.00000000000000355 ) ;
#56508 = VECTOR ( 'NONE', #65652, 1000.000000000000000 ) ;
#56509 = B_SPLINE_CURVE_WITH_KNOTS ( 'NONE', 3,
 ( #55607, #30181, #41425, #62879, #66192, #46336, #65834, #46002, #39429, #3105, #17631, #3783, #19616, #25254, #39099, #17985, #7074, #67469, #22905, #44715, #62176, #19263, #41076, #46690 ),
 .UNSPECIFIED., .F., .F.,
 ( 4, 2, 2, 2, 2, 2, 2, 2, 2, 2, 2, 4 ),
 ( 0.01054657901234073818, 0.01186033960812336516, 0.01251721990601467951, 0.01317410020390599387, 0.01448786079968862606, 0.01514474109757995256, 0.01580162139547127906, 0.01711538199125392859, 0.01777226228914526723, 0.01842914258703660935, 0.01974290318281925541, 0.02105666377860190147 ),
 .UNSPECIFIED. ) ;
#56510 = FACE_BOUND ( 'NONE', #23428, .T. ) ;
#56511 = VECTOR ( 'NONE', #55825, 1000.000000000000227 ) ;
#56512 = CARTESIAN_POINT ( 'NONE',  ( 188.1848725084043110, 86.09288252323347024, -95.00000000000133582 ) ) ;
#56513 = ORIENTED_EDGE ( 'NONE', *, *, #5876, .F. ) ;
#56514 = VECTOR ( 'NONE', #4261, 1000.000000000000000 ) ;
#56515 = B_SPLINE_CURVE_WITH_KNOTS ( 'NONE', 3,
 ( #68986, #63734, #15542, #26444, #36993, #31712, #53143, #47881 ),
 .UNSPECIFIED., .F., .F.,
 ( 4, 2, 2, 4 ),
 ( 0.004673709593152149643, 0.005837709341827642534, 0.007001709090503134558, 0.009329708587854118607 ),
 .UNSPECIFIED. ) ;
#56516 = CARTESIAN_POINT ( 'NONE',  ( 156.9750372531276525, 58.53928062478365746, 83.09115216898715062 ) ) ;
#56517 = ORIENTED_EDGE ( 'NONE', *, *, #16118, .T. ) ;
#56518 = CARTESIAN_POINT ( 'NONE',  ( 33.53140065650502066, -18.57796444702716343, 13.32819299319723072 ) ) ;
#56519 = DIRECTION ( 'NONE',  ( 0.000000000000000000, 0.000000000000000000, -1.000000000000000000 ) ) ;
#56520 = CARTESIAN_POINT ( 'NONE',  ( -156.6862310659955710, 71.88416263379569671, 40.46439280054978838 ) ) ;
#56521 = AXIS2_PLACEMENT_3D ( 'NONE', #68828, #43481, #15725 ) ;
#56523 = EDGE_CURVE ( 'NONE', #59923, #58815, #69490, .T. ) ;
#56522 = CARTESIAN_POINT ( 'NONE',  ( -30.00000000000000355, -30.00000000000000355, 15.00000000000000000 ) ) ;
#56524 = DIRECTION ( 'NONE',  ( 0.000000000000000000, 0.000000000000000000, 1.000000000000000000 ) ) ;
#56526 = ORIENTED_EDGE ( 'NONE', *, *, #19929, .T. ) ;
#56525 = DIRECTION ( 'NONE',  ( 1.000000000000000000, 0.000000000000000000, 0.000000000000000000 ) ) ;
#56527 = CARTESIAN_POINT ( 'NONE',  ( 62.52742438962774685, 12.55954017561947822, 44.81296093922129131 ) ) ;
#56528 = EDGE_CURVE ( 'NONE', #23369, #61020, #65767, .T. ) ;
#56529 = ORIENTED_EDGE ( 'NONE', *, *, #54131, .T. ) ;
#56530 = ORIENTED_EDGE ( 'NONE', *, *, #5092, .T. ) ;
#56531 = CARTESIAN_POINT ( 'NONE',  ( -166.3231866619663037, 81.31146386205584520, 14.65755802791554174 ) ) ;
#56532 = EDGE_CURVE ( 'NONE', #64743, #39418, #42756, .T. ) ;
#56533 = CARTESIAN_POINT ( 'NONE',  ( 20.74093720376648875, 6.709541214524347374, -75.51682261295336218 ) ) ;
#56534 = B_SPLINE_CURVE_WITH_KNOTS ( 'NONE', 3,
 ( #12700, #51028, #2842, #19015, #61910, #13735, #28885, #2154, #23608, #4561, #67907, #41510, #51719, #9848, #3525, #63314, #36583, #20386, #57692, #24997, #14769, #52409, #68253, #20058, #46428, #10177, #26024, #53073, #19705, #25347, #35888, #9501, #41168, #52064, #68585, #36234, #46782, #62266, #62627, #14438, #58029, #62962, #35545, #21093, #15122, #20739, #25693, #31308, #63661, #4903 ),
 .UNSPECIFIED., .F., .F.,
 ( 4, 2, 2, 2, 2, 2, 2, 2, 2, 2, 2, 2, 2, 2, 2, 2, 2, 2, 2, 2, 2, 2, 2, 2, 4 ),
 ( 0.03126542424884321686, 0.03330676804260263718, 0.03534811183636205056, 0.03738945563012147089, 0.03943079942388089121, 0.04045147132076060137, 0.04147214321764031153, 0.04249281511452002169, 0.04351348701139972491, 0.04555483080515914524, 0.04657550270203887621, 0.04759617459891860025, 0.04810651054735845533, 0.04861684649579831041, 0.04963751839267802057, 0.05065819028955773073, 0.05167886218643744090, 0.05269953408331715106, 0.05372020598019686122, 0.05474087787707657138, 0.05576154977395628154, 0.05780289356771577125, 0.05984423736147527484, 0.06188558115523477149, 0.06392692494899426814 ),
 .UNSPECIFIED. ) ;
#56536 = ORIENTED_EDGE ( 'NONE', *, *, #25121, .F. ) ;
#56535 = CARTESIAN_POINT ( 'NONE',  ( -132.2286325684322605, 52.04087929935078449, 68.98771376788437237 ) ) ;
#56537 = CARTESIAN_POINT ( 'NONE',  ( -97.11368346811575236, 31.34882221015812576, 86.26249857170712687 ) ) ;
#56538 = EDGE_CURVE ( 'NONE', #39735, #58197, #34285, .T. ) ;
#56539 = CARTESIAN_POINT ( 'NONE',  ( -74.18622060908363380, 21.73430079572374396, -48.64965096766535879 ) ) ;
#56540 = ORIENTED_EDGE ( 'NONE', *, *, #21450, .F. ) ;
#56541 = CARTESIAN_POINT ( 'NONE',  ( 204.6977192012829789, 108.0580384837235073, -63.17048162308526571 ) ) ;
#56542 = CARTESIAN_POINT ( 'NONE',  ( 139.2794027252094224, 45.99190465195511024, 42.21385594671063046 ) ) ;
#56544 = CARTESIAN_POINT ( 'NONE',  ( 113.8724110608469005, 31.71510301790680941, 30.53043836141040046 ) ) ;
#56543 = PRESENTATION_LAYER_ASSIGNMENT (  '', '', ( #34118 ) ) ;
#56545 = CARTESIAN_POINT ( 'NONE',  ( 44.99999999999999289, 20.00000000000000355, 4.000000000000000000 ) ) ;
#56546 = CARTESIAN_POINT ( 'NONE',  ( 66.30636076182545935, 14.49616748423541424, -63.30812756663202379 ) ) ;
#56547 = ADVANCED_FACE ( 'NONE', ( #5478 ), #31193, .F. ) ;
#56548 = B_SPLINE_CURVE_WITH_KNOTS ( 'NONE', 3,
 ( #50954, #55174, #2766, #17903, #43915, #36504, #67484, #19632, #67833, #3123, #41784, #51986, #29842, #41093, #62194, #57619, #30887, #9086, #24583, #51650, #14011, #57956, #41440, #30537, #62895, #14698, #61837, #24920, #13663, #68184, #46708, #51312, #62554, #15050, #36160, #3803, #14364, #35821, #19280, #9776, #31238, #57274, #25271, #19988, #68512 ),
 .UNSPECIFIED., .F., .F.,
 ( 4, 2, 2, 2, 2, 2, 2, 2, 1, 2, 2, 2, 2, 2, 2, 2, 2, 2, 2, 2, 2, 2, 4 ),
 ( 0.000000000000000000, 0.001470449819620692038, 0.002205674729431027214, 0.002940899639241362391, 0.004411349458862014530, 0.005881799278482666669, 0.007352249098103315339, 0.008087474007913642710, 0.008822698917723968345, 0.009557923827534293981, 0.01029314873734462135, 0.01176359855696526915, 0.01249882346677558959, 0.01323404837658591002, 0.01470449819620655435, 0.01543972310601688346, 0.01617494801582720909, 0.01764539783544786383, 0.01911584765506852204, 0.01985107256487885982, 0.02058629747468919760, 0.02205674729430986969, 0.02352719711393054525 ),
 .UNSPECIFIED. ) ;
#56549 = ORIENTED_EDGE ( 'NONE', *, *, #51267, .F. ) ;
#56550 = EDGE_LOOP ( 'NONE', ( #18829, #48443, #46061, #33025 ) ) ;
#56551 = MECHANICAL_DESIGN_GEOMETRIC_PRESENTATION_REPRESENTATION (  '', ( #25141 ), #27357 ) ;
#56552 = CARTESIAN_POINT ( 'NONE',  ( 188.9999999999999432, -0.000000000000000000, 0.000000000000000000 ) ) ;
#56553 = CARTESIAN_POINT ( 'NONE',  ( 8.000000000000007105, 249.8719672152120381, -95.00000000000133582 ) ) ;
#56554 = AXIS2_PLACEMENT_3D ( 'NONE', #38568, #53001, #22391 ) ;
#56555 = CARTESIAN_POINT ( 'NONE',  ( -54.20011053040712312, 14.45452627381339461, -88.95099551034488172 ) ) ;
#56556 = FACE_OUTER_BOUND ( 'NONE', #22787, .T. ) ;
#56557 = CARTESIAN_POINT ( 'NONE',  ( -142.2626321327577443, 58.26997216742664421, 36.26161877387822585 ) ) ;
#56558 = CARTESIAN_POINT ( 'NONE',  ( -128.1384526288949814, 47.98891607499721346, 57.79359961142665014 ) ) ;
#56559 = CARTESIAN_POINT ( 'NONE',  ( -165.9986675144415642, 79.53506019208350608, -66.68918146554828752 ) ) ;
#56560 = EDGE_LOOP ( 'NONE', ( #14415, #39225, #41051, #27068 ) ) ;
#56561 = B_SPLINE_CURVE_WITH_KNOTS ( 'NONE', 3,
 ( #35616, #57070, #8883, #25757, #31372, #5651, #4298, #47187, #42936, #21161, #27110, #36650, #4624, #26088, #26780, #48206, #21833, #64403, #42605, #68643, #64059, #31, #381, #59116, #37317, #69338, #20455, #10242, #26439, #53832, #16215, #63380, #52801, #41918, #21486, #15871, #58096, #15190, #53139, #15538, #5322, #63728, #47875 ),
 .UNSPECIFIED., .F., .F.,
 ( 4, 2, 2, 2, 2, 2, 2, 2, 2, 2, 2, 2, 1, 2, 2, 2, 2, 2, 2, 2, 2, 4 ),
 ( 0.02362927190606132002, 0.02510248541563186997, 0.02583909217041715015, 0.02657569892520242685, 0.02804891243477298374, 0.02952212594434354409, 0.03025873269912882080, 0.03099533945391410097, 0.03246855296348467868, 0.03394176647305524597, 0.03541497998262582714, 0.03615158673741111772, 0.03688819349219642219, 0.03762480024698171971, 0.03836140700176701723, 0.03983462051133761228, 0.04130783402090821427, 0.04278104753047881625, 0.04351765428526410684, 0.04425426104004939742, 0.04572747454961999247, 0.04720068805919059446 ),
 .UNSPECIFIED. ) ;
#56563 = CARTESIAN_POINT ( 'NONE',  ( -102.7447593990059289, 34.14748189312174276, 30.51907450641510522 ) ) ;
#56562 = AXIS2_PLACEMENT_3D ( 'NONE', #15672, #172, #42403 ) ;
#56564 = VERTEX_POINT ( 'NONE', #20613 ) ;
#56565 = CARTESIAN_POINT ( 'NONE',  ( -176.9364071963078686, 91.47427511280444890, -89.38709468048955387 ) ) ;
#56566 = B_SPLINE_CURVE_WITH_KNOTS ( 'NONE', 3,
 ( #20511, #19835, #30048, #4004, #41292, #58155 ),
 .UNSPECIFIED., .F., .F.,
 ( 4, 2, 4 ),
 ( 0.03218932480516803474, 0.06469831007220622210, 0.09720729533924440946 ),
 .UNSPECIFIED. ) ;
#56567 = AXIS2_PLACEMENT_3D ( 'NONE', #39394, #6334, #33076 ) ;
#56568 = CARTESIAN_POINT ( 'NONE',  ( 83.38619203015946368, 19.39783821526630803, 57.27713636182927814 ) ) ;
#56569 = ORIENTED_EDGE ( 'NONE', *, *, #11015, .F. ) ;
#56570 = CYLINDRICAL_SURFACE ( 'NONE', #31854, 245.3095347406802205 ) ;
#56571 = CARTESIAN_POINT ( 'NONE',  ( -189.2352924136013428, 107.0839554967701162, -69.40233452781009760 ) ) ;
#56572 = DIRECTION ( 'NONE',  ( 1.000000000000000000, 0.000000000000000000, 0.000000000000000000 ) ) ;
#56573 = DIRECTION ( 'NONE',  ( -1.000000000000000000, 0.000000000000000000, -0.000000000000000000 ) ) ;
#56574 = DIRECTION ( 'NONE',  ( 1.000000000000000000, 0.000000000000000000, 0.000000000000000000 ) ) ;
#56575 = CARTESIAN_POINT ( 'NONE',  ( -15.32584732649904424, 8.506915958926391852, -42.42966520005830233 ) ) ;
#56576 = VECTOR ( 'NONE', #21612, 1000.000000000000000 ) ;
#56577 = DIRECTION ( 'NONE',  ( -1.000000000000000000, 0.000000000000000000, 0.000000000000000000 ) ) ;
#56578 = ORIENTED_EDGE ( 'NONE', *, *, #47447, .F. ) ;
#56579 = CARTESIAN_POINT ( 'NONE',  ( -8.000000000000000000, 4.618802153517024500, -8.785468820183664818 ) ) ;
#56580 = ORIENTED_EDGE ( 'NONE', *, *, #54622, .T. ) ;
#56581 = CARTESIAN_POINT ( 'NONE',  ( 0.000000000000000000, 35.00000000000000000, 0.000000000000000000 ) ) ;
#56582 = CARTESIAN_POINT ( 'NONE',  ( -60.66101049381766330, 17.30588917955501671, 69.66552825106393243 ) ) ;
#56583 = FACE_OUTER_BOUND ( 'NONE', #21922, .T. ) ;
#56584 = ORIENTED_EDGE ( 'NONE', *, *, #62660, .T. ) ;
#56585 = CARTESIAN_POINT ( 'NONE',  ( 15.55634918610397399, -26.11269837220809364, 85.00100000000000477 ) ) ;
#56586 = CARTESIAN_POINT ( 'NONE',  ( 154.4435090467314922, 56.59612921827835663, -63.60279279905601868 ) ) ;
#56587 = CARTESIAN_POINT ( 'NONE',  ( -38.93878980550034896, 10.94326053663842302, 38.21361434711087668 ) ) ;
#56588 = CARTESIAN_POINT ( 'NONE',  ( 135.6842057900327347, 42.53841116629840968, -36.23475628795622328 ) ) ;
#56589 = ORIENTED_EDGE ( 'NONE', *, *, #30023, .F. ) ;
#56590 = CARTESIAN_POINT ( 'NONE',  ( 620.5071894358270583, 928.5915846175170145, 486.5068267248709049 ) ) ;
#56591 = DIRECTION ( 'NONE',  ( 0.000000000000000000, 0.000000000000000000, 1.000000000000000000 ) ) ;
#56592 = CARTESIAN_POINT ( 'NONE',  ( -119.5576859660651508, 42.46117483543969939, 34.09885795874915715 ) ) ;
#56593 = CARTESIAN_POINT ( 'NONE',  ( -61.86845765289634613, 16.61548683002701665, -45.85609512080901595 ) ) ;
#56594 = VERTEX_POINT ( 'NONE', #48359 ) ;
#56595 = CARTESIAN_POINT ( 'NONE',  ( -180.2243452982808662, 96.99029284948635166, -66.63178993611138878 ) ) ;
#56596 = EDGE_CURVE ( 'NONE', #32692, #52465, #43101, .T. ) ;
#56597 = CARTESIAN_POINT ( 'NONE',  ( 128.9420992581156042, 39.69520347227675217, 85.02391764104523020 ) ) ;
#56598 = CARTESIAN_POINT ( 'NONE',  ( 111.1767565371974769, 29.31586421952251698, 29.65471990763289512 ) ) ;
#56599 = SURFACE_SIDE_STYLE ('',( #56958 ) ) ;
#56600 = VECTOR ( 'NONE', #26403, 1000.000000000000000 ) ;
#56601 = CARTESIAN_POINT ( 'NONE',  ( -122.7930600691577894, 44.48546375740913561, -62.41358845972529679 ) ) ;
#56602 = ORIENTED_EDGE ( 'NONE', *, *, #44367, .F. ) ;
#56603 = CARTESIAN_POINT ( 'NONE',  ( 197.1974290009104891, 96.59277840252784131, 36.38369672051224057 ) ) ;
#56604 = CARTESIAN_POINT ( 'NONE',  ( 6.800000000000000711, 6.123233995736767268E-16, -5.000000000000000888 ) ) ;
#56605 = AXIS2_PLACEMENT_3D ( 'NONE', #63152, #9689, #14612 ) ;
#56606 = CARTESIAN_POINT ( 'NONE',  ( 69.49862690228272299, 14.27023134440514340, 60.35422735765934021 ) ) ;
#56607 = DIRECTION ( 'NONE',  ( 0.000000000000000000, 1.000000000000000000, -0.000000000000000000 ) ) ;
#56608 = DIRECTION ( 'NONE',  ( 0.04486483035051862939, -0.9989930665413143673, 0.000000000000000000 ) ) ;
#56609 = AXIS2_PLACEMENT_3D ( 'NONE', #22229, #27851, #22577 ) ;
#56610 = ORIENTED_EDGE ( 'NONE', *, *, #43895, .T. ) ;
#56611 = VECTOR ( 'NONE', #63995, 1000.000000000000000 ) ;
#56612 = CARTESIAN_POINT ( 'NONE',  ( 164.1352994389932576, 64.33767534192698179, -20.22913284204803475 ) ) ;
#56613 = AXIS2_PLACEMENT_3D ( 'NONE', #12755, #32813, #54603 ) ;
#56614 = EDGE_CURVE ( 'NONE', #30648, #35148, #67001, .T. ) ;
#56615 = VERTEX_POINT ( 'NONE', #6869 ) ;
#56616 = DIRECTION ( 'NONE',  ( -0.000000000000000000, -0.000000000000000000, -1.000000000000000000 ) ) ;
#56617 = CARTESIAN_POINT ( 'NONE',  ( 129.7260862822010665, 38.98566587309944964, 84.43068361936597910 ) ) ;
#56618 = VECTOR ( 'NONE', #17855, 1000.000000000000000 ) ;
#56619 = VECTOR ( 'NONE', #15579, 1000.000000000000000 ) ;
#56620 = ORIENTED_EDGE ( 'NONE', *, *, #21499, .T. ) ;
#56621 = CARTESIAN_POINT ( 'NONE',  ( -142.8450945664715448, 58.72815783657284783, -65.70266265617578938 ) ) ;
#56622 = EDGE_CURVE ( 'NONE', #37519, #629, #60243, .T. ) ;
#56623 = CARTESIAN_POINT ( 'NONE',  ( 64.98797965777978902, 1.250000000000011990, 40.00000000000003553 ) ) ;
#56624 = DIRECTION ( 'NONE',  ( -1.000000000000000000, -0.000000000000000000, 0.000000000000000000 ) ) ;
#56625 = CARTESIAN_POINT ( 'NONE',  ( 164.9559213734324885, 63.71338633026439879, -43.08067803092567516 ) ) ;
#56626 = ORIENTED_EDGE ( 'NONE', *, *, #55645, .T. ) ;
#56627 = LINE ( 'NONE', #56982, #58068 ) ;
#56628 = DIRECTION ( 'NONE',  ( -0.000000000000000000, 1.000000000000000000, -0.000000000000000000 ) ) ;
#56629 = CARTESIAN_POINT ( 'NONE',  ( 152.0703578754941248, 54.82056822058789436, -92.09310849956577272 ) ) ;
#56630 = LINE ( 'NONE', #35174, #2783 ) ;
#56631 = CARTESIAN_POINT ( 'NONE',  ( -143.6073342927367946, 59.33214134111805294, -91.36572565367391974 ) ) ;
#56632 = DIRECTION ( 'NONE',  ( 0.000000000000000000, 1.000000000000000000, -0.000000000000000000 ) ) ;
#56633 = EDGE_CURVE ( 'NONE', #31912, #63750, #45197, .T. ) ;
#56634 = ORIENTED_EDGE ( 'NONE', *, *, #68141, .F. ) ;
#56635 = DIRECTION ( 'NONE',  ( 0.000000000000000000, 1.000000000000000000, 0.000000000000000000 ) ) ;
#56636 = CARTESIAN_POINT ( 'NONE',  ( -40.99999999999996447, 0.000000000000000000, -6.071532165918820097E-15 ) ) ;
#56637 = ORIENTED_EDGE ( 'NONE', *, *, #59414, .T. ) ;
#56638 = EDGE_CURVE ( 'NONE', #22146, #62158, #62421, .T. ) ;
#56639 = EDGE_CURVE ( 'NONE', #33379, #8399, #63694, .T. ) ;
#56640 = CARTESIAN_POINT ( 'NONE',  ( -155.5977325361978103, 70.88311713755696530, -37.92850440926633837 ) ) ;
#56641 = CARTESIAN_POINT ( 'NONE',  ( 17.14961137969540772, -48.73599164036525622, 26.66469066592269499 ) ) ;
#56642 = CARTESIAN_POINT ( 'NONE',  ( -38.54712373114178092, 11.89174538567467820, 35.27342008138545282 ) ) ;
#56643 = B_SPLINE_CURVE_WITH_KNOTS ( 'NONE', 3,
 ( #29049, #50489, #18482, #2652 ),
 .UNSPECIFIED., .F., .F.,
 ( 4, 4 ),
 ( 9.900409499053008115E-07, 0.05658314289920116785 ),
 .UNSPECIFIED. ) ;
#56644 = CARTESIAN_POINT ( 'NONE',  ( -156.6819053601226130, 70.51177710383653618, -66.89866658464235627 ) ) ;
#56645 = PLANE ( 'NONE',  #42690 ) ;
#56646 = CARTESIAN_POINT ( 'NONE',  ( -48.32993240732255913, 12.98137013984324817, -66.19890796893723461 ) ) ;
#56647 = DIRECTION ( 'NONE',  ( -1.000000000000000000, 0.000000000000000000, 0.000000000000000000 ) ) ;
#56648 = CARTESIAN_POINT ( 'NONE',  ( 179.4279766878530040, 76.94722012158231905, 2.637092671877164118 ) ) ;
#56649 = CARTESIAN_POINT ( 'NONE',  ( 111.1868021579656727, 29.32055685204859330, 17.72207817859029078 ) ) ;
#56650 = ORIENTED_EDGE ( 'NONE', *, *, #47020, .F. ) ;
#56651 = VECTOR ( 'NONE', #33363, 1000.000000000000114 ) ;
#56652 = CARTESIAN_POINT ( 'NONE',  ( 311.0133388548732114, 0.000000000000000000, -153.4166086460792826 ) ) ;
#56653 = VERTEX_POINT ( 'NONE', #68055 ) ;
#56654 = DIRECTION ( 'NONE',  ( 0.000000000000000000, 1.000000000000000000, -0.000000000000000000 ) ) ;
#56655 = B_SPLINE_CURVE_WITH_KNOTS ( 'NONE', 3,
 ( #30389, #51840, #25127, #41635, #68703, #57814, #20513, #63438, #34981, #56425, #31427, #69035, #20866, #37047, #799, #64819, #27168, #42325, #48265, #21218, #58483, #43688, #15931, #48605, #63788, #10299, #36711, #27516, #9975, #4683, #37377, #15596, #58834, #92, #37732, #5027, #31769, #43346, #26150, #6057, #26493, #22253, #69399, #38075, #21546, #47928, #32806, #16618, #5382, #42993, #64464, #16276, #42664, #59175, #10646 ),
 .UNSPECIFIED., .F., .F.,
 ( 4, 2, 2, 2, 2, 2, 2, 2, 2, 2, 2, 2, 2, 2, 2, 2, 2, 2, 2, 1, 2, 2, 2, 2, 2, 2, 2, 4 ),
 ( 0.000000000000000000, 0.001947665408787207977, 0.002921498113180811748, 0.003895330817574415953, 0.004869163521968020159, 0.005842996226361623496, 0.006816828930755227701, 0.007790661635148831907, 0.009738327043936040317, 0.01071215974832964365, 0.01168599245272324699, 0.01265982515711685207, 0.01363365786151045540, 0.01460749056590405874, 0.01558132327029766381, 0.01752898867908487396, 0.01850282138347847383, 0.01947665408787208063, 0.02045048679226568397, 0.02142431949665928731, 0.02239815220105289065, 0.02337198490544649399, 0.02434581760984010079, 0.02531965031423370413, 0.02726731572302086917, 0.02824114842741447598, 0.02921498113180807585, 0.03116264654059524436 ),
 .UNSPECIFIED. ) ;
#56656 = CARTESIAN_POINT ( 'NONE',  ( 46.23304607317102466, 10.41544405387738337, -19.38122357973218968 ) ) ;
#56657 = PRESENTATION_LAYER_ASSIGNMENT (  '', '', ( #40936 ) ) ;
#56658 = CARTESIAN_POINT ( 'NONE',  ( 0.000000000000000000, -36.09918303830819752, 0.000000000000000000 ) ) ;
#56659 = LINE ( 'NONE', #68262, #40144 ) ;
#56660 = CARTESIAN_POINT ( 'NONE',  ( -9.450810044394341247, 7.002157412775469325, 83.97576989457125762 ) ) ;
#56661 = FACE_OUTER_BOUND ( 'NONE', #24522, .T. ) ;
#56662 = AXIS2_PLACEMENT_3D ( 'NONE', #65233, #27242, #48675 ) ;
#56663 = CARTESIAN_POINT ( 'NONE',  ( 141.0229350107040887, 45.92325889728665800, -95.00000000000133582 ) ) ;
#56664 = CARTESIAN_POINT ( 'NONE',  ( -51.84164840787185113, 39.21024726209461875, 170.0000000000000000 ) ) ;
#56665 = VERTEX_POINT ( 'NONE', #19858 ) ;
#56666 = VECTOR ( 'NONE', #28184, 1000.000000000000000 ) ;
#56667 = ORIENTED_EDGE ( 'NONE', *, *, #42718, .T. ) ;
#56668 = AXIS2_PLACEMENT_3D ( 'NONE', #33169, #18031, #64826 ) ;
#56669 = FACE_OUTER_BOUND ( 'NONE', #57868, .T. ) ;
#56670 = CARTESIAN_POINT ( 'NONE',  ( -27.00000000000000355, -27.00000000000000355, 0.000000000000000000 ) ) ;
#56671 = CARTESIAN_POINT ( 'NONE',  ( 13.02837909493185720, 36.05214288467553985, 13.32819397642332326 ) ) ;
#56672 = CARTESIAN_POINT ( 'NONE',  ( 105.8229724512851107, 27.98935528750253710, 57.89168491306591591 ) ) ;
#56673 = CONICAL_SURFACE ( 'NONE', #52197, 65.00000000000000000, 0.7853981633974497223 ) ;
#56674 = DIRECTION ( 'NONE',  ( 0.000000000000000000, -1.000000000000000000, 0.000000000000000000 ) ) ;
#56675 = FACE_OUTER_BOUND ( 'NONE', #65646, .T. ) ;
#56676 = ORIENTED_EDGE ( 'NONE', *, *, #20982, .T. ) ;
#56677 = CARTESIAN_POINT ( 'NONE',  ( -24.75616454008743972, 3.483147608716851806, 0.000000000000000000 ) ) ;
#56678 = CARTESIAN_POINT ( 'NONE',  ( 209.5118425285948831, 113.1852661712287329, 15.61864072547802351 ) ) ;
#56679 = CARTESIAN_POINT ( 'NONE',  ( -143.2587158300142107, 60.34092810886539837, 42.37670143261917843 ) ) ;
#56680 = CARTESIAN_POINT ( 'NONE',  ( 183.2136430849847955, 0.000000000000000000, -46.68900338898722424 ) ) ;
#56681 = EDGE_CURVE ( 'NONE', #30296, #17040, #41315, .T. ) ;
#56682 = CARTESIAN_POINT ( 'NONE',  ( 12.53962518824996408, 6.418270956987105258, -89.93529441773186761 ) ) ;
#56683 = ADVANCED_BREP_SHAPE_REPRESENTATION ( '', ( #41867, #66832 ), #23071 ) ;
#56684 = EDGE_CURVE ( 'NONE', #39170, #53637, #24106, .T. ) ;
#56685 = ORIENTED_EDGE ( 'NONE', *, *, #69178, .F. ) ;
#56686 = VERTEX_POINT ( 'NONE', #23751 ) ;
#56687 = CARTESIAN_POINT ( 'NONE',  ( 6.375108774214766072E-14, 31.11269837220806167, 2.000000000000001776 ) ) ;
#56688 = DIRECTION ( 'NONE',  ( 0.000000000000000000, -0.000000000000000000, -1.000000000000000000 ) ) ;
#56689 = CARTESIAN_POINT ( 'NONE',  ( -1.683356153843273750, 65.34430428700410687, 6.377659838150135158E-18 ) ) ;
#56690 = CARTESIAN_POINT ( 'NONE',  ( 36.44731223145974752, 20.32014051031833191, 13.79046340968177908 ) ) ;
#56691 = CARTESIAN_POINT ( 'NONE',  ( 21.54731028615039534, 6.753297381550458667, 86.38792578528536126 ) ) ;
#56692 = CARTESIAN_POINT ( 'NONE',  ( 83.60262962804348774, 18.41036205028015260, -77.03250514454457232 ) ) ;
#56693 = VERTEX_POINT ( 'NONE', #66677 ) ;
#56695 = EDGE_CURVE ( 'NONE', #29393, #14950, #18473, .T. ) ;
#56694 = CARTESIAN_POINT ( 'NONE',  ( -196.7348448768811409, -170.0000000000000000, -95.80018497893539120 ) ) ;
#56696 = DIRECTION ( 'NONE',  ( 0.000000000000000000, -0.000000000000000000, -1.000000000000000000 ) ) ;
#56697 = VERTEX_POINT ( 'NONE', #37396 ) ;
#56698 = ADVANCED_FACE ( 'NONE', ( #15612 ), #53219, .F. ) ;
#56699 = LINE ( 'NONE', #56014, #38473 ) ;
#56700 = ORIENTED_EDGE ( 'NONE', *, *, #56684, .T. ) ;
#56701 = VECTOR ( 'NONE', #37157, 1000.000000000000000 ) ;
#56702 = LINE ( 'NONE', #60809, #17389 ) ;
#56703 = LINE ( 'NONE', #3246, #63482 ) ;
#56704 = CYLINDRICAL_SURFACE ( 'NONE', #3281, 7.500000000000020428 ) ;
#56705 = EDGE_LOOP ( 'NONE', ( #57184, #48164, #4263, #14001 ) ) ;
#56706 = EDGE_CURVE ( 'NONE', #29231, #35096, #31445, .T. ) ;
#56707 = ORIENTED_EDGE ( 'NONE', *, *, #20722, .T. ) ;
#56708 = DIRECTION ( 'NONE',  ( 0.000000000000000000, 1.000000000000000000, 0.000000000000000000 ) ) ;
#56709 = ADVANCED_FACE ( 'NONE', ( #53568 ), #47598, .T. ) ;
#56710 = CARTESIAN_POINT ( 'NONE',  ( 44.99999999999999289, 22.99999999999998579, 0.000000000000000000 ) ) ;
#56711 = CARTESIAN_POINT ( 'NONE',  ( 107.2614272668149056, 28.62909081796204092, 17.15260657237848463 ) ) ;
#56712 = AXIS2_PLACEMENT_3D ( 'NONE', #15744, #10808, #5530 ) ;
#56713 = ORIENTED_EDGE ( 'NONE', *, *, #16888, .F. ) ;
#56714 = CIRCLE ( 'NONE', #5031, 5.000000000000060396 ) ;
#56715 = VECTOR ( 'NONE', #55183, 999.9999999999998863 ) ;
#56716 = FACE_OUTER_BOUND ( 'NONE', #16197, .T. ) ;
#56717 = CARTESIAN_POINT ( 'NONE',  ( 177.0027897064244655, 75.97676392242549070, -64.26111881574348672 ) ) ;
#56718 = AXIS2_PLACEMENT_3D ( 'NONE', #7231, #13209, #2309 ) ;
#56719 = PLANE ( 'NONE',  #43765 ) ;
#56720 = CARTESIAN_POINT ( 'NONE',  ( 115.0454575488273434, 31.16784721673997893, -22.34374271908251686 ) ) ;
#56721 = CARTESIAN_POINT ( 'NONE',  ( 83.59652366361575559, 19.46709838196857945, -36.45791133507715642 ) ) ;
#56722 = CARTESIAN_POINT ( 'NONE',  ( 0.1230226671127766652, 25.12215469714594107, 0.000000000000000000 ) ) ;
#56723 = ORIENTED_EDGE ( 'NONE', *, *, #53495, .T. ) ;
#56724 = EDGE_CURVE ( 'NONE', #29739, #51945, #20885, .T. ) ;
#56725 = EDGE_CURVE ( 'NONE', #13975, #910, #24192, .T. ) ;
#56726 = ORIENTED_EDGE ( 'NONE', *, *, #17630, .T. ) ;
#56727 = CARTESIAN_POINT ( 'NONE',  ( 43.14356474118743989, 8.925336319666879348, 4.050586556182519615 ) ) ;
#56728 = CARTESIAN_POINT ( 'NONE',  ( 178.1965488566139868, 77.14488558164482868, 3.028789085135533465 ) ) ;
#56729 = CARTESIAN_POINT ( 'NONE',  ( -38.02163356681019479, 11.78964455120423693, 94.99999999999866418 ) ) ;
#56730 = CARTESIAN_POINT ( 'NONE',  ( 210.6189312023034574, 114.8321746285510301, 94.99999999999866418 ) ) ;
#56731 = ADVANCED_FACE ( 'NONE', ( #42344 ), #4023, .T. ) ;
#56732 = CARTESIAN_POINT ( 'NONE',  ( -55.05276343752909440, 15.72344139423348430, 3.472777182467473800 ) ) ;
#56733 = CARTESIAN_POINT ( 'NONE',  ( -17.50000000000000000, -17.50000000000000000, 1.999999999999998224 ) ) ;
#56734 = CARTESIAN_POINT ( 'NONE',  ( 211.8348321742968778, 118.5227572644700160, 92.73579468022644789 ) ) ;
#56735 = CARTESIAN_POINT ( 'NONE',  ( 212.1669304543881935, 119.0398299474538675, 36.00701586133611443 ) ) ;
#56736 = CARTESIAN_POINT ( 'NONE',  ( -81.89510452344296709, 24.66033552777453863, 57.97658800716016003 ) ) ;
#56737 = PLANE ( 'NONE',  #1717 ) ;
#56738 = ORIENTED_EDGE ( 'NONE', *, *, #15580, .T. ) ;
#56739 = CARTESIAN_POINT ( 'NONE',  ( 12.91653430408660697, 7.431946598423014194, -23.11569640008216098 ) ) ;
#56740 = VERTEX_POINT ( 'NONE', #9992 ) ;
#56741 = CARTESIAN_POINT ( 'NONE',  ( 200.8410151090926092, 101.2014854111317277, -10.53460766635205559 ) ) ;
#56742 = ORIENTED_EDGE ( 'NONE', *, *, #14076, .T. ) ;
#56743 = CARTESIAN_POINT ( 'NONE',  ( -34.75846525699014933, 54.92585086258208804, 170.0000000000000000 ) ) ;
#56744 = CARTESIAN_POINT ( 'NONE',  ( 188.5838389098762775, 88.03667982118678026, -70.26040297313004146 ) ) ;
#56745 = CARTESIAN_POINT ( 'NONE',  ( -38.55173488399534421, 11.89269613674691328, 93.80691191228474679 ) ) ;
#56746 = CARTESIAN_POINT ( 'NONE',  ( -95.86612279493103017, 29.64021615886205652, -38.61911933511777306 ) ) ;
#56747 = B_SPLINE_CURVE_WITH_KNOTS ( 'NONE', 3,
 ( #25090, #68345, #14863, #63059, #10272, #32433, #60, #69367, #15904, #64090, #26806, #38395, #69010, #64785, #42633, #59835, #10614, #33130 ),
 .UNSPECIFIED., .F., .F.,
 ( 4, 2, 2, 2, 2, 2, 2, 2, 4 ),
 ( 0.01321666563952497188, 0.01669835041696196912, 0.01843919280568048769, 0.02018003519439900625, 0.02192087758311752482, 0.02366171997183604339, 0.02540256236055456196, 0.02627298355491380216, 0.02714340474927304583 ),
 .UNSPECIFIED. ) ;
#56748 = CARTESIAN_POINT ( 'NONE',  ( 31.90184941268614693, 7.552181687745345151, -43.36186114419296445 ) ) ;
#56749 = DIRECTION ( 'NONE',  ( 0.000000000000000000, 0.000000000000000000, -1.000000000000000000 ) ) ;
#56750 = CARTESIAN_POINT ( 'NONE',  ( 15.29305096970403000, 7.491604910111008486, -35.51894409868578606 ) ) ;
#56751 = DIRECTION ( 'NONE',  ( -0.000000000000000000, 1.000000000000000000, -0.000000000000000000 ) ) ;
#56752 = VERTEX_POINT ( 'NONE', #58500 ) ;
#56753 = EDGE_LOOP ( 'NONE', ( #32641, #55669, #19030, #30997 ) ) ;
#56754 = VECTOR ( 'NONE', #7437, 1000.000000000000000 ) ;
#56755 = FACE_OUTER_BOUND ( 'NONE', #5056, .T. ) ;
#56756 =( LENGTH_UNIT ( ) NAMED_UNIT ( * ) SI_UNIT ( .MILLI., .METRE. ) );
#56757 = LINE ( 'NONE', #8579, #60318 ) ;
#56758 = FACE_OUTER_BOUND ( 'NONE', #38768, .T. ) ;
#56759 = VECTOR ( 'NONE', #6275, 1000.000000000000000 ) ;
#56760 = DIRECTION ( 'NONE',  ( 0.000000000000000000, 0.000000000000000000, -1.000000000000000000 ) ) ;
#56761 = ORIENTED_EDGE ( 'NONE', *, *, #50768, .T. ) ;
#56762 = CARTESIAN_POINT ( 'NONE',  ( 283.9746407525165637, 21.78913134333902590, -3.050900938606339263 ) ) ;
#56763 = AXIS2_PLACEMENT_3D ( 'NONE', #45048, #43646, #65123 ) ;
#56764 = CIRCLE ( 'NONE', #43271, 65.00000000000000000 ) ;
#56765 = CARTESIAN_POINT ( 'NONE',  ( -60.66101049381764909, 17.30588917955502026, -64.55722470125444090 ) ) ;
#56766 = DIRECTION ( 'NONE',  ( -0.000000000000000000, 0.000000000000000000, -1.000000000000000000 ) ) ;
#56767 = DIRECTION ( 'NONE',  ( -1.000000000000000000, -1.205632815804107235E-16, 1.156482317317879614E-16 ) ) ;
#56768 = CARTESIAN_POINT ( 'NONE',  ( -179.2262621278718200, 94.19039042964671182, -37.82663789750925787 ) ) ;
#56769 = CARTESIAN_POINT ( 'NONE',  ( 105.8022841538864185, 26.88074187880708976, 4.203527470635210150 ) ) ;
#56770 = CARTESIAN_POINT ( 'NONE',  ( -24.71604178686820319, 9.599501655372948861, 61.22755308168638777 ) ) ;
#56771 = DIRECTION ( 'NONE',  ( 0.000000000000000000, 0.000000000000000000, 1.000000000000000000 ) ) ;
#56772 = CARTESIAN_POINT ( 'NONE',  ( -20.55634918610405748, -10.55634918610400597, 2.000000000000001776 ) ) ;
#56773 = AXIS2_PLACEMENT_3D ( 'NONE', #28229, #18042, #39158 ) ;
#56774 = EDGE_CURVE ( 'NONE', #55132, #13975, #15951, .T. ) ;
#56775 = VECTOR ( 'NONE', #68734, 1000.000000000000000 ) ;
#56776 = CARTESIAN_POINT ( 'NONE',  ( -1.876547441458561005, 6.576559737910137038, 59.88607102599485188 ) ) ;
#56777 = VERTEX_POINT ( 'NONE', #5047 ) ;
#56778 = DIRECTION ( 'NONE',  ( 0.000000000000000000, 0.000000000000000000, -1.000000000000000000 ) ) ;
#56779 = DIRECTION ( 'NONE',  ( -0.000000000000000000, -0.000000000000000000, -1.000000000000000000 ) ) ;
#56780 = CARTESIAN_POINT ( 'NONE',  ( 63.72039997003709288, 12.83396383267841223, 40.00000000000003553 ) ) ;
#56781 = CARTESIAN_POINT ( 'NONE',  ( -52.66507163626136645, 14.05394608175174653, -35.59014718343654238 ) ) ;
#56782 = DIRECTION ( 'NONE',  ( -1.000000000000000000, -1.001918046209079887E-14, 9.729495617646301779E-15 ) ) ;
#56783 = DIRECTION ( 'NONE',  ( 0.000000000000000000, 1.000000000000000000, 0.000000000000000000 ) ) ;
#56784 = B_SPLINE_CURVE_WITH_KNOTS ( 'NONE', 3,
 ( #29566, #62268, #40130, #51030, #67558, #57003, #19708, #2844, #19358, #40814, #13062, #61239, #8470, #29229, #61587, #40468, #13399, #19017, #51721, #14088, #34522, #50675, #46430, #56298, #24311, #30272, #7777, #34861, #8822, #45399, #3527, #67232, #25000, #39778, #23950, #66881, #45752, #18677, #61912, #67909, #41170, #40004, #38971, #12939, #28052, #55127, #61114 ),
 .UNSPECIFIED., .F., .F.,
 ( 4, 2, 2, 2, 2, 2, 2, 2, 2, 2, 2, 2, 1, 2, 2, 2, 2, 2, 2, 2, 2, 2, 2, 4 ),
 ( 1.734723475976807094E-18, 0.001493793014771601681, 0.002240689522157399919, 0.002987586029543198157, 0.004481379044314774684, 0.005228275551700562948, 0.005975172059086351212, 0.007468965073857914728, 0.008215861581243703859, 0.008962758088629493858, 0.01045655110340106171, 0.01120344761078684824, 0.01195034411817263130, 0.01269724062555841609, 0.01344413713294419915, 0.01493793014771577048, 0.01568482665510155527, 0.01643172316248733139, 0.01792551617725889751, 0.01941930919203046363, 0.02016620569941623281, 0.02091310220680200893, 0.02240689522157355423, 0.02390068823634509954 ),
 .UNSPECIFIED. ) ;
#56785 = ORIENTED_EDGE ( 'NONE', *, *, #19771, .T. ) ;
#56787 = EDGE_CURVE ( 'NONE', #15010, #25468, #58610, .T. ) ;
#56786 = CARTESIAN_POINT ( 'NONE',  ( -444.4229916354184979, 388.0000000000064233, 96.05029585798874336 ) ) ;
#56788 = CARTESIAN_POINT ( 'NONE',  ( -447.6627218934913230, 367.0710678118653050, 108.5502958579877202 ) ) ;
#56789 = VERTEX_POINT ( 'NONE', #6075 ) ;
#56790 = ORIENTED_EDGE ( 'NONE', *, *, #9396, .F. ) ;
#56791 = CARTESIAN_POINT ( 'NONE',  ( 0.000000000000000000, 0.000000000000000000, -9.500000000000000000 ) ) ;
#56792 = CARTESIAN_POINT ( 'NONE',  ( 447.3372781065085633, 399.9999999999998863, 83.55029585798818914 ) ) ;
#56793 = EDGE_CURVE ( 'NONE', #27253, #57871, #59886, .T. ) ;
#56794 = DIRECTION ( 'NONE',  ( -1.000000000000000000, 0.000000000000000000, 0.000000000000000000 ) ) ;
#56795 = VERTEX_POINT ( 'NONE', #48619 ) ;
#56796 = CARTESIAN_POINT ( 'NONE',  ( 311.9975424824652350, 20.00000000000003197, 256.6193948016162381 ) ) ;
#56797 = EDGE_CURVE ( 'NONE', #1734, #57856, #60249, .T. ) ;
#56798 = CARTESIAN_POINT ( 'NONE',  ( -36.11269837220806522, 5.000000000000056843, 85.00100000000000477 ) ) ;
#56799 = CARTESIAN_POINT ( 'NONE',  ( -2.874437057892795355, 6.618922960888052209, 5.116205444759493126 ) ) ;
#56800 = CARTESIAN_POINT ( 'NONE',  ( 109.9975424824652634, 296.0000000000000000, 529.9060149868646477 ) ) ;
#56801 = CARTESIAN_POINT ( 'NONE',  ( -79.62207341875655686, 23.76621716825512109, 45.37247973810714541 ) ) ;
#56802 = CARTESIAN_POINT ( 'NONE',  ( 156.9739725704451985, 57.26595269248011988, 83.10889256476860965 ) ) ;
#56803 = CARTESIAN_POINT ( 'NONE',  ( 134.7770330630253284, 41.98246829846536343, 17.62339256512675689 ) ) ;
#56804 = VERTEX_POINT ( 'NONE', #1508 ) ;
#56805 = DIRECTION ( 'NONE',  ( 0.6427876096865403621, 0.7660444431189770143, 8.577375050694297349E-17 ) ) ;
#56806 = VECTOR ( 'NONE', #10009, 1000.000000000000000 ) ;
#56807 = DIRECTION ( 'NONE',  ( 0.000000000000000000, 0.000000000000000000, 1.000000000000000000 ) ) ;
#56808 = CARTESIAN_POINT ( 'NONE',  ( 45.90128843543708115, 9.343910238294478532, -46.89477593665989019 ) ) ;
#56809 = CARTESIAN_POINT ( 'NONE',  ( -76.58306521830746760, 22.61222690308086669, 84.39593471637930122 ) ) ;
#56810 = VECTOR ( 'NONE', #40136, 1000.000000000000000 ) ;
#56812 = ORIENTED_EDGE ( 'NONE', *, *, #51784, .T. ) ;
#56811 = FACE_OUTER_BOUND ( 'NONE', #2713, .T. ) ;
#56813 = CARTESIAN_POINT ( 'NONE',  ( 4.165045035620114966, 64.88046627338042072, 170.0000000000000000 ) ) ;
#56814 = ORIENTED_EDGE ( 'NONE', *, *, #29727, .F. ) ;
#56815 = ADVANCED_FACE ( 'NONE', ( #66251 ), #54612, .T. ) ;
#56816 = AXIS2_PLACEMENT_3D ( 'NONE', #33674, #66391, #18875 ) ;
#56817 = VECTOR ( 'NONE', #10216, 1000.000000000000114 ) ;
#56818 = ORIENTED_EDGE ( 'NONE', *, *, #14530, .F. ) ;
#56819 = CARTESIAN_POINT ( 'NONE',  ( -142.0062637385109952, 58.06920992247431457, 65.61584438720122137 ) ) ;
#56820 = CARTESIAN_POINT ( 'NONE',  ( 79.22872707466397912, 18.07970189365809688, 38.45465439937479601 ) ) ;
#56821 = CARTESIAN_POINT ( 'NONE',  ( 197.1974290009105459, 96.59277840252785552, -70.99450564134252772 ) ) ;
#56822 = EDGE_CURVE ( 'NONE', #135, #51413, #60599, .T. ) ;
#56824 = CARTESIAN_POINT ( 'NONE',  ( 188.0141161196706321, 85.90515114331884661, -13.99854441431428498 ) ) ;
#56823 = CIRCLE ( 'NONE', #68027, 10.00000000000000000 ) ;
#56825 = CARTESIAN_POINT ( 'NONE',  ( 445.3372781065085633, 217.8591479523844612, -111.4497041420119388 ) ) ;
#56826 = CARTESIAN_POINT ( 'NONE',  ( -85.66184035008926401, 26.20110535976566979, -13.05454194820700486 ) ) ;
#56827 = CARTESIAN_POINT ( 'NONE',  ( -173.9617926765114362, 89.58633395456783433, -7.902830288932056746 ) ) ;
#56828 = AXIS2_PLACEMENT_3D ( 'NONE', #55689, #54983, #1897 ) ;
#56829 = CARTESIAN_POINT ( 'NONE',  ( -48.71337292867757895, 14.10768470390589258, 41.83269798608346690 ) ) ;
#56830 = ORIENTED_EDGE ( 'NONE', *, *, #19397, .F. ) ;
#56831 = ORIENTED_EDGE ( 'NONE', *, *, #44105, .T. ) ;
#56832 = CARTESIAN_POINT ( 'NONE',  ( -107.7886332494339143, 36.81249801143971467, 16.28760631461256736 ) ) ;
#56833 = DIRECTION ( 'NONE',  ( 1.000000000000000000, 0.000000000000000000, -0.000000000000000000 ) ) ;
#56834 = CARTESIAN_POINT ( 'NONE',  ( 162.6190874793280159, 61.76782592053311305, 58.29531679009903655 ) ) ;
#56835 = CARTESIAN_POINT ( 'NONE',  ( -189.8071159312682994, 107.8771087123619878, 62.38726094205951256 ) ) ;
#56836 = CARTESIAN_POINT ( 'NONE',  ( 188.2076037774874635, 86.11782719225438143, -46.08847689396432656 ) ) ;
#56837 = DIRECTION ( 'NONE',  ( -1.000000000000000000, 0.000000000000000000, 0.000000000000000000 ) ) ;
#56838 = CARTESIAN_POINT ( 'NONE',  ( 163.1495034066983862, 62.20479872133083887, -65.54385288365227780 ) ) ;
#56839 = EDGE_LOOP ( 'NONE', ( #32608, #67605, #32367, #14513 ) ) ;
#56840 = ORIENTED_EDGE ( 'NONE', *, *, #13575, .T. ) ;
#56841 = ORIENTED_EDGE ( 'NONE', *, *, #23843, .F. ) ;
#56842 = CARTESIAN_POINT ( 'NONE',  ( -71.23432872518910131, 19.62839606228986256, 90.54878966649707195 ) ) ;
#56843 = FACE_OUTER_BOUND ( 'NONE', #18230, .T. ) ;
#56844 = CARTESIAN_POINT ( 'NONE',  ( 66.73594759725095571, 13.56641407806657007, -36.70390389039621937 ) ) ;
#56845 = CARTESIAN_POINT ( 'NONE',  ( 105.6615829231343042, -21.85840048673441771, -2.507220999339062839 ) ) ;
#56846 = CARTESIAN_POINT ( 'NONE',  ( -61.76386578474847511, 17.63453064612500754, 34.43260724535770123 ) ) ;
#56847 = CARTESIAN_POINT ( 'NONE',  ( -38.87871322265797858, 11.95691939779335300, -68.68042223677132085 ) ) ;
#56848 = PRODUCT_DEFINITION ( 'UNKNOWN', '', #57964, #53532 ) ;
#56849 = CARTESIAN_POINT ( 'NONE',  ( 55.52751777340356654, 12.08567914268658505, 37.80264004355908725 ) ) ;
#56850 = CARTESIAN_POINT ( 'NONE',  ( 44.25717266065687028, 9.090606898751403264, 85.37709734524574401 ) ) ;
#56851 =( NAMED_UNIT ( * ) PLANE_ANGLE_UNIT ( ) SI_UNIT ( $, .RADIAN. ) );
#56852 = VERTEX_POINT ( 'NONE', #43364 ) ;
#56853 = CARTESIAN_POINT ( 'NONE',  ( -2.190131154568196070, 6.589492063460818727, -47.87333299203348957 ) ) ;
#56854 = CARTESIAN_POINT ( 'NONE',  ( 447.3372781065086201, 370.0000000000043769, 108.5502958579838264 ) ) ;
#56855 = CARTESIAN_POINT ( 'NONE',  ( -119.5267374018686866, 42.44190186039715229, 15.27167418143519484 ) ) ;
#56856 = CYLINDRICAL_SURFACE ( 'NONE', #35383, 66.50000000000000000 ) ;
#56857 = CARTESIAN_POINT ( 'NONE',  ( 128.3856248084844935, 38.21741401878868771, -21.83233341589641796 ) ) ;
#56859 = EDGE_CURVE ( 'NONE', #67530, #11439, #1874, .T. ) ;
#56858 = CARTESIAN_POINT ( 'NONE',  ( -35.00000000000000000, 0.000000000000000000, 0.000000000000000000 ) ) ;
#56860 = CARTESIAN_POINT ( 'NONE',  ( 86.62931800182293784, -170.0000000000000000, 90.90118875340668581 ) ) ;
#56861 = EDGE_CURVE ( 'NONE', #8652, #61707, #61936, .T. ) ;
#56862 = VERTEX_POINT ( 'NONE', #38806 ) ;
#56863 = AXIS2_PLACEMENT_3D ( 'NONE', #46015, #29839, #26298 ) ;
#56864 = PRODUCT_CONTEXT ( 'NONE', #10707, 'mechanical' ) ;
#56865 = CARTESIAN_POINT ( 'NONE',  ( 127.4992165631961569, 38.87141012667722606, -47.53367025290549464 ) ) ;
#56866 = LINE ( 'NONE', #47322, #57862 ) ;
#56867 = CARTESIAN_POINT ( 'NONE',  ( 55.76286625948333864, 12.13284185313540142, -95.00000000000133582 ) ) ;
#56868 = CARTESIAN_POINT ( 'NONE',  ( 183.7875981612219505, 82.83906702837190039, -36.72598982284740998 ) ) ;
#56869 = VERTEX_POINT ( 'NONE', #32824 ) ;
#56870 = VECTOR ( 'NONE', #45260, 1000.000000000000000 ) ;
#56871 = AXIS2_PLACEMENT_3D ( 'NONE', #48183, #47848, #36968 ) ;
#56872 = AXIS2_PLACEMENT_3D ( 'NONE', #61773, #34019, #39639 ) ;
#56873 = EDGE_LOOP ( 'NONE', ( #62772, #35241, #67820, #15692 ) ) ;
#56875 = EDGE_CURVE ( 'NONE', #46890, #48257, #54966, .T. ) ;
#56874 = CARTESIAN_POINT ( 'NONE',  ( -28.81317668042940028, 9.175023678939290050, -23.00213673641785306 ) ) ;
#56876 = AXIS2_PLACEMENT_3D ( 'NONE', #741, #17254, #54177 ) ;
#56877 = CARTESIAN_POINT ( 'NONE',  ( 200.4590013143046860, 102.3556155835303088, 3.658552749324740727 ) ) ;
#56878 = ORIENTED_EDGE ( 'NONE', *, *, #2306, .F. ) ;
#56879 = VECTOR ( 'NONE', #60197, 1000.000000000000227 ) ;
#56880 = ADVANCED_FACE ( 'NONE', ( #49679 ), #44416, .T. ) ;
#56881 = CARTESIAN_POINT ( 'NONE',  ( 150.0666142602886168, 53.35666697496139932, 89.34269639003078112 ) ) ;
#56882 = VERTEX_POINT ( 'NONE', #65899 ) ;
#56883 = CARTESIAN_POINT ( 'NONE',  ( 126.4757069339777473, 38.29528077539269049, -71.72474436022167765 ) ) ;
#56884 = CARTESIAN_POINT ( 'NONE',  ( 128.0848616812662613, 38.04676222636084049, 41.82567121914378561 ) ) ;
#56885 = EDGE_CURVE ( 'NONE', #19020, #59151, #55314, .T. ) ;
#56886 = CARTESIAN_POINT ( 'NONE',  ( -41.21054189337212392, 41.29403905406989850, 27.58472369436602634 ) ) ;
#56887 = LINE ( 'NONE', #62850, #41575 ) ;
#56888 = CARTESIAN_POINT ( 'NONE',  ( 10.55634918610397577, -31.11269837220809364, 85.00100000000000477 ) ) ;
#56890 = ORIENTED_EDGE ( 'NONE', *, *, #13885, .F. ) ;
#56889 = DIRECTION ( 'NONE',  ( -0.000000000000000000, -0.000000000000000000, -1.000000000000000000 ) ) ;
#56891 = CARTESIAN_POINT ( 'NONE',  ( 56.30171512200999473, 11.21502580416395922, 40.66478564769037263 ) ) ;
#56892 = VERTEX_POINT ( 'NONE', #461 ) ;
#56893 = ORIENTED_EDGE ( 'NONE', *, *, #26299, .F. ) ;
#56894 = CARTESIAN_POINT ( 'NONE',  ( -165.7140086129056158, 80.68381997492572566, 10.26169782557952992 ) ) ;
#56895 = CARTESIAN_POINT ( 'NONE',  ( 21.88606409348644277, 6.772455198693823952, -74.23695490937706154 ) ) ;
#56897 = ORIENTED_EDGE ( 'NONE', *, *, #68516, .T. ) ;
#56896 = CARTESIAN_POINT ( 'NONE',  ( -127.4644500646575125, 48.74852676951795161, 57.62729058137536953 ) ) ;
#56898 = CARTESIAN_POINT ( 'NONE',  ( 109.9975424824652634, 20.00000000000003197, 536.6193948016162949 ) ) ;
#56899 = CARTESIAN_POINT ( 'NONE',  ( -71.42546113164834765, 20.75891408601218657, -40.59665863684374898 ) ) ;
#56900 = ORIENTED_EDGE ( 'NONE', *, *, #38759, .T. ) ;
#56901 = CARTESIAN_POINT ( 'NONE',  ( 212.0779786303466210, 118.9010947973413437, -72.04810227374618137 ) ) ;
#56902 = ADVANCED_FACE ( 'NONE', ( #21914 ), #59537, .T. ) ;
#56903 = DIRECTION ( 'NONE',  ( -0.000000000000000000, -0.000000000000000000, -1.000000000000000000 ) ) ;
#56904 = DIRECTION ( 'NONE',  ( -0.000000000000000000, -1.000000000000000000, 0.000000000000000000 ) ) ;
#56905 = CARTESIAN_POINT ( 'NONE',  ( -129.6079169496901784, 50.20899308323959787, 17.79538119927901718 ) ) ;
#56906 = CARTESIAN_POINT ( 'NONE',  ( 63.49941241090385802, 13.81848793187418423, -77.56524142263344856 ) ) ;
#56907 = ORIENTED_EDGE ( 'NONE', *, *, #60280, .T. ) ;
#56908 = EDGE_LOOP ( 'NONE', ( #14771, #65158, #27132, #51482 ) ) ;
#56909 = CIRCLE ( 'NONE', #28845, 65.00000000000000000 ) ;
#56910 = CARTESIAN_POINT ( 'NONE',  ( 8.678106553679038271, 7.383286152329689322, -94.17589882202238982 ) ) ;
#56911 = CARTESIAN_POINT ( 'NONE',  ( -39.55079474733702227, 51.59997227570980982, 170.0000000000000000 ) ) ;
#56912 = FACE_OUTER_BOUND ( 'NONE', #48117, .T. ) ;
#56913 = VECTOR ( 'NONE', #56929, 1000.000000000000000 ) ;
#56914 = CARTESIAN_POINT ( 'NONE',  ( -52.13778968636795241, 39.42540649521991014, 43.58025477438756212 ) ) ;
#56915 = CARTESIAN_POINT ( 'NONE',  ( 50.97490815085634352, 6.000000000000000000, -14.43565316649549679 ) ) ;
#56916 = DIRECTION ( 'NONE',  ( -0.5128992774059071280, 0.8584487936018656562, 2.500042656554809847E-16 ) ) ;
#56917 = ORIENTED_EDGE ( 'NONE', *, *, #24976, .T. ) ;
#56918 = CARTESIAN_POINT ( 'NONE',  ( 65.39792658623288446, 14.27332852928127949, -36.10495004355786364 ) ) ;
#56919 = PLANE ( 'NONE',  #22718 ) ;
#56920 = CARTESIAN_POINT ( 'NONE',  ( -166.5686015187717999, 80.11916873959174268, -65.39727901222690321 ) ) ;
#56921 = ORIENTED_EDGE ( 'NONE', *, *, #50561, .F. ) ;
#56922 = CARTESIAN_POINT ( 'NONE',  ( -109.6752351740181410, 37.84903014964772439, 39.29581709369001885 ) ) ;
#56923 = VERTEX_POINT ( 'NONE', #22270 ) ;
#56925 = AXIS2_PLACEMENT_3D ( 'NONE', #41064, #15364, #20290 ) ;
#56924 = CARTESIAN_POINT ( 'NONE',  ( -34.74740905761646559, 10.15745573515589228, 17.62056773612129135 ) ) ;
#56926 = PRESENTATION_STYLE_ASSIGNMENT (( #23528 ) ) ;
#56927 = ORIENTED_EDGE ( 'NONE', *, *, #6427, .T. ) ;
#56928 = CARTESIAN_POINT ( 'NONE',  ( 31.11269837220809364, 15.55634918610396866, 0.000000000000000000 ) ) ;
#56929 = DIRECTION ( 'NONE',  ( -0.5407162030609373726, -0.6444004775717706579, 0.5407162030609374836 ) ) ;
#56930 = CARTESIAN_POINT ( 'NONE',  ( 313.9975424824652350, 296.0000000000000000, 418.0000000000000000 ) ) ;
#56931 = FILL_AREA_STYLE_COLOUR ( '', #65308 ) ;
#56932 = CARTESIAN_POINT ( 'NONE',  ( 183.2136430849848239, 6.000000000000000000, -9.435653166495541200 ) ) ;
#56933 = CARTESIAN_POINT ( 'NONE',  ( -15.32495246574476155, 8.506829480038513580, -43.42002976355023947 ) ) ;
#56934 = ADVANCED_FACE ( 'NONE', ( #16976 ), #3941, .T. ) ;
#56935 = ORIENTED_EDGE ( 'NONE', *, *, #25327, .F. ) ;
#56936 = CYLINDRICAL_SURFACE ( 'NONE', #18503, 21.99999999999998579 ) ;
#56937 = ORIENTED_EDGE ( 'NONE', *, *, #29596, .F. ) ;
#56938 = CARTESIAN_POINT ( 'NONE',  ( -56.02358673658415000, 14.94347049174936792, 30.36477236479575126 ) ) ;
#56939 = CARTESIAN_POINT ( 'NONE',  ( -60.64199216239837398, 17.30050036439947547, 59.65478111955487606 ) ) ;
#56940 = FACE_OUTER_BOUND ( 'NONE', #43102, .T. ) ;
#56941 = ORIENTED_EDGE ( 'NONE', *, *, #16414, .F. ) ;
#56942 = CARTESIAN_POINT ( 'NONE',  ( 5.799999999999999822, 9.237604307034018802, 0.000000000000000000 ) ) ;
#56944 = EDGE_CURVE ( 'NONE', #64350, #54998, #43231, .T. ) ;
#56943 = CARTESIAN_POINT ( 'NONE',  ( -57.36093876233154276, 15.31244721770222306, -89.26622691136491028 ) ) ;
#56945 = CARTESIAN_POINT ( 'NONE',  ( -33.84080342750781512, 9.997552308299097135, 30.59459340086282353 ) ) ;
#56946 = CARTESIAN_POINT ( 'NONE',  ( 135.6651581599210203, 42.52720121194707303, -50.80564077755548169 ) ) ;
#56947 = EDGE_CURVE ( 'NONE', #41805, #53590, #14410, .T. ) ;
#56948 = ORIENTED_EDGE ( 'NONE', *, *, #6251, .T. ) ;
#56949 = EDGE_CURVE ( 'NONE', #35096, #31093, #24626, .T. ) ;
#56950 = LINE ( 'NONE', #14387, #39696 ) ;
#56951 = CARTESIAN_POINT ( 'NONE',  ( -20.55634918610403261, 2.818925648462311528E-14, 0.000000000000000000 ) ) ;
#56952 = FACE_OUTER_BOUND ( 'NONE', #43874, .T. ) ;
#56953 = EDGE_LOOP ( 'NONE', ( #29598, #19623 ) ) ;
#56954 = CARTESIAN_POINT ( 'NONE',  ( -178.5750994113944330, 94.98114813978523330, -74.22894033587822094 ) ) ;
#56955 = CARTESIAN_POINT ( 'NONE',  ( 130.5700081980325251, 40.64031760446221853, 83.95029887580108152 ) ) ;
#56956 = PRODUCT_DEFINITION_SHAPE ( 'NONE', 'NONE',  #53790 ) ;
#56957 = CARTESIAN_POINT ( 'NONE',  ( 115.7746371641014775, 31.52600568297706829, 42.19931404672254871 ) ) ;
#56958 = SURFACE_STYLE_FILL_AREA ( #67511 ) ;
#56959 = CIRCLE ( 'NONE', #33356, 24.99999999999985434 ) ;
#56960 = EDGE_CURVE ( 'NONE', #21528, #9719, #62335, .T. ) ;
#56961 = CARTESIAN_POINT ( 'NONE',  ( -118.4622862908118890, 41.79153065058245886, -68.21174534165025705 ) ) ;
#56962 = ORIENTED_EDGE ( 'NONE', *, *, #5307, .T. ) ;
#56963 = CARTESIAN_POINT ( 'NONE',  ( 200.4559562755961792, 100.7034888016685557, 30.50516796803767150 ) ) ;
#56964 = CARTESIAN_POINT ( 'NONE',  ( 112.5721302457195634, 29.97407549554797868, -63.12220954116383353 ) ) ;
#56965 = CARTESIAN_POINT ( 'NONE',  ( 70.50372867914782660, 14.53505678900967624, 64.64800341258842309 ) ) ;
#56966 = CARTESIAN_POINT ( 'NONE',  ( 141.0792860804899362, 47.16255757051794006, 8.074677092446195914 ) ) ;
#56967 = CARTESIAN_POINT ( 'NONE',  ( 311.9975424824652350, 20.00000000000003197, 254.5114349394235091 ) ) ;
#56968 = VECTOR ( 'NONE', #56099, 1000.000000000000000 ) ;
#56969 = ORIENTED_EDGE ( 'NONE', *, *, #68466, .F. ) ;
#56970 = AXIS2_PLACEMENT_3D ( 'NONE', #40232, #55355, #2260 ) ;
#56971 = CARTESIAN_POINT ( 'NONE',  ( 164.9547823171480161, 65.03046442419434925, -17.33931518955914441 ) ) ;
#56972 = EDGE_LOOP ( 'NONE', ( #62779, #23404, #26017, #15974 ) ) ;
#56973 = AXIS2_PLACEMENT_3D ( 'NONE', #43802, #17428, #22715 ) ;
#56974 = DIRECTION ( 'NONE',  ( -0.000000000000000000, 1.000000000000000000, -0.000000000000000000 ) ) ;
#56975 = CARTESIAN_POINT ( 'NONE',  ( 133.3039865199672533, 41.09165617245334801, 83.21332837341623190 ) ) ;
#56977 = VERTEX_POINT ( 'NONE', #46401 ) ;
#56976 = LINE ( 'NONE', #52034, #38792 ) ;
#56978 = CARTESIAN_POINT ( 'NONE',  ( 159.2325040199866919, 60.31699144791974732, -36.27868694413073314 ) ) ;
#56979 = FACE_BOUND ( 'NONE', #39133, .T. ) ;
#56980 = CARTESIAN_POINT ( 'NONE',  ( 162.0835148203877054, 61.32844276806159911, -49.55681444341564656 ) ) ;
#56981 = ORIENTED_EDGE ( 'NONE', *, *, #5076, .T. ) ;
#56982 = CARTESIAN_POINT ( 'NONE',  ( 218.0000000000000000, 126.6235316737731296, 94.99999999999866418 ) ) ;
#56983 = CARTESIAN_POINT ( 'NONE',  ( -130.5740389938243311, 49.65308610043483384, 44.00008722492239599 ) ) ;
#56984 = CARTESIAN_POINT ( 'NONE',  ( 34.43940527065477397, -66.63700071734618291, 170.0000000000000000 ) ) ;
#56985 = CARTESIAN_POINT ( 'NONE',  ( 86.62931800182293784, 20.48449268398422518, -23.97701360844805407 ) ) ;
#56986 = CARTESIAN_POINT ( 'NONE',  ( -172.3057147739577033, 86.22480007276998037, 30.85461157478519212 ) ) ;
#56987 = LINE ( 'NONE', #52051, #53619 ) ;
#56988 = LINE ( 'NONE', #25679, #41710 ) ;
#56989 = ORIENTED_EDGE ( 'NONE', *, *, #19381, .T. ) ;
#56990 = CARTESIAN_POINT ( 'NONE',  ( -95.21085197937826194, 30.44372064875430439, 67.42056744027632931 ) ) ;
#56991 = CARTESIAN_POINT ( 'NONE',  ( -10.24974837193995469, 8.069704751038631940, 71.57424783662469281 ) ) ;
#56992 = ORIENTED_EDGE ( 'NONE', *, *, #27629, .T. ) ;
#56993 = CARTESIAN_POINT ( 'NONE',  ( 152.8373718734504791, 55.38925997611394791, -10.86163724592964819 ) ) ;
#56994 = CARTESIAN_POINT ( 'NONE',  ( 422.4999999999999432, -17.50000000000000000, 1.999999999999998224 ) ) ;
#56995 = CARTESIAN_POINT ( 'NONE',  ( 103.0004140566503423, 26.76634862952792915, 39.12544781792537663 ) ) ;
#56996 = EDGE_CURVE ( 'NONE', #14102, #35061, #55668, .T. ) ;
#56997 = CARTESIAN_POINT ( 'NONE',  ( -1.328627985309864146, 7.561890325089883014, 33.86022777313294085 ) ) ;
#56998 = VECTOR ( 'NONE', #8856, 1000.000000000000000 ) ;
#56999 = CARTESIAN_POINT ( 'NONE',  ( 62.71028589264315656, 12.60192304540389863, 83.50116889568769807 ) ) ;
#57000 = CARTESIAN_POINT ( 'NONE',  ( 10.01137213834966921, -64.59476928204590251, 41.38025477438755928 ) ) ;
#57001 = DIRECTION ( 'NONE',  ( -0.000000000000000000, -0.000000000000000000, 1.000000000000000000 ) ) ;
#57002 = LINE ( 'NONE', #13737, #60163 ) ;
#57003 = CARTESIAN_POINT ( 'NONE',  ( -57.42615654242917600, 15.33060010148602714, 18.09145754529776084 ) ) ;
#57004 = VERTEX_POINT ( 'NONE', #62603 ) ;
#57005 = VECTOR ( 'NONE', #49813, 1000.000000000000000 ) ;
#57006 = FACE_OUTER_BOUND ( 'NONE', #55575, .T. ) ;
#57007 = ORIENTED_EDGE ( 'NONE', *, *, #28276, .T. ) ;
#57008 = DIRECTION ( 'NONE',  ( 1.000000000000000000, -0.000000000000000000, 0.000000000000000000 ) ) ;
#57009 = DIRECTION ( 'NONE',  ( 0.8890122540821405739, 0.000000000000000000, 0.4578834044730072383 ) ) ;
#57010 = VECTOR ( 'NONE', #19384, 1000.000000000000000 ) ;
#57011 = FACE_OUTER_BOUND ( 'NONE', #42542, .T. ) ;
#57012 = DIRECTION ( 'NONE',  ( -0.000000000000000000, -1.000000000000000000, -0.000000000000000000 ) ) ;
#57013 = CARTESIAN_POINT ( 'NONE',  ( -2.533432677019553658, 6.603837116479292391, 85.96053544918321165 ) ) ;
#57014 =( GEOMETRIC_REPRESENTATION_CONTEXT ( 3 ) GLOBAL_UNCERTAINTY_ASSIGNED_CONTEXT ( ( #35994 ) ) GLOBAL_UNIT_ASSIGNED_CONTEXT ( ( #33878, #1878, #18382 ) ) REPRESENTATION_CONTEXT ( 'NONE', 'WORKASPACE' ) );
#57015 = LINE ( 'NONE', #61923, #24343 ) ;
#57016 = ORIENTED_EDGE ( 'NONE', *, *, #66990, .T. ) ;
#57018 = AXIS2_PLACEMENT_3D ( 'NONE', #32404, #11622, #65103 ) ;
#57017 = CARTESIAN_POINT ( 'NONE',  ( 61.01080120047389244, 13.24737680938180695, -89.67107551088051309 ) ) ;
#57019 = CARTESIAN_POINT ( 'NONE',  ( -165.6212796729685408, 79.15047440262053158, 64.85932769107682816 ) ) ;
#57020 = ORIENTED_EDGE ( 'NONE', *, *, #22542, .T. ) ;
#57021 = ORIENTED_EDGE ( 'NONE', *, *, #26622, .F. ) ;
#57023 = ADVANCED_FACE ( 'NONE', ( #25318, #20033 ), #58005, .F. ) ;
#57022 = CARTESIAN_POINT ( 'NONE',  ( -154.2585856850055279, 68.31650218414627318, 32.41269129084507483 ) ) ;
#57024 = CARTESIAN_POINT ( 'NONE',  ( 157.4703587214989398, -170.0000000000000000, -16.77963370867396975 ) ) ;
#57025 = CARTESIAN_POINT ( 'NONE',  ( 8.904582680623983393, 23.36040254969773144, 0.000000000000000000 ) ) ;
#57026 = CARTESIAN_POINT ( 'NONE',  ( 55.00000000000000000, 19.01593100277521131, 6.196318915105386793 ) ) ;
#57027 = AXIS2_PLACEMENT_3D ( 'NONE', #22030, #38554, #11461 ) ;
#57028 = CARTESIAN_POINT ( 'NONE',  ( -59.42430146430427840, 27.22983999535709998, 3.125053320693569132E-16 ) ) ;
#57029 = EDGE_CURVE ( 'NONE', #35032, #8968, #17431, .T. ) ;
#57030 = CARTESIAN_POINT ( 'NONE',  ( 55.91494169499917177, 12.16343363043255899, -13.94887811350051798 ) ) ;
#57031 = EDGE_LOOP ( 'NONE', ( #21558, #23295, #15166, #32612 ) ) ;
#57032 = DIRECTION ( 'NONE',  ( 0.000000000000000000, 0.000000000000000000, -1.000000000000000000 ) ) ;
#57033 = ORIENTED_EDGE ( 'NONE', *, *, #31675, .T. ) ;
#57034 = CARTESIAN_POINT ( 'NONE',  ( 211.0967808702091304, 115.5516932918877586, 5.941490033705162155 ) ) ;
#57035 = CARTESIAN_POINT ( 'NONE',  ( 9.275903038161098735, 7.385619229189523516, 68.11142882406396382 ) ) ;
#57036 = CARTESIAN_POINT ( 'NONE',  ( 211.5066273949819333, 116.1727691518061505, 33.51412873826703986 ) ) ;
#57037 = CARTESIAN_POINT ( 'NONE',  ( 8.000000000000007105, 249.8719672152120381, 0.000000000000000000 ) ) ;
#57038 = B_SPLINE_CURVE_WITH_KNOTS ( 'NONE', 3,
 ( #37964, #43577, #41949, #28098, #20835, #9945, #17188, #1030, #22480, #38660, #42296, #17552, #63757, #22831, #44271, #65755, #59408, #11220, #39020, #60464, #32686, #12278, #63412, #55177, #7000, #47215, #68673, #31401, #61840, #51314, #1727, #34787, #34093, #66808, #2768, #40055, #24235, #35120, #40395, #55527, #56226, #45682, #7358, #50605, #18247, #23879, #8042 ),
 .UNSPECIFIED., .F., .F.,
 ( 4, 2, 2, 2, 2, 2, 2, 2, 2, 2, 2, 1, 2, 2, 2, 2, 2, 2, 2, 2, 2, 2, 2, 4 ),
 ( 0.000000000000000000, 0.003297771944419005796, 0.004122214930523721357, 0.004946657916628437353, 0.006595543888837858068, 0.007419986874942590543, 0.008244429861047323019, 0.009068872847152055494, 0.009893315833256787969, 0.01154220180546625119, 0.01236664479157098366, 0.01319108777767571614, 0.01401553076378044688, 0.01483997374988517762, 0.01566441673598990836, 0.01648885972209463910, 0.01813774569430405201, 0.01896218868040878622, 0.01978663166651352043, 0.02061107465261825464, 0.02143551763872298885, 0.02308440361093245380, 0.02473328958314192222, 0.02638217555535139064 ),
 .UNSPECIFIED. ) ;
#57039 = EDGE_CURVE ( 'NONE', #8739, #37319, #8793, .T. ) ;
#57040 = VERTEX_POINT ( 'NONE', #26002 ) ;
#57041 = ORIENTED_EDGE ( 'NONE', *, *, #55834, .F. ) ;
#57042 = CARTESIAN_POINT ( 'NONE',  ( 111.9975424824652634, 295.8720703627916464, 535.5371946177799600 ) ) ;
#57043 = CARTESIAN_POINT ( 'NONE',  ( -132.3448531020190160, 52.12286071311145719, 87.93207172015587503 ) ) ;
#57044 = CARTESIAN_POINT ( 'NONE',  ( 32.30062460741315533, 8.603096374765343057, -72.38972614245851389 ) ) ;
#57045 = CARTESIAN_POINT ( 'NONE',  ( -50.00000000000001421, 19.99999999999996447, 2.000000000000015543 ) ) ;
#57046 = CARTESIAN_POINT ( 'NONE',  ( 18.37289129162609314, 6.596424546175636117, 84.13215553489163767 ) ) ;
#57047 = CARTESIAN_POINT ( 'NONE',  ( 79.11678624235125312, 16.99307331934756604, -70.15752560060720100 ) ) ;
#57048 = CIRCLE ( 'NONE', #6474, 74.95140232871122521 ) ;
#57049 = ORIENTED_EDGE ( 'NONE', *, *, #21990, .F. ) ;
#57050 = FACE_OUTER_BOUND ( 'NONE', #25170, .T. ) ;
#57051 = FACE_OUTER_BOUND ( 'NONE', #46630, .T. ) ;
#57052 = ORIENTED_EDGE ( 'NONE', *, *, #9525, .F. ) ;
#57053 = CARTESIAN_POINT ( 'NONE',  ( -12.50000000000000000, 207.5000000000000284, 1.999999999999998224 ) ) ;
#57054 = ORIENTED_EDGE ( 'NONE', *, *, #66286, .T. ) ;
#57055 = DIRECTION ( 'NONE',  ( 0.6234898018587431423, -0.7818314824680220321, 0.000000000000000000 ) ) ;
#57056 = CARTESIAN_POINT ( 'NONE',  ( 394.5137675702981710, 500.0000000000000000, 0.000000000000000000 ) ) ;
#57057 =( REPRESENTATION_RELATIONSHIP ('NONE','NONE', #40274, #60409 ) REPRESENTATION_RELATIONSHIP_WITH_TRANSFORMATION ( #35635 )SHAPE_REPRESENTATION_RELATIONSHIP( ) );
#57058 = ORIENTED_EDGE ( 'NONE', *, *, #51929, .F. ) ;
#57059 = VECTOR ( 'NONE', #29098, 1000.000000000000000 ) ;
#57060 = ORIENTED_EDGE ( 'NONE', *, *, #12915, .T. ) ;
#57061 = CARTESIAN_POINT ( 'NONE',  ( 14.80582440982707659, 6.470883766728822373, -35.56753452839079443 ) ) ;
#57062 = CARTESIAN_POINT ( 'NONE',  ( -109.6064662507157266, 37.81086785902052583, -94.52989562943487556 ) ) ;
#57063 = VECTOR ( 'NONE', #20200, 1000.000000000000000 ) ;
#57064 = CARTESIAN_POINT ( 'NONE',  ( 0.000000000000000000, 0.000000000000000000, 40.00000000000003553 ) ) ;
#57065 = EDGE_LOOP ( 'NONE', ( #35447, #4168, #40702 ) ) ;
#57066 = CARTESIAN_POINT ( 'NONE',  ( -30.17641273894449938, 9.386748470934174193, 83.98431897038294380 ) ) ;
#57067 = CARTESIAN_POINT ( 'NONE',  ( -51.34542473642582650, 14.75635007918829267, 4.448568100648282453 ) ) ;
#57068 = DIRECTION ( 'NONE',  ( 1.000000000000000000, 0.000000000000000000, -0.000000000000000000 ) ) ;
#57069 = CARTESIAN_POINT ( 'NONE',  ( 105.8203563788590600, 26.88901185006198702, -37.36032832094576150 ) ) ;
#57070 = CARTESIAN_POINT ( 'NONE',  ( -30.95355748062276291, 9.511738996772320931, 30.21645440618916112 ) ) ;
#57071 = CARTESIAN_POINT ( 'NONE',  ( 0.000000000000000000, 0.000000000000000000, 41.38025477438755928 ) ) ;
#57072 = EDGE_LOOP ( 'NONE', ( #38746, #21811, #5041, #14119 ) ) ;
#57073 = VERTEX_POINT ( 'NONE', #51354 ) ;
#57074 = CARTESIAN_POINT ( 'NONE',  ( 0.7145311798163198613, -4.618802153516998743, 7.999999999999998224 ) ) ;
#57075 = CARTESIAN_POINT ( 'NONE',  ( 116.5873858943359807, 31.92924745533265352, -93.09020542203545290 ) ) ;
#57076 = CARTESIAN_POINT ( 'NONE',  ( -20.00000000000002842, -6.319444444444441089, 0.000000000000000000 ) ) ;
#57077 = EDGE_CURVE ( 'NONE', #11859, #48814, #62239, .T. ) ;
#57078 = CARTESIAN_POINT ( 'NONE',  ( -430.1627218934915504, 399.9999999999998863, -123.9497041420119530 ) ) ;
#57079 = CARTESIAN_POINT ( 'NONE',  ( 138.7884383316737171, 44.48287833083414000, -91.54775918821466973 ) ) ;
#57080 = CARTESIAN_POINT ( 'NONE',  ( -53.17301625261200826, -40.17754262171835933, 34.48241823999801881 ) ) ;
#57081 = CARTESIAN_POINT ( 'NONE',  ( 200.7511827984944830, 102.7381817183304804, 84.01209064570359430 ) ) ;
#57082 = CARTESIAN_POINT ( 'NONE',  ( 212.0075063341773500, 118.7912820769029167, 34.99884505030436088 ) ) ;
#57083 = CARTESIAN_POINT ( 'NONE',  ( -68.11501976657856972, 31.41506934893843805, 170.0000000000000000 ) ) ;
#57084 = PLANE ( 'NONE',  #45496 ) ;
#57086 = EDGE_LOOP ( 'NONE', ( #57280, #67806 ) ) ;
#57085 = EDGE_CURVE ( 'NONE', #23953, #55398, #56976, .T. ) ;
#57087 = CARTESIAN_POINT ( 'NONE',  ( 8.767814708128311096, 7.383611927972575373, -18.82455866429043922 ) ) ;
#57088 = ORIENTED_EDGE ( 'NONE', *, *, #5859, .T. ) ;
#57089 = CARTESIAN_POINT ( 'NONE',  ( 200.4559562755961224, 100.7034888016685272, -23.18393321288967002 ) ) ;
#57090 = ORIENTED_EDGE ( 'NONE', *, *, #53199, .T. ) ;
#57091 = CARTESIAN_POINT ( 'NONE',  ( -10.00000000000000178, 35.26862320190615208, -5.000000000000000000 ) ) ;
#57092 = CARTESIAN_POINT ( 'NONE',  ( 188.4374648754671568, 87.87346242052443301, -72.07443739198600952 ) ) ;
#57093 = CARTESIAN_POINT ( 'NONE',  ( -143.7133518487516710, 60.70463114991426323, 69.83424584982832073 ) ) ;
#57094 = CARTESIAN_POINT ( 'NONE',  ( 38.91493890549796930, 8.346224043800599901, -50.61981746542777927 ) ) ;
#57095 = CARTESIAN_POINT ( 'NONE',  ( -15.55634918610403439, 5.000000000000028422, 0.000000000000000000 ) ) ;
#57096 = CARTESIAN_POINT ( 'NONE',  ( 12.91653430408660697, 7.431946598423015082, -49.96024699054583351 ) ) ;
#57097 = CARTESIAN_POINT ( 'NONE',  ( 130.3245512970360380, 39.33195360491890114, -36.89023367850691670 ) ) ;
#57098 = ORIENTED_EDGE ( 'NONE', *, *, #35119, .F. ) ;
#57099 = EDGE_CURVE ( 'NONE', #68971, #43782, #35862, .T. ) ;
#57100 = ORIENTED_EDGE ( 'NONE', *, *, #61796, .T. ) ;
#57101 = EDGE_CURVE ( 'NONE', #36484, #41593, #30061, .T. ) ;
#57102 = B_SPLINE_CURVE_WITH_KNOTS ( 'NONE', 3,
 ( #68663, #4991, #47537, #22116 ),
 .UNSPECIFIED., .F., .F.,
 ( 4, 4 ),
 ( 0.1259919275528357807, 0.1829744153748745217 ),
 .UNSPECIFIED. ) ;
#57103 = VECTOR ( 'NONE', #45083, 1000.000000000000114 ) ;
#57104 = FACE_OUTER_BOUND ( 'NONE', #45919, .T. ) ;
#57105 = DIRECTION ( 'NONE',  ( -0.000000000000000000, -0.000000000000000000, -1.000000000000000000 ) ) ;
#57106 = DIRECTION ( 'NONE',  ( -0.000000000000000000, 0.000000000000000000, -1.000000000000000000 ) ) ;
#57107 = CIRCLE ( 'NONE', #24533, 4.999999999999996447 ) ;
#57108 = UNCERTAINTY_MEASURE_WITH_UNIT (LENGTH_MEASURE( 1.000000000000000082E-05 ), #63074, 'distance_accuracy_value', 'NONE');
#57109 = EDGE_CURVE ( 'NONE', #8643, #24463, #37925, .T. ) ;
#57110 = CARTESIAN_POINT ( 'NONE',  ( 13.37820144534468980, 6.435512790162279728, 17.77664207586528988 ) ) ;
#57111 = CIRCLE ( 'NONE', #33519, 4.999999999999990230 ) ;
#57112 = CARTESIAN_POINT ( 'NONE',  ( 284.7429971699386329, 21.94267019860760470, -1.616224894600692297 ) ) ;
#57113 = DIRECTION ( 'NONE',  ( 1.000000000000000000, 0.000000000000000000, 0.000000000000000000 ) ) ;
#57114 = CARTESIAN_POINT ( 'NONE',  ( 15.78827728214693416, 7.507518794609589818, -77.36349468914950478 ) ) ;
#57115 =( NAMED_UNIT ( * ) PLANE_ANGLE_UNIT ( ) SI_UNIT ( $, .RADIAN. ) );
#57116 = CARTESIAN_POINT ( 'NONE',  ( 274.9997958498912567, -22.00004639774357074, -0.3283548106454412530 ) ) ;
#57117 = CARTESIAN_POINT ( 'NONE',  ( 87.10668362745094839, 19.58396519288862336, -23.97701360844806118 ) ) ;
#57118 = CARTESIAN_POINT ( 'NONE',  ( 444.9999999999999432, 225.0000000000000000, -2.000000000000000000 ) ) ;
#57119 = DIRECTION ( 'NONE',  ( -0.000000000000000000, 1.000000000000000000, -0.000000000000000000 ) ) ;
#57120 = CARTESIAN_POINT ( 'NONE',  ( -50.13771638889894433, 13.41835215703894058, 70.34807068584244405 ) ) ;
#57121 = EDGE_CURVE ( 'NONE', #68876, #59075, #59371, .T. ) ;
#57122 = CARTESIAN_POINT ( 'NONE',  ( -102.0721892947742049, 32.67541014876152161, -88.70367844590329298 ) ) ;
#57123 = VERTEX_POINT ( 'NONE', #10152 ) ;
#57124 = DIRECTION ( 'NONE',  ( -0.000000000000000000, 1.000000000000000000, -0.000000000000000000 ) ) ;
#57125 = CARTESIAN_POINT ( 'NONE',  ( 155.2992895652387801, 57.24699634758577815, 56.56127440692515052 ) ) ;
#57126 = FACE_OUTER_BOUND ( 'NONE', #9898, .T. ) ;
#57127 = CARTESIAN_POINT ( 'NONE',  ( -47.95468448182521115, 12.89252559348046034, -40.28134454572786893 ) ) ;
#57128 = EDGE_CURVE ( 'NONE', #13740, #22362, #992, .T. ) ;
#57129 = DIRECTION ( 'NONE',  ( 0.000000000000000000, 0.000000000000000000, 1.000000000000000000 ) ) ;
#57130 = EDGE_CURVE ( 'NONE', #22437, #51470, #53391, .T. ) ;
#57131 = DIRECTION ( 'NONE',  ( -0.000000000000000000, -0.000000000000000000, -1.000000000000000000 ) ) ;
#57132 = EDGE_CURVE ( 'NONE', #43717, #23495, #59025, .T. ) ;
#57133 = B_SPLINE_CURVE_WITH_KNOTS ( 'NONE', 3,
 ( #69279, #27395, #38303, #6297, #38659, #39018, #55526, #23188, #33739, #49189, #6646, #33396, #23535, #55176, #34450, #54825, #29152, #18245, #34786, #1726, #12983, #40054, #39358, #65398, #13329, #50260, #11923, #65754, #60801, #1371, #43916, #56223, #6998, #45323, #22829, #17186, #55887, #12628, #44270, #7357, #28451, #61510, #22478 ),
 .UNSPECIFIED., .F., .F.,
 ( 4, 2, 2, 2, 2, 2, 2, 2, 2, 2, 2, 2, 1, 2, 2, 2, 2, 2, 2, 2, 2, 4 ),
 ( 0.02390068823634509954, 0.02538837671117071676, 0.02613222094858352537, 0.02687606518599633398, 0.02836375366082196856, 0.02985144213564760313, 0.03059528637306042909, 0.03133913061047325505, 0.03282681908529891390, 0.03431450756012457970, 0.03580219603495024550, 0.03654604027236307839, 0.03728988450977591129, 0.03803372874718874419, 0.03877757298460157015, 0.04026526145942722901, 0.04175294993425288093, 0.04324063840907853978, 0.04398448264649136574, 0.04472832688390419170, 0.04621601535872983668, 0.04770370383355547472 ),
 .UNSPECIFIED. ) ;
#57134 = EDGE_LOOP ( 'NONE', ( #20242, #32666, #16321, #54749, #16017, #64596, #2191, #43024, #10439, #50409, #63331, #7927, #27459, #48777, #68553, #50564, #23322, #2230, #39645, #7077 ) ) ;
#57135 = FILL_AREA_STYLE ('',( #35682 ) ) ;
#57136 = DIRECTION ( 'NONE',  ( -0.2225209339563041788, -0.9749279121818259508, 0.000000000000000000 ) ) ;
#57137 = VERTEX_POINT ( 'NONE', #59710 ) ;
#57138 = VERTEX_POINT ( 'NONE', #63642 ) ;
#57139 = CARTESIAN_POINT ( 'NONE',  ( 10.55634918610403084, -3.079134169858832593E-14, 0.000000000000000000 ) ) ;
#57140 = CARTESIAN_POINT ( 'NONE',  ( -180.0175713311536754, 95.14770835574077523, -72.01836099242309785 ) ) ;
#57141 = DIRECTION ( 'NONE',  ( -0.000000000000000000, -0.000000000000000000, -1.000000000000000000 ) ) ;
#57142 = ORIENTED_EDGE ( 'NONE', *, *, #18682, .T. ) ;
#57143 = DIRECTION ( 'NONE',  ( 0.000000000000000000, -1.000000000000000000, 0.000000000000000000 ) ) ;
#57144 = CARTESIAN_POINT ( 'NONE',  ( 26.11269837220803325, -15.55634918610409656, 85.00100000000000477 ) ) ;
#57145 = CARTESIAN_POINT ( 'NONE',  ( 4.165045035620114966, 64.88046627338042072, 170.0000000000000000 ) ) ;
#57146 = DIRECTION ( 'NONE',  ( 0.5128992774059071280, -0.8584487936018656562, 5.102127870520019688E-18 ) ) ;
#57147 = CARTESIAN_POINT ( 'NONE',  ( -85.66184035008927822, 26.20110535976568045, 40.63455923272034909 ) ) ;
#57148 = DIRECTION ( 'NONE',  ( 0.000000000000000000, 0.000000000000000000, 1.000000000000000000 ) ) ;
#57149 = CARTESIAN_POINT ( 'NONE',  ( -190.4966031023458868, 108.8421921967459127, 42.59989763244942651 ) ) ;
#57150 = ORIENTED_EDGE ( 'NONE', *, *, #56066, .T. ) ;
#57151 = CARTESIAN_POINT ( 'NONE',  ( 109.7782172510783170, 29.77507867835876709, -24.07788697519002241 ) ) ;
#57152 = DIRECTION ( 'NONE',  ( -0.8118923937861950435, -0.5838071093367415143, 0.000000000000000000 ) ) ;
#57153 = CARTESIAN_POINT ( 'NONE',  ( 39.89571693415784637, 8.473773298340391946, -35.61981746542776506 ) ) ;
#57154 = VECTOR ( 'NONE', #978, 1000.000000000000000 ) ;
#57155 = CARTESIAN_POINT ( 'NONE',  ( 112.3013380801408232, 388.0000000000077307, 101.0502958579874644 ) ) ;
#57157 = ORIENTED_EDGE ( 'NONE', *, *, #6323, .T. ) ;
#57156 = FACE_OUTER_BOUND ( 'NONE', #55628, .T. ) ;
#57158 = CARTESIAN_POINT ( 'NONE',  ( 133.8566784816069060, 41.42467568809810530, -77.86786152285937135 ) ) ;
#57159 = EDGE_LOOP ( 'NONE', ( #55889, #55421, #4249, #43123 ) ) ;
#57160 = AXIS2_PLACEMENT_3D ( 'NONE', #66094, #49884, #44614 ) ;
#57161 = ORIENTED_EDGE ( 'NONE', *, *, #37409, .T. ) ;
#57162 = CARTESIAN_POINT ( 'NONE',  ( -11.01093400780220932, -22.58090174195397992, 0.000000000000000000 ) ) ;
#57163 = CARTESIAN_POINT ( 'NONE',  ( 0.000000000000000000, 0.000000000000000000, 41.38025477438755928 ) ) ;
#57164 = FACE_BOUND ( 'NONE', #55939, .T. ) ;
#57165 = CARTESIAN_POINT ( 'NONE',  ( 55.14772863908675049, -34.40534879854660488, 40.00000000000003553 ) ) ;
#57166 = DIRECTION ( 'NONE',  ( 1.000000000000000000, 0.000000000000000000, -0.000000000000000000 ) ) ;
#57167 = CARTESIAN_POINT ( 'NONE',  ( 89.99999999999998579, 0.000000000000000000, -10.00000000000000000 ) ) ;
#57168 = CARTESIAN_POINT ( 'NONE',  ( -2.609024107869115977E-14, 3.000000000000030198, -46.99999999999997158 ) ) ;
#57169 = ADVANCED_FACE ( 'NONE', ( #32313 ), #58677, .F. ) ;
#57170 = CARTESIAN_POINT ( 'NONE',  ( -149.5074843970971017, 64.17983161892347255, -34.81283053149196149 ) ) ;
#57171 = ORIENTED_EDGE ( 'NONE', *, *, #37145, .T. ) ;
#57172 = VERTEX_POINT ( 'NONE', #32995 ) ;
#57173 = CARTESIAN_POINT ( 'NONE',  ( -108.9444157621018263, 37.44493815491210853, 14.65362961424871813 ) ) ;
#57174 = CARTESIAN_POINT ( 'NONE',  ( 108.3819860115547158, 28.02992728837241287, 56.67516201583306668 ) ) ;
#57175 = CARTESIAN_POINT ( 'NONE',  ( 109.0263699319888957, 28.32214139819616960, 83.37130228228382123 ) ) ;
#57176 = CARTESIAN_POINT ( 'NONE',  ( 432.4999999999999432, -18.06806526123148160, 0.000000000000000000 ) ) ;
#57177 = CARTESIAN_POINT ( 'NONE',  ( -62.31345272479909880, 18.49415068377641447, 170.0000000000000000 ) ) ;
#57178 = CARTESIAN_POINT ( 'NONE',  ( 0.000000000000000000, 6.928203230275505220, -4.000000000000007994 ) ) ;
#57179 = CARTESIAN_POINT ( 'NONE',  ( 160.9241720448059425, 60.38677655937337363, -63.79514627286779671 ) ) ;
#57180 = ORIENTED_EDGE ( 'NONE', *, *, #41691, .F. ) ;
#57181 = EDGE_CURVE ( 'NONE', #68312, #43775, #39898, .T. ) ;
#57182 = VERTEX_POINT ( 'NONE', #54431 ) ;
#57183 = ADVANCED_FACE ( 'NONE', ( #32647 ), #69239, .F. ) ;
#57184 = ORIENTED_EDGE ( 'NONE', *, *, #40760, .F. ) ;
#57185 = ADVANCED_FACE ( 'NONE', ( #15779 ), #11807, .T. ) ;
#57186 = DIRECTION ( 'NONE',  ( -1.000000000000000000, 0.000000000000000000, 0.000000000000000000 ) ) ;
#57187 = CARTESIAN_POINT ( 'NONE',  ( -82.32931163805226049, 23.75065981441938234, 58.21357082001073024 ) ) ;
#57188 = FACE_OUTER_BOUND ( 'NONE', #20368, .T. ) ;
#57189 = CARTESIAN_POINT ( 'NONE',  ( 106.5117512545002825, 27.19336236623133374, -90.59354463606661056 ) ) ;
#57190 = ADVANCED_FACE ( 'NONE', ( #50224 ), #8002, .F. ) ;
#57191 = DIRECTION ( 'NONE',  ( 0.000000000000000000, -1.000000000000000000, 0.000000000000000000 ) ) ;
#57192 = CARTESIAN_POINT ( 'NONE',  ( -31.43908319763709969, 10.61114334766717171, -62.16174795566551836 ) ) ;
#57193 = VECTOR ( 'NONE', #68488, 1000.000000000000000 ) ;
#57194 = CARTESIAN_POINT ( 'NONE',  ( 32.15641333221389431, 7.577415570152254531, 66.21096673341479288 ) ) ;
#57195 = CARTESIAN_POINT ( 'NONE',  ( 46.79315560871277313, 9.486230672254121643, 92.53801376008529189 ) ) ;
#57196 = VERTEX_POINT ( 'NONE', #2047 ) ;
#57197 = CARTESIAN_POINT ( 'NONE',  ( 24.91130694661015710, -3.250319586706349018, 3.061616997868437868E-16 ) ) ;
#57198 = CARTESIAN_POINT ( 'NONE',  ( 183.3913492984168272, 80.96922346472078402, 56.51364387551240043 ) ) ;
#57199 = CARTESIAN_POINT ( 'NONE',  ( -123.6619986853277879, 45.04188181212060016, 18.43930124660816716 ) ) ;
#57200 = CARTESIAN_POINT ( 'NONE',  ( 3.678442866637813759E-12, -65.13282190615278466, 5.000000000000000000 ) ) ;
#57201 = CARTESIAN_POINT ( 'NONE',  ( 0.000000000000000000, 0.000000000000000000, 40.00000000000003553 ) ) ;
#57202 = CARTESIAN_POINT ( 'NONE',  ( 23.28845814680231996, 7.864847136539609096, -16.66102632038655429 ) ) ;
#57203 = CARTESIAN_POINT ( 'NONE',  ( 198.8687991397275994, 98.67887821384411495, 58.82597387875455297 ) ) ;
#57204 = EDGE_LOOP ( 'NONE', ( #51626, #3923, #4565, #20973, #560, #13102, #5500, #64378 ) ) ;
#57205 = APPLICATION_PROTOCOL_DEFINITION ( 'draft international standard', 'automotive_design', 1998, #44409 ) ;
#57206 = CARTESIAN_POINT ( 'NONE',  ( 129.5225439633634608, 40.02995148249141977, -49.66244657560051223 ) ) ;
#57207 = CARTESIAN_POINT ( 'NONE',  ( -126.3508039230932525, 46.79479538767113667, -34.91370389823391207 ) ) ;
#57208 = ADVANCED_FACE ( 'NONE', ( #17866 ), #39667, .T. ) ;
#57209 = CARTESIAN_POINT ( 'NONE',  ( 444.9999999999999432, -35.00000000000000000, 0.000000000000000000 ) ) ;
#57210 = EDGE_CURVE ( 'NONE', #12795, #30189, #20821, .T. ) ;
#57211 = CONTEXT_DEPENDENT_SHAPE_REPRESENTATION ( #19342, #33821 ) ;
#57212 = CARTESIAN_POINT ( 'NONE',  ( 185.1710994180821785, 84.30654632312743502, -37.42057970017137336 ) ) ;
#57213 = ORIENTED_EDGE ( 'NONE', *, *, #48506, .F. ) ;
#57214 = ORIENTED_EDGE ( 'NONE', *, *, #38759, .F. ) ;
#57215 = ADVANCED_FACE ( 'NONE', ( #28410 ), #7320, .T. ) ;
#57216 = PLANE ( 'NONE',  #58339 ) ;
#57217 = DIRECTION ( 'NONE',  ( 1.000000000000000000, 0.000000000000000000, 0.000000000000000000 ) ) ;
#57218 = ORIENTED_EDGE ( 'NONE', *, *, #61959, .T. ) ;
#57219 = CARTESIAN_POINT ( 'NONE',  ( 164.8776669336225780, 64.96501004561835657, 89.40796121432521204 ) ) ;
#57220 = ORIENTED_EDGE ( 'NONE', *, *, #10333, .F. ) ;
#57221 = CARTESIAN_POINT ( 'NONE',  ( -60.66101049381767751, 17.30588917955502026, 15.97642707013661045 ) ) ;
#57222 = CARTESIAN_POINT ( 'NONE',  ( 447.3372781065085633, 217.8591479523844612, -111.4497041420119388 ) ) ;
#57223 = CARTESIAN_POINT ( 'NONE',  ( -156.1477286774994013, 71.38742644140633331, 41.71781464117591298 ) ) ;
#57224 = AXIS2_PLACEMENT_3D ( 'NONE', #56197, #45991, #46327 ) ;
#57225 = AXIS2_PLACEMENT_3D ( 'NONE', #18243, #39704, #56573 ) ;
#57226 = CARTESIAN_POINT ( 'NONE',  ( -96.45845418068302024, 29.92035703021964821, 33.26432808515374973 ) ) ;
#57227 = DIRECTION ( 'NONE',  ( 1.000000000000000000, 0.000000000000000000, 0.000000000000000000 ) ) ;
#57229 = ORIENTED_EDGE ( 'NONE', *, *, #24622, .F. ) ;
#57228 = DIRECTION ( 'NONE',  ( 0.000000000000000000, 6.123233995736761105E-17, -1.000000000000000000 ) ) ;
#57230 = CARTESIAN_POINT ( 'NONE',  ( -21.27554331372911278, -61.43430442924894663, 43.58025477438756923 ) ) ;
#57231 = EDGE_LOOP ( 'NONE', ( #67357, #5766, #7163, #44119, #1412, #33292, #62491, #41845, #46358 ) ) ;
#57232 = EDGE_LOOP ( 'NONE', ( #20219, #51872, #19475, #37809 ) ) ;
#57233 = CARTESIAN_POINT ( 'NONE',  ( 175.5429257635131250, 74.57009623370765894, 41.88879822895370353 ) ) ;
#57234 = CARTESIAN_POINT ( 'NONE',  ( 19.75784582661441391, 6.660183274347811100, -63.49536201651760337 ) ) ;
#57236 = VERTEX_POINT ( 'NONE', #23147 ) ;
#57235 = CARTESIAN_POINT ( 'NONE',  ( -126.8016613879753294, 48.30316697011515004, 72.42301449268042290 ) ) ;
#57237 = CARTESIAN_POINT ( 'NONE',  ( -447.6627218934913230, 399.9999999999997726, 83.55029585798818914 ) ) ;
#57238 = AXIS2_PLACEMENT_3D ( 'NONE', #14671, #51623, #57245 ) ;
#57239 = DIRECTION ( 'NONE',  ( 0.000000000000000000, 1.000000000000000000, -0.000000000000000000 ) ) ;
#57240 = ORIENTED_EDGE ( 'NONE', *, *, #44624, .F. ) ;
#57241 = CARTESIAN_POINT ( 'NONE',  ( 204.6977192012829789, 108.0580384837234789, -36.32593103262158252 ) ) ;
#57242 = CARTESIAN_POINT ( 'NONE',  ( 136.7690435008550764, 44.39743995805023502, 30.09502234337038118 ) ) ;
#57243 = EDGE_CURVE ( 'NONE', #61254, #60730, #62861, .T. ) ;
#57244 = DIRECTION ( 'NONE',  ( 0.000000000000000000, 0.000000000000000000, 1.000000000000000000 ) ) ;
#57245 = DIRECTION ( 'NONE',  ( 1.000000000000000000, 0.000000000000000000, -0.000000000000000000 ) ) ;
#57246 = LINE ( 'NONE', #68489, #21664 ) ;
#57247 = ORIENTED_EDGE ( 'NONE', *, *, #51003, .T. ) ;
#57248 = VECTOR ( 'NONE', #13887, 1000.000000000000114 ) ;
#57249 = ORIENTED_EDGE ( 'NONE', *, *, #33090, .T. ) ;
#57250 = CARTESIAN_POINT ( 'NONE',  ( -142.0070007485041117, 59.34878529741513375, -15.73778325578669524 ) ) ;
#57251 = PLANE ( 'NONE',  #19963 ) ;
#57252 = CARTESIAN_POINT ( 'NONE',  ( 0.000000000000000000, 0.000000000000000000, 43.58025477438756212 ) ) ;
#57253 = VECTOR ( 'NONE', #38511, 1000.000000000000000 ) ;
#57254 = B_SPLINE_CURVE_WITH_KNOTS ( 'NONE', 3,
 ( #51447, #46150, #41232, #41569, #57752, #2907, #13798, #29628, #29983, #19077, #19419, #9219, #35613, #25412, #30330, #40877, #61980, #51782, #4294, #51097, #35258, #67974, #9568, #68315, #3592, #31028, #25062, #19773, #35950, #57401, #62693, #14493, #52470, #20118, #30676, #52123, #68640, #46847, #56717, #8537, #63023, #14829, #34920, #36298 ),
 .UNSPECIFIED., .F., .F.,
 ( 4, 2, 2, 2, 2, 2, 2, 2, 2, 2, 2, 2, 2, 2, 2, 2, 2, 2, 2, 2, 2, 4 ),
 ( 0.02895403260893137515, 0.03071603688922228473, 0.03247804116951319431, 0.03424004544980410042, 0.03600204973009500653, 0.03776405401038591958, 0.03864505615053134835, 0.03952605829067677712, 0.04040706043082220589, 0.04128806257096763466, 0.04216906471111306343, 0.04305006685125849220, 0.04393106899140392096, 0.04481207113154934973, 0.04569307327169477850, 0.04657407541184020727, 0.04745507755198563604, 0.04833607969213106481, 0.05009808397242192235, 0.05186008825271277989, 0.05362209253300363743, 0.05714610109358538720 ),
 .UNSPECIFIED. ) ;
#57255 = CARTESIAN_POINT ( 'NONE',  ( -50.14405925094052918, 13.42012186841128418, -90.73077881499243347 ) ) ;
#57256 = DIRECTION ( 'NONE',  ( -0.000000000000000000, 0.000000000000000000, -1.000000000000000000 ) ) ;
#57257 = CARTESIAN_POINT ( 'NONE',  ( 16.78635691501517613, 6.000000000000000000, -41.68900338898716740 ) ) ;
#57258 = CARTESIAN_POINT ( 'NONE',  ( 70.26936813788616121, 15.51386666370915357, -45.19091827645912929 ) ) ;
#57259 = CARTESIAN_POINT ( 'NONE',  ( -28.32746765835526048, 69.45586423092609607, 170.0000000000000000 ) ) ;
#57260 = CARTESIAN_POINT ( 'NONE',  ( 209.4789161463551750, 113.1367444519304115, 57.76954579875279450 ) ) ;
#57261 = ADVANCED_FACE ( 'NONE', ( #25584 ), #67795, .F. ) ;
#57262 = ORIENTED_EDGE ( 'NONE', *, *, #51937, .T. ) ;
#57263 = DIRECTION ( 'NONE',  ( -0.000000000000000000, 0.000000000000000000, -1.000000000000000000 ) ) ;
#57264 = VERTEX_POINT ( 'NONE', #24548 ) ;
#57265 = CARTESIAN_POINT ( 'NONE',  ( -37.79601571721867259, 10.72155118426296205, 14.85940810243080534 ) ) ;
#57266 = FILL_AREA_STYLE ('',( #14358 ) ) ;
#57267 = EDGE_CURVE ( 'NONE', #67476, #44138, #67451, .T. ) ;
#57268 = ORIENTED_EDGE ( 'NONE', *, *, #24718, .T. ) ;
#57269 = CARTESIAN_POINT ( 'NONE',  ( -83.06245155374612921, 24.04494455745185633, -90.22407819767580861 ) ) ;
#57270 = B_SPLINE_CURVE_WITH_KNOTS ( 'NONE', 3,
 ( #14501, #68325, #10250, #37325, #15194, #25764, #46858, #58103, #47193, #9576, #20125, #20460, #20812, #68648, #31035, #36654, #67982, #46502, #41577, #41244, #4302, #14840, #36307, #41923, #47523, #9921, #62701, #35960, #57413, #30684, #64066, #58433, #42271, #9229, #63387, #57762, #52134, #31376, #52809, #4629, #26093, #3952, #30340, #21166, #3601, #25419 ),
 .UNSPECIFIED., .F., .F.,
 ( 4, 2, 2, 2, 2, 2, 2, 2, 2, 2, 2, 2, 2, 2, 2, 2, 2, 2, 2, 2, 2, 2, 4 ),
 ( 0.02420077021543439941, 0.02572112563160181692, 0.02648130333968554823, 0.02724148104776927953, 0.02876183646393674215, 0.02952201417202046652, 0.03028219188010418741, 0.03180254729627166044, 0.03332290271243912999, 0.03408308042052287518, 0.03484325812860662036, 0.03636361354477407604, 0.03712379125285780040, 0.03788396896094152477, 0.03864414666902524914, 0.03940432437710897351, 0.04092467979327645000, 0.04244503520944392649, 0.04396539062561140299, 0.04548574604177887948, 0.04624592374986261079, 0.04700610145794634903, 0.04852645687411386022 ),
 .UNSPECIFIED. ) ;
#57271 = LINE ( 'NONE', #41436, #7512 ) ;
#57272 = DIRECTION ( 'NONE',  ( 0.000000000000000000, 0.000000000000000000, 1.000000000000000000 ) ) ;
#57273 = ADVANCED_FACE ( 'NONE', ( #3085 ), #67120, .F. ) ;
#57274 = CARTESIAN_POINT ( 'NONE',  ( 37.46254810722764006, 8.164772623042704680, 3.307947441784442333 ) ) ;
#57275 = DIRECTION ( 'NONE',  ( -0.000000000000000000, 1.000000000000000000, -0.000000000000000000 ) ) ;
#57276 = AXIS2_PLACEMENT_3D ( 'NONE', #11999, #17623, #45748 ) ;
#57277 = DIRECTION ( 'NONE',  ( 0.000000000000000000, 1.000000000000000000, -0.000000000000000000 ) ) ;
#57278 = ORIENTED_EDGE ( 'NONE', *, *, #60993, .T. ) ;
#57279 = CARTESIAN_POINT ( 'NONE',  ( 99.99999999999997158, 6.000000000000000000, -25.00000000000000000 ) ) ;
#57280 = ORIENTED_EDGE ( 'NONE', *, *, #627, .F. ) ;
#57281 = CARTESIAN_POINT ( 'NONE',  ( -58.76006735892197952, 15.70681061434692616, 31.29311785761185050 ) ) ;
#57282 = CARTESIAN_POINT ( 'NONE',  ( -62.49137879463569334, 17.85440472148629709, 65.65172476684578839 ) ) ;
#57283 = CARTESIAN_POINT ( 'NONE',  ( 55.65793654284612302, 50.28674377798304107, 170.0000000000000000 ) ) ;
#57284 = FACE_OUTER_BOUND ( 'NONE', #23894, .T. ) ;
#57285 = CARTESIAN_POINT ( 'NONE',  ( -14.32241591711279938, 7.401556312061829956, -66.00773135621913923 ) ) ;
#57286 = CARTESIAN_POINT ( 'NONE',  ( -99.11448999425219597, 31.20120877265620152, -22.48539650098521392 ) ) ;
#57287 = VECTOR ( 'NONE', #23875, 1000.000000000000000 ) ;
#57288 = ORIENTED_EDGE ( 'NONE', *, *, #43529, .T. ) ;
#57289 = DIRECTION ( 'NONE',  ( -0.4127148655274870404, 0.9108602745606090290, 7.732827752419633099E-15 ) ) ;
#57290 = AXIS2_PLACEMENT_3D ( 'NONE', #54720, #1266, #12177 ) ;
#57291 = CARTESIAN_POINT ( 'NONE',  ( -154.6085044440278295, 69.98390342970667177, 59.56211392109398872 ) ) ;
#57292 = CARTESIAN_POINT ( 'NONE',  ( 175.8874477961783214, 74.89984466412599318, -11.45168165142409578 ) ) ;
#57293 = CARTESIAN_POINT ( 'NONE',  ( -122.8118341587045137, 44.49743491855734590, 31.26718143031790476 ) ) ;
#57294 = LINE ( 'NONE', #20009, #28792 ) ;
#57295 = ORIENTED_EDGE ( 'NONE', *, *, #54869, .T. ) ;
#57296 = CARTESIAN_POINT ( 'NONE',  ( -180.6158171975815776, 97.47361786002632300, -69.38088246809070370 ) ) ;
#57297 = CARTESIAN_POINT ( 'NONE',  ( 126.8027934882252339, 38.47872101784862053, 88.12645126614253854 ) ) ;
#57298 = EDGE_CURVE ( 'NONE', #54282, #33561, #40151, .T. ) ;
#57299 = CARTESIAN_POINT ( 'NONE',  ( 115.2288739107204378, 31.25773204386718263, 31.50320768227159007 ) ) ;
#57300 = DIRECTION ( 'NONE',  ( 0.000000000000000000, -1.000000000000000000, 0.000000000000000000 ) ) ;
#57301 = B_SPLINE_CURVE_WITH_KNOTS ( 'NONE', 3,
 ( #3773, #8723, #47359, #42098, #19966, #4127 ),
 .UNSPECIFIED., .F., .F.,
 ( 4, 2, 4 ),
 ( 1.095770181094175974E-06, 0.03239442681617710207, 0.06478775786217311206 ),
 .UNSPECIFIED. ) ;
#57302 = LINE ( 'NONE', #14725, #43618 ) ;
#57303 = EDGE_LOOP ( 'NONE', ( #29710, #40029, #27738, #17924, #63527, #2048, #65083 ) ) ;
#57304 = CARTESIAN_POINT ( 'NONE',  ( 157.4703587214989113, 57.65129005721576760, 29.40946747225336466 ) ) ;
#57305 = CARTESIAN_POINT ( 'NONE',  ( 112.5554747942045850, 29.96654954475020816, -77.40549949264581642 ) ) ;
#57306 = CARTESIAN_POINT ( 'NONE',  ( 188.4374648754671568, 87.87346242052444723, 35.30376496986874457 ) ) ;
#57307 = CARTESIAN_POINT ( 'NONE',  ( 181.0840389613909736, 78.60582251573003987, -89.91415884680696990 ) ) ;
#57308 = CARTESIAN_POINT ( 'NONE',  ( 264.4165763529819628, -27.00000000000000355, 108.9999999999999858 ) ) ;
#57309 = AXIS2_PLACEMENT_3D ( 'NONE', #31687, #25396, #31012 ) ;
#57310 = ORIENTED_EDGE ( 'NONE', *, *, #4674, .T. ) ;
#57311 = CARTESIAN_POINT ( 'NONE',  ( 157.9121974517528031, 59.27335488206247760, -24.27963370867398396 ) ) ;
#57312 = ORIENTED_EDGE ( 'NONE', *, *, #31365, .T. ) ;
#57313 = CARTESIAN_POINT ( 'NONE',  ( 0.000000000000000000, 0.000000000000000000, 0.000000000000000000 ) ) ;
#57314 = CARTESIAN_POINT ( 'NONE',  ( 141.2947372838333990, 46.10078095604043824, 91.72802395535696007 ) ) ;
#57316 = ORIENTED_EDGE ( 'NONE', *, *, #27889, .T. ) ;
#57315 = DIRECTION ( 'NONE',  ( 1.000000000000000000, 0.000000000000000000, 0.000000000000000000 ) ) ;
#57317 = CARTESIAN_POINT ( 'NONE',  ( -142.4991775570126151, 58.45550857435406300, -66.43273307728649968 ) ) ;
#57318 = CIRCLE ( 'NONE', #44957, 10.00000000000000000 ) ;
#57319 = CARTESIAN_POINT ( 'NONE',  ( -25.99999999999999289, 0.000000000000000000, -17.00000000000000711 ) ) ;
#57320 = LINE ( 'NONE', #36211, #41807 ) ;
#57321 = ORIENTED_EDGE ( 'NONE', *, *, #51700, .T. ) ;
#57322 = CARTESIAN_POINT ( 'NONE',  ( -94.83091526606381194, 30.26550147229322718, 10.15853931445705705 ) ) ;
#57323 = EDGE_CURVE ( 'NONE', #27253, #11718, #50029, .T. ) ;
#57324 = ADVANCED_FACE ( 'NONE', ( #5820 ), #59626, .T. ) ;
#57325 = CARTESIAN_POINT ( 'NONE',  ( -132.2199390322348620, 50.80243550247266882, 42.17967972708286339 ) ) ;
#57326 = CARTESIAN_POINT ( 'NONE',  ( 34.76618902119824384, -54.93755186520707667, 170.0000000000000000 ) ) ;
#57327 = CARTESIAN_POINT ( 'NONE',  ( 82.14396250120410059, 18.99560174459422157, -22.49292728426798860 ) ) ;
#57328 = EDGE_CURVE ( 'NONE', #44581, #57471, #39276, .T. ) ;
#57329 = CARTESIAN_POINT ( 'NONE',  ( -166.3188283541502699, 79.86268666707378827, 35.15081015259792707 ) ) ;
#57330 = CARTESIAN_POINT ( 'NONE',  ( 209.3223706822284100, 0.000000000000000000, 277.8007638641562380 ) ) ;
#57331 = CARTESIAN_POINT ( 'NONE',  ( 91.67776154311744108, 22.27748043241296116, 42.76395149726314315 ) ) ;
#57332 = ORIENTED_EDGE ( 'NONE', *, *, #66400, .F. ) ;
#57333 = DIRECTION ( 'NONE',  ( -0.000000000000000000, 1.000000000000000000, -0.000000000000000000 ) ) ;
#57334 = DIRECTION ( 'NONE',  ( -0.000000000000000000, -0.000000000000000000, 1.000000000000000000 ) ) ;
#57335 = VERTEX_POINT ( 'NONE', #68806 ) ;
#57336 = EDGE_CURVE ( 'NONE', #69014, #40747, #20622, .T. ) ;
#57337 = VECTOR ( 'NONE', #35030, 1000.000000000000000 ) ;
#57338 = DIRECTION ( 'NONE',  ( -1.000000000000000000, 0.000000000000000000, 0.000000000000000000 ) ) ;
#57339 = CARTESIAN_POINT ( 'NONE',  ( 211.4997502125519304, 118.0043045815490359, -20.15512624053809176 ) ) ;
#57340 = DIRECTION ( 'NONE',  ( 0.000000000000000000, 1.000000000000000000, 0.000000000000000000 ) ) ;
#57341 = CARTESIAN_POINT ( 'NONE',  ( -5.879983509979052947, 7.779504553499496211, 30.35576161878026014 ) ) ;
#57342 = CARTESIAN_POINT ( 'NONE',  ( -34.75846525698938194, -54.92585086258257121, 40.00000000000003553 ) ) ;
#57343 = LINE ( 'NONE', #4902, #16796 ) ;
#57344 = CARTESIAN_POINT ( 'NONE',  ( -60.00000000000000000, 0.000000000000000000, -5.000000000000000000 ) ) ;
#57345 = DIRECTION ( 'NONE',  ( 0.000000000000000000, 0.000000000000000000, 1.000000000000000000 ) ) ;
#57346 = VERTEX_POINT ( 'NONE', #63548 ) ;
#57347 = CARTESIAN_POINT ( 'NONE',  ( -51.82969867401513397, 54.20961478705410030, 0.000000000000000000 ) ) ;
#57348 = VERTEX_POINT ( 'NONE', #4796 ) ;
#57349 = CARTESIAN_POINT ( 'NONE',  ( 105.8022841538864469, 26.88074187880710753, -76.33012430075584120 ) ) ;
#57350 = EDGE_CURVE ( 'NONE', #29070, #62258, #47692, .T. ) ;
#57351 = CARTESIAN_POINT ( 'NONE',  ( 58.48209831743722731, 11.66636741727084825, -64.07070076514432344 ) ) ;
#57352 = EDGE_CURVE ( 'NONE', #57676, #62102, #12164, .T. ) ;
#57353 = CARTESIAN_POINT ( 'NONE',  ( -4.999999999999971578, 15.55634918610403084, 85.00100000000000477 ) ) ;
#57354 = CYLINDRICAL_SURFACE ( 'NONE', #16532, 30.00000000000000000 ) ;
#57355 = LINE ( 'NONE', #14447, #3032 ) ;
#57356 = DIRECTION ( 'NONE',  ( -0.000000000000000000, -0.000000000000000000, -1.000000000000000000 ) ) ;
#57357 = ORIENTED_EDGE ( 'NONE', *, *, #69324, .T. ) ;
#57358 = CARTESIAN_POINT ( 'NONE',  ( -76.32962633615589709, 21.44528079176262025, 57.63206797190907338 ) ) ;
#57359 = CARTESIAN_POINT ( 'NONE',  ( -166.5686015187718283, 80.11916873959170005, 68.82547394009152697 ) ) ;
#57360 = ORIENTED_EDGE ( 'NONE', *, *, #33608, .F. ) ;
#57361 = ORIENTED_EDGE ( 'NONE', *, *, #61006, .T. ) ;
#57362 = CARTESIAN_POINT ( 'NONE',  ( -154.6171773099879658, 68.63761944777705537, 43.71609283412200853 ) ) ;
#57363 = FACE_OUTER_BOUND ( 'NONE', #45291, .T. ) ;
#57364 = CARTESIAN_POINT ( 'NONE',  ( 177.2011275744679608, 74.76848439756739140, -23.30107000260681360 ) ) ;
#57365 = FACE_OUTER_BOUND ( 'NONE', #57822, .T. ) ;
#57366 = DIRECTION ( 'NONE',  ( 4.691548276051942630E-18, 2.005263967813518922E-18, -1.000000000000000000 ) ) ;
#57367 = AXIS2_PLACEMENT_3D ( 'NONE', #11145, #27669, #6572 ) ;
#57368 = VERTEX_POINT ( 'NONE', #66686 ) ;
#57369 = CARTESIAN_POINT ( 'NONE',  ( -55.05276343752910151, -170.0000000000000000, 3.472777182467474244 ) ) ;
#57370 = ORIENTED_EDGE ( 'NONE', *, *, #61066, .F. ) ;
#57371 = CARTESIAN_POINT ( 'NONE',  ( 210.9506883977752523, 115.3310071214937693, 5.713674614841949939 ) ) ;
#57372 = CARTESIAN_POINT ( 'NONE',  ( 9.689943677145722134, 7.388265075009366356, 59.98655866053932328 ) ) ;
#57373 = VECTOR ( 'NONE', #1317, 1000.000000000000000 ) ;
#57374 = CARTESIAN_POINT ( 'NONE',  ( 210.9747454890631957, 115.3673079504855821, 40.82073227286706896 ) ) ;
#57375 = CYLINDRICAL_SURFACE ( 'NONE', #17180, 243.4957430088094839 ) ;
#57376 = AXIS2_PLACEMENT_3D ( 'NONE', #18993, #19678, #30589 ) ;
#57377 = ORIENTED_EDGE ( 'NONE', *, *, #42307, .F. ) ;
#57378 = ORIENTED_EDGE ( 'NONE', *, *, #1044, .T. ) ;
#57379 = DIRECTION ( 'NONE',  ( -0.000000000000000000, -0.000000000000000000, -1.000000000000000000 ) ) ;
#57380 = CARTESIAN_POINT ( 'NONE',  ( -129.5122926757072719, 50.14302427363037395, 85.23333541525167334 ) ) ;
#57381 = CARTESIAN_POINT ( 'NONE',  ( 39.40195752203891999, 9.424259417798142024, -62.46436805589144114 ) ) ;
#57382 = DIRECTION ( 'NONE',  ( -0.000000000000000000, -1.000000000000000000, -0.000000000000000000 ) ) ;
#57383 = CARTESIAN_POINT ( 'NONE',  ( 23.10939849154102887, 6.845445181420994452, 92.86463421238133265 ) ) ;
#57384 = VECTOR ( 'NONE', #30201, 1000.000000000000114 ) ;
#57385 = CARTESIAN_POINT ( 'NONE',  ( 79.53408731553403754, 17.12082763744058767, -67.68499423098313628 ) ) ;
#57386 = ORIENTED_EDGE ( 'NONE', *, *, #65947, .F. ) ;
#57387 = FACE_OUTER_BOUND ( 'NONE', #45805, .T. ) ;
#57388 = CARTESIAN_POINT ( 'NONE',  ( 203.9203998321607969, 106.9845510704142271, -36.35590919959582834 ) ) ;
#57389 = ORIENTED_EDGE ( 'NONE', *, *, #6603, .F. ) ;
#57390 = CARTESIAN_POINT ( 'NONE',  ( -81.23297981660239486, 23.31577157498399089, 18.12494301450533385 ) ) ;
#57391 = VERTEX_POINT ( 'NONE', #54348 ) ;
#57392 = CARTESIAN_POINT ( 'NONE',  ( 394.5137675702982847, 500.0000000000001137, -91.64566090791306863 ) ) ;
#57393 = VERTEX_POINT ( 'NONE', #55406 ) ;
#57394 = ORIENTED_EDGE ( 'NONE', *, *, #43655, .T. ) ;
#57395 = CARTESIAN_POINT ( 'NONE',  ( 311.9975424824652350, 172.0000000000000284, 527.9060149868646477 ) ) ;
#57396 = CARTESIAN_POINT ( 'NONE',  ( -60.41792053122280493, 24.01035990323433822, 41.38025477438755928 ) ) ;
#57397 = LINE ( 'NONE', #18380, #35074 ) ;
#57398 = ORIENTED_EDGE ( 'NONE', *, *, #1761, .T. ) ;
#57399 = EDGE_CURVE ( 'NONE', #14754, #34394, #27633, .T. ) ;
#57400 = LINE ( 'NONE', #25061, #54781 ) ;
#57401 = CARTESIAN_POINT ( 'NONE',  ( 174.1348882614951776, 73.23561817543361485, -67.73415502738041027 ) ) ;
#57402 = EDGE_CURVE ( 'NONE', #23678, #24054, #29047, .T. ) ;
#57403 = CARTESIAN_POINT ( 'NONE',  ( 432.4999999999999432, -17.50000000000000000, 20.00000000000000000 ) ) ;
#57404 = DIRECTION ( 'NONE',  ( 0.000000000000000000, 0.000000000000000000, 1.000000000000000000 ) ) ;
#57405 = CARTESIAN_POINT ( 'NONE',  ( 84.74089592029042706, 19.84571403269344714, -50.58391462091437063 ) ) ;
#57406 = CARTESIAN_POINT ( 'NONE',  ( 110.2429982417149574, -170.0000000000000000, -9.077886975189999319 ) ) ;
#57407 = B_SPLINE_CURVE_WITH_KNOTS ( 'NONE', 3,
 ( #7057, #33794, #23936, #7421, #34847, #55233, #29549, #18663, #49600, #2141, #1433, #28515, #1796, #45385, #28872, #56283, #44696, #51017, #13386, #22888, #23593, #2826, #40454, #34508, #60520, #12337, #2480, #8099, #50323, #24295, #39414, #60862, #12686, #45031, #45737, #66515, #66864, #18307, #55949, #7764, #29213, #61899, #67216, #19002, #41499, #30949 ),
 .UNSPECIFIED., .F., .F.,
 ( 4, 2, 2, 2, 2, 2, 2, 2, 2, 2, 2, 2, 2, 2, 2, 2, 2, 2, 2, 2, 2, 2, 4 ),
 ( 3.103167691559091397E-17, 0.001572224531395634414, 0.003144449062791238036, 0.004716673594186841442, 0.006288898125582444848, 0.007861122656978048254, 0.009433347188373651659, 0.01021945945407147331, 0.01100557171976929496, 0.01179168398546711662, 0.01257779625116493827, 0.01415002078256057810, 0.01493613304825838935, 0.01572224531395620406, 0.01650835757965401704, 0.01729446984535183002, 0.01886669437674749761, 0.01965280664244534181, 0.02043891890814318255, 0.02201114343953889177, 0.02358336797093459752, 0.02436948023663241050, 0.02515559250233022348 ),
 .UNSPECIFIED. ) ;
#57408 = ORIENTED_EDGE ( 'NONE', *, *, #61218, .T. ) ;
#57409 = EDGE_CURVE ( 'NONE', #13226, #33133, #27980, .T. ) ;
#57410 = AXIS2_PLACEMENT_3D ( 'NONE', #6921, #5524, #64618 ) ;
#57411 = EDGE_LOOP ( 'NONE', ( #24595, #47932, #19946, #27349 ) ) ;
#57412 = DIRECTION ( 'NONE',  ( 0.000000000000000000, 0.000000000000000000, 1.000000000000000000 ) ) ;
#57413 = CARTESIAN_POINT ( 'NONE',  ( -85.90077524418998678, 26.30132018890136436, -67.46541528951036071 ) ) ;
#57415 = CARTESIAN_POINT ( 'NONE',  ( 173.6024011093110460, 72.73634049052009232, 9.360915578664817716 ) ) ;
#57414 = VECTOR ( 'NONE', #96, 1000.000000000000000 ) ;
#57416 = CARTESIAN_POINT ( 'NONE',  ( 39.99999999999996447, 29.79383981485516486, -79.99999999999998579 ) ) ;
#57417 = CARTESIAN_POINT ( 'NONE',  ( 60.82895951008428170, -30.68107831874537084, 170.0000000000000000 ) ) ;
#57418 = CARTESIAN_POINT ( 'NONE',  ( 107.3013380801407237, 395.0000000000010232, 96.05029585798752123 ) ) ;
#57419 = CARTESIAN_POINT ( 'NONE',  ( 32.89621043149783475, 7.652303554303282240, -93.07142327913575741 ) ) ;
#57420 = CARTESIAN_POINT ( 'NONE',  ( -121.2119672714299412, 44.67540322905998096, -63.37905527228651437 ) ) ;
#57422 = CARTESIAN_POINT ( 'NONE',  ( 212.0779786303465642, 118.9010947973413579, 35.33010008810850167 ) ) ;
#57421 = CIRCLE ( 'NONE', #27077, 21.02499999999999858 ) ;
#57423 = CIRCLE ( 'NONE', #27079, 25.12245591505646303 ) ;
#57424 = CARTESIAN_POINT ( 'NONE',  ( -78.18913509716431065, 22.13995206110505265, -61.96000122218156747 ) ) ;
#57425 = CARTESIAN_POINT ( 'NONE',  ( 13.24564585880038514, 63.65041531508843065, 170.0000000000000000 ) ) ;
#57426 = VERTEX_POINT ( 'NONE', #1966 ) ;
#57427 = ITEM_DEFINED_TRANSFORMATION ( 'NONE', 'NONE', #42195,  #66832 ) ;
#57428 = CARTESIAN_POINT ( 'NONE',  ( -62.50344214308532997, 17.85806481441974469, 90.58836406955566645 ) ) ;
#57429 = ORIENTED_EDGE ( 'NONE', *, *, #50363, .F. ) ;
#57430 = LINE ( 'NONE', #55425, #54262 ) ;
#57431 = ORIENTED_EDGE ( 'NONE', *, *, #65288, .T. ) ;
#57432 = EDGE_CURVE ( 'NONE', #54495, #43039, #24205, .T. ) ;
#57433 = CARTESIAN_POINT ( 'NONE',  ( -130.2647544212423725, 131.3624518482487247, 10.00000000000000000 ) ) ;
#57434 = CARTESIAN_POINT ( 'NONE',  ( 15.78827728214693416, 7.507518794609588042, 56.85925826316891829 ) ) ;
#57435 = CARTESIAN_POINT ( 'NONE',  ( -171.0950923142953854, 86.38958441093224394, 31.08788057152530016 ) ) ;
#57436 = CARTESIAN_POINT ( 'NONE',  ( 450.2085304802404266, 2.000000000000000000, 7.478223336038896996 ) ) ;
#57437 = CIRCLE ( 'NONE', #43898, 2.999999999999999112 ) ;
#57438 = FACE_OUTER_BOUND ( 'NONE', #63602, .T. ) ;
#57439 = CARTESIAN_POINT ( 'NONE',  ( 32.28603806442401236, 7.590310383548729334, -45.53980477190197007 ) ) ;
#57440 = PLANE ( 'NONE',  #45007 ) ;
#57441 = CARTESIAN_POINT ( 'NONE',  ( 13.36262230781615123, 7.441298897118797662, -35.90524268855146062 ) ) ;
#57442 = CARTESIAN_POINT ( 'NONE',  ( 126.8015497489690375, 37.32461426945041438, -46.08151831055564429 ) ) ;
#57443 = ORIENTED_EDGE ( 'NONE', *, *, #44466, .F. ) ;
#57444 = ORIENTED_EDGE ( 'NONE', *, *, #39192, .F. ) ;
#57445 = PLANE ( 'NONE',  #66435 ) ;
#57446 = SURFACE_STYLE_USAGE ( .BOTH. , #51485 ) ;
#57447 = CARTESIAN_POINT ( 'NONE',  ( -25.80058235236790054, 8.733375263008326783, -64.69209604585124396 ) ) ;
#57448 = CARTESIAN_POINT ( 'NONE',  ( 8.670103207226931730, 6.377073801252347351, 8.257049701868895752 ) ) ;
#57449 = CARTESIAN_POINT ( 'NONE',  ( 280.0000000000000000, 21.42428528562853884, -4.999999999999990230 ) ) ;
#57450 = ORIENTED_EDGE ( 'NONE', *, *, #50991, .F. ) ;
#57451 = DIRECTION ( 'NONE',  ( -0.000000000000000000, -6.405132834375902056E-16, 1.000000000000000000 ) ) ;
#57452 = CARTESIAN_POINT ( 'NONE',  ( 173.8575673535406452, 71.59843387604340137, -72.59740664150669431 ) ) ;
#57453 =( LENGTH_UNIT ( ) NAMED_UNIT ( * ) SI_UNIT ( .MILLI., .METRE. ) );
#57454 = CARTESIAN_POINT ( 'NONE',  ( -178.7483298110140026, 93.61800926271540391, -47.17654204188055900 ) ) ;
#57455 = CARTESIAN_POINT ( 'NONE',  ( 91.11342358617748971, 21.00000175105270372, -22.49380947096609518 ) ) ;
#57456 = CARTESIAN_POINT ( 'NONE',  ( -55.05276343752910151, -170.0000000000000000, -8.371773407996171201 ) ) ;
#57457 = CARTESIAN_POINT ( 'NONE',  ( 105.2647131865113295, 21.94130279673638384, 1.613668875657356283 ) ) ;
#57458 = B_SPLINE_CURVE_WITH_KNOTS ( 'NONE', 3,
 ( #48268, #53204, #9637, #20869, #42328, #31772, #26841, #4357 ),
 .UNSPECIFIED., .F., .F.,
 ( 4, 2, 2, 4 ),
 ( 0.004673709593152147908, 0.005837709341827639065, 0.007001709090503129354, 0.009329708587854111668 ),
 .UNSPECIFIED. ) ;
#57459 = FACE_OUTER_BOUND ( 'NONE', #48018, .T. ) ;
#57460 = APPLICATION_CONTEXT ( 'automotive_design' ) ;
#57461 = ORIENTED_EDGE ( 'NONE', *, *, #55104, .T. ) ;
#57462 = FACE_OUTER_BOUND ( 'NONE', #509, .T. ) ;
#57463 = VECTOR ( 'NONE', #27596, 1000.000000000000000 ) ;
#57464 = DIRECTION ( 'NONE',  ( 1.000000000000000000, -0.000000000000000000, -0.000000000000000000 ) ) ;
#57465 = CARTESIAN_POINT ( 'NONE',  ( -109.7643866341847314, 37.89854104106755273, -69.91044693626231776 ) ) ;
#57466 = CARTESIAN_POINT ( 'NONE',  ( -52.68007207639879397, 14.05813534436550682, -49.83524973432806604 ) ) ;
#57467 = FACE_BOUND ( 'NONE', #26676, .T. ) ;
#57468 = CARTESIAN_POINT ( 'NONE',  ( 290.0000000000000568, 5.000000000000000888, 21.42428528562853529 ) ) ;
#57469 = CIRCLE ( 'NONE', #41751, 10.00000000000000000 ) ;
#57470 = EDGE_CURVE ( 'NONE', #4530, #25239, #61726, .T. ) ;
#57471 = VERTEX_POINT ( 'NONE', #2650 ) ;
#57472 = DIRECTION ( 'NONE',  ( 0.000000000000000000, 0.000000000000000000, 1.000000000000000000 ) ) ;
#57473 = CARTESIAN_POINT ( 'NONE',  ( 41.66904755831212981, 20.55634918610394735, 2.000000000000001776 ) ) ;
#57474 = VERTEX_POINT ( 'NONE', #35705 ) ;
#57475 = CIRCLE ( 'NONE', #14790, 2.999999999999981792 ) ;
#57476 =( GEOMETRIC_REPRESENTATION_CONTEXT ( 3 ) GLOBAL_UNCERTAINTY_ASSIGNED_CONTEXT ( ( #57792 ) ) GLOBAL_UNIT_ASSIGNED_CONTEXT ( ( #15145, #36604, #58054 ) ) REPRESENTATION_CONTEXT ( 'NONE', 'WORKASPACE' ) );
#57477 = ORIENTED_EDGE ( 'NONE', *, *, #12155, .T. ) ;
#57478 = CARTESIAN_POINT ( 'NONE',  ( 177.2011275744679040, 74.76848439756736298, -50.14562059307051101 ) ) ;
#57479 = CARTESIAN_POINT ( 'NONE',  ( -180.4654253355436708, 95.69358270527507671, -70.60706783670912046 ) ) ;
#57480 = CARTESIAN_POINT ( 'NONE',  ( -36.11269837220812207, -26.11269837220801193, 0.000000000000000000 ) ) ;
#57481 = ORIENTED_EDGE ( 'NONE', *, *, #4654, .T. ) ;
#57482 = DIRECTION ( 'NONE',  ( 0.000000000000000000, -0.7071067811865475727, 0.7071067811865475727 ) ) ;
#57483 = DIRECTION ( 'NONE',  ( -0.7818314824680311359, 0.6234898018587318180, 2.500042656554809847E-16 ) ) ;
#57484 = LINE ( 'NONE', #43617, #46566 ) ;
#57485 = AXIS2_PLACEMENT_3D ( 'NONE', #3886, #36933, #68924 ) ;
#57486 = CARTESIAN_POINT ( 'NONE',  ( 61.09977118998601497, 13.26754120022606287, -50.47593651538998927 ) ) ;
#57487 = LINE ( 'NONE', #41313, #68552 ) ;
#57488 = CARTESIAN_POINT ( 'NONE',  ( -23.93895920923072040, 9.495000752338444983, -16.21472940711745281 ) ) ;
#57489 = CARTESIAN_POINT ( 'NONE',  ( 45.39413431650373809, 0.000000000000000000, -9.999999999999998224 ) ) ;
#57490 = ADVANCED_FACE ( 'NONE', ( #56811 ), #8630, .F. ) ;
#57491 = ORIENTED_EDGE ( 'NONE', *, *, #33914, .T. ) ;
#57492 = ADVANCED_FACE ( 'NONE', ( #29724 ), #59009, .T. ) ;
#57493 = LINE ( 'NONE', #20888, #57063 ) ;
#57494 = CARTESIAN_POINT ( 'NONE',  ( -41.50537345350632279, -50.04124777106357413, 170.0000000000000000 ) ) ;
#57495 = CARTESIAN_POINT ( 'NONE',  ( -26.50207385662995918, 9.849226639603651634, 32.04887038639355268 ) ) ;
#57496 = CARTESIAN_POINT ( 'NONE',  ( 199.3764470687682149, 100.9548044849099284, 41.99854440117639598 ) ) ;
#57497 = DIRECTION ( 'NONE',  ( 0.000000000000000000, 0.000000000000000000, 1.000000000000000000 ) ) ;
#57499 = EDGE_LOOP ( 'NONE', ( #59104, #63148, #38385, #34834 ) ) ;
#57498 = DIRECTION ( 'NONE',  ( -0.000000000000000000, -1.000000000000000000, -0.000000000000000000 ) ) ;
#57500 = CARTESIAN_POINT ( 'NONE',  ( 70.46579300139244140, 15.56614468937218909, 38.31143274373327046 ) ) ;
#57501 = ORIENTED_EDGE ( 'NONE', *, *, #62745, .F. ) ;
#57502 = EDGE_CURVE ( 'NONE', #31099, #28345, #40617, .T. ) ;
#57503 = VERTEX_POINT ( 'NONE', #67713 ) ;
#57504 = CARTESIAN_POINT ( 'NONE',  ( 112.5537757279407032, 31.07998172410696114, -63.11594588500084058 ) ) ;
#57505 = DIRECTION ( 'NONE',  ( -1.000000000000000000, 0.000000000000000000, -0.000000000000000000 ) ) ;
#57506 = FACE_BOUND ( 'NONE', #34596, .T. ) ;
#57507 = CARTESIAN_POINT ( 'NONE',  ( -38.88884187334146247, 11.95889603743729346, 63.56416379048864229 ) ) ;
#57508 = LINE ( 'NONE', #24811, #56775 ) ;
#57509 = DIRECTION ( 'NONE',  ( 0.000000000000000000, 1.000000000000000000, 0.000000000000000000 ) ) ;
#57510 = CARTESIAN_POINT ( 'NONE',  ( 200.0000000000000000, 0.000000000000000000, -10.00000000000000000 ) ) ;
#57511 = CARTESIAN_POINT ( 'NONE',  ( -50.52615126106341137, 14.55080735582892792, 31.81763226821556501 ) ) ;
#57512 = ORIENTED_EDGE ( 'NONE', *, *, #18743, .T. ) ;
#57513 = VERTEX_POINT ( 'NONE', #62778 ) ;
#57514 = EDGE_CURVE ( 'NONE', #22341, #34424, #64645, .T. ) ;
#57515 = PLANE ( 'NONE',  #64578 ) ;
#57516 = AXIS2_PLACEMENT_3D ( 'NONE', #5294, #48519, #10562 ) ;
#57517 = CARTESIAN_POINT ( 'NONE',  ( -85.35172689181705152, 26.07142112926218758, -46.05152394499496182 ) ) ;
#57518 = CARTESIAN_POINT ( 'NONE',  ( 115.0566045393160550, 31.17277249902146252, 85.01040373191897004 ) ) ;
#57520 = ADVANCED_FACE ( 'NONE', ( #62431 ), #29379, .F. ) ;
#57519 = CARTESIAN_POINT ( 'NONE',  ( -444.4229916354184979, 394.6798985497181889, -128.9497041420121093 ) ) ;
#57521 = ADVANCED_FACE ( 'NONE', ( #57156 ), #18825, .F. ) ;
#57522 = VECTOR ( 'NONE', #67204, 1000.000000000000000 ) ;
#57523 = CARTESIAN_POINT ( 'NONE',  ( 187.2354698746857764, 85.05376776489248414, -48.04494933370835241 ) ) ;
#57524 = CARTESIAN_POINT ( 'NONE',  ( -6.183861102004804070E-16, 9.237604307034020579, -9.500000000000000000 ) ) ;
#57525 = CARTESIAN_POINT ( 'NONE',  ( 157.9160637431159273, 57.99786926216935257, -62.96873488960130771 ) ) ;
#57526 = ORIENTED_EDGE ( 'NONE', *, *, #12497, .F. ) ;
#57527 = VERTEX_POINT ( 'NONE', #45905 ) ;
#57528 = ORIENTED_EDGE ( 'NONE', *, *, #61409, .T. ) ;
#57529 = AXIS2_PLACEMENT_3D ( 'NONE', #3877, #47809, #36923 ) ;
#57530 = VECTOR ( 'NONE', #28756, 1000.000000000000000 ) ;
#57531 = CARTESIAN_POINT ( 'NONE',  ( 0.000000000000000000, 0.000000000000000000, -2.499999999999970246 ) ) ;
#57532 = CARTESIAN_POINT ( 'NONE',  ( -17.90772993695118132, 72.84144224619132046, 43.58025477438756923 ) ) ;
#57533 = CARTESIAN_POINT ( 'NONE',  ( 69.49862690228275142, 14.27023134440514873, -47.02397500419540677 ) ) ;
#57534 = CARTESIAN_POINT ( 'NONE',  ( 74.39890044415652426, -7.951074708186081530, 41.38025477438755928 ) ) ;
#57535 = VECTOR ( 'NONE', #5901, 1000.000000000000227 ) ;
#57536 = CLOSED_SHELL ( 'NONE', ( #52521, #57324, #26442, #60915, #59800, #45273, #10960, #66572, #50205, #61468, #44133, #30328, #27709, #50825, #33030, #3559, #53200, #63894, #37408, #36053, #66792 ) ) ;
#57537 = CARTESIAN_POINT ( 'NONE',  ( -38.93847286785604211, 11.96870349976818737, -70.16847028595665847 ) ) ;
#57538 = PLANE ( 'NONE',  #8281 ) ;
#57539 = CARTESIAN_POINT ( 'NONE',  ( 183.7875981612220073, 82.83906702837188618, 70.65221253900733700 ) ) ;
#57540 = CARTESIAN_POINT ( 'NONE',  ( 10.83046137699561662, 6.392429922561257527, -10.52554053518067789 ) ) ;
#57541 = ORIENTED_EDGE ( 'NONE', *, *, #2634, .F. ) ;
#57542 = CARTESIAN_POINT ( 'NONE',  ( 16.27775141556968919, 7.523247835309962106, 3.170157082241546131 ) ) ;
#57543 = CARTESIAN_POINT ( 'NONE',  ( 181.5127080940606845, 79.03904173130084132, 71.15314469597512925 ) ) ;
#57544 = CARTESIAN_POINT ( 'NONE',  ( -118.4063383664800000, 41.75753822095644097, 11.78578461217687590 ) ) ;
#57545 = DIRECTION ( 'NONE',  ( -0.000000000000000000, -0.000000000000000000, -1.000000000000000000 ) ) ;
#57546 = DIRECTION ( 'NONE',  ( -0.000000000000000000, -0.000000000000000000, 1.000000000000000000 ) ) ;
#57547 = CARTESIAN_POINT ( 'NONE',  ( 20.74185656603722094, 7.717159106492277765, -21.82745635861012445 ) ) ;
#57548 = CARTESIAN_POINT ( 'NONE',  ( 9.819093282782493048, 7.389085782749407194, 15.23728359609124894 ) ) ;
#57549 = ORIENTED_EDGE ( 'NONE', *, *, #22814, .F. ) ;
#57550 = CARTESIAN_POINT ( 'NONE',  ( 188.4389256074243804, 86.37278721358585187, 11.46150878901021919 ) ) ;
#57551 = APPLICATION_PROTOCOL_DEFINITION ( 'draft international standard', 'automotive_design', 1998, #19240 ) ;
#57552 = LINE ( 'NONE', #13599, #68895 ) ;
#57553 = LINE ( 'NONE', #30471, #54472 ) ;
#57554 = CARTESIAN_POINT ( 'NONE',  ( -109.7790042512817905, 37.90666514836943435, -42.80576273198390425 ) ) ;
#57555 = CARTESIAN_POINT ( 'NONE',  ( 26.11269837220803325, -15.55634918610409656, 0.000000000000000000 ) ) ;
#57556 = ORIENTED_EDGE ( 'NONE', *, *, #17114, .F. ) ;
#57557 = EDGE_CURVE ( 'NONE', #59365, #14479, #68401, .T. ) ;
#57558 = ORIENTED_EDGE ( 'NONE', *, *, #32326, .T. ) ;
#57559 = CARTESIAN_POINT ( 'NONE',  ( -31.11269837220806878, 5.594483210025202879E-14, 85.00100000000000477 ) ) ;
#57560 = CARTESIAN_POINT ( 'NONE',  ( 31.11269837220812562, 36.11269837220800838, 0.000000000000000000 ) ) ;
#57561 = ORIENTED_EDGE ( 'NONE', *, *, #33124, .T. ) ;
#57562 = ADVANCED_FACE ( 'NONE', ( #34675 ), #67373, .F. ) ;
#57563 = CARTESIAN_POINT ( 'NONE',  ( 116.8937673311173029, 32.08228998570056234, 60.48004562628608483 ) ) ;
#57564 = B_SPLINE_CURVE_WITH_KNOTS ( 'NONE', 3,
 ( #4801, #26265, #51959, #31886, #46677, #47355, #52642, #53316, #68153, #20628, #31541, #68812, #36826, #36131, #63211, #62522, #47697, #47028, #63895, #41752, #58264, #15014, #4466, #69162, #58600, #36477, #19962, #10417, #35791, #57929, #30505, #26607, #41413, #48046, #10083, #14667, #19600, #14336, #57590, #9401, #30858, #52304, #4122, #25592, #6179, #59633, #33631 ),
 .UNSPECIFIED., .F., .F.,
 ( 4, 2, 2, 2, 2, 2, 2, 2, 2, 2, 2, 2, 1, 2, 2, 2, 2, 2, 2, 2, 2, 2, 2, 4 ),
 ( 7.152448122690996019E-18, 0.001493793014771594959, 0.002240689522157387776, 0.002987586029543181244, 0.004481379044314751266, 0.005228275551700536927, 0.005975172059086323456, 0.007468965073857915596, 0.008215861581243707329, 0.008962758088629495593, 0.01045655110340106171, 0.01120344761078684304, 0.01195034411817262089, 0.01269724062555839007, 0.01344413713294415752, 0.01493793014771570456, 0.01568482665510148935, 0.01643172316248727241, 0.01792551617725884894, 0.01941930919203042200, 0.02016620569941620159, 0.02091310220680198464, 0.02240689522157354382, 0.02390068823634510300 ),
 .UNSPECIFIED. ) ;
#57565 = ORIENTED_EDGE ( 'NONE', *, *, #25885, .T. ) ;
#57566 = CARTESIAN_POINT ( 'NONE',  ( 126.3580464630938991, 38.22944795020838171, -70.66847772514068993 ) ) ;
#57567 = DIRECTION ( 'NONE',  ( 0.000000000000000000, 0.000000000000000000, -1.000000000000000000 ) ) ;
#57568 = LINE ( 'NONE', #9378, #51054 ) ;
#57569 = AXIS2_PLACEMENT_3D ( 'NONE', #34737, #7990, #56519 ) ;
#57570 = CARTESIAN_POINT ( 'NONE',  ( -94.89192151156323973, 29.18342430963128464, 36.70293385600623282 ) ) ;
#57571 = CYLINDRICAL_SURFACE ( 'NONE', #21493, 10.00000000000000178 ) ;
#57572 = VECTOR ( 'NONE', #7335, 1000.000000000000000 ) ;
#57574 = VERTEX_POINT ( 'NONE', #67036 ) ;
#57573 = LINE ( 'NONE', #9383, #30860 ) ;
#57575 = EDGE_CURVE ( 'NONE', #32966, #48407, #9305, .T. ) ;
#57576 = CARTESIAN_POINT ( 'NONE',  ( 110.2429982417149432, 29.99119854320847267, -24.07788697519002596 ) ) ;
#57578 = ORIENTED_EDGE ( 'NONE', *, *, #36205, .F. ) ;
#57577 = B_SPLINE_CURVE_WITH_KNOTS ( 'NONE', 3,
 ( #52451, #56340, #8156, #27087, #4951, #21810, #11253, #8, #42583, #48522, #31346, #52774, #54149, #37644, #36969, #16193, #43255, #58744, #353, #59094, #5974, #32381, #10566, #64734, #26068, #63704, #15514, #10910, #53807, #32725, #5631, #32034, #63354, #53465, #4602, #59440, #58075, #717, #47496, #15164, #27433, #15848, #16543 ),
 .UNSPECIFIED., .F., .F.,
 ( 4, 2, 2, 2, 2, 2, 2, 2, 2, 2, 2, 2, 1, 2, 2, 2, 2, 2, 2, 2, 2, 4 ),
 ( 0.02371951416048008118, 0.02520633211177541674, 0.02594974108742306371, 0.02669315006307071067, 0.02817996801436600113, 0.02966678596566128812, 0.03041019494130892814, 0.03115360391695656470, 0.03264042186825183434, 0.03412723981954710745, 0.03561405777084238056, 0.03635746674649002752, 0.03710087572213767448, 0.03784428469778532145, 0.03858769367343296841, 0.04007451162472827622, 0.04156132957602358402, 0.04304814752731889183, 0.04379155650296655267, 0.04453496547861421351, 0.04602178342990952825, 0.04750860138120484299 ),
 .UNSPECIFIED. ) ;
#57579 = VECTOR ( 'NONE', #19995, 1000.000000000000000 ) ;
#57581 = VERTEX_POINT ( 'NONE', #19868 ) ;
#57580 = EDGE_CURVE ( 'NONE', #22806, #35973, #46583, .T. ) ;
#57582 = CARTESIAN_POINT ( 'NONE',  ( -171.5023337025455703, 86.83681590836891928, 4.142432042481735799 ) ) ;
#57583 = CARTESIAN_POINT ( 'NONE',  ( -180.6213815675304772, 95.88446356933845038, -15.67696249584733437 ) ) ;
#57584 = EDGE_CURVE ( 'NONE', #22014, #66758, #57917, .T. ) ;
#57586 = ORIENTED_EDGE ( 'NONE', *, *, #42926, .T. ) ;
#57585 = CARTESIAN_POINT ( 'NONE',  ( 6.933333333333328241, 8.000000000000000000, -11.86666666666666536 ) ) ;
#57587 = CARTESIAN_POINT ( 'NONE',  ( -102.6338077722834043, 34.09093689858332255, 84.21073488133825435 ) ) ;
#57588 = FACE_BOUND ( 'NONE', #27245, .T. ) ;
#57589 = ORIENTED_EDGE ( 'NONE', *, *, #22064, .T. ) ;
#57590 = CARTESIAN_POINT ( 'NONE',  ( -58.96922974609609724, 15.76655591015168412, -22.27256446023782388 ) ) ;
#57591 = B_SPLINE_CURVE_WITH_KNOTS ( 'NONE', 3,
 ( #65771, #11938, #48498, #43588, #16518, #33410, #28110, #33048, #332, #693, #1387, #64709, #37975, #22842, #49205, #7015, #64353, #32360, #59419, #11230, #54484, #6310, #32696, #54128, #1041, #22492, #23893, #66132, #1743, #62208, #14024, #34801, #24251, #44650, #40752, #13003, #18264, #49913, #45339, #24599, #55903, #17919, #66820 ),
 .UNSPECIFIED., .F., .F.,
 ( 4, 2, 2, 2, 2, 2, 2, 2, 2, 2, 2, 2, 1, 2, 2, 2, 2, 2, 2, 2, 2, 4 ),
 ( 0.02362927190606133043, 0.02510248541563191854, 0.02583909217041721607, 0.02657569892520251359, 0.02804891243477309823, 0.02952212594434368634, 0.03025873269912898039, 0.03099533945391427098, 0.03246855296348487296, 0.03394176647305548189, 0.03541497998262608388, 0.03615158673741138140, 0.03688819349219668586, 0.03762480024698199033, 0.03836140700176728785, 0.03983462051133786208, 0.04130783402090842937, 0.04278104753047899667, 0.04351765428526427337, 0.04425426104004954314, 0.04572747454962008268, 0.04720068805919061528 ),
 .UNSPECIFIED. ) ;
#57592 = CARTESIAN_POINT ( 'NONE',  ( 74.39890044415652426, -7.951074708186050444, 170.0000000000000000 ) ) ;
#57593 = DIRECTION ( 'NONE',  ( 0.000000000000000000, 1.000000000000000000, 0.000000000000000000 ) ) ;
#57594 = CARTESIAN_POINT ( 'NONE',  ( -6.000000000000000000, 0.000000000000000000, 5.000000000000000000 ) ) ;
#57595 = DIRECTION ( 'NONE',  ( 1.000000000000000000, -0.000000000000000000, 0.000000000000000000 ) ) ;
#57596 = ORIENTED_EDGE ( 'NONE', *, *, #44296, .T. ) ;
#57597 = EDGE_LOOP ( 'NONE', ( #32887, #65413, #46446, #54458 ) ) ;
#57598 = CARTESIAN_POINT ( 'NONE',  ( 9.907111016279298354, 7.389490965936898803, -91.97754063910812761 ) ) ;
#57599 = CARTESIAN_POINT ( 'NONE',  ( -167.6386155194958292, 81.22597462185134987, -37.06873647268641037 ) ) ;
#57601 = EDGE_CURVE ( 'NONE', #66548, #55194, #46940, .T. ) ;
#57600 = DIRECTION ( 'NONE',  ( 0.000000000000000000, 0.000000000000000000, 1.000000000000000000 ) ) ;
#57602 = EDGE_CURVE ( 'NONE', #13054, #27636, #5055, .T. ) ;
#57603 = LINE ( 'NONE', #8381, #38931 ) ;
#57604 = CARTESIAN_POINT ( 'NONE',  ( -16.68907004672281502, -73.11959341363693454, 43.58025477438756212 ) ) ;
#57605 = CARTESIAN_POINT ( 'NONE',  ( -66.97713359923356791, 33.64188291208976977, 41.38025477438755928 ) ) ;
#57606 = ADVANCED_FACE ( 'NONE', ( #37404 ), #57841, .F. ) ;
#57607 = DIRECTION ( 'NONE',  ( 0.5000000000000014433, -0.8660254037844379305, 0.000000000000000000 ) ) ;
#57608 = DIRECTION ( 'NONE',  ( -0.000000000000000000, 1.000000000000000000, -0.000000000000000000 ) ) ;
#57609 = CARTESIAN_POINT ( 'NONE',  ( -165.6393662153604396, 79.16886183052815795, -68.45080963872082691 ) ) ;
#57610 = EDGE_LOOP ( 'NONE', ( #31323, #16334, #10773, #67886, #55383, #34107, #47339 ) ) ;
#57611 = DIRECTION ( 'NONE',  ( -0.000000000000000000, 1.000000000000000000, -0.000000000000000000 ) ) ;
#57612 = VERTEX_POINT ( 'NONE', #53917 ) ;
#57613 = CARTESIAN_POINT ( 'NONE',  ( -35.17686701826946205, 10.23452050416468317, 17.39241332462970036 ) ) ;
#57614 = CARTESIAN_POINT ( 'NONE',  ( 83.37782009939535044, 19.39546426214656449, 70.81951084743843694 ) ) ;
#57615 = FACE_OUTER_BOUND ( 'NONE', #44067, .T. ) ;
#57616 = DIRECTION ( 'NONE',  ( 1.000000000000000000, 0.000000000000000000, -0.000000000000000000 ) ) ;
#57617 = DIRECTION ( 'NONE',  ( 1.000000000000000000, 0.000000000000000000, -0.000000000000000000 ) ) ;
#57618 = CARTESIAN_POINT ( 'NONE',  ( 266.9165763529819628, 242.0000000000000000, 108.9999999999999858 ) ) ;
#57619 = CARTESIAN_POINT ( 'NONE',  ( 32.67604581760324578, 7.629767527669949700, 13.89685609384374487 ) ) ;
#57620 = CARTESIAN_POINT ( 'NONE',  ( -14.56151485655250077, 8.434196591921342190, -46.25215706853945363 ) ) ;
#57621 = VECTOR ( 'NONE', #40177, 1000.000000000000000 ) ;
#57622 = LINE ( 'NONE', #41786, #37135 ) ;
#57623 = B_SPLINE_CURVE_WITH_KNOTS ( 'NONE', 3,
 ( #20132, #9583, #3272, #35630, #63042, #40896, #14848, #19092, #68657, #61997, #62708, #46512, #63396, #35278, #36314, #3608, #31043, #24732, #46167, #25076, #8200, #14168, #57770, #56735, #30691, #57422, #57082, #19789, #52487, #25771, #8895, #8551, #47200, #67306, #67990, #30003, #15201, #67640, #56379, #29651, #19435, #14509, #35968, #51113 ),
 .UNSPECIFIED., .F., .F.,
 ( 4, 2, 2, 2, 2, 2, 2, 2, 2, 2, 2, 2, 2, 2, 2, 2, 2, 2, 2, 2, 2, 4 ),
 ( 1.551583845779545699E-17, 0.004120577325733583603, 0.006180865988600344613, 0.008241154651467106490, 0.01030144331433386490, 0.01133158764576721635, 0.01236173197720056779, 0.01339187630863392271, 0.01442202064006727416, 0.01545216497150062561, 0.01648230930293397359, 0.01699738146865065885, 0.01751245363436734759, 0.01854259796580074587, 0.01957274229723415110, 0.02060288662866755285, 0.02266317529153432167, 0.02472346395440109049, 0.02678375261726785930, 0.02781389694870120208, 0.02884404128013454832, 0.03296461860586802350 ),
 .UNSPECIFIED. ) ;
#57624 = VERTEX_POINT ( 'NONE', #475 ) ;
#57625 = CARTESIAN_POINT ( 'NONE',  ( -119.6718585611729679, 43.71387783726355281, -91.88895242600902691 ) ) ;
#57626 = ORIENTED_EDGE ( 'NONE', *, *, #4908, .F. ) ;
#57627 = CARTESIAN_POINT ( 'NONE',  ( -7.329206686002009974E-14, -41.66904755831212270, 0.000000000000000000 ) ) ;
#57628 = SURFACE_STYLE_FILL_AREA ( #14707 ) ;
#57629 = CARTESIAN_POINT ( 'NONE',  ( -25.48237668717800375, 8.689083390666771933, 15.45542771530772441 ) ) ;
#57630 = PLANE ( 'NONE',  #51342 ) ;
#57631 = CARTESIAN_POINT ( 'NONE',  ( -11.78792974237933500, 7.181513757308657375, -76.13506112128496284 ) ) ;
#57632 = CARTESIAN_POINT ( 'NONE',  ( -37.04655464516844177, 53.85410457537858520, 43.58025477438756212 ) ) ;
#57633 = AXIS2_PLACEMENT_3D ( 'NONE', #56581, #46359, #18607 ) ;
#57634 = CARTESIAN_POINT ( 'NONE',  ( 149.9714610887121466, 53.28792066194168342, -43.93159308990031064 ) ) ;
#57635 = VECTOR ( 'NONE', #51830, 1000.000000000000114 ) ;
#57636 = EDGE_LOOP ( 'NONE', ( #69521, #56578, #62015, #65377, #22482, #69056 ) ) ;
#57638 = AXIS2_PLACEMENT_3D ( 'NONE', #12519, #65645, #28344 ) ;
#57637 = DIRECTION ( 'NONE',  ( 1.000000000000000000, 9.989315170677502600E-15, -9.989315170677463157E-15 ) ) ;
#57639 = DIRECTION ( 'NONE',  ( 0.000000000000000000, -1.000000000000000000, 5.102127870520020458E-18 ) ) ;
#57640 = CARTESIAN_POINT ( 'NONE',  ( 440.2662102946430878, 395.0000000000000568, -139.3786363301463211 ) ) ;
#57641 = LINE ( 'NONE', #15416, #2035 ) ;
#57642 = DIRECTION ( 'NONE',  ( -3.081487911019579554E-32, -1.000000000000000000, -3.469446951953612956E-17 ) ) ;
#57643 = ORIENTED_EDGE ( 'NONE', *, *, #56596, .T. ) ;
#57644 = DIRECTION ( 'NONE',  ( 0.000000000000000000, -1.000000000000000000, 0.000000000000000000 ) ) ;
#57645 = CARTESIAN_POINT ( 'NONE',  ( -1.876547441458561893, 6.576559737910139702, -20.64758074539619770 ) ) ;
#57646 = CARTESIAN_POINT ( 'NONE',  ( 117.4696399285658543, 32.37118663718646872, 35.03847803874900535 ) ) ;
#57647 = CARTESIAN_POINT ( 'NONE',  ( -173.1211646369891355, -170.0000000000000000, 18.97714401617737323 ) ) ;
#57648 = ADVANCED_FACE ( 'NONE', ( #10671 ), #28700, .T. ) ;
#57649 = CARTESIAN_POINT ( 'NONE',  ( -124.1033713525885389, 45.32626312604504193, -61.97149759412182135 ) ) ;
#57650 = ORIENTED_EDGE ( 'NONE', *, *, #8349, .F. ) ;
#57651 = CARTESIAN_POINT ( 'NONE',  ( 197.6145711261845008, 97.10888456119690204, 34.16122082187249731 ) ) ;
#57652 = DIRECTION ( 'NONE',  ( 0.9639628606958550172, -0.2660368455666687892, 0.000000000000000000 ) ) ;
#57653 = CARTESIAN_POINT ( 'NONE',  ( 188.2091813586561386, 87.61952156613882892, 39.16720350456787969 ) ) ;
#57654 = DIRECTION ( 'NONE',  ( -0.1342332658176522420, -0.9909497617679352555, 0.000000000000000000 ) ) ;
#57655 = DIRECTION ( 'NONE',  ( 1.000000000000000000, 0.000000000000000000, 0.000000000000000000 ) ) ;
#57656 = ORIENTED_EDGE ( 'NONE', *, *, #39700, .T. ) ;
#57657 = EDGE_CURVE ( 'NONE', #24361, #66914, #56823, .T. ) ;
#57658 = CARTESIAN_POINT ( 'NONE',  ( 175.0696098417091662, 74.11936424544843760, 59.16513549669191008 ) ) ;
#57659 = ORIENTED_EDGE ( 'NONE', *, *, #47398, .T. ) ;
#57660 = CARTESIAN_POINT ( 'NONE',  ( -104.1244073710070239, 33.72720758483609416, -35.23009648099888125 ) ) ;
#57661 = CARTESIAN_POINT ( 'NONE',  ( 141.0352762984948356, 45.93128157562509983, 88.49822799473426471 ) ) ;
#57662 = ADVANCED_FACE ( 'NONE', ( #59203 ), #43374, .F. ) ;
#57663 = DIRECTION ( 'NONE',  ( 0.000000000000000000, 0.000000000000000000, -1.000000000000000000 ) ) ;
#57664 = ADVANCED_FACE ( 'NONE', ( #31120 ), #31455, .T. ) ;
#57665 = VECTOR ( 'NONE', #57008, 1000.000000000000000 ) ;
#57667 = ORIENTED_EDGE ( 'NONE', *, *, #34158, .T. ) ;
#57666 = CARTESIAN_POINT ( 'NONE',  ( 157.0357419681844533, 58.58786672900119186, 2.574317928867096317 ) ) ;
#57668 = CARTESIAN_POINT ( 'NONE',  ( -180.6011569556094969, 95.85968111394265634, 37.69164199392516679 ) ) ;
#57669 = DIRECTION ( 'NONE',  ( 0.7071067811865408004, -2.275957200481570908E-15, -0.7071067811865543451 ) ) ;
#57670 = CARTESIAN_POINT ( 'NONE',  ( 110.2429982417149432, 29.99119854320846201, -35.92243756565368784 ) ) ;
#57671 = AXIS2_PLACEMENT_3D ( 'NONE', #20315, #20660, #41779 ) ;
#57672 = VERTEX_POINT ( 'NONE', #5408 ) ;
#57673 = CYLINDRICAL_SURFACE ( 'NONE', #18759, 20.00000000000000000 ) ;
#57674 = AXIS2_PLACEMENT_3D ( 'NONE', #66429, #47271, #68723 ) ;
#57675 = FACE_OUTER_BOUND ( 'NONE', #51774, .T. ) ;
#57676 = VERTEX_POINT ( 'NONE', #26519 ) ;
#57677 = DIRECTION ( 'NONE',  ( 0.000000000000000000, -6.123233995736870806E-17, 1.000000000000000000 ) ) ;
#57678 = CARTESIAN_POINT ( 'NONE',  ( 0.000000000000000000, 0.000000000000000000, 170.0000000000000000 ) ) ;
#57679 = AXIS2_PLACEMENT_3D ( 'NONE', #27591, #22321, #37112 ) ;
#57680 = CARTESIAN_POINT ( 'NONE',  ( 150.0433793199863430, 52.09973307442956525, 62.67375200242342004 ) ) ;
#57681 = DIRECTION ( 'NONE',  ( 0.000000000000000000, 1.000000000000000000, -0.000000000000000000 ) ) ;
#57682 = ORIENTED_EDGE ( 'NONE', *, *, #4681, .F. ) ;
#57683 = CARTESIAN_POINT ( 'NONE',  ( 39.89582146299188281, 9.488756994579087944, 18.06928371549960488 ) ) ;
#57684 = ORIENTED_EDGE ( 'NONE', *, *, #62279, .F. ) ;
#57685 = CARTESIAN_POINT ( 'NONE',  ( 156.5890478960376981, 58.24007662587948886, -9.318429201860791267 ) ) ;
#57686 = CARTESIAN_POINT ( 'NONE',  ( 211.7318474105134385, 118.3631723164074714, -19.60079423289586487 ) ) ;
#57687 = CARTESIAN_POINT ( 'NONE',  ( -27.92096212090788399, 31.01184537397639929, 13.79046340968177908 ) ) ;
#57688 = CARTESIAN_POINT ( 'NONE',  ( -153.1121305730336815, 67.29834700374524914, -62.57647805126995166 ) ) ;
#57689 = DIRECTION ( 'NONE',  ( -0.000000000000000000, 0.5000000000000009992, 0.8660254037844380415 ) ) ;
#57690 = EDGE_CURVE ( 'NONE', #49450, #56234, #10722, .T. ) ;
#57691 = FACE_OUTER_BOUND ( 'NONE', #66161, .T. ) ;
#57692 = CARTESIAN_POINT ( 'NONE',  ( 211.7419975634644800, 116.5322580952101674, -46.48037847538860490 ) ) ;
#57693 = CARTESIAN_POINT ( 'NONE',  ( 110.2429982417149574, -170.0000000000000000, 10.26666361527366078 ) ) ;
#57694 = ORIENTED_EDGE ( 'NONE', *, *, #57101, .T. ) ;
#57695 = CARTESIAN_POINT ( 'NONE',  ( 60.74750367560205433, 24.13405452624939329, 43.58025477438756212 ) ) ;
#57696 = ORIENTED_EDGE ( 'NONE', *, *, #42418, .F. ) ;
#57697 = CARTESIAN_POINT ( 'NONE',  ( -71.57660578921959882, 20.81129687646280502, 67.25978822818018443 ) ) ;
#57698 = CARTESIAN_POINT ( 'NONE',  ( 57.39083379741712321, 11.43779987330584547, -75.05095958129902556 ) ) ;
#57699 = CARTESIAN_POINT ( 'NONE',  ( 450.2085304802404266, 190.0000000000000000, -250.0000000000000000 ) ) ;
#57700 = CARTESIAN_POINT ( 'NONE',  ( 0.000000000000000000, 0.000000000000000000, 0.000000000000000000 ) ) ;
#57701 = CARTESIAN_POINT ( 'NONE',  ( -4.384507269342570623, 6.691209796733446069, 84.63264704995823706 ) ) ;
#57702 = CARTESIAN_POINT ( 'NONE',  ( -109.0291978193666722, 37.49173305805086898, -18.95094030686922082 ) ) ;
#57703 = EDGE_LOOP ( 'NONE', ( #15613, #68081, #12297, #44352 ) ) ;
#57704 = CARTESIAN_POINT ( 'NONE',  ( -76.77329340382466683, 21.60914066444074066, 72.03569539077717820 ) ) ;
#57705 = LINE ( 'NONE', #68598, #6037 ) ;
#57706 = EDGE_LOOP ( 'NONE', ( #16077, #59270 ) ) ;
#57707 = ORIENTED_EDGE ( 'NONE', *, *, #23599, .T. ) ;
#57708 = CARTESIAN_POINT ( 'NONE',  ( -153.6931187576189188, 67.81270084382354923, 31.99307535251548629 ) ) ;
#57709 = LINE ( 'NONE', #4580, #50175 ) ;
#57710 = CARTESIAN_POINT ( 'NONE',  ( 179.4279766878530609, 76.94722012158237590, -24.20745791858651330 ) ) ;
#57711 = DIRECTION ( 'NONE',  ( -0.000000000000000000, -0.000000000000000000, -1.000000000000000000 ) ) ;
#57712 =( GEOMETRIC_REPRESENTATION_CONTEXT ( 3 ) GLOBAL_UNCERTAINTY_ASSIGNED_CONTEXT ( ( #17744 ) ) GLOBAL_UNIT_ASSIGNED_CONTEXT ( ( #46815, #47486, #46462 ) ) REPRESENTATION_CONTEXT ( 'NONE', 'WORKASPACE' ) );
#57713 = CARTESIAN_POINT ( 'NONE',  ( -142.0251973982165339, 58.08401473564118334, 10.78919118282799339 ) ) ;
#57714 = VERTEX_POINT ( 'NONE', #4381 ) ;
#57715 = CARTESIAN_POINT ( 'NONE',  ( 0.000000000000000000, -27.00000000000000355, 12.00000000000000000 ) ) ;
#57716 = PRODUCT_DEFINITION ( 'UNKNOWN', '', #36631, #15578 ) ;
#57717 = ORIENTED_EDGE ( 'NONE', *, *, #14777, .F. ) ;
#57718 = CARTESIAN_POINT ( 'NONE',  ( 211.1200456646896839, 115.5868795682033010, 13.74673903110627293 ) ) ;
#57719 = CARTESIAN_POINT ( 'NONE',  ( 110.2429982417149574, -170.0000000000000000, 44.61121420573733332 ) ) ;
#57720 = AXIS2_PLACEMENT_3D ( 'NONE', #33834, #55276, #28913 ) ;
#57721 = CARTESIAN_POINT ( 'NONE',  ( 209.4789161463551750, 113.1367444519304257, 30.92499520828909709 ) ) ;
#57722 = CARTESIAN_POINT ( 'NONE',  ( 9.681512146547785136, 6.381925336433647900, -92.33363154823911145 ) ) ;
#57723 = EDGE_CURVE ( 'NONE', #695, #19391, #10330, .T. ) ;
#57724 = VECTOR ( 'NONE', #53888, 1000.000000000000000 ) ;
#57725 = EDGE_CURVE ( 'NONE', #56059, #54414, #15620, .T. ) ;
#57726 = ORIENTED_EDGE ( 'NONE', *, *, #36386, .T. ) ;
#57727 = ORIENTED_EDGE ( 'NONE', *, *, #24510, .F. ) ;
#57728 = CARTESIAN_POINT ( 'NONE',  ( -149.5074843970971017, 65.50121172469319220, 57.56537183036274286 ) ) ;
#57729 = CARTESIAN_POINT ( 'NONE',  ( -121.5894932252149800, 44.91329912928144097, 85.63689221737818968 ) ) ;
#57730 = AXIS2_PLACEMENT_3D ( 'NONE', #8134, #62286, #66896 ) ;
#57731 = CARTESIAN_POINT ( 'NONE',  ( -166.7068579965637412, 80.26142964949316649, -19.26318465954255643 ) ) ;
#57732 = DIRECTION ( 'NONE',  ( -0.000000000000000000, 1.000000000000000000, -0.000000000000000000 ) ) ;
#57733 = CARTESIAN_POINT ( 'NONE',  ( 22.95565677133307148, 6.835936356918209889, 88.97060043287888220 ) ) ;
#57734 = CARTESIAN_POINT ( 'NONE',  ( 23.28997038562041055, 7.864942668124619729, 90.91843093332407477 ) ) ;
#57735 = ORIENTED_EDGE ( 'NONE', *, *, #49208, .F. ) ;
#57736 = PLANE ( 'NONE',  #47146 ) ;
#57737 = CARTESIAN_POINT ( 'NONE',  ( -95.21430597939261986, 29.33390900154316938, 62.29818221739061102 ) ) ;
#57738 = ORIENTED_EDGE ( 'NONE', *, *, #66253, .F. ) ;
#57739 = SHAPE_REPRESENTATION ( 'Part1', ( #66832 ), #11761 ) ;
#57740 = CARTESIAN_POINT ( 'NONE',  ( -85.90441187606239737, 25.21188850826090899, 13.10346238197241853 ) ) ;
#57741 = ORIENTED_EDGE ( 'NONE', *, *, #57181, .T. ) ;
#57742 = LINE ( 'NONE', #35940, #558 ) ;
#57743 = ADVANCED_FACE ( 'NONE', ( #5740 ), #25842, .T. ) ;
#57744 = ORIENTED_EDGE ( 'NONE', *, *, #66674, .T. ) ;
#57745 = EDGE_CURVE ( 'NONE', #39519, #10376, #69424, .T. ) ;
#57746 = ORIENTED_EDGE ( 'NONE', *, *, #34004, .F. ) ;
#57747 = CARTESIAN_POINT ( 'NONE',  ( 8.288104306525690745, 6.376394648992967262, -43.50552248815810685 ) ) ;
#57748 = FACE_OUTER_BOUND ( 'NONE', #16819, .T. ) ;
#57749 = CARTESIAN_POINT ( 'NONE',  ( 128.0848616812662613, 38.04676222636086891, 68.67022180960751143 ) ) ;
#57750 = ORIENTED_EDGE ( 'NONE', *, *, #20805, .T. ) ;
#57751 = DIRECTION ( 'NONE',  ( 0.000000000000000000, 0.000000000000000000, 1.000000000000000000 ) ) ;
#57752 = CARTESIAN_POINT ( 'NONE',  ( 179.0091171455098049, 77.94933395983136393, -77.78972269939623629 ) ) ;
#57753 = AXIS2_PLACEMENT_3D ( 'NONE', #31122, #53827, #63121 ) ;
#57754 = CARTESIAN_POINT ( 'NONE',  ( 444.9999999999999432, 225.0000000000000000, 380.0000000000000000 ) ) ;
#57755 = DIRECTION ( 'NONE',  ( -1.850371928290090422E-16, 1.000000000000000000, 1.110223024625156171E-16 ) ) ;
#57756 = CARTESIAN_POINT ( 'NONE',  ( 79.39764314491567632, 18.13166883367084736, -45.32563429318312842 ) ) ;
#57757 = CARTESIAN_POINT ( 'NONE',  ( 4.165045035621076863, -64.88046627338039229, 41.38025477438755928 ) ) ;
#57758 = ORIENTED_EDGE ( 'NONE', *, *, #52948, .F. ) ;
#57759 = VECTOR ( 'NONE', #20925, 1000.000000000000227 ) ;
#57760 = FACE_OUTER_BOUND ( 'NONE', #60685, .T. ) ;
#57761 = AXIS2_PLACEMENT_3D ( 'NONE', #21968, #49031, #26563 ) ;
#57762 = CARTESIAN_POINT ( 'NONE',  ( -83.53167274806556009, 25.32068190668985253, -63.73130560477633111 ) ) ;
#57763 = CARTESIAN_POINT ( 'NONE',  ( 175.5429257635130966, 74.57009623370765894, 15.04424763849001501 ) ) ;
#57764 = CARTESIAN_POINT ( 'NONE',  ( 51.85299110299440173, 39.21848821248450179, 41.38025477438755928 ) ) ;
#57765 = CARTESIAN_POINT ( 'NONE',  ( -188.6739852773920347, 108.2139733222100375, -13.56090942305224267 ) ) ;
#57766 = CARTESIAN_POINT ( 'NONE',  ( 127.4750938923429828, 37.70245908594343831, 6.217222705552873485 ) ) ;
#57767 = AXIS2_PLACEMENT_3D ( 'NONE', #37346, #58802, #46886 ) ;
#57768 = CARTESIAN_POINT ( 'NONE',  ( 6.123233995736766282E-16, 0.000000000000000000, 5.000000000000000000 ) ) ;
#57769 = CARTESIAN_POINT ( 'NONE',  ( 197.2438487909066396, 98.25413800600045988, 89.45392550497817297 ) ) ;
#57770 = CARTESIAN_POINT ( 'NONE',  ( 212.1913428512247037, 119.0779339498137546, 36.35316656546646641 ) ) ;
#57771 = CARTESIAN_POINT ( 'NONE',  ( 162.0835148203877054, 61.32844276806159201, 4.132286737511699393 ) ) ;
#57772 = CARTESIAN_POINT ( 'NONE',  ( -109.3432140528234697, 36.51591785955880454, 40.59350856912254102 ) ) ;
#57773 = VERTEX_POINT ( 'NONE', #68726 ) ;
#57774 = AXIS2_PLACEMENT_3D ( 'NONE', #37918, #53044, #32303 ) ;
#57775 = CARTESIAN_POINT ( 'NONE',  ( -62.32077575123996382, 17.80262092668387197, 89.62707857507018616 ) ) ;
#57776 = ORIENTED_EDGE ( 'NONE', *, *, #69525, .F. ) ;
#57777 = LINE ( 'NONE', #52823, #48633 ) ;
#57778 = ORIENTED_EDGE ( 'NONE', *, *, #44777, .F. ) ;
#57779 = CARTESIAN_POINT ( 'NONE',  ( 18.88468164817598449, 7.626722602998420975, -76.69889805417930972 ) ) ;
#57780 = PLANE ( 'NONE',  #16624 ) ;
#57781 = CARTESIAN_POINT ( 'NONE',  ( -8.000000000000000000, 4.618802153516996079, -9.500000000000000000 ) ) ;
#57782 = CARTESIAN_POINT ( 'NONE',  ( 141.2361973397653401, 47.26569015399787332, -42.15863887015712663 ) ) ;
#57783 = CARTESIAN_POINT ( 'NONE',  ( 32.56927464314649967, 7.618924692399907883, -46.22225308106595776 ) ) ;
#57784 = DIRECTION ( 'NONE',  ( -1.000000000000000000, 0.000000000000000000, 0.000000000000000000 ) ) ;
#57785 = DIRECTION ( 'NONE',  ( 1.000000000000000000, 0.000000000000000000, 0.000000000000000000 ) ) ;
#57786 = DIRECTION ( 'NONE',  ( 0.000000000000000000, 0.000000000000000000, 1.000000000000000000 ) ) ;
#57787 = ORIENTED_EDGE ( 'NONE', *, *, #11103, .F. ) ;
#57788 = ORIENTED_EDGE ( 'NONE', *, *, #24838, .T. ) ;
#57789 = CARTESIAN_POINT ( 'NONE',  ( 50.59696764854425766, 10.45241199037308455, 26.66469066592268433 ) ) ;
#57790 = CARTESIAN_POINT ( 'NONE',  ( 0.000000000000000000, 0.000000000000000000, -0.5251556536572842271 ) ) ;
#57791 = CARTESIAN_POINT ( 'NONE',  ( -24.32937228292060539, 8.531905774118438757, -72.09986348764125808 ) ) ;
#57792 = UNCERTAINTY_MEASURE_WITH_UNIT (LENGTH_MEASURE( 1.000000000000000082E-05 ), #15145, 'distance_accuracy_value', 'NONE');
#57793 = CARTESIAN_POINT ( 'NONE',  ( 13.84120792123768773, 6.445822122644893959, 3.410756033091004724 ) ) ;
#57794 = ADVANCED_FACE ( 'NONE', ( #64495 ), #15277, .F. ) ;
#57795 = CARTESIAN_POINT ( 'NONE',  ( 45.89232972084000295, 10.36128169546909739, -73.73081192014224428 ) ) ;
#57796 = CARTESIAN_POINT ( 'NONE',  ( -417.6627218934913230, 219.4906275429376308, 113.5502958579881749 ) ) ;
#57797 = DIRECTION ( 'NONE',  ( -1.000000000000000000, 0.000000000000000000, 0.000000000000000000 ) ) ;
#57798 = CARTESIAN_POINT ( 'NONE',  ( -178.0658882571760842, 92.80593104957425510, -47.85589308113880946 ) ) ;
#57799 = CARTESIAN_POINT ( 'NONE',  ( 87.58098510096633049, 19.74745174099417255, -23.93185505127985380 ) ) ;
#57800 = CARTESIAN_POINT ( 'NONE',  ( -29.50439180771547854, 10.29976981300625205, 57.29848261981403112 ) ) ;
#57801 = CARTESIAN_POINT ( 'NONE',  ( 106.9495076362458548, 21.63869423720477769, 3.975053342410763246 ) ) ;
#57802 = B_SPLINE_CURVE_WITH_KNOTS ( 'NONE', 3,
 ( #4345, #34970, #30729, #8589, #47232, #46196, #68690, #36348, #63428, #51829, #41282, #68365, #14545, #3996, #8931, #19471, #52176, #8236, #63077, #67676, #13850, #3639, #45865, #62034, #56413, #67337, #24763, #46901, #56770, #30038, #51500, #25114, #3302, #46546, #19829, #9268, #20166, #62741, #36005, #14881, #57800, #9620, #37036, #42653 ),
 .UNSPECIFIED., .F., .F.,
 ( 4, 2, 2, 2, 2, 2, 2, 2, 2, 2, 2, 2, 2, 2, 2, 2, 2, 2, 2, 2, 2, 4 ),
 ( 0.000000000000000000, 0.001473754749730416067, 0.002210632124595628221, 0.002947509499460839941, 0.004421264249191274656, 0.005895018998921709372, 0.007368773748652143220, 0.008105651123517363180, 0.008842528498382584007, 0.01031628324811306209, 0.01179003799784354191, 0.01252691537270880263, 0.01326379274757406336, 0.01473754749730458134, 0.01547442487216983166, 0.01621130224703508371, 0.01768505699676558435, 0.01915881174649608845, 0.01989568912136133877, 0.02063256649622658562, 0.02210632124595708972, 0.02358007599568759036 ),
 .UNSPECIFIED. ) ;
#57803 = CARTESIAN_POINT ( 'NONE',  ( -49.62489392740899063, 13.29305723289026986, 59.48038597728405819 ) ) ;
#57804 = EDGE_CURVE ( 'NONE', #59960, #30631, #15961, .T. ) ;
#57805 = VECTOR ( 'NONE', #32159, 1000.000000000000000 ) ;
#57806 = ADVANCED_FACE ( 'NONE', ( #21574 ), #53376, .T. ) ;
#57807 = ORIENTED_EDGE ( 'NONE', *, *, #12873, .T. ) ;
#57808 = CARTESIAN_POINT ( 'NONE',  ( 132.9557829392755082, 42.05591979570414907, 2.706097766650628955 ) ) ;
#57809 = CARTESIAN_POINT ( 'NONE',  ( 11.30618213853490239, -74.15344055032291237, 170.0000000000000000 ) ) ;
#57810 = ADVANCED_FACE ( 'NONE', ( #37756 ), #6087, .F. ) ;
#57811 = CARTESIAN_POINT ( 'NONE',  ( 153.2208437558772118, 55.67531116261157109, 69.95159403288403155 ) ) ;
#57812 = CARTESIAN_POINT ( 'NONE',  ( -109.7686203588200868, 37.90089348911612888, -68.86741973818818963 ) ) ;
#57813 = CARTESIAN_POINT ( 'NONE',  ( -4.999999999999922728, 46.66904755831208718, 2.000000000000001776 ) ) ;
#57814 = CARTESIAN_POINT ( 'NONE',  ( -0.3423060809770838708, 7.525952860323299021, 91.90469597356303666 ) ) ;
#57815 = AXIS2_PLACEMENT_3D ( 'NONE', #26901, #48327, #33588 ) ;
#57816 = ORIENTED_EDGE ( 'NONE', *, *, #51620, .F. ) ;
#57817 = AXIS2_PLACEMENT_3D ( 'NONE', #69536, #37533, #60024 ) ;
#57818 = CARTESIAN_POINT ( 'NONE',  ( 0.1317522424472098441, 1.959574484719855292, 7.999999999999998224 ) ) ;
#57819 = AXIS2_PLACEMENT_3D ( 'NONE', #42073, #48028, #58932 ) ;
#57820 = CARTESIAN_POINT ( 'NONE',  ( -55.05276343752910151, 14.68156374112636797, 72.16187836339486239 ) ) ;
#57821 = ORIENTED_EDGE ( 'NONE', *, *, #58160, .T. ) ;
#57822 = EDGE_LOOP ( 'NONE', ( #59925, #56790, #9075, #31689, #67062, #23318, #22385, #32022, #30694 ) ) ;
#57823 = AXIS2_PLACEMENT_3D ( 'NONE', #25487, #46926, #54512 ) ;
#57824 = CARTESIAN_POINT ( 'NONE',  ( 33.84530598357039111, 8.763572915769019644, 86.05493817697373515 ) ) ;
#57825 = DIRECTION ( 'NONE',  ( 0.000000000000000000, -0.000000000000000000, 1.000000000000000000 ) ) ;
#57826 = DIRECTION ( 'NONE',  ( 0.000000000000000000, -0.000000000000000000, -1.000000000000000000 ) ) ;
#57827 = EDGE_CURVE ( 'NONE', #40256, #62711, #38813, .T. ) ;
#57828 = ORIENTED_EDGE ( 'NONE', *, *, #37730, .F. ) ;
#57829 = PLANE ( 'NONE',  #49092 ) ;
#57830 = CARTESIAN_POINT ( 'NONE',  ( -48.12872802574264597, 43.70867239603710885, 3.061616997868437868E-16 ) ) ;
#57831 = CARTESIAN_POINT ( 'NONE',  ( -0.3740447803642799607, 7.527031846085010081, 9.787104204890834325 ) ) ;
#57832 = CARTESIAN_POINT ( 'NONE',  ( -85.75002235020438945, 26.23806300442547723, 40.39546564861201006 ) ) ;
#57833 = CARTESIAN_POINT ( 'NONE',  ( -8.000000000000000000, 4.618802153517024500, -8.785468820183664818 ) ) ;
#57834 = DIRECTION ( 'NONE',  ( 1.000000000000000000, 0.000000000000000000, -0.000000000000000000 ) ) ;
#57835 = ORIENTED_EDGE ( 'NONE', *, *, #62086, .T. ) ;
#57836 = CARTESIAN_POINT ( 'NONE',  ( 104.4006536356073980, 27.36759527624477073, -21.30726361956479664 ) ) ;
#57837 = CARTESIAN_POINT ( 'NONE',  ( 9.416603677636260272, 6.380307115728824918, 60.39548338895173174 ) ) ;
#57838 = DIRECTION ( 'NONE',  ( -1.000000000000000000, 0.000000000000000000, 0.000000000000000000 ) ) ;
#57839 = CARTESIAN_POINT ( 'NONE',  ( 198.8732368717152212, 100.3103976497390732, 41.43945101493392258 ) ) ;
#57840 = CARTESIAN_POINT ( 'NONE',  ( -71.97767679134960872, 20.95111989827391596, 94.99999999999866418 ) ) ;
#57842 = ORIENTED_EDGE ( 'NONE', *, *, #16598, .T. ) ;
#57841 = PLANE ( 'NONE',  #29856 ) ;
#57843 = CARTESIAN_POINT ( 'NONE',  ( 70.45451534980409747, 15.56315969138429089, 36.32525407553249153 ) ) ;
#57844 = ORIENTED_EDGE ( 'NONE', *, *, #33829, .F. ) ;
#57845 = ORIENTED_EDGE ( 'NONE', *, *, #15570, .T. ) ;
#57846 = CARTESIAN_POINT ( 'NONE',  ( 116.9197133427646804, 33.22079464767578827, -73.72094471291028128 ) ) ;
#57847 = LINE ( 'NONE', #42357, #53573 ) ;
#57848 = CARTESIAN_POINT ( 'NONE',  ( 200.8298320869470217, 101.1869877914233342, -77.11050760436773999 ) ) ;
#57849 = PLANE ( 'NONE',  #4690 ) ;
#57850 = CARTESIAN_POINT ( 'NONE',  ( 70.26840926437850499, 14.47268499222803584, -95.00000000000133582 ) ) ;
#57851 = CARTESIAN_POINT ( 'NONE',  ( -83.51110947562233378, 25.31252704029285638, -21.50135568052127866 ) ) ;
#57852 = CARTESIAN_POINT ( 'NONE',  ( 290.0000000000000568, 5.000000000000000888, 18.50000000000000000 ) ) ;
#57853 = AXIS2_PLACEMENT_3D ( 'NONE', #33200, #64509, #42700 ) ;
#57854 = FACE_BOUND ( 'NONE', #61950, .T. ) ;
#57855 = ORIENTED_EDGE ( 'NONE', *, *, #36906, .T. ) ;
#57856 = VERTEX_POINT ( 'NONE', #23674 ) ;
#57857 = CARTESIAN_POINT ( 'NONE',  ( 64.69738688745241006, 14.10375742873388560, -9.063140076922552524 ) ) ;
#57858 = AXIS2_PLACEMENT_3D ( 'NONE', #67225, #34854, #35540 ) ;
#57859 = CARTESIAN_POINT ( 'NONE',  ( -84.23336401058610079, 25.60798568215573923, -37.56591546589165631 ) ) ;
#57860 = CARTESIAN_POINT ( 'NONE',  ( 115.9898432474883805, 31.63259700092694615, 85.96951199300247026 ) ) ;
#57861 = LINE ( 'NONE', #51557, #7149 ) ;
#57862 = VECTOR ( 'NONE', #52605, 1000.000000000000000 ) ;
#57863 = B_SPLINE_CURVE_WITH_KNOTS ( 'NONE', 3,
 ( #36854, #9777, #10797, #48075, #58295, #11141, #68842, #42799, #52669, #22047, #16426, #32267, #53699, #25955, #5520, #26974, #63583, #48404, #43493, #237, #21020, #21694, #43145, #63924, #15396, #10113, #31570, #59327, #32605, #54032, #4830, #5858, #64970, #16762, #38223, #23460 ),
 .UNSPECIFIED., .F., .F.,
 ( 4, 2, 2, 2, 2, 2, 2, 2, 2, 2, 2, 2, 2, 2, 2, 2, 2, 4 ),
 ( 1.551583845779545699E-17, 0.001548367318450189758, 0.003096734636900363904, 0.004645101955350544772, 0.006193469273800726073, 0.007741836592250900435, 0.008516020251475976341, 0.009290203910701053114, 0.01083857122915120319, 0.01238693854760135500, 0.01393530586605150681, 0.01548367318450165862, 0.01703204050295181043, 0.01858040782140196051, 0.02012877513985211753, 0.02167714245830227107, 0.02322550977675242809, 0.02477387709520258163 ),
 .UNSPECIFIED. ) ;
#57864 = ADVANCED_FACE ( 'NONE', ( #64845 ), #50407, .F. ) ;
#57865 = CARTESIAN_POINT ( 'NONE',  ( 188.4389256074244088, 86.37278721358585187, -42.22759239191712055 ) ) ;
#57866 = CARTESIAN_POINT ( 'NONE',  ( 414.4083459183738114, 395.0000000000040927, 80.62136366984962876 ) ) ;
#57867 = CARTESIAN_POINT ( 'NONE',  ( 162.8142581494936110, 61.92799983924231810, -65.18475365324361803 ) ) ;
#57868 = EDGE_LOOP ( 'NONE', ( #7694, #53233, #25738, #25235 ) ) ;
#57869 = ORIENTED_EDGE ( 'NONE', *, *, #24455, .T. ) ;
#57870 = AXIS2_PLACEMENT_3D ( 'NONE', #3166, #52380, #57315 ) ;
#57871 = VERTEX_POINT ( 'NONE', #60607 ) ;
#57872 = AXIS2_PLACEMENT_3D ( 'NONE', #4795, #54347, #27276 ) ;
#57873 = DIRECTION ( 'NONE',  ( 1.000000000000000000, 1.387778780781445429E-16, 0.000000000000000000 ) ) ;
#57874 = CARTESIAN_POINT ( 'NONE',  ( -83.52505811737951547, 24.23179517241435832, 59.02801608792132981 ) ) ;
#57875 = CARTESIAN_POINT ( 'NONE',  ( 106.6971892993744149, -21.67618688890531331, 3.767895544566254085 ) ) ;
#57876 = LINE ( 'NONE', #3378, #18076 ) ;
#57877 = DIRECTION ( 'NONE',  ( 0.000000000000000000, 0.000000000000000000, -1.000000000000000000 ) ) ;
#57878 = CARTESIAN_POINT ( 'NONE',  ( 0.000000000000000000, 6.928203230275506108, 4.000000000000006217 ) ) ;
#57879 = CARTESIAN_POINT ( 'NONE',  ( 9.416603677636260272, 6.380307115728824030, -20.13816838243932494 ) ) ;
#57880 = CARTESIAN_POINT ( 'NONE',  ( -65.36598343705435354, 0.000000000000000000, 41.38025477438755928 ) ) ;
#57881 = CARTESIAN_POINT ( 'NONE',  ( 187.8959968237853673, 85.77553094678178525, 60.50337096870740083 ) ) ;
#57882 = CARTESIAN_POINT ( 'NONE',  ( -123.6699087229882394, 45.04696784753412686, 4.109065455722274329 ) ) ;
#57883 = DIRECTION ( 'NONE',  ( -0.000000000000000000, -0.000000000000000000, 1.000000000000000000 ) ) ;
#57884 = CARTESIAN_POINT ( 'NONE',  ( 126.4324872316702795, 37.11876756822024248, -15.58278715265817382 ) ) ;
#57885 = CARTESIAN_POINT ( 'NONE',  ( -20.63749999999999574, 0.000000000000000000, 0.000000000000000000 ) ) ;
#57886 = CARTESIAN_POINT ( 'NONE',  ( 12.03162622199373644, 7.415834979634797541, 17.16615268946964079 ) ) ;
#57887 = EDGE_CURVE ( 'NONE', #23937, #31009, #13000, .T. ) ;
#57888 = ORIENTED_EDGE ( 'NONE', *, *, #44934, .T. ) ;
#57889 = CARTESIAN_POINT ( 'NONE',  ( 188.2950202724321116, 86.21411212788227374, 7.881204597112279053 ) ) ;
#57890 = SHAPE_DEFINITION_REPRESENTATION ( #4593, #32051 ) ;
#57891 = ADVANCED_FACE ( 'NONE', ( #828 ), #33884, .F. ) ;
#57892 = CARTESIAN_POINT ( 'NONE',  ( 173.7227242028391743, 71.47307702680407715, 35.34404529599159872 ) ) ;
#57893 = DIRECTION ( 'NONE',  ( -0.000000000000000000, 0.000000000000000000, -1.000000000000000000 ) ) ;
#57894 = CARTESIAN_POINT ( 'NONE',  ( 41.09671232177015554, 8.635892912882347616, -77.27450094475904052 ) ) ;
#57895 = CARTESIAN_POINT ( 'NONE',  ( 186.2680729609084835, 85.48839327635668894, -49.16545261310956505 ) ) ;
#57896 = ORIENTED_EDGE ( 'NONE', *, *, #5050, .T. ) ;
#57897 = ORIENTED_EDGE ( 'NONE', *, *, #15410, .F. ) ;
#57898 = CARTESIAN_POINT ( 'NONE',  ( -23.98903001682803549, 8.486614814224619607, -16.96685653807542593 ) ) ;
#57899 = CARTESIAN_POINT ( 'NONE',  ( 199.2049631873262854, 100.7347227143600321, 14.97624135697880021 ) ) ;
#57900 = ORIENTED_EDGE ( 'NONE', *, *, #53726, .T. ) ;
#57901 = AXIS2_PLACEMENT_3D ( 'NONE', #34249, #35280, #8897 ) ;
#57902 = CARTESIAN_POINT ( 'NONE',  ( 113.4351684956570807, 30.38657459074489964, 57.15270542610819859 ) ) ;
#57903 = ADVANCED_FACE ( 'NONE', ( #44065 ), #43713, .F. ) ;
#57904 = ORIENTED_EDGE ( 'NONE', *, *, #12100, .F. ) ;
#57905 = CARTESIAN_POINT ( 'NONE',  ( -40.27405704175546930, -63.28161525591320924, 170.0000000000000000 ) ) ;
#57906 = CARTESIAN_POINT ( 'NONE',  ( 126.4754729582248132, 37.14269484129876986, 38.36551284386316496 ) ) ;
#57907 = CARTESIAN_POINT ( 'NONE',  ( 2.699999999999990408, 2.486033002269127373E-15, 20.30000000000000071 ) ) ;
#57908 = EDGE_CURVE ( 'NONE', #28889, #62698, #17707, .T. ) ;
#57909 = PLANE ( 'NONE',  #46098 ) ;
#57910 = AXIS2_PLACEMENT_3D ( 'NONE', #55480, #43870, #38613 ) ;
#57912 = CYLINDRICAL_SURFACE ( 'NONE', #33873, 7.500000000000020428 ) ;
#57911 = CIRCLE ( 'NONE', #32099, 8.000000000000000000 ) ;
#57914 = ORIENTED_EDGE ( 'NONE', *, *, #61227, .F. ) ;
#57913 = CARTESIAN_POINT ( 'NONE',  ( 10.55634918610411432, 51.66904755831205875, 0.000000000000000000 ) ) ;
#57915 = AXIS2_PLACEMENT_3D ( 'NONE', #23207, #44654, #66134 ) ;
#57916 = FACE_OUTER_BOUND ( 'NONE', #24806, .T. ) ;
#57917 = CIRCLE ( 'NONE', #55650, 246.3582898394606957 ) ;
#57918 = ORIENTED_EDGE ( 'NONE', *, *, #43316, .F. ) ;
#57919 = ORIENTED_EDGE ( 'NONE', *, *, #65039, .T. ) ;
#57920 = CARTESIAN_POINT ( 'NONE',  ( -121.2008155373973892, 43.48033530165984217, -21.43964104200714615 ) ) ;
#57921 = AXIS2_PLACEMENT_3D ( 'NONE', #23938, #64589, #11450 ) ;
#57922 = LINE ( 'NONE', #31200, #12257 ) ;
#57923 = CARTESIAN_POINT ( 'NONE',  ( -144.9412191745148846, 61.69548892475975066, -36.34343113144615955 ) ) ;
#57925 = ORIENTED_EDGE ( 'NONE', *, *, #41674, .F. ) ;
#57924 = CARTESIAN_POINT ( 'NONE',  ( 0.000000000000000000, 2.999999999999969802, 0.000000000000000000 ) ) ;
#57926 = CARTESIAN_POINT ( 'NONE',  ( 63.01563776193091826, 13.70579113808095073, 2.968410348757589468 ) ) ;
#57927 = PLANE ( 'NONE',  #25041 ) ;
#57928 = ORIENTED_EDGE ( 'NONE', *, *, #5920, .T. ) ;
#57929 = CARTESIAN_POINT ( 'NONE',  ( -62.15799747763098537, 16.70234469631018115, -18.32392564386741896 ) ) ;
#57930 = CARTESIAN_POINT ( 'NONE',  ( -128.1267916618074594, 49.19573276651588145, -62.08358998231160797 ) ) ;
#57931 = CARTESIAN_POINT ( 'NONE',  ( 61.40360494384000845, 12.30429482808983721, -89.57394958506790772 ) ) ;
#57932 = LINE ( 'NONE', #62164, #33647 ) ;
#57933 = CARTESIAN_POINT ( 'NONE',  ( -95.04120270830171080, 29.25306318840327791, -67.33052735652132981 ) ) ;
#57934 = VERTEX_POINT ( 'NONE', #39168 ) ;
#57935 = VERTEX_POINT ( 'NONE', #1170 ) ;
#57936 = CARTESIAN_POINT ( 'NONE',  ( 188.0141161196705752, 85.90515114331887503, -67.68764559524167623 ) ) ;
#57937 = DIRECTION ( 'NONE',  ( 1.000000000000000000, 0.000000000000000000, 0.000000000000000000 ) ) ;
#57938 = PLANE ( 'NONE',  #32902 ) ;
#57939 = DIRECTION ( 'NONE',  ( -0.000000000000000000, -1.000000000000000000, -0.000000000000000000 ) ) ;
#57940 = CARTESIAN_POINT ( 'NONE',  ( -75.43495400358861502, 22.18831810339349886, 31.14574269627557612 ) ) ;
#57941 = ADVANCED_FACE ( 'NONE', ( #12079 ), #54625, .T. ) ;
#57942 = CARTESIAN_POINT ( 'NONE',  ( 81.74909803672915132, 17.81295302817862947, 31.49550494790652522 ) ) ;
#57943 = CARTESIAN_POINT ( 'NONE',  ( 0.01688885742776611437, 6.535341423375590431, -4.680456609903974829 ) ) ;
#57944 = DIRECTION ( 'NONE',  ( -7.703719777548945123E-34, -1.479221584281240009E-31, 1.000000000000000000 ) ) ;
#57945 = CARTESIAN_POINT ( 'NONE',  ( -165.9122696334865168, 79.44688201528255433, -71.14683853636709898 ) ) ;
#57946 = ORIENTED_EDGE ( 'NONE', *, *, #11506, .F. ) ;
#57947 = CARTESIAN_POINT ( 'NONE',  ( -109.7078892845591582, 36.71702188566215597, -14.59872168737284781 ) ) ;
#57948 = ORIENTED_EDGE ( 'NONE', *, *, #22384, .T. ) ;
#57949 = ADVANCED_FACE ( 'NONE', ( #33188 ), #12426, .T. ) ;
#57950 = CARTESIAN_POINT ( 'NONE',  ( -180.5668408223793904, 95.81768001203278118, -95.00000000000133582 ) ) ;
#57951 = CARTESIAN_POINT ( 'NONE',  ( 183.2136430849848239, 6.000000000000000000, -14.43565316649556074 ) ) ;
#57952 = CARTESIAN_POINT ( 'NONE',  ( 39.48989092546764823, -13.48566889876655672, 13.79046412312118974 ) ) ;
#57953 = LINE ( 'NONE', #69190, #41135 ) ;
#57955 = LINE ( 'NONE', #62193, #19251 ) ;
#57954 = AXIS2_PLACEMENT_3D ( 'NONE', #50599, #61158, #2080 ) ;
#57956 = CARTESIAN_POINT ( 'NONE',  ( 31.90217595456442012, 7.552213897210513949, 11.06335214983522874 ) ) ;
#57957 = LINE ( 'NONE', #47731, #45754 ) ;
#57958 = CARTESIAN_POINT ( 'NONE',  ( -38.45778834351241926, 11.87434869453507247, -13.31764495626525857 ) ) ;
#57959 = AXIS2_PLACEMENT_3D ( 'NONE', #33240, #13175, #33591 ) ;
#57960 = VECTOR ( 'NONE', #2899, 1000.000000000000000 ) ;
#57961 = ORIENTED_EDGE ( 'NONE', *, *, #15549, .F. ) ;
#57962 = FACE_OUTER_BOUND ( 'NONE', #41432, .T. ) ;
#57963 = EDGE_LOOP ( 'NONE', ( #28548, #16385, #18884, #35637 ) ) ;
#57964 = PRODUCT_DEFINITION_FORMATION_WITH_SPECIFIED_SOURCE ( 'ANY', '', #26510, .NOT_KNOWN. ) ;
#57965 = DIRECTION ( 'NONE',  ( 0.000000000000000000, 0.000000000000000000, -1.000000000000000000 ) ) ;
#57966 = CARTESIAN_POINT ( 'NONE',  ( -27.70562707895079768, 9.007984652865420827, 4.348468677708457797 ) ) ;
#57967 = EDGE_CURVE ( 'NONE', #65564, #56288, #25078, .T. ) ;
#57968 = CARTESIAN_POINT ( 'NONE',  ( 45.82394788922798767, 46.11928342727497210, 170.0000000000000000 ) ) ;
#57969 = AXIS2_PLACEMENT_3D ( 'NONE', #36990, #53833, #68320 ) ;
#57970 = CARTESIAN_POINT ( 'NONE',  ( -55.05276343752910151, 14.68156374112637330, -88.90542517938719413 ) ) ;
#57971 = CARTESIAN_POINT ( 'NONE',  ( -96.43148989374459745, 29.90755650959363621, -10.94842023032891376 ) ) ;
#57972 = EDGE_CURVE ( 'NONE', #66237, #32020, #54973, .T. ) ;
#57973 = CARTESIAN_POINT ( 'NONE',  ( 154.0515132159917755, 56.29926936869309628, -50.31581255231360927 ) ) ;
#57974 = VECTOR ( 'NONE', #21094, 1000.000000000000000 ) ;
#57975 = ADVANCED_FACE ( 'NONE', ( #49687 ), #27902, .F. ) ;
#57976 = ORIENTED_EDGE ( 'NONE', *, *, #3399, .F. ) ;
#57977 = CARTESIAN_POINT ( 'NONE',  ( 620.5071894358228519, 928.5915846175158777, 663.5068267248771008 ) ) ;
#57978 = ADVANCED_FACE ( 'NONE', ( #34236 ), #1885, .T. ) ;
#57979 = CARTESIAN_POINT ( 'NONE',  ( 31.11269837220803325, -10.55634918610409656, 0.000000000000000000 ) ) ;
#57980 = CARTESIAN_POINT ( 'NONE',  ( 173.7225111622554437, 72.84868911716897344, -15.41689420582882697 ) ) ;
#57981 = DIRECTION ( 'NONE',  ( 0.000000000000000000, 0.000000000000000000, 1.000000000000000000 ) ) ;
#57982 = CARTESIAN_POINT ( 'NONE',  ( -128.1282195935087600, 49.19720162550164844, -49.57677375076018222 ) ) ;
#57983 = ORIENTED_EDGE ( 'NONE', *, *, #809, .F. ) ;
#57984 = CARTESIAN_POINT ( 'NONE',  ( -178.2328124332056518, 94.56955476227570045, -74.56460458710455441 ) ) ;
#57985 = CARTESIAN_POINT ( 'NONE',  ( -0.8055628312658243972, 6.535476276302841114, -18.72534061433564290 ) ) ;
#57986 = CARTESIAN_POINT ( 'NONE',  ( 204.3750762779230001, 107.6105286537017207, -90.01503221354896311 ) ) ;
#57987 = LINE ( 'NONE', #40767, #40538 ) ;
#57988 = CARTESIAN_POINT ( 'NONE',  ( 135.6651581599210203, 42.52720121194704461, 29.72801099383555723 ) ) ;
#57989 = ADVANCED_FACE ( 'NONE', ( #18740 ), #8541, .F. ) ;
#57990 = ORIENTED_EDGE ( 'NONE', *, *, #55401, .T. ) ;
#57991 = CARTESIAN_POINT ( 'NONE',  ( -149.5074843970971017, 64.17983161892347255, 45.72082123989907387 ) ) ;
#57992 = DIRECTION ( 'NONE',  ( 0.000000000000000000, 0.000000000000000000, -1.000000000000000000 ) ) ;
#57993 = CARTESIAN_POINT ( 'NONE',  ( 186.7642514597453385, 86.02880938169742819, 41.71253118051657083 ) ) ;
#57994 = CARTESIAN_POINT ( 'NONE',  ( 162.0812592823605485, 62.62783216273698628, 15.99956616506345952 ) ) ;
#57995 = DIRECTION ( 'NONE',  ( -1.000000000000000000, 0.000000000000000000, 0.000000000000000000 ) ) ;
#57996 = ADVANCED_FACE ( 'NONE', ( #61985 ), #45466, .T. ) ;
#57997 = EDGE_CURVE ( 'NONE', #11610, #27523, #40882, .T. ) ;
#57998 = ORIENTED_EDGE ( 'NONE', *, *, #16773, .F. ) ;
#57999 = CARTESIAN_POINT ( 'NONE',  ( 181.0840389613909736, 80.03940679743415387, 17.46404351504774866 ) ) ;
#58000 = VERTEX_POINT ( 'NONE', #62697 ) ;
#58001 = VECTOR ( 'NONE', #12697, 1000.000000000000000 ) ;
#58002 = CARTESIAN_POINT ( 'NONE',  ( 31.11269837220803325, -10.55634918610409656, 0.000000000000000000 ) ) ;
#58003 = CARTESIAN_POINT ( 'NONE',  ( 70.45466089417030275, 14.52203022703030832, -69.07882228772790256 ) ) ;
#58004 = CARTESIAN_POINT ( 'NONE',  ( -62.30463872474475551, 16.74658165105247676, 35.83966074286138337 ) ) ;
#58006 = VERTEX_POINT ( 'NONE', #56366 ) ;
#58005 = PLANE ( 'NONE',  #57870 ) ;
#58007 = CARTESIAN_POINT ( 'NONE',  ( -174.7869898116916545, 88.99756909636809610, 45.68310981282044025 ) ) ;
#58008 = CARTESIAN_POINT ( 'NONE',  ( 75.31295361348104223, 1.012249897501722014E-14, -2.499999999999970246 ) ) ;
#58009 = CARTESIAN_POINT ( 'NONE',  ( 110.7117404013331452, 30.20916032354563185, -50.92243756565370916 ) ) ;
#58010 = VECTOR ( 'NONE', #38068, 1000.000000000000000 ) ;
#58011 = ORIENTED_EDGE ( 'NONE', *, *, #50575, .F. ) ;
#58012 = PLANE ( 'NONE',  #31700 ) ;
#58013 = CARTESIAN_POINT ( 'NONE',  ( -40.99999999999996447, 0.000000000000000000, -6.071532165918820097E-15 ) ) ;
#58014 = CARTESIAN_POINT ( 'NONE',  ( 51.65020379092739944, 1.250000000000015099, 26.66469066592269499 ) ) ;
#58015 = VECTOR ( 'NONE', #26115, 1000.000000000000000 ) ;
#58016 = DIRECTION ( 'NONE',  ( 1.000000000000000000, 0.000000000000000000, 0.000000000000000000 ) ) ;
#58017 = DIRECTION ( 'NONE',  ( 0.000000000000000000, 0.000000000000000000, 1.000000000000000000 ) ) ;
#58018 = CARTESIAN_POINT ( 'NONE',  ( 153.4268936273268480, 54.57409659828383752, 57.43301500385714320 ) ) ;
#58019 = CARTESIAN_POINT ( 'NONE',  ( 450.2085304802404835, 190.0000000000000000, -219.9999999999999147 ) ) ;
#58020 = ORIENTED_EDGE ( 'NONE', *, *, #20955, .F. ) ;
#58021 = CARTESIAN_POINT ( 'NONE',  ( -9.779603649692301559, 8.034615131607075966, 71.71790837464678248 ) ) ;
#58022 = ORIENTED_EDGE ( 'NONE', *, *, #57109, .F. ) ;
#58023 = CARTESIAN_POINT ( 'NONE',  ( 155.7265855639938650, 57.57443315515121895, -24.08749366127067049 ) ) ;
#58024 = CARTESIAN_POINT ( 'NONE',  ( 210.0055645826033981, 115.7254585628714523, -22.30316490195718160 ) ) ;
#58025 = DIRECTION ( 'NONE',  ( -0.8118923937861950435, -0.5838071093367415143, 0.000000000000000000 ) ) ;
#58026 = CARTESIAN_POINT ( 'NONE',  ( -154.0718453320783112, 68.14976693162391541, -75.11313154428037819 ) ) ;
#58027 = CARTESIAN_POINT ( 'NONE',  ( 56.03258084883530188, 11.16066123285296641, 93.81981338172488449 ) ) ;
#58028 = CARTESIAN_POINT ( 'NONE',  ( 181.0840389613909736, 80.03940679743415387, 17.46404351504774866 ) ) ;
#58029 = CARTESIAN_POINT ( 'NONE',  ( 209.5118425285948547, 113.1852661712287329, -38.07046045544934998 ) ) ;
#58030 = CARTESIAN_POINT ( 'NONE',  ( -78.66644367742111399, -170.0000000000000000, 37.91820113967311556 ) ) ;
#58031 = EDGE_LOOP ( 'NONE', ( #38627, #45738, #20083, #24516 ) ) ;
#58032 = ADVANCED_FACE ( 'NONE', ( #34924 ), #8575, .T. ) ;
#58033 = DIRECTION ( 'NONE',  ( -0.000000000000000000, 1.000000000000000000, -0.000000000000000000 ) ) ;
#58034 = ORIENTED_EDGE ( 'NONE', *, *, #49853, .T. ) ;
#58035 = CARTESIAN_POINT ( 'NONE',  ( -72.21889834709581635, 21.03534256744171671, 68.62594976653699064 ) ) ;
#58036 = CARTESIAN_POINT ( 'NONE',  ( 204.6977192012829789, 106.3443248447423599, -78.17048162308530834 ) ) ;
#58037 = CARTESIAN_POINT ( 'NONE',  ( 56.53776994993147298, 11.26292242501182450, -66.27727168919989253 ) ) ;
#58038 = CARTESIAN_POINT ( 'NONE',  ( 0.000000000000000000, 0.000000000000000000, -2.499999999999970246 ) ) ;
#58039 = CARTESIAN_POINT ( 'NONE',  ( -31.43908319763709969, 9.591432048623756756, -89.00629854612920155 ) ) ;
#58040 = CARTESIAN_POINT ( 'NONE',  ( -149.5074843970971301, -170.0000000000000000, 72.56537183036277838 ) ) ;
#58041 = CARTESIAN_POINT ( 'NONE',  ( -102.2801239173131052, 33.91021738430207222, -8.170026674512225640 ) ) ;
#58042 = ORIENTED_EDGE ( 'NONE', *, *, #47796, .T. ) ;
#58043 = CARTESIAN_POINT ( 'NONE',  ( -71.21970990337014484, 19.62334883444994560, 63.73658943180317493 ) ) ;
#58044 = CARTESIAN_POINT ( 'NONE',  ( -2.368959188627552503, -24.88750755625419941, 0.000000000000000000 ) ) ;
#58045 = ORIENTED_EDGE ( 'NONE', *, *, #11570, .T. ) ;
#58046 = ORIENTED_EDGE ( 'NONE', *, *, #15115, .T. ) ;
#58047 = ADVANCED_FACE ( 'NONE', ( #67297 ), #30680, .F. ) ;
#58048 = EDGE_CURVE ( 'NONE', #18940, #11337, #63596, .T. ) ;
#58049 = CARTESIAN_POINT ( 'NONE',  ( -157.0069704378501569, 70.81086990254192415, 38.80300155337447165 ) ) ;
#58050 = CARTESIAN_POINT ( 'NONE',  ( 59.72897338775216269, 11.93428797217974768, -49.96663325469457817 ) ) ;
#58051 = CARTESIAN_POINT ( 'NONE',  ( 442.3372781065089612, 367.0710678118721262, -141.4497041420121377 ) ) ;
#58052 = EDGE_CURVE ( 'NONE', #60277, #44118, #52128, .T. ) ;
#58053 = VECTOR ( 'NONE', #26113, 1000.000000000000000 ) ;
#58054 =( NAMED_UNIT ( * ) SI_UNIT ( $, .STERADIAN. ) SOLID_ANGLE_UNIT ( ) );
#58055 = B_SPLINE_CURVE_WITH_KNOTS ( 'NONE', 3,
 ( #50074, #49356, #44804, #7529, #65932, #17727, #28979, #64863, #17003, #39185, #23694, #1189, #65566, #38472, #59913, #11734, #60627, #16666, #38119, #54644, #12443, #33903, #7166, #17357, #38834, #40554, #3282, #56389, #13149, #8208, #24740, #61667, #9245, #67648, #50764, #3969, #67315, #2585, #56048, #19100, #19444, #39866, #34613, #30012, #41261, #35977 ),
 .UNSPECIFIED., .F., .F.,
 ( 4, 2, 2, 2, 2, 2, 2, 2, 2, 2, 2, 2, 2, 2, 2, 2, 2, 2, 2, 2, 2, 2, 4 ),
 ( 0.000000000000000000, 0.003373244802897278679, 0.004216556003621594988, 0.005059867204345911730, 0.006746489605794545215, 0.007589800806518857620, 0.008433112007243172628, 0.009276423207967485901, 0.01011973440869179917, 0.01180635681014042572, 0.01349297921158905053, 0.01433629041231336033, 0.01517960161303767187, 0.01686622401448626893, 0.01770953521521054924, 0.01855284641593482955, 0.02023946881738342488, 0.02108278001810769825, 0.02192609121883197509, 0.02361271362028052878, 0.02445602482100480216, 0.02529933602172907553, 0.02698595842317762922 ),
 .UNSPECIFIED. ) ;
#58056 = CARTESIAN_POINT ( 'NONE',  ( -144.2188519266539970, 59.82027639618912929, 6.052588554004912247 ) ) ;
#58057 = EDGE_CURVE ( 'NONE', #57368, #33912, #51451, .T. ) ;
#58058 = CIRCLE ( 'NONE', #41237, 5.000000000000004441 ) ;
#58059 = ORIENTED_EDGE ( 'NONE', *, *, #11970, .F. ) ;
#58060 = DIRECTION ( 'NONE',  ( 0.04486483035051862939, -0.9989930665413143673, 0.000000000000000000 ) ) ;
#58061 = VECTOR ( 'NONE', #67007, 1000.000000000000000 ) ;
#58062 = VERTEX_POINT ( 'NONE', #56722 ) ;
#58063 = CARTESIAN_POINT ( 'NONE',  ( 210.0292194063021896, 113.9511645670926470, 15.14336717752075323 ) ) ;
#58064 = CARTESIAN_POINT ( 'NONE',  ( -142.0860844253782886, 59.41107357617636353, 37.10142862026528121 ) ) ;
#58065 = CARTESIAN_POINT ( 'NONE',  ( -439.4229916354183274, 394.9999999999998295, 96.05029585798874336 ) ) ;
#58066 = CARTESIAN_POINT ( 'NONE',  ( -6.125624616441583292, 7.794071945221088704, 71.76905348450266331 ) ) ;
#58067 = CIRCLE ( 'NONE', #35734, 65.00000000000000000 ) ;
#58068 = VECTOR ( 'NONE', #62245, 1000.000000000000000 ) ;
#58069 = ORIENTED_EDGE ( 'NONE', *, *, #52443, .F. ) ;
#58070 = VERTEX_POINT ( 'NONE', #13129 ) ;
#58071 = CARTESIAN_POINT ( 'NONE',  ( 111.6144526446208403, -21.48289790755741890, -4.743601953786281911 ) ) ;
#58072 = CARTESIAN_POINT ( 'NONE',  ( -123.7116175647536096, 46.27018554618426549, 84.61033409315344045 ) ) ;
#58073 = CARTESIAN_POINT ( 'NONE',  ( 32.66364305947234214, 8.639871491745250154, -66.63435592309144795 ) ) ;
#58074 = CARTESIAN_POINT ( 'NONE',  ( 141.0645618855930365, 45.95036951196540542, -72.50746714427457107 ) ) ;
#58075 = CARTESIAN_POINT ( 'NONE',  ( 66.30567821786755189, 13.45988234822860896, 44.05720671718261627 ) ) ;
#58076 = EDGE_CURVE ( 'NONE', #26121, #40620, #25820, .T. ) ;
#58077 = CARTESIAN_POINT ( 'NONE',  ( 8.401684033729910794, 7.382743251898692627, 92.54379397006360364 ) ) ;
#58078 = VERTEX_POINT ( 'NONE', #29292 ) ;
#58079 = EDGE_CURVE ( 'NONE', #66442, #22625, #67979, .T. ) ;
#58080 = FACE_OUTER_BOUND ( 'NONE', #53933, .T. ) ;
#58081 = CARTESIAN_POINT ( 'NONE',  ( -95.88718821240198054, 29.65015105908826953, 60.93360808619399904 ) ) ;
#58082 = ORIENTED_EDGE ( 'NONE', *, *, #15240, .T. ) ;
#58083 = CARTESIAN_POINT ( 'NONE',  ( -86.17927978631389863, 25.32700573188346738, 11.08567002189708717 ) ) ;
#58084 = ORIENTED_EDGE ( 'NONE', *, *, #94, .T. ) ;
#58085 = ORIENTED_EDGE ( 'NONE', *, *, #12162, .F. ) ;
#58086 = ORIENTED_EDGE ( 'NONE', *, *, #35735, .T. ) ;
#58087 = CARTESIAN_POINT ( 'NONE',  ( 9.290502160020462696, 6.379616279862541539, -46.77255880539932065 ) ) ;
#58088 = DIRECTION ( 'NONE',  ( 0.000000000000000000, -1.000000000000000000, 0.000000000000000000 ) ) ;
#58089 = CARTESIAN_POINT ( 'NONE',  ( 16.77391662606470746, 6.533867394142989227, 18.12154318931471408 ) ) ;
#58090 = VERTEX_POINT ( 'NONE', #14497 ) ;
#58091 = CARTESIAN_POINT ( 'NONE',  ( -27.21071548940745544, 8.935354224959075609, 85.20262481687709055 ) ) ;
#58092 = CIRCLE ( 'NONE', #20989, 5.000000000000004441 ) ;
#58093 = LINE ( 'NONE', #26085, #17415 ) ;
#58094 = PLANE ( 'NONE',  #30311 ) ;
#58095 = CARTESIAN_POINT ( 'NONE',  ( 181.0840389613909736, -170.0000000000000000, -43.72505766587962484 ) ) ;
#58096 = CARTESIAN_POINT ( 'NONE',  ( -28.13266652174639759, 9.071935854491412599, 44.45274732610694457 ) ) ;
#58097 = VECTOR ( 'NONE', #59339, 1000.000000000000000 ) ;
#58098 = CARTESIAN_POINT ( 'NONE',  ( -142.9843132609581744, 60.12226089556227038, -65.44703247124222401 ) ) ;
#58099 = ORIENTED_EDGE ( 'NONE', *, *, #47563, .T. ) ;
#58100 = VECTOR ( 'NONE', #13706, 1000.000000000000000 ) ;
#58101 = PRODUCT_DEFINITION ( 'UNKNOWN', '', #17593, #5692 ) ;
#58102 = DIRECTION ( 'NONE',  ( 0.000000000000000000, 0.000000000000000000, -1.000000000000000000 ) ) ;
#58103 = CARTESIAN_POINT ( 'NONE',  ( -81.89510452344296709, 24.66033552777454929, -76.24616494515825593 ) ) ;
#58104 = CARTESIAN_POINT ( 'NONE',  ( -4.530419073632062421, 6.697511735426034285, -89.81587080412703017 ) ) ;
#58105 = DIRECTION ( 'NONE',  ( -0.9749279121818227312, -0.2225209339563184729, 2.500042656554810833E-16 ) ) ;
#58106 = CARTESIAN_POINT ( 'NONE',  ( 50.97490815085634352, 6.000000000000000000, -4.435653166495503896 ) ) ;
#58107 = VECTOR ( 'NONE', #19717, 1000.000000000000000 ) ;
#58108 = CARTESIAN_POINT ( 'NONE',  ( 126.6576865394845584, 37.24426596493989194, 12.28561084184393870 ) ) ;
#58109 = CARTESIAN_POINT ( 'NONE',  ( 36.57758730571628547, 8.058950843173096956, -89.85795502034081039 ) ) ;
#58110 = DIRECTION ( 'NONE',  ( 0.000000000000000000, 0.000000000000000000, 1.000000000000000000 ) ) ;
#58111 = EDGE_CURVE ( 'NONE', #37531, #27576, #35954, .T. ) ;
#58112 = CARTESIAN_POINT ( 'NONE',  ( 66.94779593213119995, 13.61918177102165650, 16.85966954521656547 ) ) ;
#58113 = CARTESIAN_POINT ( 'NONE',  ( -79.62207341875654265, 23.76621716825510688, 72.21703032857082860 ) ) ;
#58114 = CARTESIAN_POINT ( 'NONE',  ( -102.2801239173131052, 32.78103895658057354, 30.51907450641510522 ) ) ;
#58115 = ORIENTED_EDGE ( 'NONE', *, *, #40365, .T. ) ;
#58116 = AXIS2_PLACEMENT_3D ( 'NONE', #9313, #58186, #63125 ) ;
#58117 = EDGE_CURVE ( 'NONE', #48269, #39558, #53470, .T. ) ;
#58118 = ITEM_DEFINED_TRANSFORMATION ( 'NONE', 'NONE', #61280,  #66832 ) ;
#58119 = CARTESIAN_POINT ( 'NONE',  ( -52.01032469896254185, 14.92508508686765367, 84.64386905501486069 ) ) ;
#58120 = VERTEX_POINT ( 'NONE', #4625 ) ;
#58121 = CARTESIAN_POINT ( 'NONE',  ( 149.0250918491436494, 6.000000000000000000, -46.68900338898718161 ) ) ;
#58122 = EDGE_LOOP ( 'NONE', ( #23163, #49148, #56723, #23500 ) ) ;
#58123 = CARTESIAN_POINT ( 'NONE',  ( 17.48988570800758424, 7.568061572928496794, -62.55499197079009122 ) ) ;
#58124 = DIRECTION ( 'NONE',  ( 1.000000000000000000, 0.000000000000000000, -1.697894969632809662E-16 ) ) ;
#58125 = FACE_OUTER_BOUND ( 'NONE', #8752, .T. ) ;
#58126 = CARTESIAN_POINT ( 'NONE',  ( 63.49940197359692462, 12.78497925206075969, -23.87614024170608573 ) ) ;
#58127 = CARTESIAN_POINT ( 'NONE',  ( 136.9654665832768501, 44.52067472585216734, -36.69392891266659262 ) ) ;
#58128 = CARTESIAN_POINT ( 'NONE',  ( 32.09567473596477072, 7.571373529017937365, -41.40819426019592697 ) ) ;
#58129 = DIRECTION ( 'NONE',  ( -1.000000000000000000, 0.000000000000000000, 0.000000000000000000 ) ) ;
#58130 = DIRECTION ( 'NONE',  ( 0.000000000000000000, 0.000000000000000000, 1.000000000000000000 ) ) ;
#58131 = DIRECTION ( 'NONE',  ( -0.000000000000000000, -0.000000000000000000, -1.000000000000000000 ) ) ;
#58132 = EDGE_LOOP ( 'NONE', ( #65748, #67896, #6975, #41297 ) ) ;
#58133 = VERTEX_POINT ( 'NONE', #20122 ) ;
#58134 = ADVANCED_FACE ( 'NONE', ( #42606 ), #37318, .T. ) ;
#58135 = CARTESIAN_POINT ( 'NONE',  ( 175.3045235163616837, 74.34220674874238455, 85.66341389582093768 ) ) ;
#58136 = LINE ( 'NONE', #8918, #51037 ) ;
#58137 = CARTESIAN_POINT ( 'NONE',  ( 25.39413431650373099, 1.224646799147353059E-15, -5.000000000000000000 ) ) ;
#58138 = EDGE_CURVE ( 'NONE', #61651, #13178, #17536, .T. ) ;
#58139 = EDGE_CURVE ( 'NONE', #35639, #56892, #44507, .T. ) ;
#58140 = FACE_OUTER_BOUND ( 'NONE', #12617, .T. ) ;
#58141 = CARTESIAN_POINT ( 'NONE',  ( 280.3314448577247049, 21.42428528562853529, 4.999999999999991118 ) ) ;
#58142 = FACE_OUTER_BOUND ( 'NONE', #48988, .T. ) ;
#58143 = CARTESIAN_POINT ( 'NONE',  ( -65.36598343705435354, 0.000000000000000000, 41.38025477438755928 ) ) ;
#58144 = VECTOR ( 'NONE', #45889, 1000.000000000000114 ) ;
#58145 = CARTESIAN_POINT ( 'NONE',  ( -4.999999999999922728, 51.66904755831208718, 0.000000000000000000 ) ) ;
#58146 = CARTESIAN_POINT ( 'NONE',  ( 89.87518614971250486, 20.55373388674512825, -23.25513048290722296 ) ) ;
#58147 = FACE_OUTER_BOUND ( 'NONE', #45801, .T. ) ;
#58148 = CARTESIAN_POINT ( 'NONE',  ( 7.762887554996211747E-14, 46.66904755831208718, 85.00100000000000477 ) ) ;
#58149 = DIRECTION ( 'NONE',  ( 0.000000000000000000, -1.000000000000000000, 0.000000000000000000 ) ) ;
#58150 =( BOUNDED_CURVE ( )  B_SPLINE_CURVE ( 3, ( #18537, #60402, #34727, #39989 ),
 .UNSPECIFIED., .F., .F. ) 
 B_SPLINE_CURVE_WITH_KNOTS ( ( 4, 4 ),
 ( 2.506209174768084580, 3.776976132411492326 ),
 .UNSPECIFIED. ) 
 CURVE ( )  GEOMETRIC_REPRESENTATION_ITEM ( )  RATIONAL_B_SPLINE_CURVE ( ( 1.000000000000000000, 0.8698961108463052483, 0.8698961108463052483, 1.000000000000000000 ) ) 
 REPRESENTATION_ITEM ( '' )  );
#58151 = ORIENTED_EDGE ( 'NONE', *, *, #39858, .F. ) ;
#58152 = CARTESIAN_POINT ( 'NONE',  ( 126.7877523219523539, 38.47018873135925077, 12.72568023100204293 ) ) ;
#58153 = CARTESIAN_POINT ( 'NONE',  ( -17.50000000000002842, 207.5000000000000284, -2.000000000000000000 ) ) ;
#58154 = DIRECTION ( 'NONE',  ( -0.000000000000000000, 1.000000000000000000, -0.000000000000000000 ) ) ;
#58155 = CARTESIAN_POINT ( 'NONE',  ( -2.113472939309121834, -74.92159864268212743, 41.38025477438755928 ) ) ;
#58156 = CARTESIAN_POINT ( 'NONE',  ( -47.95193882091084703, 12.89180642785319009, -45.18069670428837270 ) ) ;
#58157 = CARTESIAN_POINT ( 'NONE',  ( -49.42000000000000171, -26.09918303830819397, 15.41169613715280562 ) ) ;
#58158 = STYLED_ITEM ( 'NONE', ( #2217 ), #63029 ) ;
#58159 = VERTEX_POINT ( 'NONE', #41573 ) ;
#58160 = EDGE_CURVE ( 'NONE', #68068, #5133, #18654, .T. ) ;
#58161 = PLANE ( 'NONE',  #54976 ) ;
#58162 = LINE ( 'NONE', #5385, #57414 ) ;
#58163 = EDGE_LOOP ( 'NONE', ( #21438, #26003, #49391, #6262 ) ) ;
#58164 = AXIS2_PLACEMENT_3D ( 'NONE', #58614, #15025, #10429 ) ;
#58165 = EDGE_LOOP ( 'NONE', ( #33306, #34143, #37898, #7160 ) ) ;
#58166 = CARTESIAN_POINT ( 'NONE',  ( 32.99392442438140449, 8.673943046035248017, 94.99999999999866418 ) ) ;
#58167 = CARTESIAN_POINT ( 'NONE',  ( -180.3158531669106139, 95.51092859788505507, -71.19633455476439110 ) ) ;
#58168 = CARTESIAN_POINT ( 'NONE',  ( 136.8043112934651617, 44.41959649939953181, -90.31326922588782224 ) ) ;
#58169 = ORIENTED_EDGE ( 'NONE', *, *, #55277, .T. ) ;
#58170 = FACE_BOUND ( 'NONE', #17164, .T. ) ;
#58171 = DIRECTION ( 'NONE',  ( -0.3930250316539148359, -0.9195277725514544587, 0.000000000000000000 ) ) ;
#58172 = CARTESIAN_POINT ( 'NONE',  ( 32.14349651933086705, 7.576119504381661152, -18.22641918543651585 ) ) ;
#58173 = CARTESIAN_POINT ( 'NONE',  ( 180.2565361171341181, 79.19912802278405195, -51.19124638010620032 ) ) ;
#58174 = CARTESIAN_POINT ( 'NONE',  ( 162.0913721763116087, 61.33513738594646725, 84.68278974389512825 ) ) ;
#58175 = CARTESIAN_POINT ( 'NONE',  ( 0.000000000000000000, 0.000000000000000000, 0.000000000000000000 ) ) ;
#58176 = ORIENTED_EDGE ( 'NONE', *, *, #54467, .F. ) ;
#58177 = CARTESIAN_POINT ( 'NONE',  ( 110.2429982417149432, 29.99119854320847267, -24.07788697519002596 ) ) ;
#58178 = CARTESIAN_POINT ( 'NONE',  ( 15.29899606819417279, 6.485153354884285015, 56.85925826316891118 ) ) ;
#58179 = CARTESIAN_POINT ( 'NONE',  ( 12.04188192036245297, 7.416006018508747744, 31.01281317854670760 ) ) ;
#58180 = CARTESIAN_POINT ( 'NONE',  ( 199.3764173596861724, 100.9540560740992134, 31.39806225150986663 ) ) ;
#58181 = CARTESIAN_POINT ( 'NONE',  ( 15.55634918610403261, -3.079134169858832593E-14, 85.00100000000000477 ) ) ;
#58183 = VERTEX_POINT ( 'NONE', #42937 ) ;
#58182 = CARTESIAN_POINT ( 'NONE',  ( -149.5074843970971301, -170.0000000000000000, 65.06537183036276417 ) ) ;
#58184 = ORIENTED_EDGE ( 'NONE', *, *, #66326, .F. ) ;
#58185 = VERTEX_POINT ( 'NONE', #4971 ) ;
#58186 = DIRECTION ( 'NONE',  ( 0.000000000000000000, 0.000000000000000000, 1.000000000000000000 ) ) ;
#58187 = PLANE ( 'NONE',  #55693 ) ;
#58188 = CYLINDRICAL_SURFACE ( 'NONE', #1330, 7.500000000000013323 ) ;
#58189 = EDGE_CURVE ( 'NONE', #28423, #15622, #31708, .T. ) ;
#58190 = CARTESIAN_POINT ( 'NONE',  ( -123.6619986853277879, 45.04188181212062148, 72.12840242753554776 ) ) ;
#58191 = AXIS2_PLACEMENT_3D ( 'NONE', #59245, #60300, #511 ) ;
#58192 = CARTESIAN_POINT ( 'NONE',  ( 150.0501577908836737, 52.10460126680128212, -69.34286162853243241 ) ) ;
#58193 = CARTESIAN_POINT ( 'NONE',  ( 22.86512557549835378, 7.838421172085543454, -94.18957475688611680 ) ) ;
#58194 = EDGE_CURVE ( 'NONE', #59496, #1313, #55709, .T. ) ;
#58195 = CARTESIAN_POINT ( 'NONE',  ( -35.00000000000000000, -35.00000000000000000, 0.000000000000000000 ) ) ;
#58196 = ORIENTED_EDGE ( 'NONE', *, *, #13276, .F. ) ;
#58197 = VERTEX_POINT ( 'NONE', #25416 ) ;
#58198 = AXIS2_PLACEMENT_3D ( 'NONE', #60837, #55558, #12658 ) ;
#58199 = DIRECTION ( 'NONE',  ( 0.000000000000000000, 0.000000000000000000, -1.000000000000000000 ) ) ;
#58200 = EDGE_CURVE ( 'NONE', #20027, #35779, #58772, .T. ) ;
#58201 = CARTESIAN_POINT ( 'NONE',  ( -83.53167274806556009, 25.32068190668983831, -36.88675501431261949 ) ) ;
#58202 = CARTESIAN_POINT ( 'NONE',  ( 102.8207208422076491, 25.59711495857310837, 89.66725988627140964 ) ) ;
#58203 = CARTESIAN_POINT ( 'NONE',  ( -156.6644740249450933, 71.86407434531903959, 9.117256437103197442 ) ) ;
#58204 = CARTESIAN_POINT ( 'NONE',  ( -62.31345272479909880, 18.49415068377641447, 170.0000000000000000 ) ) ;
#58205 = DIRECTION ( 'NONE',  ( -0.000000000000000000, -0.000000000000000000, 1.000000000000000000 ) ) ;
#58206 = DIRECTION ( 'NONE',  ( 1.000000000000000000, 1.387778780781444936E-16, 0.000000000000000000 ) ) ;
#58207 = EDGE_LOOP ( 'NONE', ( #64632, #55746, #7921 ) ) ;
#58208 = ORIENTED_EDGE ( 'NONE', *, *, #10223, .F. ) ;
#58209 = ORIENTED_EDGE ( 'NONE', *, *, #61795, .T. ) ;
#58210 = AXIS2_PLACEMENT_3D ( 'NONE', #5349, #12012, #26803 ) ;
#58211 = DIRECTION ( 'NONE',  ( -0.000000000000000000, -0.000000000000000000, -1.000000000000000000 ) ) ;
#58212 = CARTESIAN_POINT ( 'NONE',  ( 31.96192885395475614, 8.569232728322425885, -42.14181525861992839 ) ) ;
#58213 = EDGE_CURVE ( 'NONE', #13740, #34313, #51254, .T. ) ;
#58214 = DIRECTION ( 'NONE',  ( -1.000000000000000000, 0.000000000000000000, 0.000000000000000000 ) ) ;
#58215 = EDGE_CURVE ( 'NONE', #9408, #56892, #9000, .T. ) ;
#58216 = CARTESIAN_POINT ( 'NONE',  ( -35.38962320578854559, 11.29584325137389200, -63.28181392470004596 ) ) ;
#58217 = LINE ( 'NONE', #31830, #1538 ) ;
#58218 = ORIENTED_EDGE ( 'NONE', *, *, #37814, .F. ) ;
#58219 = FACE_OUTER_BOUND ( 'NONE', #19599, .T. ) ;
#58220 = CYLINDRICAL_SURFACE ( 'NONE', #58496, 7.500000000000013323 ) ;
#58221 =( NAMED_UNIT ( * ) SI_UNIT ( $, .STERADIAN. ) SOLID_ANGLE_UNIT ( ) );
#58222 = CARTESIAN_POINT ( 'NONE',  ( 22.28556289340101060, 7.803548444155008035, 6.915694015335128952 ) ) ;
#58223 = CARTESIAN_POINT ( 'NONE',  ( 12.99074365121421692, 21.50298515537768296, 0.000000000000000000 ) ) ;
#58224 = CARTESIAN_POINT ( 'NONE',  ( -119.6995109608660925, 42.54844499216736153, 7.039243325925482964 ) ) ;
#58225 = DIRECTION ( 'NONE',  ( -0.000000000000000000, -1.000000000000000000, -0.000000000000000000 ) ) ;
#58226 = CARTESIAN_POINT ( 'NONE',  ( 126.6576865394845584, 37.24426596493988484, -14.55893974861973916 ) ) ;
#58227 = LINE ( 'NONE', #37806, #22001 ) ;
#58228 = CARTESIAN_POINT ( 'NONE',  ( 11.82929895397812636, 7.412564870773630687, 4.295403894678821111 ) ) ;
#58229 = ORIENTED_EDGE ( 'NONE', *, *, #48174, .T. ) ;
#58230 = CARTESIAN_POINT ( 'NONE',  ( 181.9406741394862195, 79.47484497224793643, 17.42709078222137009 ) ) ;
#58231 = APPLICATION_PROTOCOL_DEFINITION ( 'draft international standard', 'automotive_design', 1998, #12058 ) ;
#58232 = CARTESIAN_POINT ( 'NONE',  ( 175.5406524085945534, 73.17873692326779178, 31.73118722595227936 ) ) ;
#58233 = DIRECTION ( 'NONE',  ( 1.000000000000000000, 0.000000000000000000, -0.000000000000000000 ) ) ;
#58234 = CARTESIAN_POINT ( 'NONE',  ( -109.7079446832839125, 37.86719386855315861, -43.58491357317385706 ) ) ;
#58235 = CARTESIAN_POINT ( 'NONE',  ( 187.2384682876462421, 86.54721710842892435, -39.40919725149962005 ) ) ;
#58236 = VERTEX_POINT ( 'NONE', #9573 ) ;
#58237 = ORIENTED_EDGE ( 'NONE', *, *, #57298, .T. ) ;
#58238 = DIRECTION ( 'NONE',  ( -0.000000000000000000, 1.000000000000000000, -0.000000000000000000 ) ) ;
#58239 = CARTESIAN_POINT ( 'NONE',  ( 173.5979703267912271, 71.35727699437038041, 89.88741889385630657 ) ) ;
#58240 = ORIENTED_EDGE ( 'NONE', *, *, #42935, .T. ) ;
#58241 = VECTOR ( 'NONE', #20508, 1000.000000000000000 ) ;
#58242 = CARTESIAN_POINT ( 'NONE',  ( 117.6865880453676283, 32.48051379280607165, 62.90051310914670779 ) ) ;
#58243 = ORIENTED_EDGE ( 'NONE', *, *, #22795, .T. ) ;
#58244 = DIRECTION ( 'NONE',  ( -1.000000000000000000, 0.000000000000000000, 0.000000000000000000 ) ) ;
#58245 = LINE ( 'NONE', #39146, #44082 ) ;
#58246 = AXIS2_PLACEMENT_3D ( 'NONE', #44924, #23130, #60753 ) ;
#58247 = DIRECTION ( 'NONE',  ( 1.000000000000000000, -0.000000000000000000, -0.000000000000000000 ) ) ;
#58248 = CARTESIAN_POINT ( 'NONE',  ( 161.3420394500905957, 60.72502592113882969, -90.87834266692578922 ) ) ;
#58249 = AXIS2_PLACEMENT_3D ( 'NONE', #36229, #15464, #58025 ) ;
#58250 = CARTESIAN_POINT ( 'NONE',  ( 0.000000000000000000, 0.000000000000000000, -2.499999999999970246 ) ) ;
#58252 = EDGE_LOOP ( 'NONE', ( #46143, #13239, #6152, #17193 ) ) ;
#58251 = FACE_OUTER_BOUND ( 'NONE', #57411, .T. ) ;
#58253 = CARTESIAN_POINT ( 'NONE',  ( 2.112947028649122760, -24.91054906769651112, 0.000000000000000000 ) ) ;
#58254 = ORIENTED_EDGE ( 'NONE', *, *, #29392, .T. ) ;
#58255 = ORIENTED_EDGE ( 'NONE', *, *, #51131, .T. ) ;
#58256 = CARTESIAN_POINT ( 'NONE',  ( -118.5043919384111746, 41.81711884544878899, -14.25870488645683842 ) ) ;
#58257 = CARTESIAN_POINT ( 'NONE',  ( 41.49663191311347532, 50.03028622612080767, 40.00000000000003553 ) ) ;
#58258 = CARTESIAN_POINT ( 'NONE',  ( -180.0179082103088035, 95.14811732286300128, -12.40625655228225988 ) ) ;
#58260 = VERTEX_POINT ( 'NONE', #47189 ) ;
#58259 = CARTESIAN_POINT ( 'NONE',  ( -148.6426981422629297, 63.44891673852537650, -49.77548511292598477 ) ) ;
#58261 = CARTESIAN_POINT ( 'NONE',  ( -106.0230121908585375, 35.86256082048880955, 85.20199266763809476 ) ) ;
#58262 = DIRECTION ( 'NONE',  ( -7.703719777548945123E-34, -1.479221584281240009E-31, 1.000000000000000000 ) ) ;
#58263 = ORIENTED_EDGE ( 'NONE', *, *, #14752, .T. ) ;
#58264 = CARTESIAN_POINT ( 'NONE',  ( -62.30100056228381789, 16.74548393487071607, -13.88027663460116123 ) ) ;
#58265 = EDGE_CURVE ( 'NONE', #145, #39302, #16578, .T. ) ;
#58266 = CARTESIAN_POINT ( 'NONE',  ( -125.8938041572051389, 47.69968343338780414, -61.75825448869760237 ) ) ;
#58267 = CARTESIAN_POINT ( 'NONE',  ( 0.000000000000000000, 0.000000000000000000, 85.00000000000000000 ) ) ;
#58268 = CARTESIAN_POINT ( 'NONE',  ( -95.04120270830166817, 29.25306318840326369, 13.20312441486970911 ) ) ;
#58269 = CARTESIAN_POINT ( 'NONE',  ( -101.8145602049406051, 32.54453702486151201, -61.85912785543960268 ) ) ;
#58270 = ORIENTED_EDGE ( 'NONE', *, *, #67137, .T. ) ;
#58271 = ORIENTED_EDGE ( 'NONE', *, *, #68136, .F. ) ;
#58272 = EDGE_CURVE ( 'NONE', #32966, #18071, #65821, .T. ) ;
#58273 = CARTESIAN_POINT ( 'NONE',  ( 188.2988323915788840, 86.21831227955483712, -68.49994268373441741 ) ) ;
#58274 = CARTESIAN_POINT ( 'NONE',  ( 427.4999999999999432, -18.06806526123148160, 0.000000000000000000 ) ) ;
#58275 = DIRECTION ( 'NONE',  ( 0.000000000000000000, -0.000000000000000000, -1.000000000000000000 ) ) ;
#58276 = CARTESIAN_POINT ( 'NONE',  ( 109.3154830994003675, 29.56170298203815250, -77.72415834473385132 ) ) ;
#58277 = CARTESIAN_POINT ( 'NONE',  ( -75.00636493611887090, 22.03142602679956852, 44.48221497804134117 ) ) ;
#58278 = CARTESIAN_POINT ( 'NONE',  ( -75.43271753227890031, 22.18711452892411273, -62.67581109114816940 ) ) ;
#58279 = CARTESIAN_POINT ( 'NONE',  ( -3.973643313806734888E-15, 6.732211846623391338, -4.339467034331192075 ) ) ;
#58280 = CARTESIAN_POINT ( 'NONE',  ( -120.1650841064593749, 44.02024060322521137, 42.96702436344589415 ) ) ;
#58281 = DIRECTION ( 'NONE',  ( 0.000000000000000000, -1.000000000000000000, 0.000000000000000000 ) ) ;
#58282 = ORIENTED_EDGE ( 'NONE', *, *, #32132, .F. ) ;
#58283 = CARTESIAN_POINT ( 'NONE',  ( 313.9975424824652350, 295.6904194069557548, 539.5330678552892323 ) ) ;
#58284 = ORIENTED_EDGE ( 'NONE', *, *, #48709, .T. ) ;
#58285 = CARTESIAN_POINT ( 'NONE',  ( -12.78015296493257935, 7.264294661536299103, -37.26654318863142379 ) ) ;
#58286 = CARTESIAN_POINT ( 'NONE',  ( 84.26390409839193296, 19.68678207880320485, 71.19001783865050470 ) ) ;
#58287 = CARTESIAN_POINT ( 'NONE',  ( 121.4242852856285566, 6.000000000000000000, -30.00000000000000000 ) ) ;
#58288 = EDGE_CURVE ( 'NONE', #42865, #38399, #41106, .T. ) ;
#58289 = CARTESIAN_POINT ( 'NONE',  ( 157.4703587214989113, 57.65129005721576050, -9.279633708673953763 ) ) ;
#58290 = DIRECTION ( 'NONE',  ( 0.5877852522924686962, 0.8090169943749506709, 5.102127870520021228E-18 ) ) ;
#58291 = AXIS2_PLACEMENT_3D ( 'NONE', #6439, #1871, #44771 ) ;
#58292 = VECTOR ( 'NONE', #20283, 1000.000000000000000 ) ;
#58293 = DIRECTION ( 'NONE',  ( -0.000000000000000000, -1.000000000000000000, -0.000000000000000000 ) ) ;
#58294 = CARTESIAN_POINT ( 'NONE',  ( 38.90894112122322213, 8.345444037631240874, -62.46436805589143404 ) ) ;
#58295 = CARTESIAN_POINT ( 'NONE',  ( -99.99439884168252490, 32.75762661251357599, -62.20012547770417655 ) ) ;
#58296 = CARTESIAN_POINT ( 'NONE',  ( -35.38962320578853138, 11.29584325137385292, -9.592712743772663586 ) ) ;
#58297 = CONICAL_SURFACE ( 'NONE', #26865, 2.999999999999981792, 0.7853981633974482790 ) ;
#58298 = EDGE_LOOP ( 'NONE', ( #30846, #40237, #67286, #52726 ) ) ;
#58299 = DIRECTION ( 'NONE',  ( -0.000000000000000000, 0.000000000000000000, -1.000000000000000000 ) ) ;
#58300 = ORIENTED_EDGE ( 'NONE', *, *, #62373, .T. ) ;
#58301 = CARTESIAN_POINT ( 'NONE',  ( 204.6977192012829505, 108.0580384837234931, -51.32593103262161094 ) ) ;
#58302 = CARTESIAN_POINT ( 'NONE',  ( -50.88541732109732862, -55.03078243218159571, 41.38025477438755928 ) ) ;
#58303 = CARTESIAN_POINT ( 'NONE',  ( -24.70354720400823112, 8.582324684301863016, 14.20767813331848117 ) ) ;
#58304 = DIRECTION ( 'NONE',  ( -0.000000000000000000, 1.000000000000000000, -0.000000000000000000 ) ) ;
#58305 = CARTESIAN_POINT ( 'NONE',  ( -11.14445507968271976, 7.129894202659276203, -76.49272796307144517 ) ) ;
#58306 = CARTESIAN_POINT ( 'NONE',  ( 31.11269837220809364, 15.55634918610396866, 85.00100000000000477 ) ) ;
#58307 = CARTESIAN_POINT ( 'NONE',  ( 149.9683128897950155, 53.28564708287392904, -43.09392792187862398 ) ) ;
#58308 = ORIENTED_EDGE ( 'NONE', *, *, #16732, .F. ) ;
#58309 = CARTESIAN_POINT ( 'NONE',  ( 403.0071894358329700, 629.9915846175134675, 794.5748919861035802 ) ) ;
#58310 = DIRECTION ( 'NONE',  ( 0.000000000000000000, 1.000000000000000000, -0.000000000000000000 ) ) ;
#58311 = CARTESIAN_POINT ( 'NONE',  ( 178.1965488566140152, 77.14488558164481447, -23.81576150532814040 ) ) ;
#58312 = CARTESIAN_POINT ( 'NONE',  ( -26.00000000000000000, 0.000000000000000000, -2.818925648462311923E-15 ) ) ;
#58313 = DIRECTION ( 'NONE',  ( -0.000000000000000000, -1.000000000000000000, -0.000000000000000000 ) ) ;
#58314 = ORIENTED_EDGE ( 'NONE', *, *, #50521, .T. ) ;
#58315 = CARTESIAN_POINT ( 'NONE',  ( -125.8938041572051389, -170.0000000000000000, -8.069153307770243089 ) ) ;
#58316 = CARTESIAN_POINT ( 'NONE',  ( -0.3258398948454893640, 6.518608385615800138, -16.57484821353645188 ) ) ;
#58317 = CARTESIAN_POINT ( 'NONE',  ( 198.2588776805010582, 99.52972231602376496, -20.83770437927799435 ) ) ;
#58318 = CARTESIAN_POINT ( 'NONE',  ( -155.7921081844114894, 69.69879669332561889, 87.80423241437721060 ) ) ;
#58319 = CARTESIAN_POINT ( 'NONE',  ( 135.4423125506059478, 42.39015362494588146, 29.67632823401072173 ) ) ;
#58320 = ORIENTED_EDGE ( 'NONE', *, *, #11464, .F. ) ;
#58321 = CARTESIAN_POINT ( 'NONE',  ( 15.55634918610396511, -46.66904755831214402, 0.000000000000000000 ) ) ;
#58322 = CARTESIAN_POINT ( 'NONE',  ( -149.5074843970971301, -170.0000000000000000, 11.37627064943538890 ) ) ;
#58323 = CARTESIAN_POINT ( 'NONE',  ( 181.9295958320008708, 80.90438706151871884, 29.34426735614494319 ) ) ;
#58324 = CARTESIAN_POINT ( 'NONE',  ( 154.0515132159917755, 56.29926936869308918, 30.21783921907742609 ) ) ;
#58325 = CARTESIAN_POINT ( 'NONE',  ( -42.52062419515534941, 29.34795682323898092, 26.66469066592269144 ) ) ;
#58326 = ORIENTED_EDGE ( 'NONE', *, *, #64005, .T. ) ;
#58327 = EDGE_CURVE ( 'NONE', #27213, #23613, #22194, .T. ) ;
#58328 = CARTESIAN_POINT ( 'NONE',  ( 173.8576514579035859, 72.97529922124009261, 65.68134040125295314 ) ) ;
#58329 = ORIENTED_EDGE ( 'NONE', *, *, #7472, .F. ) ;
#58330 = EDGE_CURVE ( 'NONE', #26077, #17896, #65461, .T. ) ;
#58331 = CARTESIAN_POINT ( 'NONE',  ( -109.5025362253418564, 36.60371748273998094, -40.42792366826092376 ) ) ;
#58332 = CARTESIAN_POINT ( 'NONE',  ( 68.45098769362921587, 13.99935947269945480, -75.23886394023182334 ) ) ;
#58333 = CARTESIAN_POINT ( 'NONE',  ( 0.000000000000000000, 0.000000000000000000, 41.38025477438755928 ) ) ;
#58334 = AXIS2_PLACEMENT_3D ( 'NONE', #30076, #4710, #40968 ) ;
#58336 = ORIENTED_EDGE ( 'NONE', *, *, #56793, .F. ) ;
#58335 = CARTESIAN_POINT ( 'NONE',  ( 155.7167524447090159, 57.56687707799950715, 17.37047274630594274 ) ) ;
#58337 = CARTESIAN_POINT ( 'NONE',  ( -180.5230320745700965, 95.76406004447552789, 37.07285121458210853 ) ) ;
#58338 = CARTESIAN_POINT ( 'NONE',  ( 14.77197008895680597, 49.50853412630286954, 26.66469066592269144 ) ) ;
#58339 = AXIS2_PLACEMENT_3D ( 'NONE', #46296, #30477, #45963 ) ;
#58340 = DIRECTION ( 'NONE',  ( -0.000000000000000000, -0.000000000000000000, -1.000000000000000000 ) ) ;
#58341 = ORIENTED_EDGE ( 'NONE', *, *, #11725, .T. ) ;
#58342 = DIRECTION ( 'NONE',  ( 0.000000000000000000, 0.000000000000000000, 1.000000000000000000 ) ) ;
#58343 = ADVANCED_FACE ( 'NONE', ( #17615 ), #33797, .F. ) ;
#58344 = EDGE_CURVE ( 'NONE', #6017, #36914, #43283, .T. ) ;
#58345 = CARTESIAN_POINT ( 'NONE',  ( 139.6359093656973585, 45.02518919224739591, 68.64155198831963389 ) ) ;
#58346 = CARTESIAN_POINT ( 'NONE',  ( -174.7817412490651918, 90.52199442492064918, 30.99576591545036308 ) ) ;
#58347 = DIRECTION ( 'NONE',  ( 0.000000000000000000, 1.000000000000000000, 0.000000000000000000 ) ) ;
#58348 = CARTESIAN_POINT ( 'NONE',  ( 92.52113039222217594, 22.58921125235801952, 41.87899094217726059 ) ) ;
#58349 = EDGE_LOOP ( 'NONE', ( #44822, #12293, #22651, #26772, #65025 ) ) ;
#58350 = LINE ( 'NONE', #68242, #64739 ) ;
#58351 = EDGE_LOOP ( 'NONE', ( #23635, #531, #44387, #57586 ) ) ;
#58352 = B_SPLINE_CURVE_WITH_KNOTS ( 'NONE', 3,
 ( #31495, #47307, #41367, #15662, #3718, #36426, #57198, #31835, #20935, #14961, #68767, #25197, #20582, #52927, #68106, #57881, #4753, #26216, #46632, #42044, #4079, #68438, #14287, #19912, #52257, #62820, #25544, #42391, #14624, #63853, #47655, #69460, #9700, #37110, #53271, #5100, #47997, #21279, #41704, #36087, #42728, #35747, #57543, #9346 ),
 .UNSPECIFIED., .F., .F.,
 ( 4, 2, 2, 2, 2, 2, 2, 2, 2, 2, 2, 2, 2, 2, 2, 2, 2, 2, 2, 2, 2, 4 ),
 ( 0.02814986980477065734, 0.02995274102020802770, 0.03085417662792672502, 0.03175561223564542235, 0.03355848345108278924, 0.03536135466652016307, 0.03716422588195752996, 0.03896709709739489685, 0.03986853270511355601, 0.04076996831283221517, 0.04167140392055087433, 0.04257283952826951268, 0.04347427513598819959, 0.04437571074370687263, 0.04527714635142555955, 0.04617858195914423952, 0.04798145317458163417, 0.04978432439001902882, 0.05158719560545642346, 0.05339006682089381811, 0.05519293803633121276, 0.05699580925176860741 ),
 .UNSPECIFIED. ) ;
#58353 = EDGE_CURVE ( 'NONE', #19781, #5206, #55236, .T. ) ;
#58354 = AXIS2_PLACEMENT_3D ( 'NONE', #5648, #5318, #31705 ) ;
#58355 = PRESENTATION_STYLE_ASSIGNMENT (( #37591 ) ) ;
#58356 = CARTESIAN_POINT ( 'NONE',  ( -61.99282085258081310, 16.65258086416814010, 94.42360237343419271 ) ) ;
#58357 = CARTESIAN_POINT ( 'NONE',  ( 106.6322547488295385, 28.34756922280616465, 30.52000857272038914 ) ) ;
#58358 = CARTESIAN_POINT ( 'NONE',  ( 0.000000000000000000, 0.000000000000000000, 41.38025477438755928 ) ) ;
#58359 = DIRECTION ( 'NONE',  ( 0.1342332658176522420, 0.9909497617679351444, 0.000000000000000000 ) ) ;
#58360 = DIRECTION ( 'NONE',  ( 1.000000000000000000, 0.000000000000000000, -0.000000000000000000 ) ) ;
#58361 = CARTESIAN_POINT ( 'NONE',  ( 26.98325939156676867, -31.83109271837644627, 13.79046412397660859 ) ) ;
#58362 = CARTESIAN_POINT ( 'NONE',  ( 0.000000000000000000, 0.000000000000000000, 40.00000000000003553 ) ) ;
#58363 = ORIENTED_EDGE ( 'NONE', *, *, #54297, .F. ) ;
#58364 = DIRECTION ( 'NONE',  ( 1.000000000000000000, 0.000000000000000000, 0.000000000000000000 ) ) ;
#58365 = ORIENTED_EDGE ( 'NONE', *, *, #29341, .F. ) ;
#58366 = APPLICATION_CONTEXT ( 'automotive_design' ) ;
#58367 = CARTESIAN_POINT ( 'NONE',  ( -94.84390436305042726, 29.16104988397310294, -41.50425148441384238 ) ) ;
#58368 = EDGE_CURVE ( 'NONE', #28358, #64523, #69205, .T. ) ;
#58369 = CARTESIAN_POINT ( 'NONE',  ( 62.52742438962774685, 12.55954017561948000, -62.56524142263339172 ) ) ;
#58370 = CARTESIAN_POINT ( 'NONE',  ( -55.05276343752909440, 15.72344139423348786, -77.06087458892358200 ) ) ;
#58371 = CARTESIAN_POINT ( 'NONE',  ( -122.8202784017355498, 45.69728649588467562, 71.80980446227590619 ) ) ;
#58372 = CARTESIAN_POINT ( 'NONE',  ( 16.27775141556967853, 7.523247835309960330, 30.01470767270521733 ) ) ;
#58373 = VECTOR ( 'NONE', #11826, 1000.000000000000000 ) ;
#58374 = EDGE_CURVE ( 'NONE', #23331, #26077, #7060, .T. ) ;
#58375 = ADVANCED_FACE ( 'NONE', ( #6362 ), #62494, .T. ) ;
#58376 = CARTESIAN_POINT ( 'NONE',  ( 163.5944442552009832, 63.88381951184481267, -66.13186425301876170 ) ) ;
#58377 = EDGE_LOOP ( 'NONE', ( #11132, #57746 ) ) ;
#58378 = B_SPLINE_CURVE_WITH_KNOTS ( 'NONE', 3,
 ( #23100, #12901, #66031, #17099 ),
 .UNSPECIFIED., .F., .F.,
 ( 4, 4 ),
 ( 9.900409499088329389E-07, 0.05658314289920115397 ),
 .UNSPECIFIED. ) ;
#58379 = LINE ( 'NONE', #42882, #12841 ) ;
#58380 = CARTESIAN_POINT ( 'NONE',  ( 201.4688124904258189, 102.0170968684381450, -90.70582092648642458 ) ) ;
#58381 = VERTEX_POINT ( 'NONE', #66179 ) ;
#58382 = ORIENTED_EDGE ( 'NONE', *, *, #53734, .T. ) ;
#58383 = CARTESIAN_POINT ( 'NONE',  ( -154.7934364910360614, 68.79594655117534785, 43.54706751354447647 ) ) ;
#58384 = DIRECTION ( 'NONE',  ( 0.000000000000000000, 0.000000000000000000, -1.000000000000000000 ) ) ;
#58385 = DIRECTION ( 'NONE',  ( 0.000000000000000000, -0.000000000000000000, -1.000000000000000000 ) ) ;
#58386 = CARTESIAN_POINT ( 'NONE',  ( 31.11269837220809364, 15.55634918610396866, 85.00100000000000477 ) ) ;
#58387 = ORIENTED_EDGE ( 'NONE', *, *, #55506, .T. ) ;
#58388 = CIRCLE ( 'NONE', #38155, 65.00000000000000000 ) ;
#58389 = CARTESIAN_POINT ( 'NONE',  ( -129.3970594949620079, 50.06339481638099187, 31.47202801301698116 ) ) ;
#58390 = ORIENTED_EDGE ( 'NONE', *, *, #69004, .F. ) ;
#58391 = CARTESIAN_POINT ( 'NONE',  ( 0.000000000000000000, 0.000000000000000000, -9.500000000000000000 ) ) ;
#58392 = CARTESIAN_POINT ( 'NONE',  ( 0.7145311798163209716, 4.618802153517001408, -8.000000000000000000 ) ) ;
#58393 = CARTESIAN_POINT ( 'NONE',  ( 62.52742438962774685, 12.55954017561948000, 71.65751152968499582 ) ) ;
#58394 = CARTESIAN_POINT ( 'NONE',  ( -1.866625526081663988, 7.583073082893622363, 69.04121920335192897 ) ) ;
#58395 = DIRECTION ( 'NONE',  ( -0.000000000000000000, -1.000000000000000000, -0.000000000000000000 ) ) ;
#58396 =( NAMED_UNIT ( * ) SI_UNIT ( $, .STERADIAN. ) SOLID_ANGLE_UNIT ( ) );
#58397 = ORIENTED_EDGE ( 'NONE', *, *, #60815, .T. ) ;
#58398 = ORIENTED_EDGE ( 'NONE', *, *, #65109, .F. ) ;
#58399 = DIRECTION ( 'NONE',  ( 1.000000000000000000, 3.730349362740526607E-14, 0.000000000000000000 ) ) ;
#58400 = CARTESIAN_POINT ( 'NONE',  ( -84.49322488516129681, 0.000000000000000000, 43.58025477438756212 ) ) ;
#58401 = CARTESIAN_POINT ( 'NONE',  ( -173.1211646369891071, 87.12891641440859303, -22.86740657428632773 ) ) ;
#58402 = CARTESIAN_POINT ( 'NONE',  ( -50.92620509423012720, -55.07344309828840068, 170.0000000000000000 ) ) ;
#58403 = CARTESIAN_POINT ( 'NONE',  ( -48.41612563322100016, 14.03642305406760471, 94.99999999999866418 ) ) ;
#58404 = CONICAL_SURFACE ( 'NONE', #28075, 65.00000000000000000, 0.7853981633974497223 ) ;
#58405 = CARTESIAN_POINT ( 'NONE',  ( 21.96910889293877034, 7.784886455511741410, 86.90482503240505707 ) ) ;
#58406 = VERTEX_POINT ( 'NONE', #1799 ) ;
#58407 = EDGE_CURVE ( 'NONE', #22455, #44611, #17969, .T. ) ;
#58408 = DIRECTION ( 'NONE',  ( -2.477416674922659623E-16, -3.355888904728274975E-17, 1.000000000000000000 ) ) ;
#58409 = DIRECTION ( 'NONE',  ( -0.000000000000000000, -0.000000000000000000, 1.000000000000000000 ) ) ;
#58410 = VERTEX_POINT ( 'NONE', #1087 ) ;
#58411 = PLANE ( 'NONE',  #48582 ) ;
#58412 = ORIENTED_EDGE ( 'NONE', *, *, #52121, .T. ) ;
#58413 = EDGE_CURVE ( 'NONE', #12560, #65565, #34389, .T. ) ;
#58414 = ORIENTED_EDGE ( 'NONE', *, *, #21048, .F. ) ;
#58415 = VERTEX_POINT ( 'NONE', #49254 ) ;
#58416 = CARTESIAN_POINT ( 'NONE',  ( -118.6727642982647524, 43.09863379477474155, 9.178398134959156351 ) ) ;
#58417 = CIRCLE ( 'NONE', #44929, 8.000000000000000000 ) ;
#58418 = CARTESIAN_POINT ( 'NONE',  ( -175.9970298498767249, 90.38640259140136379, 58.22642001971374981 ) ) ;
#58419 = CARTESIAN_POINT ( 'NONE',  ( 18.89064107370903045, 6.619789970027398773, 17.50279535283585375 ) ) ;
#58420 = ORIENTED_EDGE ( 'NONE', *, *, #31696, .F. ) ;
#58421 = EDGE_CURVE ( 'NONE', #21953, #7128, #27458, .T. ) ;
#58422 = ADVANCED_FACE ( 'NONE', ( #61224 ), #2484, .F. ) ;
#58423 = CARTESIAN_POINT ( 'NONE',  ( -27.48409822889280463, 8.975441763201041923, 85.02499692473053017 ) ) ;
#58424 = CARTESIAN_POINT ( 'NONE',  ( 153.4268936273268764, 54.57409659828383752, 30.58846441339344580 ) ) ;
#58425 = CARTESIAN_POINT ( 'NONE',  ( 412.3372781065086201, 399.9999999999998863, 78.55029585798826020 ) ) ;
#58426 = CARTESIAN_POINT ( 'NONE',  ( 105.4193882736796297, 26.71329717705295081, -49.18680799141433369 ) ) ;
#58427 = ADVANCED_FACE ( 'NONE', ( #51369 ), #13389, .F. ) ;
#58428 = CARTESIAN_POINT ( 'NONE',  ( 140.2058232509808704, 46.59155168125936086, -66.34433898568947541 ) ) ;
#58429 = DIRECTION ( 'NONE',  ( -0.000000000000000000, -0.000000000000000000, 1.000000000000000000 ) ) ;
#58430 = ORIENTED_EDGE ( 'NONE', *, *, #30929, .T. ) ;
#58431 = CIRCLE ( 'NONE', #27965, 65.36598343705435354 ) ;
#58432 = DIRECTION ( 'NONE',  ( 0.000000000000000000, -1.000000000000000000, 0.000000000000000000 ) ) ;
#58433 = CARTESIAN_POINT ( 'NONE',  ( -85.36298448216594181, 26.07611629625833416, -66.04488118901366533 ) ) ;
#58434 = CARTESIAN_POINT ( 'NONE',  ( 117.4396227366912626, 32.35611529020199129, -95.00000000000133582 ) ) ;
#58435 = CARTESIAN_POINT ( 'NONE',  ( -118.4709174626548531, 42.97515378817186615, -41.30754075210906251 ) ) ;
#58436 = CARTESIAN_POINT ( 'NONE',  ( -86.16504208171677703, 26.41251233979375712, 10.54396692358523779 ) ) ;
#58437 = CARTESIAN_POINT ( 'NONE',  ( -53.31111153860302210, 37.18770477615724701, 40.00000000000003553 ) ) ;
#58438 = CARTESIAN_POINT ( 'NONE',  ( -22.50000000000003197, 207.5000000000000284, 380.0000000000000000 ) ) ;
#58439 = DIRECTION ( 'NONE',  ( -4.492911005741634170E-18, -2.417738509769586184E-18, -1.000000000000000000 ) ) ;
#58440 = CYLINDRICAL_SURFACE ( 'NONE', #18658, 7.500000000000020428 ) ;
#58441 = CARTESIAN_POINT ( 'NONE',  ( 0.000000000000000000, 0.000000000000000000, -5.000000000000000888 ) ) ;
#58442 = CARTESIAN_POINT ( 'NONE',  ( -173.1211646369891355, -170.0000000000000000, -61.55650775521367279 ) ) ;
#58443 = VERTEX_POINT ( 'NONE', #2829 ) ;
#58444 = CONTEXT_DEPENDENT_SHAPE_REPRESENTATION ( #21100, #49566 ) ;
#58445 = DIRECTION ( 'NONE',  ( -0.6427876096865403621, -0.7660444431189770143, 0.000000000000000000 ) ) ;
#58446 = ORIENTED_EDGE ( 'NONE', *, *, #5009, .F. ) ;
#58447 = LINE ( 'NONE', #27133, #32947 ) ;
#58448 = EDGE_LOOP ( 'NONE', ( #34485, #10521, #12308, #15992 ) ) ;
#58449 = CARTESIAN_POINT ( 'NONE',  ( 22.51798020284706681, 7.817376421459704794, -73.18340610876502694 ) ) ;
#58450 = SURFACE_SIDE_STYLE ('',( #68668 ) ) ;
#58451 = CARTESIAN_POINT ( 'NONE',  ( 11.51073115475400677, -31.38130280396068983, 6.893342932533044198 ) ) ;
#58452 = CARTESIAN_POINT ( 'NONE',  ( 70.26722489419891815, 14.47234958177329212, -18.35366578844314134 ) ) ;
#58453 = AXIS2_PLACEMENT_3D ( 'NONE', #46338, #29478, #25606 ) ;
#58454 = EDGE_CURVE ( 'NONE', #52737, #37939, #2144, .T. ) ;
#58455 = EDGE_CURVE ( 'NONE', #33141, #65664, #31013, .T. ) ;
#58456 = CARTESIAN_POINT ( 'NONE',  ( 140.2200249818744169, 46.60103563593122544, -47.50120530054586965 ) ) ;
#58457 = CARTESIAN_POINT ( 'NONE',  ( -52.67596829228263289, 15.09584868440940220, -76.69087494152185513 ) ) ;
#58458 = LINE ( 'NONE', #5002, #2739 ) ;
#58459 = EDGE_CURVE ( 'NONE', #19218, #26538, #40118, .T. ) ;
#58460 = CARTESIAN_POINT ( 'NONE',  ( -119.5563837756079693, 43.64229894412654431, -11.52668347953698280 ) ) ;
#58461 = ORIENTED_EDGE ( 'NONE', *, *, #49858, .F. ) ;
#58462 = EDGE_LOOP ( 'NONE', ( #13295, #69001, #29821, #39822 ) ) ;
#58463 = CARTESIAN_POINT ( 'NONE',  ( 180.1110850744962022, 79.05158019587979368, 83.03841359423326196 ) ) ;
#58464 = CARTESIAN_POINT ( 'NONE',  ( 41.66904755831212981, 15.55634918610394379, 0.000000000000000000 ) ) ;
#58465 = DIRECTION ( 'NONE',  ( -1.000000000000000000, 0.000000000000000000, 0.000000000000000000 ) ) ;
#58466 = PRODUCT_DEFINITION_CONTEXT ( 'detailed design', #34152, 'design' ) ;
#58467 = AXIS2_PLACEMENT_3D ( 'NONE', #65047, #65399, #11559 ) ;
#58468 = LINE ( 'NONE', #42973, #62238 ) ;
#58469 = CARTESIAN_POINT ( 'NONE',  ( 91.49210130311618627, 22.20929244416438308, 16.08268542465916795 ) ) ;
#58470 = CARTESIAN_POINT ( 'NONE',  ( 185.1710994180822354, 84.30654632312743502, -10.57602910970770616 ) ) ;
#58471 = CARTESIAN_POINT ( 'NONE',  ( -85.75222301046103723, 25.14826148333820299, -13.26214896379232400 ) ) ;
#58472 = CARTESIAN_POINT ( 'NONE',  ( 0.000000000000000000, -6.928203230275505220, -4.000000000000007105 ) ) ;
#58473 = CARTESIAN_POINT ( 'NONE',  ( 92.19920907511537678, 21.39700525884451210, -21.52306413018001052 ) ) ;
#58474 = CARTESIAN_POINT ( 'NONE',  ( 34.41143668122512622, -66.58502636910473882, 41.38025477438755928 ) ) ;
#58475 = CARTESIAN_POINT ( 'NONE',  ( 105.2557116016002681, 21.94295192046379128, -1.612329923324939740 ) ) ;
#58476 = CARTESIAN_POINT ( 'NONE',  ( -22.50000000000003197, -18.06806526123148160, 378.0000000000000000 ) ) ;
#58477 = ORIENTED_EDGE ( 'NONE', *, *, #14825, .F. ) ;
#58478 = CARTESIAN_POINT ( 'NONE',  ( 133.4058733589412782, 42.32720528873922206, 2.665790248531677786 ) ) ;
#58479 = DIRECTION ( 'NONE',  ( -1.000000000000000000, 0.000000000000000000, -0.000000000000000000 ) ) ;
#58480 = CARTESIAN_POINT ( 'NONE',  ( 18.62350602913452846, 70.00000000000000000, 23.51946052065798298 ) ) ;
#58481 = LINE ( 'NONE', #42661, #59042 ) ;
#58482 = CARTESIAN_POINT ( 'NONE',  ( 8.000000000000007105, 249.8719672152120381, -95.00000000000133582 ) ) ;
#58483 = CARTESIAN_POINT ( 'NONE',  ( -3.810800745967052539, 7.670052258724785688, 84.96130854411160271 ) ) ;
#58484 = ORIENTED_EDGE ( 'NONE', *, *, #21190, .T. ) ;
#58485 = DIRECTION ( 'NONE',  ( -1.000000000000000000, 0.000000000000000000, 0.000000000000000000 ) ) ;
#58486 = CARTESIAN_POINT ( 'NONE',  ( -56.96214175905167565, 15.20165595797839231, 71.91879777619202230 ) ) ;
#58487 = ORIENTED_EDGE ( 'NONE', *, *, #50771, .T. ) ;
#58488 = VERTEX_POINT ( 'NONE', #23939 ) ;
#58489 = EDGE_CURVE ( 'NONE', #69371, #40284, #54312, .T. ) ;
#58490 = CARTESIAN_POINT ( 'NONE',  ( 34.30959576864569271, 8.813794125124662315, 85.58691292226393443 ) ) ;
#58491 = CARTESIAN_POINT ( 'NONE',  ( -180.4643341113398378, 95.69224917234934935, -67.50112049958217142 ) ) ;
#58492 = CARTESIAN_POINT ( 'NONE',  ( 183.2136430849847955, 0.000000000000000000, -36.68900338898718871 ) ) ;
#58493 = EDGE_LOOP ( 'NONE', ( #40949, #28145, #37266, #1862 ) ) ;
#58494 = FACE_OUTER_BOUND ( 'NONE', #20438, .T. ) ;
#58495 = CARTESIAN_POINT ( 'NONE',  ( 37.47470427701602347, -8.071072281209895394, 13.32819397642332504 ) ) ;
#58496 = AXIS2_PLACEMENT_3D ( 'NONE', #10036, #37108, #38140 ) ;
#58497 = CARTESIAN_POINT ( 'NONE',  ( -4.072522659361690778, 7.683023425615369106, 4.272846646336744492 ) ) ;
#58498 = CARTESIAN_POINT ( 'NONE',  ( 175.8874477961783498, 74.89984466412600739, -38.29623224188777897 ) ) ;
#58499 = CARTESIAN_POINT ( 'NONE',  ( -154.0716379918897303, 69.49957566103796580, -75.12760008809200940 ) ) ;
#58500 = CARTESIAN_POINT ( 'NONE',  ( -64.61430802170482934, -7.070445451048283481, 40.00000000000003553 ) ) ;
#58501 = VECTOR ( 'NONE', #45266, 1000.000000000000000 ) ;
#58502 = ADVANCED_FACE ( 'NONE', ( #22368 ), #65282, .F. ) ;
#58503 = PRODUCT ( 'MAT-053', 'MAT-053', '', ( #3055 ) ) ;
#58504 = ORIENTED_EDGE ( 'NONE', *, *, #7407, .F. ) ;
#58505 = VECTOR ( 'NONE', #32828, 1000.000000000000000 ) ;
#58506 = CARTESIAN_POINT ( 'NONE',  ( 102.7983318509015049, 26.68040613344513545, -17.62410043733592957 ) ) ;
#58507 = LINE ( 'NONE', #53574, #14569 ) ;
#58508 = EDGE_CURVE ( 'NONE', #36015, #5564, #58350, .T. ) ;
#58509 = CARTESIAN_POINT ( 'NONE',  ( -55.05276343752910151, -170.0000000000000000, 37.81732777293115078 ) ) ;
#58510 = CARTESIAN_POINT ( 'NONE',  ( 447.3372781065085064, 364.9999999999990905, 113.5502958579887007 ) ) ;
#58511 = EDGE_CURVE ( 'NONE', #61576, #57714, #3869, .T. ) ;
#58512 = CARTESIAN_POINT ( 'NONE',  ( -85.93597956139524285, 26.31611237855608820, 93.48078942079631304 ) ) ;
#58514 = VERTEX_POINT ( 'NONE', #31628 ) ;
#58513 = DIRECTION ( 'NONE',  ( -6.939198835768237954E-16, -1.000000000000000000, -6.106226635438359986E-16 ) ) ;
#58515 = ORIENTED_EDGE ( 'NONE', *, *, #37236, .T. ) ;
#58516 = VECTOR ( 'NONE', #60175, 999.9999999999998863 ) ;
#58517 = ADVANCED_FACE ( 'NONE', ( #31299 ), #64582, .T. ) ;
#58518 = ORIENTED_EDGE ( 'NONE', *, *, #64959, .T. ) ;
#58519 = CARTESIAN_POINT ( 'NONE',  ( 29.86848256228606502, -58.14280299503694494, 43.58025477438756212 ) ) ;
#58520 = CARTESIAN_POINT ( 'NONE',  ( 8.820885042878503057, -74.43053605947400797, 41.38025477438755928 ) ) ;
#58521 = DIRECTION ( 'NONE',  ( -0.000000000000000000, -0.000000000000000000, -1.000000000000000000 ) ) ;
#58522 = CARTESIAN_POINT ( 'NONE',  ( 0.000000000000000000, 0.000000000000000000, 43.58025477438756212 ) ) ;
#58523 = CARTESIAN_POINT ( 'NONE',  ( -8.320534640989468045, 7.931748412542454219, -8.573520141480125645 ) ) ;
#58524 = CARTESIAN_POINT ( 'NONE',  ( 149.9552318559266837, 52.03645904563055069, -70.44558198621334100 ) ) ;
#58525 = CARTESIAN_POINT ( 'NONE',  ( 19.74724861314306779, 6.659670522263895442, -22.54914667598139388 ) ) ;
#58526 = FACE_OUTER_BOUND ( 'NONE', #18199, .T. ) ;
#58527 = ORIENTED_EDGE ( 'NONE', *, *, #17570, .F. ) ;
#58528 = ORIENTED_EDGE ( 'NONE', *, *, #12947, .T. ) ;
#58529 = CARTESIAN_POINT ( 'NONE',  ( 70.26639875985991068, 15.51307715494295891, -14.39416547209034647 ) ) ;
#58530 = CARTESIAN_POINT ( 'NONE',  ( -85.12122836439579032, 25.97531040437158723, -38.76424601805629777 ) ) ;
#58531 = CARTESIAN_POINT ( 'NONE',  ( 103.0509289023981125, 25.69456821447926842, 88.64481294647117693 ) ) ;
#58532 = CARTESIAN_POINT ( 'NONE',  ( -155.7457403566965581, 71.01814553754121562, 7.182542572017481142 ) ) ;
#58533 = FACE_OUTER_BOUND ( 'NONE', #26191, .T. ) ;
#58534 = CARTESIAN_POINT ( 'NONE',  ( 19.11168290073779019, 6.629794975642857580, 44.24265699935381235 ) ) ;
#58535 = EDGE_CURVE ( 'NONE', #61844, #55150, #10508, .T. ) ;
#58536 = CARTESIAN_POINT ( 'NONE',  ( -156.8260034364761282, 72.01363188529046511, 90.23433487043809009 ) ) ;
#58537 = VERTEX_POINT ( 'NONE', #35878 ) ;
#58539 = ORIENTED_EDGE ( 'NONE', *, *, #53962, .T. ) ;
#58538 = B_SPLINE_CURVE_WITH_KNOTS ( 'NONE', 3,
 ( #10520, #31991, #22119, #21424, #11549, #60094, #11914, #65036, #16836, #47812, #33026, #69272, #42866, #64336, #16147, #28443, #23527, #44968, #17541, #39699, #29485, #50947, #66453, #18240 ),
 .UNSPECIFIED., .F., .F.,
 ( 4, 2, 2, 2, 2, 2, 2, 2, 2, 2, 2, 4 ),
 ( 0.01129708592246000433, 0.01269909149731377786, 0.01410109707216755312, 0.01550310264702132665, 0.01620410543444821341, 0.01690510822187510018, 0.01830711379672887024, 0.01900811658415573965, 0.01970911937158260907, 0.02111112494643635137, 0.02181212773386321385, 0.02251313052129007633 ),
 .UNSPECIFIED. ) ;
#58540 = ORIENTED_EDGE ( 'NONE', *, *, #16721, .T. ) ;
#58541 = CARTESIAN_POINT ( 'NONE',  ( -151.2428028786328014, 66.99705074331123456, -22.77775578256537514 ) ) ;
#58542 = CARTESIAN_POINT ( 'NONE',  ( -12.50000000000002842, -18.06806526123148160, 378.0000000000000000 ) ) ;
#58543 = CARTESIAN_POINT ( 'NONE',  ( 180.2473887773228398, 77.76029175826239737, 71.15314469597515767 ) ) ;
#58544 = VECTOR ( 'NONE', #10377, 1000.000000000000000 ) ;
#58545 = CARTESIAN_POINT ( 'NONE',  ( -34.06864996337443330, 10.03773626259441798, 71.58918042140540194 ) ) ;
#58546 = DIRECTION ( 'NONE',  ( -0.000000000000000000, 1.000000000000000000, -0.000000000000000000 ) ) ;
#58547 = VERTEX_POINT ( 'NONE', #25336 ) ;
#58548 = CARTESIAN_POINT ( 'NONE',  ( -442.6627218934912662, 394.9999999999998295, 103.5502958579880612 ) ) ;
#58549 = CARTESIAN_POINT ( 'NONE',  ( 8.848532525911927848, 6.377649276597440853, -13.29886354056554509 ) ) ;
#58550 = VECTOR ( 'NONE', #54240, 1000.000000000000000 ) ;
#58551 = CARTESIAN_POINT ( 'NONE',  ( 6.381648998658842054, 37.79907703206831826, 13.32819397642332859 ) ) ;
#58552 = DIRECTION ( 'NONE',  ( 0.7530714660036099684, 0.6579387259397136978, 0.000000000000000000 ) ) ;
#58553 = DIRECTION ( 'NONE',  ( 0.000000000000000000, 0.000000000000000000, 1.000000000000000000 ) ) ;
#58554 = CARTESIAN_POINT ( 'NONE',  ( -80.54757501605355685, 23.04700348514568375, -35.35128041769551999 ) ) ;
#58555 = CARTESIAN_POINT ( 'NONE',  ( 17.74393407086868635, 6.570779001277777809, 71.61667146331731715 ) ) ;
#58556 = CARTESIAN_POINT ( 'NONE',  ( 48.11816970607300448, -43.69944786993950459, 170.0000000000000000 ) ) ;
#58557 = CARTESIAN_POINT ( 'NONE',  ( 8.478575283864733692, 7.382882227715640511, 12.36660011482083199 ) ) ;
#58558 = AXIS2_PLACEMENT_3D ( 'NONE', #8185, #51100, #39165 ) ;
#58559 = EDGE_LOOP ( 'NONE', ( #16053, #44508, #1138, #22597 ) ) ;
#58560 = CARTESIAN_POINT ( 'NONE',  ( 122.2516123306975402, 190.0000000000000000, -21.28179539054375624 ) ) ;
#58561 = SHAPE_DEFINITION_REPRESENTATION ( #54614, #19523 ) ;
#58562 = CIRCLE ( 'NONE', #67582, 74.95140232871122521 ) ;
#58563 = CARTESIAN_POINT ( 'NONE',  ( 133.8566784816069060, 42.60093787723652525, -36.02331093239566684 ) ) ;
#58564 = DIRECTION ( 'NONE',  ( 1.000000000000000000, 0.000000000000000000, 0.000000000000000000 ) ) ;
#58565 = CARTESIAN_POINT ( 'NONE',  ( -109.0291978193666438, 37.49173305805086898, -45.79549089733289691 ) ) ;
#58566 = CARTESIAN_POINT ( 'NONE',  ( 59.73312635112155533, 12.96464920523512276, -76.82611381836962039 ) ) ;
#58567 = ORIENTED_EDGE ( 'NONE', *, *, #58585, .F. ) ;
#58568 = PRODUCT_DEFINITION ( 'UNKNOWN', '', #37767, #33139 ) ;
#58569 = ORIENTED_EDGE ( 'NONE', *, *, #816, .F. ) ;
#58570 = EDGE_CURVE ( 'NONE', #56686, #41593, #15112, .T. ) ;
#58571 = CARTESIAN_POINT ( 'NONE',  ( -24.41864932425148993, 8.543938959778813569, -13.32222848996388365 ) ) ;
#58572 = EDGE_CURVE ( 'NONE', #27491, #536, #61230, .T. ) ;
#58573 = CARTESIAN_POINT ( 'NONE',  ( 197.5344433744249670, 98.61756151884684130, 12.10789136445144898 ) ) ;
#58574 = ORIENTED_EDGE ( 'NONE', *, *, #51736, .F. ) ;
#58575 = EDGE_CURVE ( 'NONE', #59876, #61401, #65116, .T. ) ;
#58576 = DIRECTION ( 'NONE',  ( 0.000000000000000000, 0.000000000000000000, 1.000000000000000000 ) ) ;
#58577 = VERTEX_POINT ( 'NONE', #6546 ) ;
#58578 = DIRECTION ( 'NONE',  ( -0.000000000000000000, -0.000000000000000000, -1.000000000000000000 ) ) ;
#58579 = FACE_BOUND ( 'NONE', #58377, .T. ) ;
#58580 = CARTESIAN_POINT ( 'NONE',  ( 39.40195752203892710, -170.0000000000000000, -89.30891864635511013 ) ) ;
#58581 = CARTESIAN_POINT ( 'NONE',  ( -95.50384525802328994, 29.46973564057715933, 41.24368704753796777 ) ) ;
#58582 = CARTESIAN_POINT ( 'NONE',  ( 93.86680996363766383, 22.01878169039502708, -41.33864978769346266 ) ) ;
#58584 = ORIENTED_EDGE ( 'NONE', *, *, #33846, .T. ) ;
#58583 = DIRECTION ( 'NONE',  ( -0.8532989592251508659, 0.000000000000000000, 0.5214219847544543374 ) ) ;
#58585 = EDGE_CURVE ( 'NONE', #39680, #55744, #18145, .T. ) ;
#58586 = EDGE_LOOP ( 'NONE', ( #54080, #58151, #20074, #9477, #19326, #55060, #33119, #1777, #62396 ) ) ;
#58587 = ORIENTED_EDGE ( 'NONE', *, *, #874, .F. ) ;
#58588 = CARTESIAN_POINT ( 'NONE',  ( -119.5267374018686724, 42.44190186039715229, -11.57287640902848302 ) ) ;
#58589 = FACE_BOUND ( 'NONE', #31359, .T. ) ;
#58590 = ADVANCED_FACE ( 'NONE', ( #33978 ), #60354, .T. ) ;
#58591 = CARTESIAN_POINT ( 'NONE',  ( -173.1211646369891071, 87.12891641440859303, -7.867406574286297527 ) ) ;
#58592 = ADVANCED_FACE ( 'NONE', ( #39600 ), #7602, .F. ) ;
#58593 = CARTESIAN_POINT ( 'NONE',  ( -168.7314919967217861, 83.83749564070829763, -62.95703578078057205 ) ) ;
#58595 = ORIENTED_EDGE ( 'NONE', *, *, #40986, .T. ) ;
#58594 = CARTESIAN_POINT ( 'NONE',  ( -146.1142527948576344, 61.35394402951020965, -35.62045372895397577 ) ) ;
#58596 = CARTESIAN_POINT ( 'NONE',  ( 62.05396267233468421, 13.48332220860126363, 3.014455481275966964 ) ) ;
#58597 = AXIS2_PLACEMENT_3D ( 'NONE', #39213, #12475, #30383 ) ;
#58598 = ORIENTED_EDGE ( 'NONE', *, *, #37816, .T. ) ;
#58599 = CARTESIAN_POINT ( 'NONE',  ( 55.93149085255341646, 12.16676074274502106, 93.48784098346216354 ) ) ;
#58600 = CARTESIAN_POINT ( 'NONE',  ( -62.56514138729678365, 16.82532522382519602, -15.86430600984316541 ) ) ;
#58601 = AXIS2_PLACEMENT_3D ( 'NONE', #39941, #8978, #3350 ) ;
#58602 = AXIS2_PLACEMENT_3D ( 'NONE', #8492, #56321, #18002 ) ;
#58603 = CARTESIAN_POINT ( 'NONE',  ( 134.3159642998340644, 41.70198410084978491, -24.17876034193201207 ) ) ;
#58604 = CARTESIAN_POINT ( 'NONE',  ( -132.2286325684322605, 52.04087929935081291, -65.23503918443411465 ) ) ;
#58605 = DIRECTION ( 'NONE',  ( -1.000000000000000000, 0.000000000000000000, 0.000000000000000000 ) ) ;
#58606 = FACE_BOUND ( 'NONE', #53733, .T. ) ;
#58607 = CARTESIAN_POINT ( 'NONE',  ( -151.7098557585652543, 66.07042764902350029, -88.82961873973066247 ) ) ;
#58608 = ORIENTED_EDGE ( 'NONE', *, *, #16575, .F. ) ;
#58609 = ORIENTED_EDGE ( 'NONE', *, *, #61209, .T. ) ;
#58610 = B_SPLINE_CURVE_WITH_KNOTS ( 'NONE', 3,
 ( #26509, #47948, #10663, #69417, #21233, #37746, #42680, #52207, #11012, #47263, #58853, #32131, #41652, #63108, #9649, #5400, #26854, #15267, #48280, #108, #31111, #41995, #43008, #59191, #25493, #46931, #52547, #68394, #68719, #4370, #36730, #14909, #20528, #22971, #27895, #43704, #38091, #38449, #23330, #27188, #16635, #17332, #7133, #17697, #49330, #28595 ),
 .UNSPECIFIED., .F., .F.,
 ( 4, 2, 2, 2, 2, 2, 2, 2, 2, 2, 2, 2, 2, 2, 2, 2, 2, 2, 2, 2, 2, 2, 4 ),
 ( 0.02404638330965502488, 0.02555608299537557096, 0.02631093283823584400, 0.02706578268109611704, 0.02857548236681666312, 0.02933033220967693616, 0.03008518205253720573, 0.03159488173825774487, 0.03310458142397829095, 0.03385943126683856746, 0.03461428110969884397, 0.03612398079541942475, 0.03687883063827971514, 0.03763368048114000552, 0.03838853032400028897, 0.03914338016686057936, 0.04065307985258115320, 0.04216277953830172703, 0.04367247922402230087, 0.04518217890974287471, 0.04593702875260315122, 0.04669187859546342079, 0.04820157828118395993 ),
 .UNSPECIFIED. ) ;
#58611 = CARTESIAN_POINT ( 'NONE',  ( 181.5072453427590347, 79.03352099595183233, -78.06960825634332934 ) ) ;
#58612 = CLOSED_SHELL ( 'NONE', ( #65266, #58823, #28280, #29320, #12014, #9011 ) ) ;
#58613 = DIRECTION ( 'NONE',  ( 0.000000000000000000, 0.000000000000000000, 1.000000000000000000 ) ) ;
#58614 = CARTESIAN_POINT ( 'NONE',  ( 8.000000000000007105, 249.8719672152120381, -95.00000000000133582 ) ) ;
#58615 = CARTESIAN_POINT ( 'NONE',  ( 22.93737758745371735, 9.943676855699235873, 0.000000000000000000 ) ) ;
#58616 = CARTESIAN_POINT ( 'NONE',  ( 102.7983318509014907, 26.68040613344513901, -71.31320161826326398 ) ) ;
#58617 = LINE ( 'NONE', #31902, #19686 ) ;
#58618 = CARTESIAN_POINT ( 'NONE',  ( 86.14852828165531662, 19.25704475759651402, 44.71208757247934074 ) ) ;
#58619 = CARTESIAN_POINT ( 'NONE',  ( 10.00000000000000000, 0.000000000000000000, -50.00000000000000711 ) ) ;
#58620 = CARTESIAN_POINT ( 'NONE',  ( -124.7710763417278486, 46.96042092553523162, 30.70098044976807472 ) ) ;
#58621 = CARTESIAN_POINT ( 'NONE',  ( 208.6132326550594200, 111.8685719053116543, 69.96301817913980869 ) ) ;
#58622 = VERTEX_POINT ( 'NONE', #61050 ) ;
#58623 = CARTESIAN_POINT ( 'NONE',  ( -103.2129897037410871, 33.25684593987702442, -8.213834404042543724 ) ) ;
#58624 = ORIENTED_EDGE ( 'NONE', *, *, #40174, .T. ) ;
#58625 = CARTESIAN_POINT ( 'NONE',  ( -33.37566357177431087, 9.916833145467597532, 3.609876264789644296 ) ) ;
#58626 = DIRECTION ( 'NONE',  ( 1.000000000000000000, 0.000000000000000000, 0.000000000000000000 ) ) ;
#58627 = CARTESIAN_POINT ( 'NONE',  ( 86.62931800182293784, 20.48449268398422163, 71.55663816294304524 ) ) ;
#58628 = CARTESIAN_POINT ( 'NONE',  ( 153.8366942494330942, 54.87992279068317458, -10.21455127450128408 ) ) ;
#58629 = DIRECTION ( 'NONE',  ( 2.213730317917102779E-18, 4.596858371395816895E-18, -1.000000000000000000 ) ) ;
#58630 = CARTESIAN_POINT ( 'NONE',  ( 31.91375106836930087, 7.553354707452896832, -70.45236121604933999 ) ) ;
#58631 = DIRECTION ( 'NONE',  ( 1.000000000000000000, 0.000000000000000000, 0.000000000000000000 ) ) ;
#58632 = CARTESIAN_POINT ( 'NONE',  ( -8.663926357539105894, 23.45072237844991747, 0.000000000000000000 ) ) ;
#58633 = ORIENTED_EDGE ( 'NONE', *, *, #30497, .T. ) ;
#58634 = DIRECTION ( 'NONE',  ( -0.9988488985473030768, 0.000000000000000000, 0.04796746679614544151 ) ) ;
#58635 = ORIENTED_EDGE ( 'NONE', *, *, #34550, .F. ) ;
#58636 = FACE_OUTER_BOUND ( 'NONE', #36891, .T. ) ;
#58637 = CARTESIAN_POINT ( 'NONE',  ( 14.08810621383466888, 7.458732232275139040, -77.17239911336513103 ) ) ;
#58638 = FACE_OUTER_BOUND ( 'NONE', #10804, .T. ) ;
#58639 = CARTESIAN_POINT ( 'NONE',  ( 0.000000000000000000, 6.123233995736766282E-16, -5.000000000000000000 ) ) ;
#58640 = CARTESIAN_POINT ( 'NONE',  ( -7.330690860789852437, 6.858814156830895570, 45.11558103944722831 ) ) ;
#58641 = CARTESIAN_POINT ( 'NONE',  ( 427.4999999999999432, 207.5000000000000284, 0.000000000000000000 ) ) ;
#58642 =( NAMED_UNIT ( * ) SI_UNIT ( $, .STERADIAN. ) SOLID_ANGLE_UNIT ( ) );
#58643 = ORIENTED_EDGE ( 'NONE', *, *, #32863, .F. ) ;
#58644 = AXIS2_PLACEMENT_3D ( 'NONE', #32378, #5970, #21807 ) ;
#58645 = DIRECTION ( 'NONE',  ( 0.3957342950827489325, 2.220446049250313081E-16, 0.9183650514339922744 ) ) ;
#58646 = FACE_OUTER_BOUND ( 'NONE', #55708, .T. ) ;
#58647 = DIRECTION ( 'NONE',  ( 0.000000000000000000, 0.000000000000000000, 1.000000000000000000 ) ) ;
#58648 = CARTESIAN_POINT ( 'NONE',  ( -104.7956873821848944, 35.21322275870666374, 57.79421275118836832 ) ) ;
#58649 = EDGE_CURVE ( 'NONE', #64355, #45918, #55597, .T. ) ;
#58650 = CONTEXT_DEPENDENT_SHAPE_REPRESENTATION ( #60642, #40078 ) ;
#58651 = CARTESIAN_POINT ( 'NONE',  ( -131.6399667378751417, 51.62465701391630546, -37.56756705236779936 ) ) ;
#58652 = ORIENTED_EDGE ( 'NONE', *, *, #2780, .T. ) ;
#58653 = DIRECTION ( 'NONE',  ( 0.000000000000000000, 0.000000000000000000, 1.000000000000000000 ) ) ;
#58654 = AXIS2_PLACEMENT_3D ( 'NONE', #65094, #34142, #59797 ) ;
#58655 = CARTESIAN_POINT ( 'NONE',  ( 86.62931800182293784, 19.42108912189599579, 71.55663816294304524 ) ) ;
#58656 = EDGE_CURVE ( 'NONE', #41223, #49197, #17801, .T. ) ;
#58657 = CARTESIAN_POINT ( 'NONE',  ( 197.1979149960397990, 98.19687999752001417, -17.31673455087552682 ) ) ;
#58658 = EDGE_CURVE ( 'NONE', #23556, #44265, #48836, .T. ) ;
#58659 = CIRCLE ( 'NONE', #67679, 30.00000000000000000 ) ;
#58660 = CARTESIAN_POINT ( 'NONE',  ( -142.0099858798915022, 58.07212099904398883, 92.31482491311859917 ) ) ;
#58661 = EDGE_CURVE ( 'NONE', #5564, #32464, #60702, .T. ) ;
#58662 = CARTESIAN_POINT ( 'NONE',  ( 141.2470358420065395, 46.06959063280892508, 38.31547528062654351 ) ) ;
#58663 = EDGE_LOOP ( 'NONE', ( #26817, #21576 ) ) ;
#58664 = CARTESIAN_POINT ( 'NONE',  ( 0.000000000000000000, 0.000000000000000000, 0.000000000000000000 ) ) ;
#58665 = CARTESIAN_POINT ( 'NONE',  ( 79.18180043629685372, 18.06526831600447380, 9.348947895539573949 ) ) ;
#58666 = CARTESIAN_POINT ( 'NONE',  ( 164.4760519199596160, 64.62478832434439369, 12.79513189614267077 ) ) ;
#58667 = EDGE_CURVE ( 'NONE', #26166, #68068, #50499, .T. ) ;
#58668 = CARTESIAN_POINT ( 'NONE',  ( -99.99439884168255332, 32.75762661251358310, 45.17807688415053491 ) ) ;
#58669 = VECTOR ( 'NONE', #26254, 1000.000000000000000 ) ;
#58670 = ORIENTED_EDGE ( 'NONE', *, *, #59213, .F. ) ;
#58671 = CARTESIAN_POINT ( 'NONE',  ( 177.7964363391245115, 76.75162026635254620, 56.89705291110796281 ) ) ;
#58672 = ORIENTED_EDGE ( 'NONE', *, *, #25257, .T. ) ;
#58673 = CARTESIAN_POINT ( 'NONE',  ( -78.19460645047368530, 22.14203592077026173, -23.27090004125422951 ) ) ;
#58674 = CARTESIAN_POINT ( 'NONE',  ( 70.51601918574516503, 14.53832276813546187, -69.82681846071810128 ) ) ;
#58675 = EDGE_CURVE ( 'NONE', #8163, #29725, #23770, .T. ) ;
#58676 = DIRECTION ( 'NONE',  ( 0.000000000000000000, 0.000000000000000000, -1.000000000000000000 ) ) ;
#58678 = ORIENTED_EDGE ( 'NONE', *, *, #15772, .F. ) ;
#58677 = PLANE ( 'NONE',  #7312 ) ;
#58679 = CARTESIAN_POINT ( 'NONE',  ( 159.2258951716709703, 60.31399909112330704, -50.92933666049088259 ) ) ;
#58680 = LINE ( 'NONE', #53394, #33937 ) ;
#58681 = DIRECTION ( 'NONE',  ( 1.000000000000000000, 0.000000000000000000, 0.000000000000000000 ) ) ;
#58682 = ORIENTED_EDGE ( 'NONE', *, *, #30411, .T. ) ;
#58683 = CARTESIAN_POINT ( 'NONE',  ( -7.825402957745085430, 6.891034867348157178, 18.27103044898354511 ) ) ;
#58684 = CARTESIAN_POINT ( 'NONE',  ( 133.8566784816069344, 41.42467568809808398, 71.35489142945907304 ) ) ;
#58685 = CARTESIAN_POINT ( 'NONE',  ( -177.1381400275772364, 93.26609858452822266, 31.97318544253296224 ) ) ;
#58686 = CARTESIAN_POINT ( 'NONE',  ( -31.43908319763709969, 9.591432048623765638, -77.16174795566554678 ) ) ;
#58687 = VERTEX_POINT ( 'NONE', #56120 ) ;
#58688 = CARTESIAN_POINT ( 'NONE',  ( -8.810383862755525541, 7.965311326754787480, 71.91157687480138350 ) ) ;
#58689 = ORIENTED_EDGE ( 'NONE', *, *, #18316, .T. ) ;
#58690 = ORIENTED_EDGE ( 'NONE', *, *, #55981, .T. ) ;
#58691 = AXIS2_PLACEMENT_3D ( 'NONE', #47860, #69322, #3928 ) ;
#58692 = DIRECTION ( 'NONE',  ( 0.000000000000000000, 0.000000000000000000, 1.000000000000000000 ) ) ;
#58693 = CARTESIAN_POINT ( 'NONE',  ( -61.75345348739024587, 16.58105022592818401, 88.12184266525186160 ) ) ;
#58694 = FILL_AREA_STYLE_COLOUR ( '', #53719 ) ;
#58695 = AXIS2_PLACEMENT_3D ( 'NONE', #19696, #41162, #30954 ) ;
#58696 = CARTESIAN_POINT ( 'NONE',  ( -40.99999999999997868, 0.000000000000000000, -6.071532165918823253E-15 ) ) ;
#58697 = DIRECTION ( 'NONE',  ( 0.000000000000000000, 0.000000000000000000, -1.000000000000000000 ) ) ;
#58698 = CARTESIAN_POINT ( 'NONE',  ( -60.41792053122248518, -24.01035990323518021, 170.0000000000000000 ) ) ;
#58699 = CARTESIAN_POINT ( 'NONE',  ( -27.00000000000000355, 29.99999999999999645, 12.00000000000000000 ) ) ;
#58700 = CARTESIAN_POINT ( 'NONE',  ( 0.000000000000000000, 0.000000000000000000, 73.58025477438756923 ) ) ;
#58701 = ORIENTED_EDGE ( 'NONE', *, *, #12227, .T. ) ;
#58702 = DIRECTION ( 'NONE',  ( -0.000000000000000000, -0.000000000000000000, 1.000000000000000000 ) ) ;
#58703 = ORIENTED_EDGE ( 'NONE', *, *, #49365, .F. ) ;
#58704 = CIRCLE ( 'NONE', #3692, 1.500000000000001332 ) ;
#58705 = CARTESIAN_POINT ( 'NONE',  ( -77.71490760329791669, 23.03637365463981013, 57.30817650044996014 ) ) ;
#58706 = CARTESIAN_POINT ( 'NONE',  ( 210.1633650091869754, 114.1507944623967035, -75.81224102313898072 ) ) ;
#58707 = CARTESIAN_POINT ( 'NONE',  ( 63.01563776193091826, 12.67277567978498176, -77.56524142263344856 ) ) ;
#58708 = CARTESIAN_POINT ( 'NONE',  ( -71.67841390531691559, 19.78168466957076177, 8.338739886184526995 ) ) ;
#58709 = CARTESIAN_POINT ( 'NONE',  ( -33.53812060177524756, 9.945300800226871019, -89.30285964580421876 ) ) ;
#58710 = DIRECTION ( 'NONE',  ( 1.000000000000000000, 0.000000000000000000, 0.000000000000000000 ) ) ;
#58711 = CIRCLE ( 'NONE', #67734, 65.36598343705435354 ) ;
#58712 = CARTESIAN_POINT ( 'NONE',  ( 197.7251597135301040, 97.24643299060919333, 93.16756453888348233 ) ) ;
#58713 = CARTESIAN_POINT ( 'NONE',  ( 79.40386128751609363, 17.08093333150470627, -95.00000000000133582 ) ) ;
#58714 = ORIENTED_EDGE ( 'NONE', *, *, #31935, .T. ) ;
#58715 = EDGE_CURVE ( 'NONE', #8339, #62331, #7937, .T. ) ;
#58716 = DIRECTION ( 'NONE',  ( -0.000000000000000000, -0.000000000000000000, -1.000000000000000000 ) ) ;
#58717 = DIRECTION ( 'NONE',  ( 0.000000000000000000, 0.000000000000000000, 1.000000000000000000 ) ) ;
#58718 = ORIENTED_EDGE ( 'NONE', *, *, #59298, .T. ) ;
#58719 = VERTEX_POINT ( 'NONE', #17077 ) ;
#58720 = CARTESIAN_POINT ( 'NONE',  ( -25.80443741485378695, 9.749985135376002532, -64.68774352177892695 ) ) ;
#58721 = CARTESIAN_POINT ( 'NONE',  ( 55.76298701799387914, 11.10663440745151576, -41.24582562440557609 ) ) ;
#58722 = CARTESIAN_POINT ( 'NONE',  ( -25.00000000000028066, -65.13282190615278466, 5.000000000000000000 ) ) ;
#58723 = CARTESIAN_POINT ( 'NONE',  ( 329.1355598199468204, 190.0000000000000000, -129.5087625010780812 ) ) ;
#58724 = CARTESIAN_POINT ( 'NONE',  ( 15.55634918610396511, -41.66904755831214402, 85.00100000000000477 ) ) ;
#58725 = ORIENTED_EDGE ( 'NONE', *, *, #31825, .T. ) ;
#58726 = EDGE_LOOP ( 'NONE', ( #48158, #16306, #54534, #50645, #57443, #49765 ) ) ;
#58727 = CARTESIAN_POINT ( 'NONE',  ( -129.4036885357273832, 50.06837984316181434, 44.75204449613408997 ) ) ;
#58728 = VERTEX_POINT ( 'NONE', #12877 ) ;
#58729 = DIRECTION ( 'NONE',  ( 1.000000000000000000, 0.000000000000000000, 0.000000000000000000 ) ) ;
#58730 = CARTESIAN_POINT ( 'NONE',  ( -145.3246383987844581, 62.00818849034185121, 31.99110557883703976 ) ) ;
#58731 = CARTESIAN_POINT ( 'NONE',  ( 56.53635105806415595, 11.26263375223564189, 60.37194408587342309 ) ) ;
#58732 = DIRECTION ( 'NONE',  ( 0.000000000000000000, 0.000000000000000000, 1.000000000000000000 ) ) ;
#58733 = DIRECTION ( 'NONE',  ( -1.000000000000000000, 0.000000000000000000, 0.000000000000000000 ) ) ;
#58734 = ADVANCED_FACE ( 'NONE', ( #12517 ), #38546, .F. ) ;
#58735 = DIRECTION ( 'NONE',  ( 0.000000000000000000, 1.000000000000000000, -0.000000000000000000 ) ) ;
#58736 = ORIENTED_EDGE ( 'NONE', *, *, #18931, .T. ) ;
#58737 = VERTEX_POINT ( 'NONE', #29388 ) ;
#58738 = DIRECTION ( 'NONE',  ( -6.405132834375897126E-16, 1.000000000000000000, 0.000000000000000000 ) ) ;
#58739 = CARTESIAN_POINT ( 'NONE',  ( -63.76691715686636996, 29.79383981485516841, -25.00000000000000711 ) ) ;
#58740 = STYLED_ITEM ( 'NONE', ( #15809 ), #39790 ) ;
#58741 = CARTESIAN_POINT ( 'NONE',  ( -167.1534554062404823, 80.72263015867909530, -10.81749311186897522 ) ) ;
#58742 = CARTESIAN_POINT ( 'NONE',  ( 139.6203063421347395, 45.01495791936839197, -75.19273776508998708 ) ) ;
#58743 = EDGE_CURVE ( 'NONE', #23096, #42469, #50844, .T. ) ;
#58744 = CARTESIAN_POINT ( 'NONE',  ( 70.11766033381772445, 14.43277633974326868, 34.85218099568896832 ) ) ;
#58745 = CARTESIAN_POINT ( 'NONE',  ( 9.004128196032667120, 7.384459627096075174, 94.41859741811346396 ) ) ;
#58746 = VECTOR ( 'NONE', #3103, 1000.000000000000000 ) ;
#58747 = ORIENTED_EDGE ( 'NONE', *, *, #22784, .F. ) ;
#58748 = VECTOR ( 'NONE', #33185, 1000.000000000000000 ) ;
#58749 = CARTESIAN_POINT ( 'NONE',  ( -99.11448999425216755, 31.20120877265620507, 58.04825527040586763 ) ) ;
#58750 = ORIENTED_EDGE ( 'NONE', *, *, #49927, .T. ) ;
#58751 = CIRCLE ( 'NONE', #63295, 5.000000000000004441 ) ;
#58752 = CARTESIAN_POINT ( 'NONE',  ( -74.79002408692176118, 20.88280597089421420, 44.34336250310679617 ) ) ;
#58753 = EDGE_LOOP ( 'NONE', ( #26360, #69294, #33491, #52288 ) ) ;
#58754 = AXIS2_PLACEMENT_3D ( 'NONE', #37633, #42229, #26404 ) ;
#58755 = B_SPLINE_CURVE_WITH_KNOTS ( 'NONE', 3,
 ( #13154, #1196, #34618, #60288, #7872, #35986, #57096, #68006, #8913, #24404, #36330, #62013, #30710, #35647, #67655, #67321, #35295, #9252, #25446, #45845, #41267, #61674, #46182, #25788, #68346, #52159, #3976, #46885, #20150, #40225, #3622, #2941, #30363, #62723, #51815, #14527, #41601, #63060, #19107, #25093, #57441, #40561, #19452, #56750, #62372 ),
 .UNSPECIFIED., .F., .F.,
 ( 4, 2, 2, 1, 2, 2, 2, 2, 2, 2, 2, 2, 2, 2, 2, 2, 2, 2, 2, 2, 2, 2, 4 ),
 ( 0.02346057189573570387, 0.02492590417315496479, 0.02565857031186459525, 0.02639123645057422224, 0.02712390258928384923, 0.02785656872799347969, 0.02932190100541272326, 0.03005456714412233984, 0.03078723328283195643, 0.03225256556025118265, 0.03298523169896080964, 0.03371789783767042969, 0.03518323011508967674, 0.03664856239250892378, 0.03738122853121855771, 0.03811389466992819164, 0.03957922694734745950, 0.04104455922476672736, 0.04250989150218598828, 0.04324255764089562915, 0.04397522377960525614, 0.04544055605702452399, 0.04690588833444379185 ),
 .UNSPECIFIED. ) ;
#58756 = EDGE_CURVE ( 'NONE', #7667, #39573, #7471, .T. ) ;
#58757 = AXIS2_PLACEMENT_3D ( 'NONE', #20652, #26631, #32935 ) ;
#58758 = EDGE_LOOP ( 'NONE', ( #51367, #53728 ) ) ;
#58759 = CARTESIAN_POINT ( 'NONE',  ( 10.13405324523498585, 6.385324379632244529, -47.97120849243911067 ) ) ;
#58760 = EDGE_CURVE ( 'NONE', #28360, #62965, #50049, .T. ) ;
#58762 = EDGE_CURVE ( 'NONE', #45363, #13402, #67726, .T. ) ;
#58761 = DIRECTION ( 'NONE',  ( -0.000000000000000000, 1.000000000000000000, -0.000000000000000000 ) ) ;
#58763 = CARTESIAN_POINT ( 'NONE',  ( 126.4083787442700242, 37.10531539900951259, 62.82957637863194122 ) ) ;
#58764 = ORIENTED_EDGE ( 'NONE', *, *, #24952, .T. ) ;
#58765 = CARTESIAN_POINT ( 'NONE',  ( 0.000000000000000000, 0.000000000000000000, 0.000000000000000000 ) ) ;
#58766 = CARTESIAN_POINT ( 'NONE',  ( 151.1873096904020883, 52.92629247302094342, 41.01321652849342314 ) ) ;
#58767 = DIRECTION ( 'NONE',  ( -1.000000000000000000, 0.000000000000000000, 0.000000000000000000 ) ) ;
#58768 = LINE ( 'NONE', #737, #46913 ) ;
#58769 = APPLICATION_CONTEXT ( 'automotive_design' ) ;
#58770 = CARTESIAN_POINT ( 'NONE',  ( 26.99999999999999645, -27.00000000000000355, 15.00000000000000000 ) ) ;
#58771 = CARTESIAN_POINT ( 'NONE',  ( 0.000000000000000000, 0.000000000000000000, 26.24939009510892518 ) ) ;
#58772 = LINE ( 'NONE', #57757, #65874 ) ;
#58773 = ORIENTED_EDGE ( 'NONE', *, *, #33919, .F. ) ;
#58774 = CYLINDRICAL_SURFACE ( 'NONE', #47651, 242.4895526022646663 ) ;
#58775 = CARTESIAN_POINT ( 'NONE',  ( 74.01791526339553684, 12.16185512414947034, 170.0000000000000000 ) ) ;
#58776 = FACE_OUTER_BOUND ( 'NONE', #53420, .T. ) ;
#58777 = CARTESIAN_POINT ( 'NONE',  ( 0.000000000000000000, 0.000000000000000000, 8.000000000000000000 ) ) ;
#58778 = CARTESIAN_POINT ( 'NONE',  ( -120.1346137380982100, 44.00127440773567145, -47.22450605392604928 ) ) ;
#58779 = CARTESIAN_POINT ( 'NONE',  ( -78.66644367742109978, 23.39876645725288284, 3.573650549209446137 ) ) ;
#58780 = CYLINDRICAL_SURFACE ( 'NONE', #61775, 65.36598343705435354 ) ;
#58781 = CARTESIAN_POINT ( 'NONE',  ( -155.2912910578197057, 69.24479901948497229, 16.15753730191864435 ) ) ;
#58782 = CARTESIAN_POINT ( 'NONE',  ( -118.3948752128398496, 42.92869324237091178, -68.96088763400301502 ) ) ;
#58783 = CARTESIAN_POINT ( 'NONE',  ( 69.74037587279241279, 14.33355757956375420, 13.82632352699276623 ) ) ;
#58784 = LINE ( 'NONE', #53506, #16440 ) ;
#58785 = CARTESIAN_POINT ( 'NONE',  ( 42.22820723387685149, 9.810205105131432290, -89.85872570437997808 ) ) ;
#58786 = ORIENTED_EDGE ( 'NONE', *, *, #13048, .T. ) ;
#58787 =( GEOMETRIC_REPRESENTATION_CONTEXT ( 3 ) GLOBAL_UNCERTAINTY_ASSIGNED_CONTEXT ( ( #28277 ) ) GLOBAL_UNIT_ASSIGNED_CONTEXT ( ( #5782, #37445, #43064 ) ) REPRESENTATION_CONTEXT ( 'NONE', 'WORKASPACE' ) );
#58788 = CARTESIAN_POINT ( 'NONE',  ( -37.07436112751822321, 11.60822760208521309, 15.84512009715484737 ) ) ;
#58789 = ORIENTED_EDGE ( 'NONE', *, *, #34739, .T. ) ;
#58790 = DIRECTION ( 'NONE',  ( 0.000000000000000000, 0.000000000000000000, 1.000000000000000000 ) ) ;
#58791 = ORIENTED_EDGE ( 'NONE', *, *, #60282, .T. ) ;
#58792 = CARTESIAN_POINT ( 'NONE',  ( 21.74799039132243905, 7.772294950329605712, -65.28364649508232276 ) ) ;
#58793 = VECTOR ( 'NONE', #9427, 1000.000000000000000 ) ;
#58794 = CARTESIAN_POINT ( 'NONE',  ( 181.0840389613909736, -170.0000000000000000, 56.15314469597509373 ) ) ;
#58795 = LINE ( 'NONE', #32770, #51503 ) ;
#58796 = CARTESIAN_POINT ( 'NONE',  ( -24.39249304643357519, -60.24953346690487166, 40.00000000000003553 ) ) ;
#58797 = CARTESIAN_POINT ( 'NONE',  ( 139.1306635769909690, 45.89653412152167533, -48.86132841697280327 ) ) ;
#58798 = CARTESIAN_POINT ( 'NONE',  ( -54.57263979903868290, 15.59415114099632227, -77.06087458892358200 ) ) ;
#58799 = VECTOR ( 'NONE', #63234, 1000.000000000000000 ) ;
#58800 = B_SPLINE_CURVE_WITH_KNOTS ( 'NONE', 3,
 ( #51825, #24759, #41618, #46542, #51497, #63073, #52515, #3635, #67672, #25111, #9617, #4342, #59505, #48588, #22235, #27156, #53537, #65151, #38061, #26822, #64803, #10979, #64106, #428, #27502, #16603, #21532, #16258, #21878, #59852, #5698, #37033, #48941, #21202, #5365, #42977, #42650, #15584, #11321, #53876, #15917, #48249, #783, #26480 ),
 .UNSPECIFIED., .F., .F.,
 ( 4, 2, 2, 2, 2, 2, 2, 2, 2, 2, 2, 2, 2, 2, 2, 2, 2, 2, 2, 2, 2, 4 ),
 ( 1.430489624538199204E-17, 0.004120577325733403191, 0.006180865988600120833, 0.008241154651466839343, 0.01030144331433355785, 0.01133158764576691277, 0.01236173197720026595, 0.01339187630863362261, 0.01442202064006697752, 0.01545216497150033244, 0.01648230930293368562, 0.01699738146865036742, 0.01751245363436704575, 0.01854259796580040934, 0.01957274229723377640, 0.02060288662866714693, 0.02266317529153388799, 0.02472346395440062905, 0.02678375261726737358, 0.02781389694870078227, 0.02884404128013419444, 0.03296461860586794024 ),
 .UNSPECIFIED. ) ;
#58801 = EDGE_CURVE ( 'NONE', #59960, #3346, #8981, .T. ) ;
#58802 = DIRECTION ( 'NONE',  ( 0.000000000000000000, 1.000000000000000000, -0.000000000000000000 ) ) ;
#58803 = LINE ( 'NONE', #47552, #2653 ) ;
#58804 = ORIENTED_EDGE ( 'NONE', *, *, #34822, .T. ) ;
#58805 = AXIS2_PLACEMENT_3D ( 'NONE', #66026, #23097, #17820 ) ;
#58806 = ORIENTED_EDGE ( 'NONE', *, *, #32620, .T. ) ;
#58807 = AXIS2_PLACEMENT_3D ( 'NONE', #26227, #10379, #68450 ) ;
#58808 = CARTESIAN_POINT ( 'NONE',  ( 63.01563776193091826, 12.67277567978500130, -35.72069083216973695 ) ) ;
#58809 = ADVANCED_FACE ( 'NONE', ( #30780, #40981, #62443 ), #14258, .T. ) ;
#58810 = FACE_OUTER_BOUND ( 'NONE', #69168, .T. ) ;
#58811 = AXIS2_PLACEMENT_3D ( 'NONE', #48870, #47849, #53118 ) ;
#58812 = CARTESIAN_POINT ( 'NONE',  ( -173.1211646369891355, 88.63826465341152527, -7.867406574286299303 ) ) ;
#58813 = VECTOR ( 'NONE', #61344, 1000.000000000000000 ) ;
#58814 = PLANE ( 'NONE',  #44097 ) ;
#58815 = VERTEX_POINT ( 'NONE', #41336 ) ;
#58816 = CARTESIAN_POINT ( 'NONE',  ( 280.0000000000000000, 21.42428528562853529, 4.999999999999990230 ) ) ;
#58817 = CARTESIAN_POINT ( 'NONE',  ( 183.1873354889583254, 82.20882912211250471, -24.09245173917307881 ) ) ;
#58818 = CARTESIAN_POINT ( 'NONE',  ( -85.09761763353360209, 24.87634954265997678, -11.90396085173015095 ) ) ;
#58819 = DIRECTION ( 'NONE',  ( 0.000000000000000000, 0.000000000000000000, -1.000000000000000000 ) ) ;
#58820 = CARTESIAN_POINT ( 'NONE',  ( 44.86216938219162387, 9.182565662897477665, -21.42266460005981799 ) ) ;
#58821 = CARTESIAN_POINT ( 'NONE',  ( 206.6955592216991420, 109.1214665502618004, -24.22191070065747098 ) ) ;
#58822 = FACE_BOUND ( 'NONE', #30976, .T. ) ;
#58823 = ADVANCED_FACE ( 'NONE', ( #52224 ), #14593, .T. ) ;
#58824 = CARTESIAN_POINT ( 'NONE',  ( 164.9547823171480729, 65.03046442419433504, 63.19433658183190516 ) ) ;
#58825 = EDGE_CURVE ( 'NONE', #45918, #3538, #4047, .T. ) ;
#58826 = ADVANCED_FACE ( 'NONE', ( #20551 ), #43386, .T. ) ;
#58827 = ORIENTED_EDGE ( 'NONE', *, *, #59236, .F. ) ;
#58828 = LINE ( 'NONE', #50377, #57103 ) ;
#58829 = CARTESIAN_POINT ( 'NONE',  ( 0.000000000000000000, 0.000000000000000000, 40.00000000000003553 ) ) ;
#58830 = DIRECTION ( 'NONE',  ( 0.000000000000000000, 1.000000000000000000, 0.000000000000000000 ) ) ;
#58831 = DIRECTION ( 'NONE',  ( 1.000000000000000000, 0.000000000000000000, -0.000000000000000000 ) ) ;
#58832 = EDGE_CURVE ( 'NONE', #48157, #43438, #29871, .T. ) ;
#58833 = CARTESIAN_POINT ( 'NONE',  ( 151.7819978880463054, 53.35998893001565335, 5.170581360776508539 ) ) ;
#58834 = CARTESIAN_POINT ( 'NONE',  ( -10.38356729277384005, 8.080077440779504627, 84.24699796321192480 ) ) ;
#58835 = VERTEX_POINT ( 'NONE', #59215 ) ;
#58836 = CARTESIAN_POINT ( 'NONE',  ( 445.3372781065086201, 217.8591479523844612, 78.55029585798806124 ) ) ;
#58837 = CARTESIAN_POINT ( 'NONE',  ( 15.55634918610403261, 4.999999999999969802, 2.000000000000001776 ) ) ;
#58838 = EDGE_LOOP ( 'NONE', ( #23788, #1399, #21341, #61366, #36902, #39603 ) ) ;
#58839 = ORIENTED_EDGE ( 'NONE', *, *, #63068, .F. ) ;
#58840 = CARTESIAN_POINT ( 'NONE',  ( 42.90062197766265228, 9.906944503464883311, 84.46083066505832448 ) ) ;
#58841 = DIRECTION ( 'NONE',  ( 0.000000000000000000, 1.000000000000000000, 0.000000000000000000 ) ) ;
#58842 = LINE ( 'NONE', #5040, #62828 ) ;
#58844 = ORIENTED_EDGE ( 'NONE', *, *, #68920, .T. ) ;
#58843 = EDGE_CURVE ( 'NONE', #8050, #11364, #34275, .T. ) ;
#58845 = CARTESIAN_POINT ( 'NONE',  ( -58.96922974609609014, 15.76655591015166458, -75.96166564116519737 ) ) ;
#58846 = VECTOR ( 'NONE', #34267, 1000.000000000000000 ) ;
#58847 = CARTESIAN_POINT ( 'NONE',  ( 36.08729376665095145, 8.001156100723203934, -9.529628389809701616 ) ) ;
#58848 = EDGE_CURVE ( 'NONE', #4257, #25778, #36528, .T. ) ;
#58850 = EDGE_CURVE ( 'NONE', #23357, #38023, #3938, .T. ) ;
#58849 = CARTESIAN_POINT ( 'NONE',  ( 174.6307688320643479, 73.70327352127000609, -47.55585792078556295 ) ) ;
#58851 = CARTESIAN_POINT ( 'NONE',  ( 164.4125506877668101, 63.25654226895625953, 93.46064493613914692 ) ) ;
#58852 = CIRCLE ( 'NONE', #36377, 72.99999999999998579 ) ;
#58853 = CARTESIAN_POINT ( 'NONE',  ( 91.11342358617754655, 21.00000175105273215, 31.19529170996127476 ) ) ;
#58854 = EDGE_LOOP ( 'NONE', ( #8482, #47639, #64470, #24874 ) ) ;
#58855 = CARTESIAN_POINT ( 'NONE',  ( 103.0004140566502997, 26.76634862952791138, -14.56365336300195601 ) ) ;
#58856 = VECTOR ( 'NONE', #65704, 1000.000000000000000 ) ;
#58857 = DIRECTION ( 'NONE',  ( 0.000000000000000000, 0.000000000000000000, 1.000000000000000000 ) ) ;
#58858 = CARTESIAN_POINT ( 'NONE',  ( -29.50439180771547854, 10.29976981300626981, 30.45393202935034438 ) ) ;
#58859 = CARTESIAN_POINT ( 'NONE',  ( 51.39999999999999858, 0.000000000000000000, 0.000000000000000000 ) ) ;
#58860 = CARTESIAN_POINT ( 'NONE',  ( 0.000000000000000000, 0.000000000000000000, 7.000000000000000000 ) ) ;
#58862 = ORIENTED_EDGE ( 'NONE', *, *, #34648, .T. ) ;
#58861 = CARTESIAN_POINT ( 'NONE',  ( 41.66904755831208007, -10.55634918610412853, 85.00100000000000477 ) ) ;
#58863 = ORIENTED_EDGE ( 'NONE', *, *, #23985, .F. ) ;
#58864 = VERTEX_POINT ( 'NONE', #44435 ) ;
#58865 = CARTESIAN_POINT ( 'NONE',  ( 117.7417271423230147, 33.63613196344607559, -69.73183056102243427 ) ) ;
#58866 = FACE_OUTER_BOUND ( 'NONE', #27847, .T. ) ;
#58867 = PLANE ( 'NONE',  #34374 ) ;
#58868 = LINE ( 'NONE', #31804, #35036 ) ;
#58869 = LINE ( 'NONE', #21584, #9674 ) ;
#58870 = CARTESIAN_POINT ( 'NONE',  ( 150.0889146124742695, 52.13243511955542431, -71.82499747338286511 ) ) ;
#58871 = CARTESIAN_POINT ( 'NONE',  ( 196.9999999999999716, 2.999999999999969802, 0.000000000000000000 ) ) ;
#58872 = ORIENTED_EDGE ( 'NONE', *, *, #20307, .T. ) ;
#58873 = DIRECTION ( 'NONE',  ( 0.000000000000000000, 0.000000000000000000, 1.000000000000000000 ) ) ;
#58874 = EDGE_LOOP ( 'NONE', ( #64741, #69285, #39182, #35816 ) ) ;
#58875 = ORIENTED_EDGE ( 'NONE', *, *, #39245, .T. ) ;
#58876 = B_SPLINE_CURVE_WITH_KNOTS ( 'NONE', 3,
 ( #69108, #26559, #69459, #32872, #27238, #1214, #60651, #1559, #33235, #12464, #22319, #6493, #38861, #43759, #28289, #54665, #23021, #44473, #49382, #33586, #50100, #65230, #17024, #27940, #33929, #22667, #37801, #49730, #21964, #44106, #59248, #54304, #1929, #866, #55367, #44826, #12123, #23388, #38142, #59582, #65589, #7188, #48671 ),
 .UNSPECIFIED., .F., .F.,
 ( 4, 2, 2, 2, 2, 2, 2, 2, 1, 2, 2, 2, 2, 2, 2, 2, 2, 2, 2, 2, 2, 4 ),
 ( 0.000000000000000000, 0.001466540241398136407, 0.002199810362097204611, 0.002933080482796272814, 0.004399620724194415293, 0.005866160965592556904, 0.007332701206990699383, 0.008065971327689771056, 0.008799241448388842729, 0.009532511569087912667, 0.01026578168978698261, 0.01173232193118512422, 0.01319886217258326756, 0.01466540241398140744, 0.01539867253468046870, 0.01613194265537952823, 0.01759848289677765423, 0.01906502313817577329, 0.01979829325887483282, 0.02053156337957389582, 0.02199810362097202529, 0.02346464386237015476 ),
 .UNSPECIFIED. ) ;
#58877 = CARTESIAN_POINT ( 'NONE',  ( -67.03031041878422513, -33.66749151869545642, 43.58025477438756923 ) ) ;
#58878 = CARTESIAN_POINT ( 'NONE',  ( -62.21585762900409833, 17.77081916367992420, -94.14025316589223280 ) ) ;
#58879 = CARTESIAN_POINT ( 'NONE',  ( -30.17038805258401624, 10.40524961744439736, 84.00665816972750122 ) ) ;
#58880 = CARTESIAN_POINT ( 'NONE',  ( -151.2428028786327445, 66.99705074331119192, 4.066794807898307162 ) ) ;
#58881 = DIRECTION ( 'NONE',  ( 0.000000000000000000, 0.000000000000000000, -1.000000000000000000 ) ) ;
#58882 = CARTESIAN_POINT ( 'NONE',  ( 23.03864809957654103, 6.841061756139152905, 39.44928671615922156 ) ) ;
#58883 = LINE ( 'NONE', #21951, #49777 ) ;
#58884 = EDGE_LOOP ( 'NONE', ( #490, #31788, #41712, #21625 ) ) ;
#58885 = VERTEX_POINT ( 'NONE', #27556 ) ;
#58886 = ORIENTED_EDGE ( 'NONE', *, *, #18265, .T. ) ;
#58887 = ADVANCED_FACE ( 'NONE', ( #23352 ), #7158, .F. ) ;
#58888 = CIRCLE ( 'NONE', #54359, 245.3095347406802205 ) ;
#58889 = DIRECTION ( 'NONE',  ( 1.000000000000000000, 2.575717417130363489E-14, 0.000000000000000000 ) ) ;
#58890 = CARTESIAN_POINT ( 'NONE',  ( 32.66364305947235636, 8.639871491745257259, -39.78980533262777897 ) ) ;
#58891 = B_SPLINE_CURVE_WITH_KNOTS ( 'NONE', 3,
 ( #49958, #1794, #23250, #60861, #44695, #55586, #12685, #50322, #2140, #66513, #23935, #13047, #34507, #9142, #25332, #52721, #41843, #62252, #30256, #40798, #68573, #41153, #36568, #9836, #57680, #3512, #30598, #62614, #46769, #24639, #20374, #3865, #67894, #46415, #42181, #14422, #36909, #25678, #68901, #58018, #36219, #46073, #15457, #19689, #68237, #20045, #51705 ),
 .UNSPECIFIED., .F., .F.,
 ( 4, 2, 2, 2, 2, 2, 2, 2, 2, 2, 2, 1, 2, 2, 2, 2, 2, 2, 2, 2, 2, 2, 2, 4 ),
 ( 0.000000000000000000, 0.003297771944419005796, 0.004122214930523717021, 0.004946657916628427812, 0.006595543888837832915, 0.007419986874942573196, 0.008244429861047314345, 0.009068872847152055494, 0.009893315833256796643, 0.01154220180546627027, 0.01236664479157100795, 0.01319108777767574216, 0.01401553076378047984, 0.01483997374988521752, 0.01566441673598995346, 0.01648885972209469114, 0.01813774569430418038, 0.01896218868040890071, 0.01978663166651362104, 0.02061107465261834484, 0.02143551763872306518, 0.02308440361093250931, 0.02473328958314195691, 0.02638217555535139758 ),
 .UNSPECIFIED. ) ;
#58892 = PRESENTATION_LAYER_ASSIGNMENT (  '', '', ( #47488 ) ) ;
#58893 = CARTESIAN_POINT ( 'NONE',  ( -37.79601571721867259, 10.72155118426296738, 68.54850928335817173 ) ) ;
#58894 = CARTESIAN_POINT ( 'NONE',  ( 198.8752826725510658, 100.3130050945023299, 58.81793774317634416 ) ) ;
#58895 = ORIENTED_EDGE ( 'NONE', *, *, #211, .F. ) ;
#58896 = VECTOR ( 'NONE', #25714, 1000.000000000000000 ) ;
#58897 = LINE ( 'NONE', #11059, #48031 ) ;
#58898 = CARTESIAN_POINT ( 'NONE',  ( -154.7998111145352311, 68.80117179139327277, 59.72958456622436785 ) ) ;
#58899 = CARTESIAN_POINT ( 'NONE',  ( 22.89270809252618832, 7.840160460323052583, 13.08620663423853436 ) ) ;
#58900 = DIRECTION ( 'NONE',  ( -0.000000000000000000, 1.000000000000000000, -0.000000000000000000 ) ) ;
#58901 = CARTESIAN_POINT ( 'NONE',  ( -85.46258339457291697, 25.02772366257408621, -45.79754920329482815 ) ) ;
#58902 = AXIS2_PLACEMENT_3D ( 'NONE', #36331, #31063, #60198 ) ;
#58903 = CARTESIAN_POINT ( 'NONE',  ( 22.80839748737788142, 6.826915557457463812, 61.70818393205063046 ) ) ;
#58904 = EDGE_CURVE ( 'NONE', #54048, #34240, #43726, .T. ) ;
#58905 = DIRECTION ( 'NONE',  ( -0.000000000000000000, -0.000000000000000000, -1.000000000000000000 ) ) ;
#58906 = CARTESIAN_POINT ( 'NONE',  ( 14.80291736570134731, 7.477373894757625372, 18.12158280542935884 ) ) ;
#58907 = VECTOR ( 'NONE', #63881, 1000.000000000000114 ) ;
#58908 = AXIS2_PLACEMENT_3D ( 'NONE', #1416, #7039, #34832 ) ;
#58909 = ADVANCED_FACE ( 'NONE', ( #22636 ), #44795, .F. ) ;
#58910 = EDGE_CURVE ( 'NONE', #30082, #47961, #49698, .T. ) ;
#58911 = ORIENTED_EDGE ( 'NONE', *, *, #52494, .T. ) ;
#58912 = CARTESIAN_POINT ( 'NONE',  ( 56.48035995027147749, -49.34540444547771187, 0.000000000000000000 ) ) ;
#58913 = FACE_OUTER_BOUND ( 'NONE', #20588, .T. ) ;
#58914 = CARTESIAN_POINT ( 'NONE',  ( -132.0958200534847435, 50.71531800824803327, -46.63840928461922886 ) ) ;
#58915 = CARTESIAN_POINT ( 'NONE',  ( -102.7447593990059289, 34.14748189312172144, -50.01457726497595502 ) ) ;
#58916 = CARTESIAN_POINT ( 'NONE',  ( 55.91133443650745960, 12.16263767238152127, -72.51936885403362965 ) ) ;
#58917 = ORIENTED_EDGE ( 'NONE', *, *, #52575, .F. ) ;
#58918 = EDGE_LOOP ( 'NONE', ( #28114, #41159, #50704, #32211 ) ) ;
#58919 = CARTESIAN_POINT ( 'NONE',  ( -24.18258876560172865, 8.512344710720677554, -17.93097106050854705 ) ) ;
#58920 = CARTESIAN_POINT ( 'NONE',  ( 174.6808034781869878, 72.36770494831971234, 86.57635966052535537 ) ) ;
#58921 = ORIENTED_EDGE ( 'NONE', *, *, #67658, .T. ) ;
#58922 = ORIENTED_EDGE ( 'NONE', *, *, #20705, .F. ) ;
#58923 = CARTESIAN_POINT ( 'NONE',  ( 110.7164744784863899, 29.10110206241301967, 71.45576479620105204 ) ) ;
#58924 = VERTEX_POINT ( 'NONE', #17351 ) ;
#58925 = CARTESIAN_POINT ( 'NONE',  ( 130.7260570116704343, 40.73146260246713268, -63.53671823496143389 ) ) ;
#58926 = FACE_OUTER_BOUND ( 'NONE', #34539, .T. ) ;
#58927 = LINE ( 'NONE', #64565, #18744 ) ;
#58928 = CARTESIAN_POINT ( 'NONE',  ( 0.000000000000000000, 0.000000000000000000, 41.38025477438755928 ) ) ;
#58929 = ADVANCED_FACE ( 'NONE', ( #54637 ), #7304, .T. ) ;
#58930 = CARTESIAN_POINT ( 'NONE',  ( 163.5277822717018523, 62.51852278986679323, -92.88600173900509560 ) ) ;
#58931 = CARTESIAN_POINT ( 'NONE',  ( -447.6627218934914367, 399.9999999999998863, -136.4497041420118251 ) ) ;
#58932 = DIRECTION ( 'NONE',  ( -1.000000000000000000, 0.000000000000000000, 0.000000000000000000 ) ) ;
#58933 = EDGE_CURVE ( 'NONE', #27439, #39998, #1529, .T. ) ;
#58934 = VERTEX_POINT ( 'NONE', #49000 ) ;
#58935 = ORIENTED_EDGE ( 'NONE', *, *, #55332, .T. ) ;
#58936 = CARTESIAN_POINT ( 'NONE',  ( -121.1775535805057444, 43.46577565517550568, -9.717201679529251734 ) ) ;
#58937 = VECTOR ( 'NONE', #62444, 1000.000000000000000 ) ;
#58938 = CARTESIAN_POINT ( 'NONE',  ( 0.000000000000000000, 0.000000000000000000, 2.000000000000000000 ) ) ;
#58939 = CARTESIAN_POINT ( 'NONE',  ( -178.2427210808089626, 93.01567669683339545, -20.85170211881552760 ) ) ;
#58940 = CARTESIAN_POINT ( 'NONE',  ( -165.7713056973201446, 80.74264649718244868, -67.53382473510175998 ) ) ;
#58941 = VECTOR ( 'NONE', #48272, 1000.000000000000000 ) ;
#58943 = ORIENTED_EDGE ( 'NONE', *, *, #18055, .T. ) ;
#58942 = CARTESIAN_POINT ( 'NONE',  ( -142.9728934044262019, 58.82891228489262403, -46.03245465095029232 ) ) ;
#58944 = LINE ( 'NONE', #10763, #6063 ) ;
#58945 = AXIS2_PLACEMENT_3D ( 'NONE', #44158, #13223, #1611 ) ;
#58946 = AXIS2_PLACEMENT_3D ( 'NONE', #47998, #65231, #15997 ) ;
#58947 = EDGE_LOOP ( 'NONE', ( #24355, #57897, #14666, #30229, #2032, #25717, #16548, #20047, #3727 ) ) ;
#58948 = DIRECTION ( 'NONE',  ( 0.000000000000000000, 0.000000000000000000, 1.000000000000000000 ) ) ;
#58949 = FACE_OUTER_BOUND ( 'NONE', #67423, .T. ) ;
#58950 = VECTOR ( 'NONE', #58984, 1000.000000000000000 ) ;
#58951 = AXIS2_PLACEMENT_3D ( 'NONE', #3500, #24968, #3853 ) ;
#58952 = LINE ( 'NONE', #11810, #38796 ) ;
#58953 = CARTESIAN_POINT ( 'NONE',  ( -127.6881387055492922, 48.89937523111243678, -76.54403142618212996 ) ) ;
#58954 = CARTESIAN_POINT ( 'NONE',  ( -38.04732649588432736, -4.679373836065037651, 13.32819299319724493 ) ) ;
#58955 = VECTOR ( 'NONE', #69062, 1000.000000000000000 ) ;
#58956 = FACE_BOUND ( 'NONE', #47981, .T. ) ;
#58957 = CARTESIAN_POINT ( 'NONE',  ( -149.5074843970971301, 64.17983161892347255, -88.50193171241930656 ) ) ;
#58958 = ORIENTED_EDGE ( 'NONE', *, *, #1499, .T. ) ;
#58959 = EDGE_LOOP ( 'NONE', ( #12751, #52963 ) ) ;
#58960 = CARTESIAN_POINT ( 'NONE',  ( 184.3941060377212295, 82.01604625189466446, -77.31420240063759763 ) ) ;
#58961 = CARTESIAN_POINT ( 'NONE',  ( 111.9975424824652634, 0.000000000000000000, 256.6193948016162381 ) ) ;
#58962 = CARTESIAN_POINT ( 'NONE',  ( -165.9111709580270997, 79.44576090485632847, -40.12534605873958071 ) ) ;
#58963 = CARTESIAN_POINT ( 'NONE',  ( -12.99999999999999645, 10.00000000000000000, -33.00000000000000000 ) ) ;
#58964 = PRODUCT_DEFINITION ( 'UNKNOWN', '', #6281, #26126 ) ;
#58965 = CARTESIAN_POINT ( 'NONE',  ( 103.8055367708241192, 27.11070767929350112, -66.38655192125422388 ) ) ;
#58966 = CARTESIAN_POINT ( 'NONE',  ( -77.71801202538873099, 23.03755222122951452, -62.00518611626486631 ) ) ;
#58967 = CARTESIAN_POINT ( 'NONE',  ( 17.05487753766634285, -34.33113485734955361, 13.32819397642332504 ) ) ;
#58968 = CARTESIAN_POINT ( 'NONE',  ( -124.9970785861867739, 47.10847819093958577, 30.67033377869767818 ) ) ;
#58969 = CARTESIAN_POINT ( 'NONE',  ( 212.1983751099433846, 117.2326047784727336, 63.69360226375801659 ) ) ;
#58971 = EDGE_LOOP ( 'NONE', ( #51763, #22765 ) ) ;
#58970 = ADVANCED_FACE ( 'NONE', ( #39178 ), #60621, .F. ) ;
#58972 = CARTESIAN_POINT ( 'NONE',  ( -109.3432140528234839, 36.51591785955882585, -13.09559261180481116 ) ) ;
#58973 = VERTEX_POINT ( 'NONE', #56042 ) ;
#58974 = FACE_OUTER_BOUND ( 'NONE', #3506, .T. ) ;
#58975 = EDGE_CURVE ( 'NONE', #14285, #42689, #50923, .T. ) ;
#58976 = DIRECTION ( 'NONE',  ( 1.000000000000000000, 0.000000000000000000, 0.000000000000000000 ) ) ;
#58977 = CARTESIAN_POINT ( 'NONE',  ( -84.88037603621106086, 24.78657832303205666, -92.09904858809437656 ) ) ;
#58978 = CARTESIAN_POINT ( 'NONE',  ( 150.2076397309211586, 52.21780102759852582, -18.67121458051684613 ) ) ;
#58979 = DIRECTION ( 'NONE',  ( 1.000000000000000000, -0.000000000000000000, 0.000000000000000000 ) ) ;
#58980 = CARTESIAN_POINT ( 'NONE',  ( 400.0000000000000000, 0.000000000000000000, 0.000000000000000000 ) ) ;
#58981 = CARTESIAN_POINT ( 'NONE',  ( 26.69682282325795697, -59.27986298182186431, 170.0000000000000000 ) ) ;
#58982 = VERTEX_POINT ( 'NONE', #34939 ) ;
#58983 = CARTESIAN_POINT ( 'NONE',  ( 206.0202013761258115, 108.1716492322431264, 82.99495773477644889 ) ) ;
#58984 = DIRECTION ( 'NONE',  ( 1.000000000000000000, 0.000000000000000000, 0.000000000000000000 ) ) ;
#58985 = ORIENTED_EDGE ( 'NONE', *, *, #871, .T. ) ;
#58986 = DIRECTION ( 'NONE',  ( 0.000000000000000000, 0.000000000000000000, -1.000000000000000000 ) ) ;
#58987 = CARTESIAN_POINT ( 'NONE',  ( 12.91653440534542341, 7.431946726541410975, -76.80479733579223023 ) ) ;
#58988 = PLANE ( 'NONE',  #56712 ) ;
#58989 = CARTESIAN_POINT ( 'NONE',  ( -38.27142574863722047, -2.189438189322980843, 13.32819397642333037 ) ) ;
#58990 = ADVANCED_FACE ( 'NONE', ( #51114 ), #3273, .F. ) ;
#58991 = CARTESIAN_POINT ( 'NONE',  ( -2.874437057892791803, 6.618922960888052209, 31.96075603522317010 ) ) ;
#58992 = DIRECTION ( 'NONE',  ( -1.000000000000000000, -0.000000000000000000, -0.000000000000000000 ) ) ;
#58993 = CARTESIAN_POINT ( 'NONE',  ( 87.94810462138822515, 20.94053779377377822, 83.51093339085589662 ) ) ;
#58994 = ADVANCED_FACE ( 'NONE', ( #25428 ), #8552, .F. ) ;
#58995 = ADVANCED_FACE ( 'NONE', ( #2579 ), #40547, .F. ) ;
#58996 = ORIENTED_EDGE ( 'NONE', *, *, #31073, .F. ) ;
#58997 = DIRECTION ( 'NONE',  ( 1.000000000000000000, 1.005272254328555925E-14, 1.005272254328559869E-14 ) ) ;
#58998 = DIRECTION ( 'NONE',  ( 0.000000000000000000, 1.000000000000000000, -0.000000000000000000 ) ) ;
#58999 = CARTESIAN_POINT ( 'NONE',  ( -132.0958200534847435, 50.71531800824803327, 7.050691896308118878 ) ) ;
#59000 = CARTESIAN_POINT ( 'NONE',  ( -108.6944271866238978, 37.30738480893074893, 68.78232788442275591 ) ) ;
#59001 = CARTESIAN_POINT ( 'NONE',  ( -180.6134399488801705, 95.87473607775544338, 91.62122452033388242 ) ) ;
#59002 = ORIENTED_EDGE ( 'NONE', *, *, #53146, .F. ) ;
#59004 = CARTESIAN_POINT ( 'NONE',  ( -17.50000000000000000, -17.50000000000000000, 1.999999999999998224 ) ) ;
#59003 = VECTOR ( 'NONE', #18336, 1000.000000000000000 ) ;
#59005 = VECTOR ( 'NONE', #36100, 1000.000000000000000 ) ;
#59006 = CARTESIAN_POINT ( 'NONE',  ( 94.11746922806584337, 22.11341285603780804, 64.54865186196720117 ) ) ;
#59007 =( GEOMETRIC_REPRESENTATION_CONTEXT ( 3 ) GLOBAL_UNCERTAINTY_ASSIGNED_CONTEXT ( ( #12116 ) ) GLOBAL_UNIT_ASSIGNED_CONTEXT ( ( #53269, #43062, #26898 ) ) REPRESENTATION_CONTEXT ( 'NONE', 'WORKASPACE' ) );
#59008 = CARTESIAN_POINT ( 'NONE',  ( 198.4045886930829283, 99.71425793793710568, -21.07018120517999549 ) ) ;
#59009 = CONICAL_SURFACE ( 'NONE', #5132, 8.000000000000001776, 1.047197551196595855 ) ;
#59010 = CARTESIAN_POINT ( 'NONE',  ( -156.9834569011572682, 70.78920417036412971, 91.28448318999808464 ) ) ;
#59011 = AXIS2_PLACEMENT_3D ( 'NONE', #30601, #56635, #66866 ) ;
#59012 = CARTESIAN_POINT ( 'NONE',  ( 140.8984307802396643, 45.84194788389002895, 34.37783282223308134 ) ) ;
#59013 = ORIENTED_EDGE ( 'NONE', *, *, #50736, .F. ) ;
#59014 = DIRECTION ( 'NONE',  ( -0.9639628606958550172, 0.2660368455666687892, 0.000000000000000000 ) ) ;
#59015 = CARTESIAN_POINT ( 'NONE',  ( 81.57915404881515542, 18.81499384983929701, 4.817277352176767558 ) ) ;
#59016 = CARTESIAN_POINT ( 'NONE',  ( 15.55634918610403261, 4.999999999999969802, 0.000000000000000000 ) ) ;
#59017 = DIRECTION ( 'NONE',  ( 1.000000000000000000, 0.000000000000000000, 0.000000000000000000 ) ) ;
#59018 = ORIENTED_EDGE ( 'NONE', *, *, #7336, .T. ) ;
#59019 = EDGE_CURVE ( 'NONE', #61067, #25434, #35969, .T. ) ;
#59020 = DIRECTION ( 'NONE',  ( -1.000000000000000000, 0.000000000000000000, 0.000000000000000000 ) ) ;
#59021 = EDGE_LOOP ( 'NONE', ( #37788, #979, #38665, #13956 ) ) ;
#59022 = CARTESIAN_POINT ( 'NONE',  ( -74.19961951691010427, 20.67022044985853313, -21.80058496222482134 ) ) ;
#59023 = CARTESIAN_POINT ( 'NONE',  ( 67.55134213333079174, 13.77030723107741395, -76.05851458524612951 ) ) ;
#59024 = CARTESIAN_POINT ( 'NONE',  ( -61.51762070241280611, 16.51067482779403406, 41.62754106045760949 ) ) ;
#59026 = VERTEX_POINT ( 'NONE', #66960 ) ;
#59025 = LINE ( 'NONE', #38265, #8468 ) ;
#59027 = CARTESIAN_POINT ( 'NONE',  ( 163.1265310614427619, 62.18610413911356005, 31.97814890642583663 ) ) ;
#59028 = CARTESIAN_POINT ( 'NONE',  ( 18.89356949897823768, 62.19351277735707839, 40.00000000000003553 ) ) ;
#59029 = DIRECTION ( 'NONE',  ( 0.000000000000000000, 0.000000000000000000, 1.000000000000000000 ) ) ;
#59030 = ORIENTED_EDGE ( 'NONE', *, *, #8179, .F. ) ;
#59031 = CARTESIAN_POINT ( 'NONE',  ( -145.6181732888550471, 62.24768171590013566, -89.57533543414972144 ) ) ;
#59032 = LINE ( 'NONE', #10853, #47688 ) ;
#59033 = CARTESIAN_POINT ( 'NONE',  ( -179.8926034784146282, 96.58272071140105197, 35.08552098014282450 ) ) ;
#59034 = CARTESIAN_POINT ( 'NONE',  ( 126.4219470349615904, 38.26519385429185149, 64.87749366262461592 ) ) ;
#59035 = ORIENTED_EDGE ( 'NONE', *, *, #2326, .F. ) ;
#59036 = ORIENTED_EDGE ( 'NONE', *, *, #21663, .T. ) ;
#59037 = AXIS2_PLACEMENT_3D ( 'NONE', #8560, #35641, #14177 ) ;
#59038 = EDGE_LOOP ( 'NONE', ( #49073, #8391, #9852, #33191 ) ) ;
#59039 = ADVANCED_FACE ( 'NONE', ( #19436 ), #13814, .F. ) ;
#59040 = CARTESIAN_POINT ( 'NONE',  ( -104.5740066103012680, 35.09687312794774527, 4.030067934921061301 ) ) ;
#59041 = CIRCLE ( 'NONE', #46711, 246.3582898394606957 ) ;
#59042 = VECTOR ( 'NONE', #59173, 1000.000000000000000 ) ;
#59043 =( LENGTH_UNIT ( ) NAMED_UNIT ( * ) SI_UNIT ( .MILLI., .METRE. ) );
#59044 = LINE ( 'NONE', #9844, #22090 ) ;
#59045 = LINE ( 'NONE', #37246, #30360 ) ;
#59046 = FACE_OUTER_BOUND ( 'NONE', #7378, .T. ) ;
#59047 = CARTESIAN_POINT ( 'NONE',  ( 110.2429982417149432, 28.88204397445228722, 71.45576479620103783 ) ) ;
#59048 = AXIS2_PLACEMENT_3D ( 'NONE', #2911, #66947, #9225 ) ;
#59049 = EDGE_CURVE ( 'NONE', #41081, #43897, #52144, .T. ) ;
#59050 = FACE_BOUND ( 'NONE', #12808, .T. ) ;
#59051 = EDGE_LOOP ( 'NONE', ( #33547, #14356, #41221, #68916 ) ) ;
#59053 = AXIS2_PLACEMENT_3D ( 'NONE', #39009, #61152, #33023 ) ;
#59052 = CARTESIAN_POINT ( 'NONE',  ( -46.66904755831210139, 5.000000000000066613, 2.000000000000001776 ) ) ;
#59055 = ORIENTED_EDGE ( 'NONE', *, *, #10165, .F. ) ;
#59054 = EDGE_CURVE ( 'NONE', #42011, #15039, #60131, .T. ) ;
#59056 = CARTESIAN_POINT ( 'NONE',  ( -78.66644367742109978, 23.39876645725289706, 57.26275173013680586 ) ) ;
#59057 = CARTESIAN_POINT ( 'NONE',  ( 188.5843222076478014, 86.53342480589844854, 37.10520038439885582 ) ) ;
#59058 = DIRECTION ( 'NONE',  ( 0.000000000000000000, 0.000000000000000000, -1.000000000000000000 ) ) ;
#59059 = CARTESIAN_POINT ( 'NONE',  ( -74.79002408692177539, 20.88280597089420709, 17.49881191264313429 ) ) ;
#59060 = CARTESIAN_POINT ( 'NONE',  ( 15.55634918610403261, -3.079134169858832593E-14, 85.00100000000000477 ) ) ;
#59061 = EDGE_CURVE ( 'NONE', #52558, #17523, #43295, .T. ) ;
#59062 = CARTESIAN_POINT ( 'NONE',  ( 22.15943197741200876, 7.796127622097904997, 33.55009939024217402 ) ) ;
#59063 = DIRECTION ( 'NONE',  ( 1.000000000000000000, 0.000000000000000000, 0.000000000000000000 ) ) ;
#59064 = CARTESIAN_POINT ( 'NONE',  ( 162.7963212667073378, 63.21900188423069977, -65.18246456083083729 ) ) ;
#59065 = VERTEX_POINT ( 'NONE', #52488 ) ;
#59066 = DIRECTION ( 'NONE',  ( 0.000000000000000000, 0.000000000000000000, 1.000000000000000000 ) ) ;
#59067 = CARTESIAN_POINT ( 'NONE',  ( -4.164416015344991173, -64.86646004871191451, 40.00000000000003553 ) ) ;
#59068 = EDGE_LOOP ( 'NONE', ( #45528, #57332, #9994, #40935 ) ) ;
#59069 = ORIENTED_EDGE ( 'NONE', *, *, #47545, .T. ) ;
#59070 = CARTESIAN_POINT ( 'NONE',  ( -29.04400972079232446, 10.22852224114065223, -62.55024186826118893 ) ) ;
#59071 = CARTESIAN_POINT ( 'NONE',  ( -190.6985136298601731, 109.1272424661242582, -95.00000000000133582 ) ) ;
#59072 = PRESENTATION_STYLE_ASSIGNMENT (( #21442 ) ) ;
#59073 = CARTESIAN_POINT ( 'NONE',  ( 16.78635691501517613, 0.000000000000000000, -14.43565316649550034 ) ) ;
#59074 = ADVANCED_FACE ( 'NONE', ( #69355 ), #31384, .F. ) ;
#59075 = VERTEX_POINT ( 'NONE', #15888 ) ;
#59076 = ORIENTED_EDGE ( 'NONE', *, *, #35155, .T. ) ;
#59077 = CARTESIAN_POINT ( 'NONE',  ( -131.6399667378751133, 51.62465701391629125, 42.96608471902324311 ) ) ;
#59078 = VERTEX_POINT ( 'NONE', #53152 ) ;
#59079 = CARTESIAN_POINT ( 'NONE',  ( 181.0840389613909736, 78.60582251573002566, 17.46404351504774510 ) ) ;
#59080 = CARTESIAN_POINT ( 'NONE',  ( 182.8317132966081999, 81.83833949797246987, -90.11192720193595562 ) ) ;
#59081 = CARTESIAN_POINT ( 'NONE',  ( 60.62939143133407072, 12.13148391928981162, 57.03056178573838508 ) ) ;
#59082 = PLANE ( 'NONE',  #34083 ) ;
#59083 = PRODUCT ( 'cutting blade 2', 'cutting blade 2', '', ( #6931 ) ) ;
#59084 = CARTESIAN_POINT ( 'NONE',  ( 46.66904755831212981, 15.55634918610394379, 2.000000000000001776 ) ) ;
#59085 = DIRECTION ( 'NONE',  ( 1.000000000000000000, 1.776356839400250465E-14, 0.000000000000000000 ) ) ;
#59086 = AXIS2_PLACEMENT_3D ( 'NONE', #13394, #34856, #60534 ) ;
#59087 = CARTESIAN_POINT ( 'NONE',  ( 86.62931800182293784, 20.48449268398422163, -62.66611478937537782 ) ) ;
#59088 = ORIENTED_EDGE ( 'NONE', *, *, #13298, .F. ) ;
#59089 = ORIENTED_EDGE ( 'NONE', *, *, #27062, .F. ) ;
#59090 = CARTESIAN_POINT ( 'NONE',  ( 442.3372781065083927, 392.9289321881345813, 108.5502958579881465 ) ) ;
#59091 = CYLINDRICAL_SURFACE ( 'NONE', #58644, 8.000000000000000000 ) ;
#59092 = CYLINDRICAL_SURFACE ( 'NONE', #16180, 65.00000000000000000 ) ;
#59093 = CARTESIAN_POINT ( 'NONE',  ( -2.699999999999990408, 0.000000000000000000, -19.99999999999999645 ) ) ;
#59094 = CARTESIAN_POINT ( 'NONE',  ( 70.46452034227868921, 14.52462608639673469, 36.30783829542910013 ) ) ;
#59095 = CARTESIAN_POINT ( 'NONE',  ( 9.319975126229035567, 7.386007236262731368, 94.99999999999866418 ) ) ;
#59096 = VECTOR ( 'NONE', #33945, 1000.000000000000000 ) ;
#59097 = VECTOR ( 'NONE', #33170, 1000.000000000000000 ) ;
#59098 = VERTEX_POINT ( 'NONE', #25772 ) ;
#59099 = AXIS2_PLACEMENT_3D ( 'NONE', #45607, #19211, #18532 ) ;
#59100 = VECTOR ( 'NONE', #50151, 999.9999999999998863 ) ;
#59101 = CARTESIAN_POINT ( 'NONE',  ( 86.62931800182293784, 19.42108912189599934, 17.86753698201564688 ) ) ;
#59102 = ORIENTED_EDGE ( 'NONE', *, *, #66240, .F. ) ;
#59103 = CARTESIAN_POINT ( 'NONE',  ( 15.78827728214693416, -170.0000000000000000, -8.674393508222099314 ) ) ;
#59104 = ORIENTED_EDGE ( 'NONE', *, *, #53019, .T. ) ;
#59105 = VECTOR ( 'NONE', #14525, 1000.000000000000000 ) ;
#59106 = VERTEX_POINT ( 'NONE', #41931 ) ;
#59107 = CARTESIAN_POINT ( 'NONE',  ( -56.92000000000000171, -26.09918303830819397, 30.00000000000000000 ) ) ;
#59108 = FACE_OUTER_BOUND ( 'NONE', #7995, .T. ) ;
#59109 = CARTESIAN_POINT ( 'NONE',  ( 129.6961120139403647, 38.96846414226717314, 57.61019598173326273 ) ) ;
#59110 = ORIENTED_EDGE ( 'NONE', *, *, #5876, .T. ) ;
#59111 = CARTESIAN_POINT ( 'NONE',  ( 153.2384531768735769, 54.43344429203622781, 43.11883740112016739 ) ) ;
#59112 = CARTESIAN_POINT ( 'NONE',  ( 64.93224207568367490, 14.16036304753835040, 44.56800710844814972 ) ) ;
#59113 = LINE ( 'NONE', #13046, #15688 ) ;
#59114 = LINE ( 'NONE', #11274, #42389 ) ;
#59115 = CARTESIAN_POINT ( 'NONE',  ( -20.00000000000002842, 3.680555555555560243, 4.000000000000000000 ) ) ;
#59116 = CARTESIAN_POINT ( 'NONE',  ( -23.99924996210628336, 8.487987924059021694, 38.69610266098428042 ) ) ;
#59117 = CARTESIAN_POINT ( 'NONE',  ( -145.9181947914994169, 62.49417193455352759, -62.56801270397023274 ) ) ;
#59118 = EDGE_LOOP ( 'NONE', ( #17214, #16446 ) ) ;
#59119 = FACE_BOUND ( 'NONE', #9203, .T. ) ;
#59120 = CARTESIAN_POINT ( 'NONE',  ( -40.24154210098712525, -63.23235722614506216, 41.38025477438755928 ) ) ;
#59121 = CARTESIAN_POINT ( 'NONE',  ( -173.1211646369891355, 88.63826465341152527, 72.66624519710475738 ) ) ;
#59122 = CARTESIAN_POINT ( 'NONE',  ( 0.000000000000000000, 0.000000000000000000, 170.0000000000000000 ) ) ;
#59123 = CARTESIAN_POINT ( 'NONE',  ( -120.1650841064594033, 44.02024060322521848, -37.56662740794514832 ) ) ;
#59124 = CARTESIAN_POINT ( 'NONE',  ( -83.15209219203885027, 25.16621997697721014, 17.10401920708160262 ) ) ;
#59125 = CARTESIAN_POINT ( 'NONE',  ( 31.11269837220812562, 31.11269837220800483, 85.00100000000000477 ) ) ;
#59126 = CARTESIAN_POINT ( 'NONE',  ( 110.3314448577247049, 21.42428528562853174, 5.000000000000002665 ) ) ;
#59127 = PLANE ( 'NONE',  #24949 ) ;
#59128 = EDGE_CURVE ( 'NONE', #25857, #49232, #55761, .T. ) ;
#59129 = CARTESIAN_POINT ( 'NONE',  ( 63.98971758354223027, 12.90030016320050699, 17.92090471930345430 ) ) ;
#59130 = CARTESIAN_POINT ( 'NONE',  ( -86.06525741550315445, 26.37048289224654241, 66.01641903232457764 ) ) ;
#59131 = CARTESIAN_POINT ( 'NONE',  ( 40.23250010525561748, 9.533837034108117336, -89.34369780650632720 ) ) ;
#59132 = EDGE_LOOP ( 'NONE', ( #10125, #32341, #60946, #67429 ) ) ;
#59133 = AXIS2_PLACEMENT_3D ( 'NONE', #24904, #46001, #66789 ) ;
#59134 = CARTESIAN_POINT ( 'NONE',  ( -34.06637338149494809, 11.05895377318622863, 3.842940194179071067 ) ) ;
#59135 = ORIENTED_EDGE ( 'NONE', *, *, #29875, .T. ) ;
#59136 = DIRECTION ( 'NONE',  ( 0.000000000000000000, 0.000000000000000000, 1.000000000000000000 ) ) ;
#59137 = ORIENTED_EDGE ( 'NONE', *, *, #22332, .T. ) ;
#59138 = CARTESIAN_POINT ( 'NONE',  ( 18.20314211955701822, 7.596739727129573794, -76.98109712673615945 ) ) ;
#59139 = AXIS2_PLACEMENT_3D ( 'NONE', #45419, #51050, #66900 ) ;
#59140 = CARTESIAN_POINT ( 'NONE',  ( -51.66904755831212981, -10.55634918610397222, 0.000000000000000000 ) ) ;
#59141 = CARTESIAN_POINT ( 'NONE',  ( -142.8492950481059154, 60.01492924994603584, 61.60267790966557300 ) ) ;
#59142 = EDGE_CURVE ( 'NONE', #8416, #65524, #58784, .T. ) ;
#59143 = CARTESIAN_POINT ( 'NONE',  ( 70.38121440378670002, 14.50253793787158862, -14.89899490779335522 ) ) ;
#59144 = CARTESIAN_POINT ( 'NONE',  ( -24.03640295269301319, 9.507963273819775907, -44.04650067501650312 ) ) ;
#59145 = AXIS2_PLACEMENT_3D ( 'NONE', #66233, #33855, #65882 ) ;
#59146 = CARTESIAN_POINT ( 'NONE',  ( 0.000000000000000000, 0.000000000000000000, 41.38025477438755928 ) ) ;
#59147 = AXIS2_PLACEMENT_3D ( 'NONE', #44120, #11776, #60666 ) ;
#59148 = CARTESIAN_POINT ( 'NONE',  ( -74.27277138815051671, 21.76582788880764596, -90.22237058240676788 ) ) ;
#59149 = CYLINDRICAL_SURFACE ( 'NONE', #67835, 7.500000000000020428 ) ;
#59150 = ORIENTED_EDGE ( 'NONE', *, *, #3280, .F. ) ;
#59151 = VERTEX_POINT ( 'NONE', #42949 ) ;
#59152 = CARTESIAN_POINT ( 'NONE',  ( 61.28323125814100081, 21.66484633135460669, 170.0000000000000000 ) ) ;
#59153 = CARTESIAN_POINT ( 'NONE',  ( -166.0012244511291613, 80.97916541034754800, 62.79134880957640519 ) ) ;
#59154 = VECTOR ( 'NONE', #43115, 1000.000000000000000 ) ;
#59155 = DIRECTION ( 'NONE',  ( 1.000000000000000000, 0.000000000000000000, 0.000000000000000000 ) ) ;
#59156 = EDGE_CURVE ( 'NONE', #52761, #56686, #20627, .T. ) ;
#59157 = B_SPLINE_CURVE_WITH_KNOTS ( 'NONE', 3,
 ( #14521, #58451, #69007, #68669, #20144, #47544 ),
 .UNSPECIFIED., .F., .F.,
 ( 4, 2, 4 ),
 ( 0.03218935267740785644, 0.06469833035354445594, 0.09720730802968105544 ),
 .UNSPECIFIED. ) ;
#59158 = CARTESIAN_POINT ( 'NONE',  ( 92.91022130985207639, 21.66059330820416307, 94.99999999999866418 ) ) ;
#59159 = ORIENTED_EDGE ( 'NONE', *, *, #44236, .F. ) ;
#59160 = PLANE ( 'NONE',  #10935 ) ;
#59161 = CARTESIAN_POINT ( 'NONE',  ( 187.2384682876462136, 86.54721710842896698, -12.56464666103593153 ) ) ;
#59162 = CARTESIAN_POINT ( 'NONE',  ( -83.51052366780672287, 24.22613130369188283, -10.03992714516486906 ) ) ;
#59163 = CARTESIAN_POINT ( 'NONE',  ( 0.000000000000000000, 0.000000000000000000, 17.57656211871651308 ) ) ;
#59164 = CARTESIAN_POINT ( 'NONE',  ( 41.33692564073609077, 8.668977654195479943, -23.52549198662623908 ) ) ;
#59165 = CARTESIAN_POINT ( 'NONE',  ( 10.78925482157266913, -22.68765681156003566, 0.000000000000000000 ) ) ;
#59166 = CARTESIAN_POINT ( 'NONE',  ( -102.2801239173131194, -170.0000000000000000, 91.70817568734248937 ) ) ;
#59167 = CARTESIAN_POINT ( 'NONE',  ( 163.7403496014744064, 64.00600007368872468, 59.63034611569458576 ) ) ;
#59168 = B_SPLINE_CURVE_WITH_KNOTS ( 'NONE', 3,
 ( #28500, #66850, #6345, #23578 ),
 .UNSPECIFIED., .F., .F.,
 ( 4, 4 ),
 ( 9.900409499146238914E-07, 0.05658314289920116785 ),
 .UNSPECIFIED. ) ;
#59169 = ORIENTED_EDGE ( 'NONE', *, *, #27484, .F. ) ;
#59170 = CARTESIAN_POINT ( 'NONE',  ( -65.00000000000000000, 7.960204194457797252E-15, 15.70156211871650775 ) ) ;
#59171 = CARTESIAN_POINT ( 'NONE',  ( 311.9975424824652350, 20.00000000000003197, 401.6295345748407613 ) ) ;
#59172 = CARTESIAN_POINT ( 'NONE',  ( -49.44484229820456278, 14.28460989390478986, 69.66605993095367921 ) ) ;
#59173 = DIRECTION ( 'NONE',  ( 0.000000000000000000, 1.000000000000000000, 0.000000000000000000 ) ) ;
#59174 = CARTESIAN_POINT ( 'NONE',  ( -24.39004539972345498, 0.000000000000000000, -9.999999999999998224 ) ) ;
#59175 = CARTESIAN_POINT ( 'NONE',  ( -14.67600935270417928, 8.444777994442205227, 94.42750418574264870 ) ) ;
#59176 = ORIENTED_EDGE ( 'NONE', *, *, #52014, .T. ) ;
#59177 = DIRECTION ( 'NONE',  ( -0.000000000000000000, 1.000000000000000000, -0.000000000000000000 ) ) ;
#59178 = VERTEX_POINT ( 'NONE', #39428 ) ;
#59179 = AXIS2_PLACEMENT_3D ( 'NONE', #12714, #49990, #12362 ) ;
#59180 = ORIENTED_EDGE ( 'NONE', *, *, #54538, .T. ) ;
#59181 = CARTESIAN_POINT ( 'NONE',  ( 35.35682721709835619, 8.930334680552826754, 84.77865436726582971 ) ) ;
#59182 = CARTESIAN_POINT ( 'NONE',  ( -65.00200000000002376, -1.250000000000021760, 41.38025477438755928 ) ) ;
#59183 = CARTESIAN_POINT ( 'NONE',  ( 92.52113039222224700, 22.58921125235802663, -65.49921141967747928 ) ) ;
#59184 = ORIENTED_EDGE ( 'NONE', *, *, #51217, .F. ) ;
#59185 = AXIS2_PLACEMENT_3D ( 'NONE', #66042, #44565, #32280 ) ;
#59186 = CARTESIAN_POINT ( 'NONE',  ( -59.36813706141739999, 15.88103696331963377, -63.42195766872510632 ) ) ;
#59187 = CARTESIAN_POINT ( 'NONE',  ( 38.42384008295177722, 8.283891555743467805, -8.823408633594510775 ) ) ;
#59188 = CARTESIAN_POINT ( 'NONE',  ( 200.0000000000000000, 3.000000000000030198, -3.000000000000030198 ) ) ;
#59189 = AXIS2_PLACEMENT_3D ( 'NONE', #30753, #4697, #19852 ) ;
#59190 = CARTESIAN_POINT ( 'NONE',  ( -152.4930836497867688, 68.09400557494207362, -76.04119844780879589 ) ) ;
#59191 = CARTESIAN_POINT ( 'NONE',  ( 94.12988949694081953, 22.11811104795076233, 37.44777776544177073 ) ) ;
#59192 = B_SPLINE_CURVE_WITH_KNOTS ( 'NONE', 3,
 ( #4016, #14566, #41644, #20876, #4363, #41306, #69048, #58168, #31777, #37054, #21227, #68046, #46923, #42334, #47938, #31436, #32125, #30750, #63450, #10657 ),
 .UNSPECIFIED., .F., .F.,
 ( 4, 2, 2, 2, 2, 2, 2, 2, 2, 4 ),
 ( 0.01042392800800004925, 0.01174416055531339598, 0.01306439310262674097, 0.01372450937628338051, 0.01438462564994002005, 0.01570485819725330606, 0.01702509074456659555, 0.01834532329187988503, 0.01966555583919317451, 0.02098578838650646053 ),
 .UNSPECIFIED. ) ;
#59193 = EDGE_CURVE ( 'NONE', #64093, #51387, #43270, .T. ) ;
#59194 = VECTOR ( 'NONE', #24059, 1000.000000000000000 ) ;
#59195 = ORIENTED_EDGE ( 'NONE', *, *, #3493, .F. ) ;
#59197 = EDGE_CURVE ( 'NONE', #49097, #32365, #15660, .T. ) ;
#59196 = CARTESIAN_POINT ( 'NONE',  ( -48.70883077256304716, 14.10659259062419224, -46.72446105713036246 ) ) ;
#59198 = VECTOR ( 'NONE', #21929, 1000.000000000000000 ) ;
#59199 = DIRECTION ( 'NONE',  ( -0.000000000000000000, 1.000000000000000000, -0.000000000000000000 ) ) ;
#59200 = CARTESIAN_POINT ( 'NONE',  ( 10.13563904803030979, 7.391572367417532874, 42.46823125868149873 ) ) ;
#59201 = FACE_OUTER_BOUND ( 'NONE', #55762, .T. ) ;
#59202 = CARTESIAN_POINT ( 'NONE',  ( -85.89736547126425137, 26.29987632947471354, 89.59003780420152907 ) ) ;
#59204 = ORIENTED_EDGE ( 'NONE', *, *, #27059, .F. ) ;
#59203 = FACE_OUTER_BOUND ( 'NONE', #54062, .T. ) ;
#59205 = VERTEX_POINT ( 'NONE', #18322 ) ;
#59206 = ORIENTED_EDGE ( 'NONE', *, *, #20573, .F. ) ;
#59207 = CARTESIAN_POINT ( 'NONE',  ( -15.27748264047828997, 7.491388194171917370, -15.09317646226059217 ) ) ;
#59208 = CARTESIAN_POINT ( 'NONE',  ( -168.6270250298198903, 83.72687254638921672, 85.99976982588017904 ) ) ;
#59209 = LINE ( 'NONE', #53924, #41256 ) ;
#59210 = DIRECTION ( 'NONE',  ( 1.000000000000000000, 0.000000000000000000, 0.000000000000000000 ) ) ;
#59211 = ADVANCED_FACE ( 'NONE', ( #24654 ), #29921, .F. ) ;
#59212 = CARTESIAN_POINT ( 'NONE',  ( -33.85171821065139142, 11.02091558840051455, 71.67896086471448314 ) ) ;
#59213 = EDGE_CURVE ( 'NONE', #1085, #67017, #35194, .T. ) ;
#59214 = CARTESIAN_POINT ( 'NONE',  ( -14.84903512415884919, 8.461292896365062433, -13.43169028553783839 ) ) ;
#59215 = CARTESIAN_POINT ( 'NONE',  ( -78.66644367742109978, 22.32174330031319442, 3.573650549209446137 ) ) ;
#59216 = CARTESIAN_POINT ( 'NONE',  ( 22.52576749827964875, 6.809805260274348626, -19.50566305713887161 ) ) ;
#59217 = VERTEX_POINT ( 'NONE', #46089 ) ;
#59218 = CARTESIAN_POINT ( 'NONE',  ( 15.78827728214693416, -170.0000000000000000, 37.51470767270523510 ) ) ;
#59219 = ORIENTED_EDGE ( 'NONE', *, *, #34578, .T. ) ;
#59220 = ORIENTED_EDGE ( 'NONE', *, *, #2401, .F. ) ;
#59221 = CARTESIAN_POINT ( 'NONE',  ( 67.93154431625912082, 14.90489441944786897, -22.06196858991532039 ) ) ;
#59222 = B_SPLINE_CURVE_WITH_KNOTS ( 'NONE', 3,
 ( #38774, #43329, #11323, #48591, #59164, #5016, #69384, #42980, #10631, #16261, #59856, #58820, #54583, #65153, #60218, #64806, #38410, #59507, #785, #54223, #32792, #6046, #37363, #21534, #27505, #26824, #21205, #12036, #10982, #1134, #64452, #16947, #22585, #32104, #42652, #22238, #11676, #53878, #26483, #33147, #48251, #6408, #27858, #49301, #65504 ),
 .UNSPECIFIED., .F., .F.,
 ( 4, 2, 2, 2, 2, 2, 2, 2, 2, 2, 2, 2, 2, 1, 2, 2, 2, 2, 2, 2, 2, 2, 4 ),
 ( 0.02352719711393055219, 0.02499986300757014307, 0.02573619595438995239, 0.02647252890120975824, 0.02794519479484937341, 0.02941786068848898511, 0.03015419363530879443, 0.03089052658212860722, 0.03236319247576821545, 0.03309952542258803171, 0.03383585836940784103, 0.03530852426304745273, 0.03604485720986726205, 0.03678119015668707831, 0.03751752310350688763, 0.03825385605032669695, 0.03972652194396632253, 0.04119918783760595504, 0.04267185373124557368, 0.04340818667806538300, 0.04414451962488518538, 0.04561718551852481096, 0.04708985141216442960 ),
 .UNSPECIFIED. ) ;
#59223 = CARTESIAN_POINT ( 'NONE',  ( 0.7145311798163349604, -9.237604307034033013, 2.857026868940023748E-16 ) ) ;
#59224 = FACE_OUTER_BOUND ( 'NONE', #63198, .T. ) ;
#59225 = EDGE_CURVE ( 'NONE', #46532, #36510, #56784, .T. ) ;
#59226 = CARTESIAN_POINT ( 'NONE',  ( -155.5977325361977819, 70.88311713755697951, 15.76059677166101380 ) ) ;
#59228 = CARTESIAN_POINT ( 'NONE',  ( 188.4937788906148910, 86.43336847120863808, -42.52624257897028315 ) ) ;
#59227 = AXIS2_PLACEMENT_3D ( 'NONE', #51067, #45435, #13435 ) ;
#59229 = CARTESIAN_POINT ( 'NONE',  ( 21.75684465274325419, 6.764994602232769161, 42.08264190274187655 ) ) ;
#59230 = CARTESIAN_POINT ( 'NONE',  ( -148.5419150567446991, 64.67935585776004359, 84.45219532842064325 ) ) ;
#59231 = VERTEX_POINT ( 'NONE', #12582 ) ;
#59232 = ORIENTED_EDGE ( 'NONE', *, *, #3498, .T. ) ;
#59233 = ORIENTED_EDGE ( 'NONE', *, *, #3121, .T. ) ;
#59234 = FACE_OUTER_BOUND ( 'NONE', #12030, .T. ) ;
#59235 = CARTESIAN_POINT ( 'NONE',  ( 31.91383250562745388, 8.564461488297009595, -42.63145424299220565 ) ) ;
#59236 = EDGE_CURVE ( 'NONE', #55870, #35197, #1678, .T. ) ;
#59237 = CIRCLE ( 'NONE', #7607, 54.03875030502680943 ) ;
#59238 = DIRECTION ( 'NONE',  ( -0.3930250316539148359, -0.9195277725514544587, 0.000000000000000000 ) ) ;
#59239 = ADVANCED_FACE ( 'NONE', ( #23140 ), #1326, .F. ) ;
#59240 = CARTESIAN_POINT ( 'NONE',  ( -151.6716822472524200, 66.03661194063734285, -22.66300283947714789 ) ) ;
#59241 = EDGE_CURVE ( 'NONE', #47843, #31978, #49847, .T. ) ;
#59242 = VERTEX_POINT ( 'NONE', #984 ) ;
#59243 = EDGE_CURVE ( 'NONE', #39395, #9288, #14079, .T. ) ;
#59244 = VECTOR ( 'NONE', #15954, 1000.000000000000114 ) ;
#59245 = CARTESIAN_POINT ( 'NONE',  ( 0.000000000000000000, 0.000000000000000000, 43.58025477438756212 ) ) ;
#59246 = CARTESIAN_POINT ( 'NONE',  ( -152.5067928559255392, 66.76529500553621688, 58.17683507072492688 ) ) ;
#59247 = AXIS2_PLACEMENT_3D ( 'NONE', #33456, #1431, #45384 ) ;
#59248 = CARTESIAN_POINT ( 'NONE',  ( -1.862553927312063262, 7.582910205528080816, -47.49339086204825833 ) ) ;
#59249 = CARTESIAN_POINT ( 'NONE',  ( 103.9652201950894579, 26.08439499369982428, 14.37774731416467411 ) ) ;
#59250 = PLANE ( 'NONE',  #46609 ) ;
#59251 = DIRECTION ( 'NONE',  ( -0.000000000000000000, -0.000000000000000000, 1.000000000000000000 ) ) ;
#59252 = FACE_OUTER_BOUND ( 'NONE', #42539, .T. ) ;
#59253 = DIRECTION ( 'NONE',  ( -0.7227948638273978821, 0.6910626489868580968, 0.000000000000000000 ) ) ;
#59254 = CARTESIAN_POINT ( 'NONE',  ( 9.058156535714477542, 6.378495712187263855, -73.18255775613405945 ) ) ;
#59255 = VECTOR ( 'NONE', #23259, 1000.000000000000000 ) ;
#59256 = VERTEX_POINT ( 'NONE', #17498 ) ;
#59257 = DIRECTION ( 'NONE',  ( 0.08963930890342654279, 0.9959742939952397345, 0.000000000000000000 ) ) ;
#59258 = PRODUCT_CONTEXT ( 'NONE', #35896, 'mechanical' ) ;
#59259 = CARTESIAN_POINT ( 'NONE',  ( 132.9453095272139649, 42.04754713161462831, -36.02331093239565973 ) ) ;
#59260 = CARTESIAN_POINT ( 'NONE',  ( -129.4098618459772183, 48.85263848239745244, -49.04253402992481625 ) ) ;
#59261 = DIRECTION ( 'NONE',  ( -5.551115123125781716E-16, 0.000000000000000000, -1.000000000000000000 ) ) ;
#59262 = CARTESIAN_POINT ( 'NONE',  ( 55.77012379229940819, 12.13428856597100669, -68.11229150268280819 ) ) ;
#59263 = ORIENTED_EDGE ( 'NONE', *, *, #3280, .T. ) ;
#59264 = ORIENTED_EDGE ( 'NONE', *, *, #69308, .F. ) ;
#59265 = PLANE ( 'NONE',  #52714 ) ;
#59266 = CARTESIAN_POINT ( 'NONE',  ( 197.1975259970231775, 98.19639476549652102, 10.18970865138460624 ) ) ;
#59267 = VERTEX_POINT ( 'NONE', #34041 ) ;
#59268 = ORIENTED_EDGE ( 'NONE', *, *, #54602, .F. ) ;
#59269 = FACE_OUTER_BOUND ( 'NONE', #5499, .T. ) ;
#59270 = ORIENTED_EDGE ( 'NONE', *, *, #17637, .F. ) ;
#59271 = CARTESIAN_POINT ( 'NONE',  ( 133.8566784816069060, 42.60093787723654657, -62.86786152285933582 ) ) ;
#59272 = DIRECTION ( 'NONE',  ( -0.000000000000000000, -0.000000000000000000, 1.000000000000000000 ) ) ;
#59273 = CARTESIAN_POINT ( 'NONE',  ( 141.0517870458593848, 47.14452711594498879, 65.98772666960701372 ) ) ;
#59274 = CARTESIAN_POINT ( 'NONE',  ( 109.9975424824652634, 0.000000000000000000, 256.8908838121927261 ) ) ;
#59275 = CARTESIAN_POINT ( 'NONE',  ( -97.85576954355163082, 30.58918648956191788, 44.09425425760385053 ) ) ;
#59276 = CARTESIAN_POINT ( 'NONE',  ( 91.67571176799447130, 21.20498955963031307, -48.87521057456431350 ) ) ;
#59277 = CARTESIAN_POINT ( 'NONE',  ( 39.99999999999999289, 29.79383981485516841, -5.248138350681833405E-15 ) ) ;
#59278 = AXIS2_PLACEMENT_3D ( 'NONE', #60049, #34395, #28047 ) ;
#59279 = VERTEX_POINT ( 'NONE', #11875 ) ;
#59280 = ORIENTED_EDGE ( 'NONE', *, *, #59929, .T. ) ;
#59281 = AXIS2_PLACEMENT_3D ( 'NONE', #48509, #21453, #42226 ) ;
#59283 = EDGE_CURVE ( 'NONE', #32318, #28360, #22433, .T. ) ;
#59282 = CARTESIAN_POINT ( 'NONE',  ( 0.000000000000000000, 0.000000000000000000, 26.24939009510892518 ) ) ;
#59284 = DIRECTION ( 'NONE',  ( 0.000000000000000000, 0.000000000000000000, 1.000000000000000000 ) ) ;
#59285 = APPLICATION_CONTEXT ( 'automotive_design' ) ;
#59286 = CARTESIAN_POINT ( 'NONE',  ( 0.000000000000000000, 0.000000000000000000, -10.00000000000000000 ) ) ;
#59287 = VECTOR ( 'NONE', #57981, 1000.000000000000000 ) ;
#59288 = LINE ( 'NONE', #11437, #30919 ) ;
#59290 = ORIENTED_EDGE ( 'NONE', *, *, #20480, .F. ) ;
#59289 = CARTESIAN_POINT ( 'NONE',  ( -125.8938041572051389, 47.69968343338781125, 72.46449846362081360 ) ) ;
#59291 = CARTESIAN_POINT ( 'NONE',  ( 55.99998955208977236, 12.18058389017405041, 13.13159707503299956 ) ) ;
#59292 = AXIS2_PLACEMENT_3D ( 'NONE', #22017, #11444, #27984 ) ;
#59293 = ORIENTED_EDGE ( 'NONE', *, *, #4673, .F. ) ;
#59294 = CARTESIAN_POINT ( 'NONE',  ( -142.2626321327577443, 58.26997216742665131, 63.10616936434193747 ) ) ;
#59295 = CARTESIAN_POINT ( 'NONE',  ( 26.69682282325711853, 59.27986298182223379, 3.061616997868437868E-16 ) ) ;
#59296 = DIRECTION ( 'NONE',  ( 0.000000000000000000, 0.000000000000000000, 1.000000000000000000 ) ) ;
#59297 = ADVANCED_FACE ( 'NONE', ( #7664 ), #60105, .F. ) ;
#59298 = EDGE_CURVE ( 'NONE', #29569, #5706, #18156, .T. ) ;
#59299 = EDGE_CURVE ( 'NONE', #6300, #1969, #48072, .T. ) ;
#59300 = CARTESIAN_POINT ( 'NONE',  ( 136.1081004736420255, 42.80058051492066085, -23.83655509551084961 ) ) ;
#59301 = AXIS2_PLACEMENT_3D ( 'NONE', #66702, #40634, #24485 ) ;
#59302 = CARTESIAN_POINT ( 'NONE',  ( -102.2801239173131052, 32.78103895658057354, -50.01457726497594081 ) ) ;
#59303 = CARTESIAN_POINT ( 'NONE',  ( 197.8572563162090603, 97.41072138832258531, 12.95325563156990789 ) ) ;
#59304 = CARTESIAN_POINT ( 'NONE',  ( -96.00016893459647349, 29.70347032303887858, 15.28240503082096069 ) ) ;
#59305 = CARTESIAN_POINT ( 'NONE',  ( -6.000000000000000000, 23.07878402833891229, -5.000000000000000000 ) ) ;
#59306 = ORIENTED_EDGE ( 'NONE', *, *, #44830, .T. ) ;
#59307 = EDGE_LOOP ( 'NONE', ( #30316, #28217, #52647, #24562 ) ) ;
#59308 = EDGE_CURVE ( 'NONE', #63135, #23015, #4685, .T. ) ;
#59309 = CARTESIAN_POINT ( 'NONE',  ( 188.2950202724320548, 86.21411212788221690, -72.65244717427873411 ) ) ;
#59310 = CARTESIAN_POINT ( 'NONE',  ( 110.2429982417149574, 29.99119854320843714, 44.61121420573733332 ) ) ;
#59311 = CARTESIAN_POINT ( 'NONE',  ( 280.0000000000000000, -22.00000000000000000, 4.999999999999990230 ) ) ;
#59312 = DIRECTION ( 'NONE',  ( 0.000000000000000000, 0.000000000000000000, -1.000000000000000000 ) ) ;
#59313 = ADVANCED_FACE ( 'NONE', ( #54387 ), #37182, .T. ) ;
#59314 = CARTESIAN_POINT ( 'NONE',  ( 109.7732660198864494, 29.77277639096406148, -62.76698815611734972 ) ) ;
#59315 = CARTESIAN_POINT ( 'NONE',  ( 82.13067365723604496, 17.93447087949267527, 31.19152029446487617 ) ) ;
#59316 = CARTESIAN_POINT ( 'NONE',  ( 6.837601902335299187, 41.16505653441733870, 13.79046340968177553 ) ) ;
#59317 = CARTESIAN_POINT ( 'NONE',  ( -119.9771613955296772, 43.90337778233485722, 33.50398703533743117 ) ) ;
#59318 = DIRECTION ( 'NONE',  ( -0.000000000000000000, -0.000000000000000000, 1.000000000000000000 ) ) ;
#59319 = B_SPLINE_CURVE_WITH_KNOTS ( 'NONE', 3,
 ( #46723, #22062, #22410, #38236, #27678, #16443, #65684, #26988, #5534, #43850, #26652, #54400, #27328, #21364, #48087, #37897, #250, #59677, #64629, #37543, #6583, #6223, #32963, #49120, #49471, #11849, #58993, #33329, #48768, #44197, #53712, #17471, #959, #43157, #59343, #65327, #17113, #11154, #38590, #16087, #32619, #5197, #1306, #10462, #64982, #60032, #69546, #31934, #54047, #48417, #53361, #605, #42811, #43504, #16777, #64279, #10813, #32281 ),
 .UNSPECIFIED., .F., .F.,
 ( 4, 2, 2, 2, 2, 2, 2, 2, 2, 2, 2, 2, 2, 2, 2, 2, 2, 2, 2, 2, 2, 2, 2, 2, 2, 2, 2, 2, 4 ),
 ( 0.000000000000000000, 0.002051743101817396931, 0.003077614652726094312, 0.004103486203634792127, 0.005129357754543489509, 0.006155229305452186890, 0.007181100856360885139, 0.008206972407269582520, 0.009232843958178280769, 0.01025871550908697902, 0.01128458705999567727, 0.01231045861090437551, 0.01436220171272178416, 0.01538807326363049455, 0.01641394481453920320, 0.01743981636544791186, 0.01846568791635662052, 0.01949155946726532918, 0.02051743101817404130, 0.02256917411999149331, 0.02359504567090022278, 0.02462091722180894879, 0.02564678877271767479, 0.02667266032362640427, 0.02769853187453513027, 0.02872440342544385627, 0.02975027497635258922, 0.03077614652726131522, 0.03282788962907880193 ),
 .UNSPECIFIED. ) ;
#59320 = VERTEX_POINT ( 'NONE', #42120 ) ;
#59321 = CARTESIAN_POINT ( 'NONE',  ( -24.95029760921699946, 9.631514785009935409, 7.102706412057313123 ) ) ;
#59322 = ORIENTED_EDGE ( 'NONE', *, *, #50831, .F. ) ;
#59323 = CARTESIAN_POINT ( 'NONE',  ( -14.66033866466834645, 7.432913330382390882, -46.01550798236979034 ) ) ;
#59324 = LINE ( 'NONE', #11137, #20597 ) ;
#59325 = CARTESIAN_POINT ( 'NONE',  ( 152.6560521232695464, 54.00248515670894278, -22.53561542425598319 ) ) ;
#59326 = CARTESIAN_POINT ( 'NONE',  ( 36.98541457540712685, 9.120571655722418569, 17.68600818565902699 ) ) ;
#59327 = CARTESIAN_POINT ( 'NONE',  ( -97.48179118242302366, 31.52606332398821820, -75.14452323989597460 ) ) ;
#59328 = CARTESIAN_POINT ( 'NONE',  ( 112.1664364330408432, 30.89547116421898565, -89.85190045744435849 ) ) ;
#59329 = EDGE_CURVE ( 'NONE', #4465, #16163, #15392, .T. ) ;
#59330 = EDGE_CURVE ( 'NONE', #67718, #31575, #24015, .T. ) ;
#59331 = ORIENTED_EDGE ( 'NONE', *, *, #33196, .F. ) ;
#59332 = CARTESIAN_POINT ( 'NONE',  ( 212.2009967487813356, 117.2366405038844022, 90.35305982578324802 ) ) ;
#59333 = FACE_OUTER_BOUND ( 'NONE', #53352, .T. ) ;
#59334 = VERTEX_POINT ( 'NONE', #44895 ) ;
#59335 = CARTESIAN_POINT ( 'NONE',  ( 56.94505604581135572, 12.37336791557970983, 59.74625065850809591 ) ) ;
#59336 = CARTESIAN_POINT ( 'NONE',  ( 15.78827728214693771, 7.507518794609575608, -62.36349468914946925 ) ) ;
#59338 = ADVANCED_FACE ( 'NONE', ( #66378 ), #65312, .F. ) ;
#59337 = CARTESIAN_POINT ( 'NONE',  ( -29.02794087136070189, 9.207646203414336483, 17.99040909154227919 ) ) ;
#59339 = DIRECTION ( 'NONE',  ( -0.000000000000000000, 1.000000000000000000, -0.000000000000000000 ) ) ;
#59340 = CARTESIAN_POINT ( 'NONE',  ( -0.3734056954813049778, 6.520221844775925923, 38.59366696979675027 ) ) ;
#59341 = CARTESIAN_POINT ( 'NONE',  ( -102.2801239173131052, 32.78103895658057354, -61.85912785543958847 ) ) ;
#59342 = VECTOR ( 'NONE', #57644, 1000.000000000000000 ) ;
#59343 = CARTESIAN_POINT ( 'NONE',  ( 84.10229504626889252, 19.63355683306561872, 83.83215316015663632 ) ) ;
#59344 = AXIS2_PLACEMENT_3D ( 'NONE', #13357, #56252, #45707 ) ;
#59345 = ORIENTED_EDGE ( 'NONE', *, *, #68084, .F. ) ;
#59346 = DIRECTION ( 'NONE',  ( 1.000000000000000000, 9.950807539071918675E-15, 9.950807539071956540E-15 ) ) ;
#59347 = CARTESIAN_POINT ( 'NONE',  ( -20.55634918610396866, 31.11269837220809009, 2.000000000000001776 ) ) ;
#59348 = CARTESIAN_POINT ( 'NONE',  ( -129.4098618459771899, 48.85263848239743822, 4.646567151002527929 ) ) ;
#59349 = CARTESIAN_POINT ( 'NONE',  ( -166.0031475600389115, 80.98114714564766814, -39.83147878504032491 ) ) ;
#59350 = ITEM_DEFINED_TRANSFORMATION ( 'NONE', 'NONE', #16434,  #66832 ) ;
#59351 = DIRECTION ( 'NONE',  ( -0.000000000000000000, -0.000000000000000000, -1.000000000000000000 ) ) ;
#59352 = EDGE_LOOP ( 'NONE', ( #31017, #36870, #22844, #20019 ) ) ;
#59353 = CARTESIAN_POINT ( 'NONE',  ( -31.11269837220804035, 15.55634918610408945, 2.000000000000001776 ) ) ;
#59354 = DIRECTION ( 'NONE',  ( -0.000000000000000000, 1.000000000000000000, -0.000000000000000000 ) ) ;
#59355 = CARTESIAN_POINT ( 'NONE',  ( 199.7291770695759965, 101.4092159658446803, -11.35800590186485515 ) ) ;
#59356 = CARTESIAN_POINT ( 'NONE',  ( -156.2685900000522849, 70.13315996971763866, 88.64677459970704376 ) ) ;
#59357 = CARTESIAN_POINT ( 'NONE',  ( 133.8566784816069628, 41.42467568809806977, 44.51034083899536142 ) ) ;
#59358 = VERTEX_POINT ( 'NONE', #1637 ) ;
#59359 = CARTESIAN_POINT ( 'NONE',  ( 0.000000000000000000, 0.000000000000000000, 5.000000000000000000 ) ) ;
#59360 = CARTESIAN_POINT ( 'NONE',  ( 83.59652366361572717, 19.46709838196857234, 17.23118984585019575 ) ) ;
#59361 = CARTESIAN_POINT ( 'NONE',  ( 164.9700808964341547, 65.04346068891115351, 10.35365659087820056 ) ) ;
#59362 = CARTESIAN_POINT ( 'NONE',  ( 0.000000000000000000, 6.000000000000000000, -3.000000000000030198 ) ) ;
#59363 = ORIENTED_EDGE ( 'NONE', *, *, #36825, .T. ) ;
#59364 = CARTESIAN_POINT ( 'NONE',  ( 311.9975424824652350, 20.00000000000003197, 256.6193948016162381 ) ) ;
#59365 = VERTEX_POINT ( 'NONE', #45237 ) ;
#59366 =( BOUNDED_CURVE ( )  B_SPLINE_CURVE ( 3, ( #12283, #23193, #11930, #33402 ),
 .UNSPECIFIED., .F., .F. ) 
 B_SPLINE_CURVE_WITH_KNOTS ( ( 4, 4 ),
 ( 2.746264796135519770, 3.776976132411494103 ),
 .UNSPECIFIED. ) 
 CURVE ( )  GEOMETRIC_REPRESENTATION_ITEM ( )  RATIONAL_B_SPLINE_CURVE ( ( 1.000000000000000000, 0.9134116588687805072, 0.9134116588687805072, 1.000000000000000000 ) ) 
 REPRESENTATION_ITEM ( '' )  );
#59368 = EDGE_CURVE ( 'NONE', #23953, #68299, #58378, .T. ) ;
#59367 = CARTESIAN_POINT ( 'NONE',  ( -118.9981077023450666, 42.11809457178108573, -93.14365615247058372 ) ) ;
#59369 = B_SPLINE_CURVE_WITH_KNOTS ( 'NONE', 3,
 ( #61668, #39524, #3283, #18413, #12798, #35288, #34947, #45840, #56390, #2248, #14179, #39867, #18765, #30357, #24741, #40908, #67650, #19446, #23695, #66618, #45486, #29660, #56744, #61325, #13486, #51121, #57092, #2934, #8562, #7867, #30013, #62364, #24398, #13150, #8905, #51472, #51809, #67316, #19101, #18074, #40555, #60973, #56049, #3617, #66282, #62008, #50428, #34256 ),
 .UNSPECIFIED., .F., .F.,
 ( 4, 2, 2, 2, 2, 2, 2, 2, 2, 2, 2, 2, 2, 2, 2, 2, 2, 2, 2, 2, 2, 2, 2, 4 ),
 ( 1.387778780781445676E-17, 0.003619254076116648709, 0.004524067595145762205, 0.005428881114174875268, 0.007238508152233127414, 0.008143321671262276906, 0.009048135190291429000, 0.01085776222834966380, 0.01176257574737874824, 0.01266738926640783268, 0.01357220278543691885, 0.01447701630446600329, 0.01538182982349508947, 0.01628664334252417217, 0.01719145686155325661, 0.01809627038058234452, 0.01900108389961142549, 0.01990589741864050993, 0.02171552445669866147, 0.02262033797572774937, 0.02352515149475683728, 0.02533477853281501657, 0.02714440557087319586, 0.02895403260893137515 ),
 .UNSPECIFIED. ) ;
#59370 = CARTESIAN_POINT ( 'NONE',  ( -15.55634918610411077, -46.66904755831208718, 2.000000000000001776 ) ) ;
#59372 = EDGE_LOOP ( 'NONE', ( #29525, #36225 ) ) ;
#59371 = LINE ( 'NONE', #21737, #49978 ) ;
#59373 = CARTESIAN_POINT ( 'NONE',  ( 160.4963793545269652, 60.04225845346908130, 30.03251751463668029 ) ) ;
#59374 = FACE_OUTER_BOUND ( 'NONE', #44173, .T. ) ;
#59375 = CYLINDRICAL_SURFACE ( 'NONE', #38428, 7.500000000000020428 ) ;
#59376 = ORIENTED_EDGE ( 'NONE', *, *, #32851, .F. ) ;
#59377 = CARTESIAN_POINT ( 'NONE',  ( -149.5074843970971017, 65.50121172469320641, -88.50193171241930656 ) ) ;
#59378 = EDGE_CURVE ( 'NONE', #54998, #56202, #17823, .T. ) ;
#59379 = CARTESIAN_POINT ( 'NONE',  ( -37.38781680082738035, 10.64362327909142358, -20.56642074805881748 ) ) ;
#59380 = CARTESIAN_POINT ( 'NONE',  ( -180.6158171975814923, 97.47361786002629458, 37.99731989376397223 ) ) ;
#59381 = CARTESIAN_POINT ( 'NONE',  ( -38.93922791710217979, 10.94334660650242341, -69.90365907529749734 ) ) ;
#59382 = EDGE_CURVE ( 'NONE', #64323, #11967, #55438, .T. ) ;
#59383 = VERTEX_POINT ( 'NONE', #55802 ) ;
#59384 = VECTOR ( 'NONE', #28311, 1000.000000000000000 ) ;
#59385 = EDGE_CURVE ( 'NONE', #4870, #67714, #2342, .T. ) ;
#59386 = VERTEX_POINT ( 'NONE', #61423 ) ;
#59387 = VERTEX_POINT ( 'NONE', #13245 ) ;
#59388 = CYLINDRICAL_SURFACE ( 'NONE', #47450, 246.3582898394606957 ) ;
#59389 = EDGE_CURVE ( 'NONE', #46344, #50609, #7959, .T. ) ;
#59390 = AXIS2_PLACEMENT_3D ( 'NONE', #50935, #34069, #17528 ) ;
#59391 = DIRECTION ( 'NONE',  ( -0.000000000000000000, 1.000000000000000000, -0.000000000000000000 ) ) ;
#59392 = DIRECTION ( 'NONE',  ( -0.000000000000000000, -0.000000000000000000, 1.000000000000000000 ) ) ;
#59393 = CARTESIAN_POINT ( 'NONE',  ( -7.825402957745083654, 7.899365992529244984, -8.573520141480125645 ) ) ;
#59394 = CARTESIAN_POINT ( 'NONE',  ( 66.21839516550542726, 13.43774118063817546, 84.18802111937300481 ) ) ;
#59395 = PLANE ( 'NONE',  #4463 ) ;
#59396 = DIRECTION ( 'NONE',  ( -0.000000000000000000, -1.000000000000000000, -0.000000000000000000 ) ) ;
#59397 = DIRECTION ( 'NONE',  ( 1.000000000000000000, 0.000000000000000000, -0.000000000000000000 ) ) ;
#59398 = ORIENTED_EDGE ( 'NONE', *, *, #62580, .F. ) ;
#59399 = DIRECTION ( 'NONE',  ( -0.000000000000000000, -0.000000000000000000, 1.000000000000000000 ) ) ;
#59400 = ORIENTED_EDGE ( 'NONE', *, *, #41240, .T. ) ;
#59401 = PLANE ( 'NONE',  #41941 ) ;
#59402 = CARTESIAN_POINT ( 'NONE',  ( 205.1049299651095623, 106.9023875785546096, -63.17048162308526571 ) ) ;
#59403 = LINE ( 'NONE', #11920, #37755 ) ;
#59404 = CARTESIAN_POINT ( 'NONE',  ( 122.2516123306975402, 190.0000000000000000, -91.28179539054376335 ) ) ;
#59405 = DIRECTION ( 'NONE',  ( 0.000000000000000000, 0.000000000000000000, -1.000000000000000000 ) ) ;
#59406 = CARTESIAN_POINT ( 'NONE',  ( -78.66644367742111399, -170.0000000000000000, -42.61545063171789849 ) ) ;
#59407 = CARTESIAN_POINT ( 'NONE',  ( 199.2433808803260717, 99.15270001483533235, 85.23814155805331438 ) ) ;
#59408 = CARTESIAN_POINT ( 'NONE',  ( 150.7926588734435711, 52.63999027731880886, -40.19948293293975183 ) ) ;
#59409 = CARTESIAN_POINT ( 'NONE',  ( 163.1313205310724754, 63.49733392291055623, -65.54288040409811344 ) ) ;
#59410 = ORIENTED_EDGE ( 'NONE', *, *, #64243, .T. ) ;
#59411 = CARTESIAN_POINT ( 'NONE',  ( -149.5074843970971301, 64.17983161892347255, -88.50193171241930656 ) ) ;
#59412 = DIRECTION ( 'NONE',  ( -0.000000000000000000, -0.000000000000000000, -1.000000000000000000 ) ) ;
#59413 = EDGE_LOOP ( 'NONE', ( #68196, #50294, #31845, #24164 ) ) ;
#59414 = EDGE_CURVE ( 'NONE', #28608, #37838, #20701, .T. ) ;
#59415 = ORIENTED_EDGE ( 'NONE', *, *, #61711, .T. ) ;
#59416 = CARTESIAN_POINT ( 'NONE',  ( -79.61931371420118353, 22.68640080971622197, 45.37248484975646079 ) ) ;
#59417 = CARTESIAN_POINT ( 'NONE',  ( -24.18270484670773968, 9.527492911955594224, -67.70162071242002355 ) ) ;
#59418 = CARTESIAN_POINT ( 'NONE',  ( 39.40195752203892710, 9.424259417798134919, 29.91383430596324899 ) ) ;
#59419 = CARTESIAN_POINT ( 'NONE',  ( -24.18258876560172865, 8.512344710720679331, 62.60268071088248831 ) ) ;
#59420 = CARTESIAN_POINT ( 'NONE',  ( 26.11269837220812562, 36.11269837220800838, 2.000000000000001776 ) ) ;
#59421 = ORIENTED_EDGE ( 'NONE', *, *, #61939, .F. ) ;
#59422 = ORIENTED_EDGE ( 'NONE', *, *, #36445, .F. ) ;
#59423 = AXIS2_PLACEMENT_3D ( 'NONE', #56733, #13476, #65284 ) ;
#59424 = LINE ( 'NONE', #68610, #23323 ) ;
#59425 = ORIENTED_EDGE ( 'NONE', *, *, #9221, .T. ) ;
#59426 = CARTESIAN_POINT ( 'NONE',  ( 39.40195752203892710, 9.424259417798131366, -23.77526687496409608 ) ) ;
#59427 = CARTESIAN_POINT ( 'NONE',  ( -146.1140637052938871, 62.65471088530799904, 31.51667258806176974 ) ) ;
#59428 = CARTESIAN_POINT ( 'NONE',  ( 56.19513604272052731, 11.19349063094195706, 67.28664494194475765 ) ) ;
#59429 = CARTESIAN_POINT ( 'NONE',  ( 0.000000000000000000, 0.000000000000000000, 41.38025477438755928 ) ) ;
#59430 = CARTESIAN_POINT ( 'NONE',  ( -29.13697796587925026, 10.24294185249329203, -89.36513106409366003 ) ) ;
#59431 = DIRECTION ( 'NONE',  ( 1.000000000000000000, 0.000000000000000000, 0.000000000000000000 ) ) ;
#59432 = CARTESIAN_POINT ( 'NONE',  ( 313.9975424824652350, 296.0000000000000000, 529.9060149868646477 ) ) ;
#59433 = ORIENTED_EDGE ( 'NONE', *, *, #63454, .F. ) ;
#59434 = VECTOR ( 'NONE', #13869, 1000.000000000000000 ) ;
#59435 = EDGE_LOOP ( 'NONE', ( #50932, #58922, #57707, #33656 ) ) ;
#59436 = CARTESIAN_POINT ( 'NONE',  ( -24.87827947785777383, -3.494138152041991408, 3.061616997868437868E-16 ) ) ;
#59437 = LINE ( 'NONE', #27430, #21595 ) ;
#59438 = CYLINDRICAL_SURFACE ( 'NONE', #43136, 5.000000000000060396 ) ;
#59439 = LINE ( 'NONE', #5630, #34386 ) ;
#59440 = CARTESIAN_POINT ( 'NONE',  ( 66.73594759725092729, 13.56641407806656296, 43.82974788099483021 ) ) ;
#59441 = EDGE_CURVE ( 'NONE', #61067, #14016, #10669, .T. ) ;
#59442 = EDGE_LOOP ( 'NONE', ( #48661, #53472 ) ) ;
#59443 = EDGE_CURVE ( 'NONE', #18390, #37473, #3375, .T. ) ;
#59444 = CYLINDRICAL_SURFACE ( 'NONE', #14783, 7.500000000000020428 ) ;
#59445 = ADVANCED_FACE ( 'NONE', ( #24146 ), #24829, .F. ) ;
#59446 = ORIENTED_EDGE ( 'NONE', *, *, #58843, .F. ) ;
#59447 = DIRECTION ( 'NONE',  ( 0.000000000000000000, 0.000000000000000000, 1.000000000000000000 ) ) ;
#59448 = ORIENTED_EDGE ( 'NONE', *, *, #35514, .T. ) ;
#59449 = ADVANCED_FACE ( 'NONE', ( #57188 ), #55646, .T. ) ;
#59450 = VERTEX_POINT ( 'NONE', #19900 ) ;
#59451 = CARTESIAN_POINT ( 'NONE',  ( 4.681481898397010788, -6.534749472788160318, -5.187229768985335276E-15 ) ) ;
#59452 = VECTOR ( 'NONE', #61897, 1000.000000000000114 ) ;
#59453 = CARTESIAN_POINT ( 'NONE',  ( 87.59061758233885087, 19.75077892934020696, 17.82126877942726040 ) ) ;
#59454 = DIRECTION ( 'NONE',  ( 1.000000000000000000, 0.000000000000000000, 0.000000000000000000 ) ) ;
#59455 = ORIENTED_EDGE ( 'NONE', *, *, #55857, .T. ) ;
#59456 = B_SPLINE_CURVE_WITH_KNOTS ( 'NONE', 3,
 ( #59341, #49119, #12209, #53710, #11153, #32618, #54045, #5870, #16776, #38235, #59676, #27677, #22409, #65326, #29427, #24514, #50877, #66734, #34015, #7639, #44909, #61769, #12556, #67762, #40324, #67415, #2697, #8327, #40666, #30131, #24160, #55456, #3389, #13595, #29090, #12917, #34372, #13258 ),
 .UNSPECIFIED., .F., .F.,
 ( 4, 2, 2, 2, 2, 2, 2, 2, 2, 2, 2, 2, 2, 2, 2, 2, 2, 2, 4 ),
 ( 0.000000000000000000, 0.001559859933532193633, 0.003119719867064387267, 0.004679579800596567023, 0.006239439734128746778, 0.007799299667660926534, 0.008579229634427035928, 0.009359159601193144454, 0.01091901953472536324, 0.01169894950149148738, 0.01247887946825761325, 0.01403873940178985980, 0.01559859933532211154, 0.01715845926885435982, 0.01871831920238660810, 0.02027817913591885637, 0.02183803906945110812, 0.02339789900298335640, 0.02495775893651560814 ),
 .UNSPECIFIED. ) ;
#59457 = DIRECTION ( 'NONE',  ( -0.8160245890732938934, -0.5780171883497599028, 0.000000000000000000 ) ) ;
#59458 = LINE ( 'NONE', #54526, #24488 ) ;
#59459 = CARTESIAN_POINT ( 'NONE',  ( 36.85262215550070408, 53.56030941157735015, 43.58025477438756923 ) ) ;
#59460 = CARTESIAN_POINT ( 'NONE',  ( 66.73467315386237431, 14.60276727483218373, 43.84403630633526916 ) ) ;
#59461 = DIRECTION ( 'NONE',  ( -0.000000000000000000, -0.000000000000000000, -1.000000000000000000 ) ) ;
#59462 = CARTESIAN_POINT ( 'NONE',  ( 62.82395629628391731, 22.24309010993259861, 34.48241795236666007 ) ) ;
#59463 = EDGE_CURVE ( 'NONE', #18937, #16807, #26428, .T. ) ;
#59464 = CARTESIAN_POINT ( 'NONE',  ( 0.000000000000000000, 35.00000000000000000, -22.00000000000000355 ) ) ;
#59465 = EDGE_LOOP ( 'NONE', ( #38356, #56584, #10858, #46875 ) ) ;
#59466 = CARTESIAN_POINT ( 'NONE',  ( 137.3861614007144851, 44.78548268714477132, -63.74609645935769464 ) ) ;
#59468 = EDGE_CURVE ( 'NONE', #61512, #25612, #36074, .T. ) ;
#59467 = CARTESIAN_POINT ( 'NONE',  ( 0.000000000000000000, 0.000000000000000000, 170.0000000000000000 ) ) ;
#59469 = ORIENTED_EDGE ( 'NONE', *, *, #34884, .F. ) ;
#59470 = FACE_BOUND ( 'NONE', #10016, .T. ) ;
#59471 = CARTESIAN_POINT ( 'NONE',  ( -4.513903087372260536, 6.697902023160579255, -76.49641857693266900 ) ) ;
#59472 = CARTESIAN_POINT ( 'NONE',  ( -148.6426892915312692, 64.76241938621078020, -7.968279941028272972 ) ) ;
#59473 = DIRECTION ( 'NONE',  ( 0.000000000000000000, 0.000000000000000000, -1.000000000000000000 ) ) ;
#59474 = CARTESIAN_POINT ( 'NONE',  ( -83.69370847062540975, 25.38703975185374162, 5.502694545838179963 ) ) ;
#59475 = DIRECTION ( 'NONE',  ( 1.000000000000000000, 0.000000000000000000, 0.000000000000000000 ) ) ;
#59476 = CARTESIAN_POINT ( 'NONE',  ( 114.9998692468128780, 21.99997028336874294, -0.3318949079940916591 ) ) ;
#59477 = CARTESIAN_POINT ( 'NONE',  ( -77.81700272789856854, 21.99959588779042718, -88.84078370873776009 ) ) ;
#59478 = CARTESIAN_POINT ( 'NONE',  ( 66.29961816943395547, 13.45804302849873579, 3.708301206476156686 ) ) ;
#59479 = CARTESIAN_POINT ( 'NONE',  ( 112.5721302457195776, 29.97407549554797868, 17.41144223022721960 ) ) ;
#59480 = CARTESIAN_POINT ( 'NONE',  ( 88.98064924903393091, 21.30386569031178468, -9.351095346740329717 ) ) ;
#59481 = ORIENTED_EDGE ( 'NONE', *, *, #24886, .F. ) ;
#59482 = CARTESIAN_POINT ( 'NONE',  ( -38.69449158134467837, 11.92067517118076658, 8.909342758798803885 ) ) ;
#59483 = VERTEX_POINT ( 'NONE', #53866 ) ;
#59484 = PLANE ( 'NONE',  #44132 ) ;
#59485 = AXIS2_PLACEMENT_3D ( 'NONE', #56028, #61645, #1512 ) ;
#59486 = DIRECTION ( 'NONE',  ( 0.000000000000000000, -1.000000000000000000, 0.000000000000000000 ) ) ;
#59487 = CARTESIAN_POINT ( 'NONE',  ( 104.0290905220488469, 27.20720373712009987, 94.99999999999866418 ) ) ;
#59488 = CARTESIAN_POINT ( 'NONE',  ( 15.55634918610409656, 36.11269837220803680, 0.000000000000000000 ) ) ;
#59489 = CARTESIAN_POINT ( 'NONE',  ( 69.74037587279241279, 14.33355757956374887, -13.01822706347090453 ) ) ;
#59491 = CARTESIAN_POINT ( 'NONE',  ( -24.18158274621863768, 9.527343002918316373, -44.77222497198581408 ) ) ;
#59490 = AXIS2_PLACEMENT_3D ( 'NONE', #2200, #24697, #56343 ) ;
#59492 = CARTESIAN_POINT ( 'NONE',  ( -51.77779688167512262, 14.86590802019196644, -76.31248613329042030 ) ) ;
#59493 = LINE ( 'NONE', #27142, #56666 ) ;
#59494 = CARTESIAN_POINT ( 'NONE',  ( -122.8011284400168250, 45.68452922414294193, -22.41731093363175020 ) ) ;
#59495 = ORIENTED_EDGE ( 'NONE', *, *, #51181, .F. ) ;
#59496 = VERTEX_POINT ( 'NONE', #27493 ) ;
#59497 = CARTESIAN_POINT ( 'NONE',  ( 31.91383250562745388, 8.564461488296997160, 64.74674811886252712 ) ) ;
#59498 = DIRECTION ( 'NONE',  ( -0.5128992774058949156, -0.8584487936018728726, 0.000000000000000000 ) ) ;
#59499 = DIRECTION ( 'NONE',  ( -0.6910626489868580968, -0.7227948638273978821, 0.000000000000000000 ) ) ;
#59500 = AXIS2_PLACEMENT_3D ( 'NONE', #55686, #50064, #18063 ) ;
#59501 = CARTESIAN_POINT ( 'NONE',  ( 63.42451435127777160, 13.80104019830836215, -89.40979201309713176 ) ) ;
#59502 = ORIENTED_EDGE ( 'NONE', *, *, #23702, .F. ) ;
#59503 = CARTESIAN_POINT ( 'NONE',  ( 88.28889510440058075, 21.05995314109331318, 17.68549489745171854 ) ) ;
#59504 = CARTESIAN_POINT ( 'NONE',  ( 184.0001683447903531, 83.06228184427189376, -23.80381492175980895 ) ) ;
#59505 = CARTESIAN_POINT ( 'NONE',  ( 211.1046732743772907, 117.3965485104337318, 13.77185182296995158 ) ) ;
#59506 = CARTESIAN_POINT ( 'NONE',  ( -80.76613269273198625, 24.21305865109442124, -89.09189068382836751 ) ) ;
#59507 = CARTESIAN_POINT ( 'NONE',  ( 46.41758729921146909, 9.425975226414264441, -18.93824580312872996 ) ) ;
#59508 = CARTESIAN_POINT ( 'NONE',  ( 14.66690460840479027, 20.39656099473415551, 3.061616997868437868E-16 ) ) ;
#59509 = CARTESIAN_POINT ( 'NONE',  ( 105.1608908971991809, 21.96390383200032304, -1.300086469598745520 ) ) ;
#59510 = PLANE ( 'NONE',  #46757 ) ;
#59511 = ORIENTED_EDGE ( 'NONE', *, *, #28907, .F. ) ;
#59512 = CARTESIAN_POINT ( 'NONE',  ( 132.9453095272139649, 42.04754713161464252, 17.66579024853170665 ) ) ;
#59513 = CARTESIAN_POINT ( 'NONE',  ( 93.87111289824407834, 23.09598275302507275, -41.30595271919344214 ) ) ;
#59514 = CARTESIAN_POINT ( 'NONE',  ( -47.55316895016326839, 13.83165595246918400, 65.16454658915249354 ) ) ;
#59515 = LINE ( 'NONE', #32457, #51192 ) ;
#59516 = DIRECTION ( 'NONE',  ( 0.000000000000000000, 0.000000000000000000, 1.000000000000000000 ) ) ;
#59517 = VECTOR ( 'NONE', #54289, 1000.000000000000000 ) ;
#59518 = DIRECTION ( 'NONE',  ( 0.000000000000000000, 1.000000000000000000, -0.000000000000000000 ) ) ;
#59519 = EDGE_LOOP ( 'NONE', ( #67772, #52029, #11366, #44410 ) ) ;
#59520 = CARTESIAN_POINT ( 'NONE',  ( 0.000000000000000000, 0.000000000000000000, 41.38025477438755928 ) ) ;
#59521 = CARTESIAN_POINT ( 'NONE',  ( 447.3372781065086201, 177.8591479523844612, 78.55029585798806124 ) ) ;
#59522 = EDGE_CURVE ( 'NONE', #29948, #8034, #45875, .T. ) ;
#59523 = VERTEX_POINT ( 'NONE', #49284 ) ;
#59524 = ORIENTED_EDGE ( 'NONE', *, *, #23572, .F. ) ;
#59525 = PLANE ( 'NONE',  #56668 ) ;
#59526 = CARTESIAN_POINT ( 'NONE',  ( -1.666933348992581942, 64.97862212458815634, 40.00000000000003553 ) ) ;
#59527 = EDGE_CURVE ( 'NONE', #4383, #2042, #37701, .T. ) ;
#59528 = CARTESIAN_POINT ( 'NONE',  ( 4.606779575613957789, 24.69646479044443765, 0.000000000000000000 ) ) ;
#59529 = ORIENTED_EDGE ( 'NONE', *, *, #47087, .T. ) ;
#59530 = CARTESIAN_POINT ( 'NONE',  ( -62.53989795537027874, 16.81768094534200841, -69.05562491124992164 ) ) ;
#59531 = EDGE_CURVE ( 'NONE', #7527, #19609, #1122, .T. ) ;
#59532 = LINE ( 'NONE', #16972, #17269 ) ;
#59533 = CARTESIAN_POINT ( 'NONE',  ( 8.000000000000007105, 249.8719672152120381, 94.99999999999866418 ) ) ;
#59534 = VECTOR ( 'NONE', #47259, 1000.000000000000000 ) ;
#59535 = CARTESIAN_POINT ( 'NONE',  ( -156.6644740249450649, 71.86407434531899696, -71.41639533428784148 ) ) ;
#59536 = DIRECTION ( 'NONE',  ( -0.000000000000000000, -0.000000000000000000, -1.000000000000000000 ) ) ;
#59537 = PLANE ( 'NONE',  #44400 ) ;
#59538 = ORIENTED_EDGE ( 'NONE', *, *, #43887, .T. ) ;
#59539 = CARTESIAN_POINT ( 'NONE',  ( -49.44484229820457699, 14.28460989390479519, -37.71214243090105356 ) ) ;
#59540 = CYLINDRICAL_SURFACE ( 'NONE', #4473, 4.999999999999990230 ) ;
#59542 = ADVANCED_FACE ( 'NONE', ( #53527 ), #22925, .F. ) ;
#59541 = CARTESIAN_POINT ( 'NONE',  ( -30.46002654261638298, 10.45132580906818021, 30.26469554571997378 ) ) ;
#59543 = CARTESIAN_POINT ( 'NONE',  ( -1.224646799147352468E-15, 16.00000000000000000, -5.803681084894614095 ) ) ;
#59544 = CARTESIAN_POINT ( 'NONE',  ( -84.19760194758025307, 25.59349365599864257, 86.53227919859817518 ) ) ;
#59546 = EDGE_LOOP ( 'NONE', ( #21396, #38680, #49354, #1772, #29487, #64862, #55307, #11232 ) ) ;
#59545 = DIRECTION ( 'NONE',  ( 0.000000000000000000, 0.000000000000000000, -1.000000000000000000 ) ) ;
#59547 = EDGE_LOOP ( 'NONE', ( #47294, #46889 ) ) ;
#59548 = VECTOR ( 'NONE', #10696, 1000.000000000000114 ) ;
#59549 = ORIENTED_EDGE ( 'NONE', *, *, #56774, .F. ) ;
#59550 = CARTESIAN_POINT ( 'NONE',  ( -13.47230132170245298, 7.324574289401430960, -11.11349493250400577 ) ) ;
#59551 = CARTESIAN_POINT ( 'NONE',  ( -48.32993240732255913, 12.98137013984324817, 41.17929439291747684 ) ) ;
#59552 = DIRECTION ( 'NONE',  ( -3.344045254895050726E-17, -1.000000000000000000, -4.069049096960790458E-32 ) ) ;
#59553 = LINE ( 'NONE', #5060, #6324 ) ;
#59554 = CARTESIAN_POINT ( 'NONE',  ( -38.54237244144231767, 11.89088379031762344, 66.98059792128260881 ) ) ;
#59555 = CARTESIAN_POINT ( 'NONE',  ( -14.33060720034883495, 8.412649192293187639, -19.83824270713523319 ) ) ;
#59556 = DIRECTION ( 'NONE',  ( 1.000000000000000000, 7.105427357601001859E-15, 0.000000000000000000 ) ) ;
#59557 = CARTESIAN_POINT ( 'NONE',  ( 23.09541709302173729, 6.844586979481591449, -17.88187169697903656 ) ) ;
#59558 = EDGE_LOOP ( 'NONE', ( #44838, #2467, #14703, #6014 ) ) ;
#59559 = DIRECTION ( 'NONE',  ( 0.000000000000000000, 0.000000000000000000, 1.000000000000000000 ) ) ;
#59560 = ORIENTED_EDGE ( 'NONE', *, *, #42773, .T. ) ;
#59561 = ORIENTED_EDGE ( 'NONE', *, *, #55981, .F. ) ;
#59562 = CARTESIAN_POINT ( 'NONE',  ( -50.12142462338810134, -12.53590381416902311, 26.66469104408688651 ) ) ;
#59563 = CARTESIAN_POINT ( 'NONE',  ( -60.58154029404758489, 17.28267858483603447, -91.33302142368104626 ) ) ;
#59564 = CARTESIAN_POINT ( 'NONE',  ( 117.4400732876363804, 32.35632188881473326, 88.66185363912092043 ) ) ;
#59565 = VECTOR ( 'NONE', #5091, 1000.000000000000000 ) ;
#59566 = CARTESIAN_POINT ( 'NONE',  ( 116.6681538161788723, 33.09439081574000596, -20.47854696611932468 ) ) ;
#59567 = LINE ( 'NONE', #60977, #22515 ) ;
#59568 = CARTESIAN_POINT ( 'NONE',  ( 444.9999999999999432, -35.00000000000000000, 0.000000000000000000 ) ) ;
#59569 = CARTESIAN_POINT ( 'NONE',  ( 140.2058232509808420, 46.59155168125931823, -12.65523780476208238 ) ) ;
#59570 = VERTEX_POINT ( 'NONE', #10620 ) ;
#59571 = ORIENTED_EDGE ( 'NONE', *, *, #1162, .T. ) ;
#59572 = ORIENTED_EDGE ( 'NONE', *, *, #30840, .T. ) ;
#59573 = LINE ( 'NONE', #27930, #40598 ) ;
#59574 = DIRECTION ( 'NONE',  ( 0.000000000000000000, -0.5000000000000009992, -0.8660254037844380415 ) ) ;
#59575 = CARTESIAN_POINT ( 'NONE',  ( 39.40195752203891999, 9.424259417798147354, -35.61981746542776506 ) ) ;
#59576 = DIRECTION ( 'NONE',  ( -3.081487911019579554E-32, -1.000000000000000000, -3.469446951953612956E-17 ) ) ;
#59577 = CARTESIAN_POINT ( 'NONE',  ( -149.9449619562961118, 64.55090813009795170, -22.96827994102829607 ) ) ;
#59578 = ORIENTED_EDGE ( 'NONE', *, *, #45480, .T. ) ;
#59579 = CARTESIAN_POINT ( 'NONE',  ( 181.9295958320008708, 80.90438706151870463, 56.18881794660865125 ) ) ;
#59580 = CARTESIAN_POINT ( 'NONE',  ( -151.6716822472524484, 66.03661194063735707, 57.87064893191389814 ) ) ;
#59581 = EDGE_CURVE ( 'NONE', #28668, #11879, #20797, .T. ) ;
#59582 = CARTESIAN_POINT ( 'NONE',  ( -5.879983509979056500, 7.779504553499495323, -50.17789015261076457 ) ) ;
#59583 = CARTESIAN_POINT ( 'NONE',  ( 104.3931729003987101, 26.26823401847090622, 14.98636371210345963 ) ) ;
#59584 = CARTESIAN_POINT ( 'NONE',  ( 31.89651141207616192, -56.63578868294582946, 170.0000000000000000 ) ) ;
#59585 = CARTESIAN_POINT ( 'NONE',  ( -442.9409111889697783, 394.9999999999998863, -132.5214871221317878 ) ) ;
#59586 = CARTESIAN_POINT ( 'NONE',  ( 22.52576749827963809, 6.809805260274344185, 61.02798871425216731 ) ) ;
#59587 = CARTESIAN_POINT ( 'NONE',  ( 0.000000000000000000, 0.000000000000000000, 133.5802547743875550 ) ) ;
#59588 = CARTESIAN_POINT ( 'NONE',  ( 15.29305096970402644, 7.491604910111012039, 18.17015708224157322 ) ) ;
#59589 = ORIENTED_EDGE ( 'NONE', *, *, #21372, .F. ) ;
#59590 = CARTESIAN_POINT ( 'NONE',  ( 183.2136430849848239, 6.000000000000000000, -4.435653166495524324 ) ) ;
#59591 = AXIS2_PLACEMENT_3D ( 'NONE', #50180, #18522, #34365 ) ;
#59592 = CARTESIAN_POINT ( 'NONE',  ( 410.0000000000000000, 190.0000000000000000, -90.00000000000000000 ) ) ;
#59593 = CARTESIAN_POINT ( 'NONE',  ( -131.1078488676298832, 50.02394948559181387, -37.01727943492374351 ) ) ;
#59594 = CARTESIAN_POINT ( 'NONE',  ( 45.04360969585142982, 9.210232288266690048, -64.99837574662008421 ) ) ;
#59595 = CARTESIAN_POINT ( 'NONE',  ( 58.46823952472683317, 12.69204591816732908, -64.08093776701846878 ) ) ;
#59596 = ORIENTED_EDGE ( 'NONE', *, *, #67592, .T. ) ;
#59597 = PRODUCT_DEFINITION_SHAPE ( 'NONE', 'NONE',  #69635 ) ;
#59598 = VECTOR ( 'NONE', #11950, 1000.000000000000000 ) ;
#59599 = ORIENTED_EDGE ( 'NONE', *, *, #26678, .T. ) ;
#59600 = ADVANCED_FACE ( 'NONE', ( #24327 ), #28908, .F. ) ;
#59601 = CARTESIAN_POINT ( 'NONE',  ( -190.6985136298602015, 109.1272424661243434, 16.02916387300914280 ) ) ;
#59602 = CARTESIAN_POINT ( 'NONE',  ( 188.5939771839741752, 86.54409833618940695, 90.35527049066209315 ) ) ;
#59603 = EDGE_CURVE ( 'NONE', #31823, #45015, #50695, .T. ) ;
#59604 = VERTEX_POINT ( 'NONE', #40148 ) ;
#59605 = VERTEX_POINT ( 'NONE', #34188 ) ;
#59606 = CARTESIAN_POINT ( 'NONE',  ( 185.1660960081723601, 84.30194217633003007, 30.51265424631614920 ) ) ;
#59607 = CARTESIAN_POINT ( 'NONE',  ( 0.000000000000000000, 0.000000000000000000, 25.00000000000007816 ) ) ;
#59608 = VERTEX_POINT ( 'NONE', #29936 ) ;
#59609 = CARTESIAN_POINT ( 'NONE',  ( 129.1052153257903683, 39.78893484542955150, -64.54437869395790983 ) ) ;
#59610 = B_SPLINE_CURVE_WITH_KNOTS ( 'NONE', 3,
 ( #5874, #32284, #26992, #27334, #4851, #47749, #21714, #69212, #21036, #50194, #65688, #66397, #65330, #32969, #2362, #22761, #34379, #66743, #34020, #23814, #60036, #17476 ),
 .UNSPECIFIED., .F., .F.,
 ( 4, 2, 2, 2, 2, 2, 2, 2, 2, 2, 4 ),
 ( 7.734610455448194220E-17, 0.001318139496345227578, 0.001977209244517785965, 0.002636278992690344568, 0.003954418489035436621, 0.005272557985380528674, 0.005931627733553080338, 0.006590697481725632002, 0.007908836978070760484, 0.009226976474415886365, 0.01054511597076101224 ),
 .UNSPECIFIED. ) ;
#59611 = CARTESIAN_POINT ( 'NONE',  ( 134.7720294983483029, 43.15885542353191084, 71.31265126893414674 ) ) ;
#59612 = CARTESIAN_POINT ( 'NONE',  ( -76.32962633615591130, 21.44528079176260249, -49.74613438994566650 ) ) ;
#59613 = EDGE_CURVE ( 'NONE', #49963, #56069, #2515, .T. ) ;
#59614 = AXIS2_PLACEMENT_3D ( 'NONE', #69440, #46958, #31142 ) ;
#59615 = CARTESIAN_POINT ( 'NONE',  ( 86.62931800182292363, 19.42108912189599224, -89.51066537983906812 ) ) ;
#59616 = CARTESIAN_POINT ( 'NONE',  ( 89.87518614971254749, 20.55373388674513535, -50.09968107337091681 ) ) ;
#59617 = CARTESIAN_POINT ( 'NONE',  ( -189.5325095384514213, 107.4952257375067433, 40.55217149438323077 ) ) ;
#59618 = ORIENTED_EDGE ( 'NONE', *, *, #60033, .F. ) ;
#59619 = ORIENTED_EDGE ( 'NONE', *, *, #2104, .T. ) ;
#59620 = CARTESIAN_POINT ( 'NONE',  ( 111.1767565371974911, 29.31586421952251698, -50.87893186375811894 ) ) ;
#59621 = FACE_BOUND ( 'NONE', #20913, .T. ) ;
#59622 = B_SPLINE_CURVE_WITH_KNOTS ( 'NONE', 3,
 ( #41078, #58279, #57943, #52317, #4481, #47371, #13998, #46692 ),
 .UNSPECIFIED., .F., .F.,
 ( 4, 2, 2, 4 ),
 ( 0.004673709593152168724, 0.005837709341827655544, 0.007001709090503143232, 0.009329708587854116872 ),
 .UNSPECIFIED. ) ;
#59623 = ADVANCED_FACE ( 'NONE', ( #46105 ), #51403, .F. ) ;
#59624 = DIRECTION ( 'NONE',  ( 0.000000000000000000, 0.000000000000000000, 1.000000000000000000 ) ) ;
#59625 = CARTESIAN_POINT ( 'NONE',  ( -170.2951623264596890, 85.51757001115470302, -62.09646688624404476 ) ) ;
#59627 = ORIENTED_EDGE ( 'NONE', *, *, #23735, .T. ) ;
#59626 = CYLINDRICAL_SURFACE ( 'NONE', #27575, 10.00000000000000000 ) ;
#59628 = CARTESIAN_POINT ( 'NONE',  ( 56.29445224195348629, 12.24017809212662122, 7.103959071770647782 ) ) ;
#59629 = ADVANCED_FACE ( 'NONE', ( #61930 ), #61602, .F. ) ;
#59630 = EDGE_CURVE ( 'NONE', #16162, #15169, #39800, .T. ) ;
#59631 = ORIENTED_EDGE ( 'NONE', *, *, #42561, .T. ) ;
#59632 = DIRECTION ( 'NONE',  ( 0.000000000000000000, 0.000000000000000000, 1.000000000000000000 ) ) ;
#59633 = CARTESIAN_POINT ( 'NONE',  ( -55.53469534616546355, 14.81076603075805487, -23.37177340799619785 ) ) ;
#59634 = DIRECTION ( 'NONE',  ( -0.000000000000000000, -0.000000000000000000, -1.000000000000000000 ) ) ;
#59635 = CARTESIAN_POINT ( 'NONE',  ( -20.63749999999999574, 0.000000000000000000, 0.000000000000000000 ) ) ;
#59636 = CARTESIAN_POINT ( 'NONE',  ( 138.1919700334460686, 44.10401742531043823, -22.81667472755705006 ) ) ;
#59637 = CARTESIAN_POINT ( 'NONE',  ( 93.86680996363769225, 22.01878169039501643, -68.18320037815716717 ) ) ;
#59638 = CARTESIAN_POINT ( 'NONE',  ( 204.6977192012829789, 106.3443248447423315, 17.36317014830577321 ) ) ;
#59639 = CARTESIAN_POINT ( 'NONE',  ( -95.21430597939257723, 29.33390900154318359, 8.609081036463225090 ) ) ;
#59640 = LINE ( 'NONE', #11454, #4799 ) ;
#59641 = ORIENTED_EDGE ( 'NONE', *, *, #45169, .T. ) ;
#59642 = ORIENTED_EDGE ( 'NONE', *, *, #23377, .F. ) ;
#59643 = AXIS2_PLACEMENT_3D ( 'NONE', #27773, #18274, #54846 ) ;
#59644 = CARTESIAN_POINT ( 'NONE',  ( 40.37438610703017616, 8.537526699166106070, 29.96096040500725977 ) ) ;
#59645 = DIRECTION ( 'NONE',  ( 1.000000000000000000, 0.000000000000000000, 0.000000000000000000 ) ) ;
#59646 = CARTESIAN_POINT ( 'NONE',  ( 25.00000000000000000, 3.061616997868383043E-15, 0.000000000000000000 ) ) ;
#59647 = FACE_OUTER_BOUND ( 'NONE', #28482, .T. ) ;
#59648 = CARTESIAN_POINT ( 'NONE',  ( 211.8345664497466885, 118.5225165986914817, -46.15373158227198758 ) ) ;
#59649 = CIRCLE ( 'NONE', #38324, 35.00000000000000000 ) ;
#59650 = CARTESIAN_POINT ( 'NONE',  ( -71.57660578921957040, 20.81129687646280146, -66.96296472413820311 ) ) ;
#59651 = DIRECTION ( 'NONE',  ( -0.000000000000000000, -0.000000000000000000, 1.000000000000000000 ) ) ;
#59652 = CARTESIAN_POINT ( 'NONE',  ( 45.89232972083998874, 10.36128169546909739, -46.88626132967853977 ) ) ;
#59653 = CARTESIAN_POINT ( 'NONE',  ( 212.1535111375854967, 117.1635556319084799, 64.38318638549677075 ) ) ;
#59654 = ORIENTED_EDGE ( 'NONE', *, *, #45032, .F. ) ;
#59655 = CARTESIAN_POINT ( 'NONE',  ( -26.50207385662995918, 9.849226639603646305, 5.204319795929868597 ) ) ;
#59656 = VERTEX_POINT ( 'NONE', #45773 ) ;
#59657 = CIRCLE ( 'NONE', #45110, 4.999999999999990230 ) ;
#59658 =( GEOMETRIC_REPRESENTATION_CONTEXT ( 3 ) GLOBAL_UNCERTAINTY_ASSIGNED_CONTEXT ( ( #25456 ) ) GLOBAL_UNIT_ASSIGNED_CONTEXT ( ( #48934, #33833, #54920 ) ) REPRESENTATION_CONTEXT ( 'NONE', 'WORKASPACE' ) );
#59659 = CARTESIAN_POINT ( 'NONE',  ( -102.2801239173131052, 33.91021738430207222, 57.36362509687880618 ) ) ;
#59660 = CYLINDRICAL_SURFACE ( 'NONE', #40884, 7.500000000000020428 ) ;
#59661 = CARTESIAN_POINT ( 'NONE',  ( 93.72687053612526142, 23.04134601640627267, 61.58162035816948077 ) ) ;
#59662 = CARTESIAN_POINT ( 'NONE',  ( 152.1327777395850660, 53.61712543276775023, -11.50499121041532469 ) ) ;
#59663 = LINE ( 'NONE', #16072, #53462 ) ;
#59664 = CARTESIAN_POINT ( 'NONE',  ( -783.0172411895269988, -622.0000000000060254, 10.00000000000000000 ) ) ;
#59665 = CIRCLE ( 'NONE', #51857, 5.000000000000004441 ) ;
#59666 = LINE ( 'NONE', #37886, #42753 ) ;
#59667 = CARTESIAN_POINT ( 'NONE',  ( 211.9344894260836725, 116.8270173945561510, 88.38486393112469841 ) ) ;
#59668 = CARTESIAN_POINT ( 'NONE',  ( 25.02868068539619628, 33.38981722302369093, 13.79046412397660148 ) ) ;
#59670 = ORIENTED_EDGE ( 'NONE', *, *, #63706, .F. ) ;
#59669 = ADVANCED_FACE ( 'NONE', ( #7090 ), #3215, .F. ) ;
#59671 = CARTESIAN_POINT ( 'NONE',  ( 61.08522853873729019, 13.26388801693372343, 71.42126950169983957 ) ) ;
#59672 = CARTESIAN_POINT ( 'NONE',  ( -102.2801239173131194, 32.78103895658057354, -8.170026674512225640 ) ) ;
#59673 = CARTESIAN_POINT ( 'NONE',  ( -12.39770133248888406, 8.241491894828985920, 4.805493982876364534 ) ) ;
#59674 = CARTESIAN_POINT ( 'NONE',  ( 46.65974587859241751, 10.48396258569371398, -71.91825419913200790 ) ) ;
#59675 = CARTESIAN_POINT ( 'NONE',  ( -0.3258398948454890864, 6.518608385615800138, 37.11425296739088253 ) ) ;
#59676 = CARTESIAN_POINT ( 'NONE',  ( -108.0980548770428129, 35.83569586822709141, -64.60032205779721437 ) ) ;
#59677 = CARTESIAN_POINT ( 'NONE',  ( 92.40462699547136083, 22.54601413076274952, 86.10444742709040611 ) ) ;
#59678 = EDGE_CURVE ( 'NONE', #58185, #16629, #60554, .T. ) ;
#59679 = EDGE_LOOP ( 'NONE', ( #49366, #7492, #22441, #25120 ) ) ;
#59680 = DIRECTION ( 'NONE',  ( -9.514340003854222824E-15, 4.261029262954733616E-15, -0.9999999999999997780 ) ) ;
#59681 = DIRECTION ( 'NONE',  ( -1.000000000000000000, 0.000000000000000000, 0.000000000000000000 ) ) ;
#59682 = DIRECTION ( 'NONE',  ( 2.201526392813417799E-16, -1.184691869787064686E-16, 1.000000000000000000 ) ) ;
#59683 = CARTESIAN_POINT ( 'NONE',  ( -169.8972248494842745, 85.08697738648012887, -35.42540969111004756 ) ) ;
#59684 = CONTEXT_DEPENDENT_SHAPE_REPRESENTATION ( #54772, #50166 ) ;
#59685 = CARTESIAN_POINT ( 'NONE',  ( -132.9227230387961072, 52.53474289881230419, -39.78390660009881685 ) ) ;
#59686 = ORIENTED_EDGE ( 'NONE', *, *, #61770, .T. ) ;
#59687 = CARTESIAN_POINT ( 'NONE',  ( -41.50537345350708307, 50.04124777106294886, 41.38025477438755928 ) ) ;
#59688 = DIRECTION ( 'NONE',  ( 0.000000000000000000, 0.000000000000000000, 1.000000000000000000 ) ) ;
#59689 = ADVANCED_FACE ( 'NONE', ( #56669 ), #49996, .F. ) ;
#59690 = CARTESIAN_POINT ( 'NONE',  ( 197.2199163281728147, 98.22431253015349739, -17.64478213631704762 ) ) ;
#59691 = CARTESIAN_POINT ( 'NONE',  ( -156.5968336791922582, 70.43374190556866665, 94.38119541604979190 ) ) ;
#59692 = EDGE_CURVE ( 'NONE', #63697, #10376, #34541, .T. ) ;
#59693 = DIRECTION ( 'NONE',  ( -0.8160245890732938934, -0.5780171883497599028, 0.000000000000000000 ) ) ;
#59694 = ADVANCED_FACE ( 'NONE', ( #66550 ), #55982, .F. ) ;
#59695 = VERTEX_POINT ( 'NONE', #7451 ) ;
#59696 = FACE_OUTER_BOUND ( 'NONE', #19588, .T. ) ;
#59697 = CARTESIAN_POINT ( 'NONE',  ( 79.54836217416615796, 18.17815803851262402, 7.882887560960153195 ) ) ;
#59698 = CARTESIAN_POINT ( 'NONE',  ( 0.000000000000000000, 0.000000000000000000, 170.0000000000000000 ) ) ;
#59699 = AXIS2_PLACEMENT_3D ( 'NONE', #27511, #48953, #43684 ) ;
#59700 = CARTESIAN_POINT ( 'NONE',  ( 0.7145311798163274108, 9.237604307034018802, -2.124379920709345337E-16 ) ) ;
#59701 = AXIS2_PLACEMENT_3D ( 'NONE', #4782, #64920, #53650 ) ;
#59702 = VERTEX_POINT ( 'NONE', #60898 ) ;
#59703 = FACE_OUTER_BOUND ( 'NONE', #32540, .T. ) ;
#59704 = ORIENTED_EDGE ( 'NONE', *, *, #21196, .F. ) ;
#59705 = AXIS2_PLACEMENT_3D ( 'NONE', #22115, #27735, #305 ) ;
#59706 = VECTOR ( 'NONE', #37988, 1000.000000000000000 ) ;
#59707 = EDGE_LOOP ( 'NONE', ( #69015, #13065 ) ) ;
#59708 = CARTESIAN_POINT ( 'NONE',  ( -118.9073340572059863, 42.06264533740859690, -93.36481285813314912 ) ) ;
#59709 = CARTESIAN_POINT ( 'NONE',  ( 213.7144242967635535, -1.188791048788683712E-16, 277.7626972944978547 ) ) ;
#59711 = VERTEX_POINT ( 'NONE', #12720 ) ;
#59710 = CARTESIAN_POINT ( 'NONE',  ( 15.55634918610411610, 46.66904755831205875, 0.000000000000000000 ) ) ;
#59712 = DIRECTION ( 'NONE',  ( -0.000000000000000000, 1.000000000000000000, -0.000000000000000000 ) ) ;
#59713 = CLOSED_SHELL ( 'NONE', ( #17044, #42169, #19483, #9832, #1687, #17972, #36985, #41724, #24077 ) ) ;
#59714 = DIRECTION ( 'NONE',  ( -0.000000000000000000, -0.000000000000000000, -1.000000000000000000 ) ) ;
#59715 = EDGE_CURVE ( 'NONE', #13434, #50950, #55622, .T. ) ;
#59716 = ADVANCED_FACE ( 'NONE', ( #61256, #7794, #56316, #8137, #29580, #51049 ), #2859, .T. ) ;
#59717 = LINE ( 'NONE', #43192, #8110 ) ;
#59718 = ORIENTED_EDGE ( 'NONE', *, *, #62824, .F. ) ;
#59719 = EDGE_CURVE ( 'NONE', #28906, #39565, #42145, .T. ) ;
#59720 = CARTESIAN_POINT ( 'NONE',  ( -71.90777365577110913, -21.14201501538416395, 41.38025477438755928 ) ) ;
#59721 = LINE ( 'NONE', #49511, #17369 ) ;
#59722 = FACE_OUTER_BOUND ( 'NONE', #61555, .T. ) ;
#59723 = CARTESIAN_POINT ( 'NONE',  ( 127.2107679985236501, 38.70844091144996924, 67.36980645316099015 ) ) ;
#59724 = ORIENTED_EDGE ( 'NONE', *, *, #28827, .F. ) ;
#59725 = ORIENTED_EDGE ( 'NONE', *, *, #3110, .T. ) ;
#59726 = ORIENTED_EDGE ( 'NONE', *, *, #47447, .T. ) ;
#59727 = CARTESIAN_POINT ( 'NONE',  ( -47.60267131192345857, 12.80969088899330721, 90.58369976394168077 ) ) ;
#59728 = PLANE ( 'NONE',  #51538 ) ;
#59729 = CARTESIAN_POINT ( 'NONE',  ( -36.84489839129339828, 53.54860840895182150, 40.00000000000003553 ) ) ;
#59730 = CARTESIAN_POINT ( 'NONE',  ( -109.7865258608846801, 36.76046659111707271, 91.82485696114136431 ) ) ;
#59731 = DIRECTION ( 'NONE',  ( -0.000000000000000000, -0.000000000000000000, -1.000000000000000000 ) ) ;
#59732 = CARTESIAN_POINT ( 'NONE',  ( -15.55634918610411077, -46.66904755831208718, 0.000000000000000000 ) ) ;
#59733 = CARTESIAN_POINT ( 'NONE',  ( -48.51071349036728009, 14.05900477738932253, 87.82452332375471826 ) ) ;
#59734 = DIRECTION ( 'NONE',  ( 1.000000000000000000, 0.000000000000000000, 0.000000000000000000 ) ) ;
#59735 = VERTEX_POINT ( 'NONE', #26391 ) ;
#59736 = CARTESIAN_POINT ( 'NONE',  ( -6.000000000000000000, 19.07878402833891229, -20.00000000000000000 ) ) ;
#59737 = ORIENTED_EDGE ( 'NONE', *, *, #7337, .F. ) ;
#59738 = DIRECTION ( 'NONE',  ( -2.398676446365434695E-14, 0.000000000000000000, 1.000000000000000000 ) ) ;
#59739 = CARTESIAN_POINT ( 'NONE',  ( 212.1707951106657504, 117.1901534358506041, -70.01254296698697033 ) ) ;
#59740 = CARTESIAN_POINT ( 'NONE',  ( 0.000000000000000000, 0.000000000000000000, 5.000000000000000000 ) ) ;
#59741 = DIRECTION ( 'NONE',  ( 1.604841615724182956E-15, 1.000000000000000000, 1.604841615724182561E-15 ) ) ;
#59742 = CARTESIAN_POINT ( 'NONE',  ( -38.78626392836186909, 10.91334659013840103, -95.00000000000133582 ) ) ;
#59743 = CARTESIAN_POINT ( 'NONE',  ( 23.28845814680232351, 7.864847136539610872, 37.02807486054078367 ) ) ;
#59744 = AXIS2_PLACEMENT_3D ( 'NONE', #55923, #60495, #18629 ) ;
#59745 = DIRECTION ( 'NONE',  ( -0.000000000000000000, 1.000000000000000000, -0.000000000000000000 ) ) ;
#59746 = FACE_OUTER_BOUND ( 'NONE', #42074, .T. ) ;
#59747 = EDGE_LOOP ( 'NONE', ( #14610, #25675, #12657, #59764 ) ) ;
#59748 = CIRCLE ( 'NONE', #30561, 4.999999999999997335 ) ;
#59749 = CARTESIAN_POINT ( 'NONE',  ( 157.4703587214989398, -170.0000000000000000, 36.90946747225337532 ) ) ;
#59750 = CARTESIAN_POINT ( 'NONE',  ( -59.94154301275508345, -45.09516516490472071, 43.58025477438756923 ) ) ;
#59751 = EDGE_LOOP ( 'NONE', ( #67526, #52190, #56187, #67505 ) ) ;
#59752 = CARTESIAN_POINT ( 'NONE',  ( -63.73419499958998813, 12.83646726144838013, 43.58025477438756923 ) ) ;
#59753 =( NAMED_UNIT ( * ) PLANE_ANGLE_UNIT ( ) SI_UNIT ( $, .RADIAN. ) );
#59754 = VERTEX_POINT ( 'NONE', #46448 ) ;
#59755 = CARTESIAN_POINT ( 'NONE',  ( -82.32750425780474757, 23.74963782027935721, 44.48151486517527076 ) ) ;
#59756 = CARTESIAN_POINT ( 'NONE',  ( 410.0000000000000000, 190.0000000000000000, -2.000000000000000000 ) ) ;
#59757 = CARTESIAN_POINT ( 'NONE',  ( 61.09275639403233527, 12.23448398202909537, -50.48616642848160296 ) ) ;
#59758 = AXIS2_PLACEMENT_3D ( 'NONE', #44299, #33766, #23217 ) ;
#59759 = LINE ( 'NONE', #49553, #15938 ) ;
#59760 = EDGE_CURVE ( 'NONE', #15636, #17325, #49290, .T. ) ;
#59761 = CARTESIAN_POINT ( 'NONE',  ( 129.1381264900934411, 38.64720302602604107, -10.82883967016261550 ) ) ;
#59762 = CIRCLE ( 'NONE', #29455, 242.4895526022646379 ) ;
#59763 = ORIENTED_EDGE ( 'NONE', *, *, #64543, .T. ) ;
#59764 = ORIENTED_EDGE ( 'NONE', *, *, #28494, .T. ) ;
#59765 = CARTESIAN_POINT ( 'NONE',  ( -89.99999999999998579, 1.102182119232617596E-14, 7.000000000000000000 ) ) ;
#59766 = ORIENTED_EDGE ( 'NONE', *, *, #64649, .T. ) ;
#59767 = CARTESIAN_POINT ( 'NONE',  ( 1.005827167100601827, 70.00000000000000000, -9.949286995052577964 ) ) ;
#59768 = CARTESIAN_POINT ( 'NONE',  ( -147.3669217311067996, 63.69361261596465340, 31.02940414706721128 ) ) ;
#59769 = CARTESIAN_POINT ( 'NONE',  ( 60.40277045393653310, 12.08176563382369650, 71.19188811025489372 ) ) ;
#59770 = CARTESIAN_POINT ( 'NONE',  ( -5.412684891282531829, 7.753215344827982136, 57.34180824127475518 ) ) ;
#59771 = EDGE_CURVE ( 'NONE', #49789, #55679, #20772, .T. ) ;
#59772 = CYLINDRICAL_SURFACE ( 'NONE', #16715, 65.36598343705435354 ) ;
#59773 = SURFACE_STYLE_USAGE ( .BOTH. , #21132 ) ;
#59774 = ORIENTED_EDGE ( 'NONE', *, *, #30042, .T. ) ;
#59775 = EDGE_CURVE ( 'NONE', #36732, #54785, #63332, .T. ) ;
#59776 = CARTESIAN_POINT ( 'NONE',  ( -4.000000000000009770, -6.928203230275505220, -9.500000000000000000 ) ) ;
#59777 = VERTEX_POINT ( 'NONE', #52753 ) ;
#59778 = EDGE_CURVE ( 'NONE', #26520, #38200, #67764, .T. ) ;
#59779 = EDGE_LOOP ( 'NONE', ( #34540, #52759, #59980, #46820 ) ) ;
#59780 = FACE_OUTER_BOUND ( 'NONE', #5894, .T. ) ;
#59781 = CARTESIAN_POINT ( 'NONE',  ( -447.6627218934912094, 389.9999999999997726, 108.5502958579879476 ) ) ;
#59782 = CARTESIAN_POINT ( 'NONE',  ( -170.2747214445850261, 84.01465441107043830, -8.415621470039866381 ) ) ;
#59783 = DIRECTION ( 'NONE',  ( -0.000000000000000000, -0.000000000000000000, 1.000000000000000000 ) ) ;
#59784 = CARTESIAN_POINT ( 'NONE',  ( -45.00000000000000000, 22.99999999999998579, 4.000000000000000000 ) ) ;
#59785 = EDGE_CURVE ( 'NONE', #14375, #14640, #37267, .T. ) ;
#59786 = ORIENTED_EDGE ( 'NONE', *, *, #7256, .T. ) ;
#59787 = CARTESIAN_POINT ( 'NONE',  ( 84.28078136020371858, 18.63296074526051527, 17.49438883205864670 ) ) ;
#59788 = ORIENTED_EDGE ( 'NONE', *, *, #58117, .F. ) ;
#59789 = CARTESIAN_POINT ( 'NONE',  ( -71.17819443284076897, 19.60909329639481058, 38.40917392580900014 ) ) ;
#59790 = ORIENTED_EDGE ( 'NONE', *, *, #63693, .T. ) ;
#59791 = CARTESIAN_POINT ( 'NONE',  ( 2.129405171194075130, 25.03204795498856683, 3.061616997868437868E-16 ) ) ;
#59792 = VECTOR ( 'NONE', #37475, 999.9999999999998863 ) ;
#59793 = ORIENTED_EDGE ( 'NONE', *, *, #52182, .T. ) ;
#59794 = CARTESIAN_POINT ( 'NONE',  ( -196.7348448768811409, -170.0000000000000000, 11.57801738291933091 ) ) ;
#59795 = CARTESIAN_POINT ( 'NONE',  ( 88.98408042523108463, 20.23787745328941767, 3.242737632188622321 ) ) ;
#59796 = EDGE_CURVE ( 'NONE', #2243, #9949, #48494, .T. ) ;
#59797 = DIRECTION ( 'NONE',  ( -1.000000000000000000, 0.000000000000000000, 0.000000000000000000 ) ) ;
#59798 = VECTOR ( 'NONE', #15362, 1000.000000000000000 ) ;
#59799 = ORIENTED_EDGE ( 'NONE', *, *, #19864, .F. ) ;
#59800 = ADVANCED_FACE ( 'NONE', ( #5947 ), #21783, .F. ) ;
#59801 = CARTESIAN_POINT ( 'NONE',  ( 133.8566784816069344, -170.0000000000000000, -77.86786152285937135 ) ) ;
#59802 = AXIS2_PLACEMENT_3D ( 'NONE', #51638, #41428, #19619 ) ;
#59803 = CARTESIAN_POINT ( 'NONE',  ( -444.1138056043201345, 394.7873829578389291, 97.81866361316865266 ) ) ;
#59804 = LINE ( 'NONE', #66171, #55636 ) ;
#59805 = CARTESIAN_POINT ( 'NONE',  ( -173.1211646369891355, 88.63826465341152527, -34.71195716474998960 ) ) ;
#59806 = CARTESIAN_POINT ( 'NONE',  ( -133.3926783185151521, 51.63401075114366279, -15.26785645255982438 ) ) ;
#59807 = LINE ( 'NONE', #22189, #21060 ) ;
#59808 = DIRECTION ( 'NONE',  ( -0.000000000000000000, 0.000000000000000000, -1.000000000000000000 ) ) ;
#59809 = VERTEX_POINT ( 'NONE', #59756 ) ;
#59810 = CARTESIAN_POINT ( 'NONE',  ( 134.0849965622593913, 42.73957449886184179, -77.86786152285938556 ) ) ;
#59811 = CARTESIAN_POINT ( 'NONE',  ( 10.55634918610406281, 15.55634918610400241, 2.000000000000001776 ) ) ;
#59812 = ORIENTED_EDGE ( 'NONE', *, *, #32153, .T. ) ;
#59813 = VECTOR ( 'NONE', #50071, 1000.000000000000000 ) ;
#59814 = FACE_BOUND ( 'NONE', #41607, .T. ) ;
#59815 = CARTESIAN_POINT ( 'NONE',  ( -0.8055628312658246193, 6.535476276302841114, -72.41444179526300218 ) ) ;
#59816 = CARTESIAN_POINT ( 'NONE',  ( -179.5109681715918271, 96.11572638569522553, 61.20124511069693085 ) ) ;
#59817 = CARTESIAN_POINT ( 'NONE',  ( 115.8407534776555252, 31.55877564758569775, -92.10373643822070733 ) ) ;
#59818 = CARTESIAN_POINT ( 'NONE',  ( -118.3918229753715252, 42.92682904595257298, -42.92333884901141516 ) ) ;
#59819 = CARTESIAN_POINT ( 'NONE',  ( 437.3372781065085633, 399.9999999999998863, 108.5502958579881891 ) ) ;
#59820 = FACE_OUTER_BOUND ( 'NONE', #4737, .T. ) ;
#59821 = CARTESIAN_POINT ( 'NONE',  ( 110.6524747721059754, 21.43176909745610814, -4.968265989321539067 ) ) ;
#59822 = CARTESIAN_POINT ( 'NONE',  ( -71.47840469610784453, 19.71248552135259757, -94.11786278736408917 ) ) ;
#59823 = CARTESIAN_POINT ( 'NONE',  ( 60.40479419793764038, 24.00543350795394915, 170.0000000000000000 ) ) ;
#59824 = CARTESIAN_POINT ( 'NONE',  ( 115.0454575488273434, 31.16784721673997183, 4.500807871381157454 ) ) ;
#59825 = CARTESIAN_POINT ( 'NONE',  ( 39.40195752203892710, 9.424259417798138472, -89.30891864635511013 ) ) ;
#59826 = VERTEX_POINT ( 'NONE', #42558 ) ;
#59827 = CARTESIAN_POINT ( 'NONE',  ( 9.962235950565768050, -64.23203137738408941, 40.00000000000003553 ) ) ;
#59828 = ORIENTED_EDGE ( 'NONE', *, *, #56066, .F. ) ;
#59829 = CARTESIAN_POINT ( 'NONE',  ( -27.00000000000000355, -27.00000000000000355, 15.00000000000000000 ) ) ;
#59830 = DIRECTION ( 'NONE',  ( 0.000000000000000000, -1.000000000000000000, 0.000000000000000000 ) ) ;
#59831 = CARTESIAN_POINT ( 'NONE',  ( 106.0076881141067702, 28.07010157927252436, 84.57606687714297777 ) ) ;
#59832 = CARTESIAN_POINT ( 'NONE',  ( 110.2429982417149574, -170.0000000000000000, -97.11153874658106133 ) ) ;
#59833 = DIRECTION ( 'NONE',  ( -0.000000000000000000, -0.000000000000000000, -1.000000000000000000 ) ) ;
#59834 = CARTESIAN_POINT ( 'NONE',  ( -30.95341298663138474, 10.53108683215057262, -50.31719736520187070 ) ) ;
#59835 = CARTESIAN_POINT ( 'NONE',  ( 211.5787168283555673, 118.1262790876037485, -94.52141717514192010 ) ) ;
#59836 = CARTESIAN_POINT ( 'NONE',  ( -78.24445602694504487, 23.23728082089436953, -88.80455181264525777 ) ) ;
#59837 = CYLINDRICAL_SURFACE ( 'NONE', #25159, 7.500000000000013323 ) ;
#59838 = ORIENTED_EDGE ( 'NONE', *, *, #43707, .F. ) ;
#59839 = ORIENTED_EDGE ( 'NONE', *, *, #50105, .F. ) ;
#59840 = EDGE_CURVE ( 'NONE', #10488, #41805, #63534, .T. ) ;
#59841 = CARTESIAN_POINT ( 'NONE',  ( 32.66364305947234925, 8.639871491745250154, 67.58839702922695380 ) ) ;
#59842 = CARTESIAN_POINT ( 'NONE',  ( 173.5843421840238250, 71.34465141434344559, 63.95638635334570665 ) ) ;
#59843 = CARTESIAN_POINT ( 'NONE',  ( -165.6404838346739155, 80.60836113891895138, 65.78406423995896546 ) ) ;
#59844 = EDGE_CURVE ( 'NONE', #2040, #65219, #55975, .T. ) ;
#59845 = DIRECTION ( 'NONE',  ( 0.000000000000000000, 1.000000000000000000, -0.000000000000000000 ) ) ;
#59846 = PRODUCT_DEFINITION_CONTEXT ( 'detailed design', #11623, 'design' ) ;
#59847 = AXIS2_PLACEMENT_3D ( 'NONE', #7782, #3202, #30276 ) ;
#59848 = FACE_OUTER_BOUND ( 'NONE', #35067, .T. ) ;
#59849 = VERTEX_POINT ( 'NONE', #39031 ) ;
#59850 = CARTESIAN_POINT ( 'NONE',  ( 0.000000000000000000, 0.000000000000000000, 41.38025477438755928 ) ) ;
#59851 = CARTESIAN_POINT ( 'NONE',  ( -15.07200981767290848, 7.471751903425209562, 66.40871753783480358 ) ) ;
#59852 = CARTESIAN_POINT ( 'NONE',  ( 211.4997502125519304, 118.0043045815490501, 6.689424349925599422 ) ) ;
#59853 = AXIS2_PLACEMENT_3D ( 'NONE', #52989, #26277, #63905 ) ;
#59854 = B_SPLINE_CURVE_WITH_KNOTS ( 'NONE', 3,
 ( #64157, #54638, #6465, #12091, #65560, #49350 ),
 .UNSPECIFIED., .F., .F.,
 ( 4, 2, 4 ),
 ( 0.03218932929355815264, 0.06469831333814429764, 0.09720729738273045650 ),
 .UNSPECIFIED. ) ;
#59855 = LINE ( 'NONE', #6407, #25099 ) ;
#59856 = CARTESIAN_POINT ( 'NONE',  ( 44.34263167748004264, 9.103379693481564061, -21.93902944785204667 ) ) ;
#59857 = CARTESIAN_POINT ( 'NONE',  ( -62.97854483871554976, -16.08424353203763957, 170.0000000000000000 ) ) ;
#59858 = FACE_BOUND ( 'NONE', #60149, .T. ) ;
#59859 = CARTESIAN_POINT ( 'NONE',  ( -61.38706483483509402, 16.47181058798475917, -38.69296264354031223 ) ) ;
#59860 = CIRCLE ( 'NONE', #9316, 65.00000000000000000 ) ;
#59861 = AXIS2_PLACEMENT_3D ( 'NONE', #43331, #54225, #32451 ) ;
#59862 = EDGE_CURVE ( 'NONE', #67613, #59387, #47755, .T. ) ;
#59863 = ORIENTED_EDGE ( 'NONE', *, *, #46363, .F. ) ;
#59864 = EDGE_CURVE ( 'NONE', #20962, #57676, #23201, .T. ) ;
#59865 = DIRECTION ( 'NONE',  ( -0.000000000000000000, -1.000000000000000000, -0.000000000000000000 ) ) ;
#59866 = CARTESIAN_POINT ( 'NONE',  ( 87.58754341703158275, 20.81465688423120142, -35.86779864721757605 ) ) ;
#59867 = CIRCLE ( 'NONE', #23941, 20.00000000000000000 ) ;
#59868 = CARTESIAN_POINT ( 'NONE',  ( -49.43836229152578454, 14.28302414152160438, 59.66443661698006906 ) ) ;
#59869 = DIRECTION ( 'NONE',  ( -0.000000000000000000, -0.000000000000000000, -1.000000000000000000 ) ) ;
#59870 = CARTESIAN_POINT ( 'NONE',  ( 151.1873096904021736, 52.92629247302095763, 14.16866593802975949 ) ) ;
#59871 = LINE ( 'NONE', #12747, #8620 ) ;
#59872 = ORIENTED_EDGE ( 'NONE', *, *, #52548, .F. ) ;
#59873 = CARTESIAN_POINT ( 'NONE',  ( 55.76298701799387914, 11.10663440745154240, 12.44327555652177608 ) ) ;
#59874 = CARTESIAN_POINT ( 'NONE',  ( -58.32860549785897319, 15.58423118879329294, 57.91070985857294318 ) ) ;
#59875 = VERTEX_POINT ( 'NONE', #39719 ) ;
#59876 = VERTEX_POINT ( 'NONE', #8052 ) ;
#59877 = DIRECTION ( 'NONE',  ( -0.000000000000000000, -0.000000000000000000, 1.000000000000000000 ) ) ;
#59878 = CARTESIAN_POINT ( 'NONE',  ( 16.62148331457488837, 18.83783649008728744, 0.000000000000000000 ) ) ;
#59879 = CARTESIAN_POINT ( 'NONE',  ( 102.8066580714140912, 25.59117171226998977, 36.10287978058507008 ) ) ;
#59880 = ORIENTED_EDGE ( 'NONE', *, *, #2948, .T. ) ;
#59881 = VERTEX_POINT ( 'NONE', #33753 ) ;
#59882 = CARTESIAN_POINT ( 'NONE',  ( 41.80372346091802882, 9.750024116765239057, 71.36764769552664234 ) ) ;
#59883 = LINE ( 'NONE', #11702, #67314 ) ;
#59884 = CARTESIAN_POINT ( 'NONE',  ( -156.9919426121902575, 72.16759471857101005, -68.59451387288930846 ) ) ;
#59885 = CARTESIAN_POINT ( 'NONE',  ( 70.12389542974194967, 15.47520081968154315, 8.025324115680595227 ) ) ;
#59886 = LINE ( 'NONE', #33179, #18554 ) ;
#59887 = CARTESIAN_POINT ( 'NONE',  ( -47.55316895016326129, 13.83165595246916801, -42.21365577270224634 ) ) ;
#59888 = AXIS2_PLACEMENT_3D ( 'NONE', #24508, #40661, #7634 ) ;
#59889 = CARTESIAN_POINT ( 'NONE',  ( -2.700000000000004619, 3.061616997868383831E-15, 25.00000000000000711 ) ) ;
#59890 = CARTESIAN_POINT ( 'NONE',  ( -155.3934881382774336, 70.69666961025296814, -91.34784486870364617 ) ) ;
#59891 = PLANE ( 'NONE',  #56263 ) ;
#59892 = CARTESIAN_POINT ( 'NONE',  ( 81.09284835776151112, 17.60558077568531132, 85.83069754542404439 ) ) ;
#59894 = ORIENTED_EDGE ( 'NONE', *, *, #28499, .F. ) ;
#59893 = CARTESIAN_POINT ( 'NONE',  ( 0.3167204509598382511, 8.479269695850865318, -1.313474075707213418 ) ) ;
#59895 = ORIENTED_EDGE ( 'NONE', *, *, #11472, .F. ) ;
#59896 = EDGE_LOOP ( 'NONE', ( #33583, #22258, #6163, #28415, #22161, #63000 ) ) ;
#59897 = DIRECTION ( 'NONE',  ( 0.000000000000000000, 0.000000000000000000, 1.000000000000000000 ) ) ;
#59898 = CARTESIAN_POINT ( 'NONE',  ( -171.5398786593827936, 86.87885897849457706, 84.67500624867942349 ) ) ;
#59899 = PLANE ( 'NONE',  #33425 ) ;
#59900 = DIRECTION ( 'NONE',  ( 1.000000000000000000, 0.000000000000000000, 0.000000000000000000 ) ) ;
#59901 = CIRCLE ( 'NONE', #38583, 5.000000000000000888 ) ;
#59902 = CARTESIAN_POINT ( 'NONE',  ( -61.53550548562875377, 17.56596194025584978, -38.91274425169289231 ) ) ;
#59903 = B_SPLINE_CURVE_WITH_KNOTS ( 'NONE', 3,
 ( #63190, #33616, #22694, #33261, #54695, #59612, #28675, #50130, #1241, #60330, #11091, #7219, #49060, #54336, #895, #39234, #28315, #44131, #545, #59968, #32898, #53984, #43785, #6155, #65622, #32553, #11428, #1957, #12151, #49413, #55042, #6865, #5810, #65259, #27264, #38886, #17409, #21998, #11785, #55390, #49757, #23053, #27969, #17052 ),
 .UNSPECIFIED., .F., .F.,
 ( 4, 2, 2, 2, 2, 2, 2, 2, 2, 2, 2, 2, 2, 2, 2, 2, 2, 2, 2, 2, 2, 4 ),
 ( 0.02432640572110343624, 0.02583721026359364625, 0.02659261253483873391, 0.02734801480608382157, 0.02885881934857402811, 0.02961422161981911577, 0.03036962389106420343, 0.03188042843355436140, 0.03339123297604452978, 0.03414663524728961397, 0.03490203751853471204, 0.03641284206102490123, 0.03716824433226999930, 0.03792364660351509736, 0.03943445114600528656, 0.04094525568849546882, 0.04245606023098566495, 0.04396686477347584721, 0.04472226704472094527, 0.04547766931596604334, 0.04698847385845628111, 0.04849927840094651194 ),
 .UNSPECIFIED. ) ;
#59904 = VECTOR ( 'NONE', #5201, 1000.000000000000000 ) ;
#59905 = CARTESIAN_POINT ( 'NONE',  ( -10.69547592951790982, 8.103864096836385755, -23.01549004601787729 ) ) ;
#59906 = CARTESIAN_POINT ( 'NONE',  ( -71.37402418445425667, 19.67651958824262692, -71.23054666910613264 ) ) ;
#59907 = CARTESIAN_POINT ( 'NONE',  ( 21.75684465274325063, 6.764994602232768273, -11.60645927818548451 ) ) ;
#59908 = ORIENTED_EDGE ( 'NONE', *, *, #49690, .F. ) ;
#59909 = AXIS2_PLACEMENT_3D ( 'NONE', #43611, #11595, #50299 ) ;
#59910 = DIRECTION ( 'NONE',  ( -1.000000000000000000, 0.000000000000000000, 0.000000000000000000 ) ) ;
#59911 = ORIENTED_EDGE ( 'NONE', *, *, #11730, .T. ) ;
#59912 = EDGE_LOOP ( 'NONE', ( #59481, #42714 ) ) ;
#59913 = CARTESIAN_POINT ( 'NONE',  ( -143.2587158300141823, 60.34092810886538416, 15.53215084215549346 ) ) ;
#59914 = FACE_OUTER_BOUND ( 'NONE', #19709, .T. ) ;
#59915 = CIRCLE ( 'NONE', #43098, 89.99999999999998579 ) ;
#59916 = CARTESIAN_POINT ( 'NONE',  ( 117.1442106208647971, 32.20759653584552495, 93.81850280107182982 ) ) ;
#59917 = CARTESIAN_POINT ( 'NONE',  ( -8.000000000000000000, 0.000000000000000000, -9.500000000000000000 ) ) ;
#59918 = EDGE_CURVE ( 'NONE', #19003, #33435, #5611, .T. ) ;
#59919 = CARTESIAN_POINT ( 'NONE',  ( 10.06749493632500503, -74.32123213259498584, 43.58025477438756212 ) ) ;
#59920 = CARTESIAN_POINT ( 'NONE',  ( -78.66644367742109978, 23.39876645725290061, 45.41820113967312977 ) ) ;
#59921 = CARTESIAN_POINT ( 'NONE',  ( 138.5684226926155702, 45.53585076428269218, -10.82367928455951400 ) ) ;
#59922 = ORIENTED_EDGE ( 'NONE', *, *, #55811, .F. ) ;
#59923 = VERTEX_POINT ( 'NONE', #52679 ) ;
#59924 = EDGE_CURVE ( 'NONE', #6513, #54974, #51191, .T. ) ;
#59925 = ORIENTED_EDGE ( 'NONE', *, *, #12069, .F. ) ;
#59926 = DIRECTION ( 'NONE',  ( 0.8090169943749422332, 0.5877852522924802425, 0.000000000000000000 ) ) ;
#59927 = CARTESIAN_POINT ( 'NONE',  ( -156.9232798886536386, 72.10386843399170687, -16.62516299996477898 ) ) ;
#59928 = CARTESIAN_POINT ( 'NONE',  ( 15.55634918610411610, 46.66904755831205875, 2.000000000000001776 ) ) ;
#59929 = EDGE_CURVE ( 'NONE', #15307, #38832, #41795, .T. ) ;
#59930 = CARTESIAN_POINT ( 'NONE',  ( 63.01563776193090405, 12.67277567978497643, -8.876140241706053757 ) ) ;
#59931 = EDGE_CURVE ( 'NONE', #47060, #9181, #14710, .T. ) ;
#59932 = CARTESIAN_POINT ( 'NONE',  ( -37.07086358537074489, 10.58360809068250141, 69.53818740131970344 ) ) ;
#59933 = CARTESIAN_POINT ( 'NONE',  ( 9.850262805259839993, 188.0000000000000000, -1.724042536399416070 ) ) ;
#59934 = ORIENTED_EDGE ( 'NONE', *, *, #48505, .T. ) ;
#59935 = DIRECTION ( 'NONE',  ( -0.000000000000000000, -0.000000000000000000, 1.000000000000000000 ) ) ;
#59936 = CARTESIAN_POINT ( 'NONE',  ( -156.6692143066620133, 70.50016761530883969, 62.82118311751774797 ) ) ;
#59937 = CARTESIAN_POINT ( 'NONE',  ( 0.000000000000000000, 0.000000000000000000, 0.000000000000000000 ) ) ;
#59938 = CARTESIAN_POINT ( 'NONE',  ( -52.73319225379862019, -53.34578647582125654, 170.0000000000000000 ) ) ;
#59939 = DIRECTION ( 'NONE',  ( -0.9009688679024218105, 0.4338837391175525693, 0.000000000000000000 ) ) ;
#59940 = DIRECTION ( 'NONE',  ( 1.000000000000000000, -0.000000000000000000, 0.000000000000000000 ) ) ;
#59941 = FACE_OUTER_BOUND ( 'NONE', #48368, .T. ) ;
#59942 = CARTESIAN_POINT ( 'NONE',  ( 20.74093720376649586, 6.709541214524347374, 58.70593033936504668 ) ) ;
#59943 = CARTESIAN_POINT ( 'NONE',  ( -190.0891074294818566, 108.2702128816165583, 88.58129052767998246 ) ) ;
#59944 = CARTESIAN_POINT ( 'NONE',  ( 10.83418588031599228, 6.392467435475928994, -75.51611801531713297 ) ) ;
#59945 =( GEOMETRIC_REPRESENTATION_CONTEXT ( 3 ) GLOBAL_UNCERTAINTY_ASSIGNED_CONTEXT ( ( #55005 ) ) GLOBAL_UNIT_ASSIGNED_CONTEXT ( ( #55200, #28475, #1394 ) ) REPRESENTATION_CONTEXT ( 'NONE', 'WORKASPACE' ) );
#59946 = EDGE_CURVE ( 'NONE', #17554, #60122, #4747, .T. ) ;
#59947 = ORIENTED_EDGE ( 'NONE', *, *, #13214, .F. ) ;
#59949 = CARTESIAN_POINT ( 'NONE',  ( -42.36049017605959932, 61.90437280228238137, 170.0000000000000000 ) ) ;
#59948 = CIRCLE ( 'NONE', #56605, 10.00000000000000178 ) ;
#59950 = CARTESIAN_POINT ( 'NONE',  ( -133.3149301983942507, 51.57857650535020611, -68.13965555861794599 ) ) ;
#59951 = DIRECTION ( 'NONE',  ( -0.000000000000000000, -0.000000000000000000, -1.000000000000000000 ) ) ;
#59952 = LINE ( 'NONE', #1226, #52574 ) ;
#59953 = CARTESIAN_POINT ( 'NONE',  ( 59.29474530993687864, 12.86968658439548463, -63.54875636054207888 ) ) ;
#59954 = ORIENTED_EDGE ( 'NONE', *, *, #57128, .T. ) ;
#59955 = VECTOR ( 'NONE', #68276, 1000.000000000000000 ) ;
#59956 = ORIENTED_EDGE ( 'NONE', *, *, #30331, .T. ) ;
#59957 = CARTESIAN_POINT ( 'NONE',  ( -131.8293781841207988, 50.52790876176725021, -91.49601856444540715 ) ) ;
#59958 = AXIS2_PLACEMENT_3D ( 'NONE', #16954, #17672, #49309 ) ;
#59959 = CARTESIAN_POINT ( 'NONE',  ( 187.0823097343935331, 84.88801889414973800, 94.99999999999866418 ) ) ;
#59960 = VERTEX_POINT ( 'NONE', #49117 ) ;
#59961 = ORIENTED_EDGE ( 'NONE', *, *, #46855, .T. ) ;
#59962 = AXIS2_PLACEMENT_3D ( 'NONE', #44584, #7302, #66064 ) ;
#59963 = CARTESIAN_POINT ( 'NONE',  ( 177.5945652320814645, 75.14951358071817822, -37.08239668887548390 ) ) ;
#59964 = DIRECTION ( 'NONE',  ( -1.000000000000000000, 0.000000000000000000, 0.000000000000000000 ) ) ;
#59965 = ORIENTED_EDGE ( 'NONE', *, *, #44150, .F. ) ;
#59966 = CARTESIAN_POINT ( 'NONE',  ( 0.000000000000000000, 0.000000000000000000, 41.38025477438755928 ) ) ;
#59967 = CARTESIAN_POINT ( 'NONE',  ( 141.3586046882815879, 47.34625111366352712, 63.34599527006825070 ) ) ;
#59968 = CARTESIAN_POINT ( 'NONE',  ( -71.43874587651170316, 19.69883891272894871, -44.63390031017252824 ) ) ;
#59969 = VECTOR ( 'NONE', #55181, 1000.000000000000000 ) ;
#59970 = CARTESIAN_POINT ( 'NONE',  ( 79.51684382776136317, 17.11558840174940954, -94.59398989896673982 ) ) ;
#59971 = DIRECTION ( 'NONE',  ( -3.417256381633830033E-15, -1.000000000000000000, -5.551115123125782702E-17 ) ) ;
#59972 = CARTESIAN_POINT ( 'NONE',  ( -190.3061188229048923, 108.5745819235681608, 42.30307631859309225 ) ) ;
#59973 = ORIENTED_EDGE ( 'NONE', *, *, #49305, .T. ) ;
#59974 =( BOUNDED_CURVE ( )  B_SPLINE_CURVE ( 3, ( #10876, #32346, #678, #27048 ),
 .UNSPECIFIED., .F., .T. ) 
 B_SPLINE_CURVE_WITH_KNOTS ( ( 4, 4 ),
 ( -8.881784197001252323E-16, 1.570796326794896336 ),
 .UNSPECIFIED. ) 
 CURVE ( )  GEOMETRIC_REPRESENTATION_ITEM ( )  RATIONAL_B_SPLINE_CURVE ( ( 1.000000000000000000, 0.8047378541243649375, 0.8047378541243649375, 1.000000000000000000 ) ) 
 REPRESENTATION_ITEM ( '' )  );
#59975 = CARTESIAN_POINT ( 'NONE',  ( -2.645453300864630819E-14, -10.55634918610403439, 85.00100000000000477 ) ) ;
#59976 = FACE_BOUND ( 'NONE', #66897, .T. ) ;
#59977 = LINE ( 'NONE', #48715, #11310 ) ;
#59978 = LINE ( 'NONE', #22358, #61242 ) ;
#59980 = ORIENTED_EDGE ( 'NONE', *, *, #22370, .F. ) ;
#59979 = CARTESIAN_POINT ( 'NONE',  ( -133.0156404686407825, 51.36557667666784965, 89.43440121892608374 ) ) ;
#59981 = CARTESIAN_POINT ( 'NONE',  ( 56.28782924480457694, 12.23883190161851076, 13.82014511301142967 ) ) ;
#59982 = ORIENTED_EDGE ( 'NONE', *, *, #36767, .T. ) ;
#59984 = EDGE_CURVE ( 'NONE', #21979, #59267, #26985, .T. ) ;
#59983 = CARTESIAN_POINT ( 'NONE',  ( -132.4951995226844872, 50.99687809989497111, 34.55095761923556097 ) ) ;
#59985 = CARTESIAN_POINT ( 'NONE',  ( 39.54205320694339321, 51.58901073076764021, 40.00000000000003553 ) ) ;
#59986 = LINE ( 'NONE', #41838, #26471 ) ;
#59987 = CARTESIAN_POINT ( 'NONE',  ( 309.8720357909272707, 18.00000000000002842, 536.6193948016162949 ) ) ;
#59988 = CARTESIAN_POINT ( 'NONE',  ( 79.22946426532584496, 17.02750615740071183, -17.72431334350951104 ) ) ;
#59989 = CARTESIAN_POINT ( 'NONE',  ( 311.9975424824652350, 20.00000000000003197, 256.6193948016162381 ) ) ;
#59990 = CARTESIAN_POINT ( 'NONE',  ( 93.92910382125423041, 22.04227458821881669, -68.42647781650052252 ) ) ;
#59991 = AXIS2_PLACEMENT_3D ( 'NONE', #46239, #5317, #14920 ) ;
#59992 = CARTESIAN_POINT ( 'NONE',  ( -24.61452482346733461, 8.570300138934635825, -93.36648426586947380 ) ) ;
#59993 = LINE ( 'NONE', #39260, #45275 ) ;
#59994 = ORIENTED_EDGE ( 'NONE', *, *, #31787, .F. ) ;
#59995 = ORIENTED_EDGE ( 'NONE', *, *, #12473, .F. ) ;
#59996 = MECHANICAL_DESIGN_GEOMETRIC_PRESENTATION_REPRESENTATION (  '', ( #47488 ), #1618 ) ;
#59997 = CARTESIAN_POINT ( 'NONE',  ( 107.3013380801408658, 388.0000000000065938, -128.9497041420121093 ) ) ;
#59998 = DIRECTION ( 'NONE',  ( 0.000000000000000000, 0.000000000000000000, 1.000000000000000000 ) ) ;
#59999 = DIRECTION ( 'NONE',  ( 0.1342332658176522697, 0.9909497617679352555, 0.000000000000000000 ) ) ;
#60000 = CARTESIAN_POINT ( 'NONE',  ( 0.000000000000000000, 0.000000000000000000, 40.00000000000003553 ) ) ;
#60001 = VECTOR ( 'NONE', #42048, 1000.000000000000114 ) ;
#60002 = CARTESIAN_POINT ( 'NONE',  ( 211.5034924207027984, 118.0100795718635140, -40.66011177504395135 ) ) ;
#60003 = DIRECTION ( 'NONE',  ( -0.000000000000000000, -0.000000000000000000, -1.000000000000000000 ) ) ;
#60004 = DIRECTION ( 'NONE',  ( -1.000000000000000000, 0.000000000000000000, 0.000000000000000000 ) ) ;
#60005 = AXIS2_PLACEMENT_3D ( 'NONE', #4575, #26040, #47471 ) ;
#60006 = CARTESIAN_POINT ( 'NONE',  ( 44.34362023773823580, 10.12115849931653599, -48.78329502920555427 ) ) ;
#60007 = CARTESIAN_POINT ( 'NONE',  ( 159.6593397521790507, 59.37286298965128140, -77.65605731442671811 ) ) ;
#60008 = ORIENTED_EDGE ( 'NONE', *, *, #38854, .T. ) ;
#60010 = CARTESIAN_POINT ( 'NONE',  ( -29.04400972079232446, 10.22852224114067354, 17.98340990312981802 ) ) ;
#60009 = VECTOR ( 'NONE', #52198, 999.9999999999998863 ) ;
#60011 = EDGE_CURVE ( 'NONE', #46836, #57348, #33377, .T. ) ;
#60012 = ORIENTED_EDGE ( 'NONE', *, *, #68379, .T. ) ;
#60013 = DIRECTION ( 'NONE',  ( -1.000000000000000000, 0.000000000000000000, 0.000000000000000000 ) ) ;
#60014 = AXIS2_PLACEMENT_3D ( 'NONE', #65981, #60680, #37833 ) ;
#60015 = CARTESIAN_POINT ( 'NONE',  ( -85.89966968015255588, 25.20990842792081565, 89.59847398112991357 ) ) ;
#60016 = CARTESIAN_POINT ( 'NONE',  ( 93.08174259058945665, 22.79847752828721141, 67.91146075705054841 ) ) ;
#60017 = CARTESIAN_POINT ( 'NONE',  ( 126.3732561463888118, 38.23795180971327312, 36.44577969812711160 ) ) ;
#60018 = CARTESIAN_POINT ( 'NONE',  ( 32.66364305947235636, 8.639871491745251930, 13.89929584829961229 ) ) ;
#60019 = LINE ( 'NONE', #11478, #12110 ) ;
#60020 = EDGE_CURVE ( 'NONE', #16987, #39848, #40017, .T. ) ;
#60021 = CARTESIAN_POINT ( 'NONE',  ( -19.15041341282721632, 47.98507848106410734, 26.66469104408690072 ) ) ;
#60022 = CARTESIAN_POINT ( 'NONE',  ( -20.55634918610396866, 31.11269837220809009, 85.00100000000000477 ) ) ;
#60023 = CARTESIAN_POINT ( 'NONE',  ( 211.6713973331038687, 116.4246122071819229, 87.60636827412143646 ) ) ;
#60024 = DIRECTION ( 'NONE',  ( 0.000000000000000000, 0.000000000000000000, -1.000000000000000000 ) ) ;
#60025 = EDGE_LOOP ( 'NONE', ( #41156, #63122, #21792, #19676 ) ) ;
#60026 = DIRECTION ( 'NONE',  ( -1.000000000000000000, 0.000000000000000000, 0.000000000000000000 ) ) ;
#60027 = CARTESIAN_POINT ( 'NONE',  ( 0.000000000000000000, 35.26862320190615208, -5.000000000000000000 ) ) ;
#60028 = PLANE ( 'NONE',  #52236 ) ;
#60029 = CARTESIAN_POINT ( 'NONE',  ( 410.0000000000000000, 0.000000000000000000, 380.0000000000000000 ) ) ;
#60030 = DIRECTION ( 'NONE',  ( -0.000000000000000000, -0.000000000000000000, -1.000000000000000000 ) ) ;
#60031 = CARTESIAN_POINT ( 'NONE',  ( 39.71871809564405709, -33.04132994422423764, 26.66469066592269854 ) ) ;
#60032 = CARTESIAN_POINT ( 'NONE',  ( 79.53788081641260987, 18.17489638840366695, 88.43542930566641758 ) ) ;
#60033 = EDGE_CURVE ( 'NONE', #32423, #34252, #49824, .T. ) ;
#60034 = ORIENTED_EDGE ( 'NONE', *, *, #61614, .T. ) ;
#60035 = DIRECTION ( 'NONE',  ( 0.002336510515849693232, -0.005156670592098671659, -0.9999839746051002454 ) ) ;
#60036 = CARTESIAN_POINT ( 'NONE',  ( -190.4966031023458584, 108.8421921967458701, -11.08920354847794876 ) ) ;
#60038 = EDGE_CURVE ( 'NONE', #3538, #52894, #28026, .T. ) ;
#60037 = CARTESIAN_POINT ( 'NONE',  ( -128.9786047358386440, 48.55852351614670681, 18.11557624711077352 ) ) ;
#60039 = CARTESIAN_POINT ( 'NONE',  ( -173.1211646369891355, 88.63826465341151106, -49.71195716475001092 ) ) ;
#60040 = CARTESIAN_POINT ( 'NONE',  ( -132.5976199670998597, 52.30296609017644016, -45.78660264953770564 ) ) ;
#60041 = ORIENTED_EDGE ( 'NONE', *, *, #16200, .F. ) ;
#60042 = CARTESIAN_POINT ( 'NONE',  ( -124.1094910780272329, 45.33021696310841975, -49.70193067791534958 ) ) ;
#60043 = DIRECTION ( 'NONE',  ( 0.000000000000000000, 0.000000000000000000, 1.000000000000000000 ) ) ;
#60044 = CARTESIAN_POINT ( 'NONE',  ( -146.1260528621668300, 61.36307454672305539, -22.17874663354146492 ) ) ;
#60045 = LINE ( 'NONE', #11867, #57373 ) ;
#60046 = CIRCLE ( 'NONE', #66821, 4.999999999999997335 ) ;
#60047 = CARTESIAN_POINT ( 'NONE',  ( -12.50000000000002842, 207.5000000000000284, 0.000000000000000000 ) ) ;
#60048 = ORIENTED_EDGE ( 'NONE', *, *, #23752, .F. ) ;
#60049 = CARTESIAN_POINT ( 'NONE',  ( 427.4999999999999432, 207.5000000000000284, 380.0000000000000000 ) ) ;
#60050 = CARTESIAN_POINT ( 'NONE',  ( 197.1980152960110217, 96.59350208824301376, -43.48860924640160874 ) ) ;
#60051 = CARTESIAN_POINT ( 'NONE',  ( -152.2873556200145515, 67.91256772393730046, 31.25152339806742319 ) ) ;
#60052 = CARTESIAN_POINT ( 'NONE',  ( 17.72992212664810907, 6.570588738776105941, -50.26741213039321821 ) ) ;
#60053 = VECTOR ( 'NONE', #58553, 1000.000000000000000 ) ;
#60055 = ORIENTED_EDGE ( 'NONE', *, *, #60568, .F. ) ;
#60054 = CARTESIAN_POINT ( 'NONE',  ( 115.0485321076020568, 32.28990710985445389, 16.04577514241892899 ) ) ;
#60056 = AXIS2_PLACEMENT_3D ( 'NONE', #69198, #53353, #65319 ) ;
#60057 = CARTESIAN_POINT ( 'NONE',  ( -31.11269837220806878, 5.000000000000056843, 0.000000000000000000 ) ) ;
#60058 = VECTOR ( 'NONE', #57228, 1000.000000000000000 ) ;
#60059 = ORIENTED_EDGE ( 'NONE', *, *, #61052, .T. ) ;
#60060 = VERTEX_POINT ( 'NONE', #33327 ) ;
#60061 = CARTESIAN_POINT ( 'NONE',  ( -119.9387902904519763, 42.69579278498642338, -91.52063911540987817 ) ) ;
#60062 = AXIS2_PLACEMENT_3D ( 'NONE', #10760, #53307, #38534 ) ;
#60063 = DIRECTION ( 'NONE',  ( 1.000000000000000000, 0.000000000000000000, 0.000000000000000000 ) ) ;
#60065 = EDGE_LOOP ( 'NONE', ( #12955, #23655, #45445, #34688 ) ) ;
#60064 = CARTESIAN_POINT ( 'NONE',  ( -14.33576511807126863, 8.413127487936190363, -66.00693546820657787 ) ) ;
#60066 = CARTESIAN_POINT ( 'NONE',  ( 160.9069879467680835, 60.37290772564308128, 30.22702203457957992 ) ) ;
#60067 = CARTESIAN_POINT ( 'NONE',  ( 8.000000000000007105, 249.8719672152120381, 94.99999999999866418 ) ) ;
#60068 = LINE ( 'NONE', #54795, #30608 ) ;
#60069 = EDGE_LOOP ( 'NONE', ( #63297, #25306, #40599, #64712 ) ) ;
#60070 = VECTOR ( 'NONE', #45321, 1000.000000000000000 ) ;
#60071 = EDGE_CURVE ( 'NONE', #37589, #5460, #29089, .T. ) ;
#60072 = LINE ( 'NONE', #12251, #49051 ) ;
#60073 = ADVANCED_FACE ( 'NONE', ( #28377 ), #12916, .F. ) ;
#60074 = CARTESIAN_POINT ( 'NONE',  ( -119.1064753703575718, 42.18441154001784099, 94.99999999999866418 ) ) ;
#60075 = CARTESIAN_POINT ( 'NONE',  ( -180.6021503146988891, 97.45669259943416307, 38.94198014546275033 ) ) ;
#60076 = CARTESIAN_POINT ( 'NONE',  ( -35.99432170610151616, 10.38324794858010591, -75.63980193136818286 ) ) ;
#60077 = CARTESIAN_POINT ( 'NONE',  ( 22.28556289340099283, 7.803548444155005370, 60.60479519626248646 ) ) ;
#60078 = ORIENTED_EDGE ( 'NONE', *, *, #48, .T. ) ;
#60079 = ORIENTED_EDGE ( 'NONE', *, *, #34403, .T. ) ;
#60080 = ORIENTED_EDGE ( 'NONE', *, *, #7053, .F. ) ;
#60081 = LINE ( 'NONE', #50241, #66575 ) ;
#60082 = CARTESIAN_POINT ( 'NONE',  ( -103.8932886509196436, 34.74144483217662582, 3.846358069395087398 ) ) ;
#60083 = DIRECTION ( 'NONE',  ( 1.232595164407830946E-32, 1.000000000000000000, -1.479221584281239571E-31 ) ) ;
#60084 = CARTESIAN_POINT ( 'NONE',  ( -37.38781680082738035, 10.64362327909143069, -47.41097133852251488 ) ) ;
#60085 = CARTESIAN_POINT ( 'NONE',  ( -95.54114085644955878, 29.48728305236672398, 94.99999999999866418 ) ) ;
#60086 = CARTESIAN_POINT ( 'NONE',  ( 10.61438981621043531, -5.226566692248933776, 4.385610183789550476 ) ) ;
#60087 = ADVANCED_FACE ( 'NONE', ( #6579 ), #12208, .F. ) ;
#60088 = DIRECTION ( 'NONE',  ( -1.000000000000000000, 0.000000000000000000, 0.000000000000000000 ) ) ;
#60089 = CARTESIAN_POINT ( 'NONE',  ( -74.20136529587826146, 21.74007521413449240, -9.739908195685467618 ) ) ;
#60090 = CARTESIAN_POINT ( 'NONE',  ( 86.62931800182293784, 19.42108912189596381, 56.55663816294300261 ) ) ;
#60091 = EDGE_CURVE ( 'NONE', #8669, #15418, #55818, .T. ) ;
#60092 = VERTEX_POINT ( 'NONE', #18181 ) ;
#60093 = CIRCLE ( 'NONE', #9606, 65.36598343705435354 ) ;
#60094 = CARTESIAN_POINT ( 'NONE',  ( -99.40451658125527956, 32.46531518262781901, -89.26390591963935606 ) ) ;
#60095 = CARTESIAN_POINT ( 'NONE',  ( -7.329206686002009974E-14, -46.66904755831211560, 0.000000000000000000 ) ) ;
#60096 = CARTESIAN_POINT ( 'NONE',  ( 212.1535111375855251, 117.1635556319084941, -69.83956656682167363 ) ) ;
#60097 = EDGE_CURVE ( 'NONE', #1003, #56426, #9662, .T. ) ;
#60098 = DIRECTION ( 'NONE',  ( 1.000000000000000000, 0.000000000000000000, 0.000000000000000000 ) ) ;
#60099 = LINE ( 'NONE', #33032, #41678 ) ;
#60100 = DIRECTION ( 'NONE',  ( -0.000000000000000000, -0.000000000000000000, 1.000000000000000000 ) ) ;
#60101 = LINE ( 'NONE', #28096, #41231 ) ;
#60102 = ADVANCED_FACE ( 'NONE', ( #55455 ), #61089, .T. ) ;
#60104 = EDGE_CURVE ( 'NONE', #26499, #40777, #23469, .T. ) ;
#60103 = CARTESIAN_POINT ( 'NONE',  ( 0.4988340113715870050, 3.871605243926952156, -8.000000000000001776 ) ) ;
#60106 = CARTESIAN_POINT ( 'NONE',  ( -63.73419499958998813, 12.83646726144834993, 170.0000000000000000 ) ) ;
#60105 = CONICAL_SURFACE ( 'NONE', #57910, 4.174999999999999822, 0.9599310885968758145 ) ;
#60107 = CIRCLE ( 'NONE', #5079, 91.99999999999997158 ) ;
#60108 = ORIENTED_EDGE ( 'NONE', *, *, #68466, .T. ) ;
#60109 = DIRECTION ( 'NONE',  ( -0.000000000000000000, -0.000000000000000000, -1.000000000000000000 ) ) ;
#60110 = DIRECTION ( 'NONE',  ( -0.000000000000000000, -0.000000000000000000, 1.000000000000000000 ) ) ;
#60111 = ORIENTED_EDGE ( 'NONE', *, *, #62722, .T. ) ;
#60112 = CARTESIAN_POINT ( 'NONE',  ( 15.78827728214693416, -170.0000000000000000, 71.85925826316895382 ) ) ;
#60113 = ORIENTED_EDGE ( 'NONE', *, *, #20966, .T. ) ;
#60114 = CARTESIAN_POINT ( 'NONE',  ( -83.52505811737952968, 24.23179517241433700, 32.18346549745763241 ) ) ;
#60115 = AXIS2_PLACEMENT_3D ( 'NONE', #9732, #27268, #58583 ) ;
#60116 = CARTESIAN_POINT ( 'NONE',  ( -24.71604178686819964, 9.599501655372948861, -72.99519987063204951 ) ) ;
#60117 = CARTESIAN_POINT ( 'NONE',  ( 46.12611922993085756, 10.39838587005582404, 34.08266634447561927 ) ) ;
#60118 = VECTOR ( 'NONE', #45739, 1000.000000000000114 ) ;
#60119 = CARTESIAN_POINT ( 'NONE',  ( -142.3178993725749137, 58.31327888234797285, 13.58478421935505409 ) ) ;
#60120 = B_SPLINE_CURVE_WITH_KNOTS ( 'NONE', 3,
 ( #9524, #20412, #26394, #47142 ),
 .UNSPECIFIED., .F., .F.,
 ( 4, 4 ),
 ( 0.1259919275528359750, 0.1829744153748750768 ),
 .UNSPECIFIED. ) ;
#60121 = EDGE_CURVE ( 'NONE', #41030, #30857, #2356, .T. ) ;
#60122 = VERTEX_POINT ( 'NONE', #66733 ) ;
#60123 = EDGE_LOOP ( 'NONE', ( #21155, #63542, #12287 ) ) ;
#60124 = ADVANCED_FACE ( 'NONE', ( #18528 ), #34716, .F. ) ;
#60125 = ADVANCED_FACE ( 'NONE', ( #24845 ), #68110, .T. ) ;
#60126 = EDGE_CURVE ( 'NONE', #32549, #20980, #24083, .T. ) ;
#60127 = FACE_OUTER_BOUND ( 'NONE', #28066, .T. ) ;
#60128 = ORIENTED_EDGE ( 'NONE', *, *, #7043, .T. ) ;
#60129 = CARTESIAN_POINT ( 'NONE',  ( 70.65683382808195745, 25.18281821780106711, 170.0000000000000000 ) ) ;
#60130 = PLANE ( 'NONE',  #16970 ) ;
#60132 = CARTESIAN_POINT ( 'NONE',  ( -7.825402957745085430, 7.899365992529246761, 18.27103044898354511 ) ) ;
#60131 = B_SPLINE_CURVE_WITH_KNOTS ( 'NONE', 3,
 ( #51801, #61998, #56380, #20133, #18756, #41586, #35279, #56736, #63044, #40212, #30004, #8896, #8201, #46513, #3609, #7859, #29307, #50758, #61660, #29652, #19790, #62709, #14510, #32421, #16577, #15551, #59130, #4640, #31720, #37683, #21174, #4986, #64075, #53847, #64771, #5665, #21504, #31044, #63397, #47889, #9584, #10601, #63743, #58113, #21852, #26452 ),
 .UNSPECIFIED., .F., .F.,
 ( 4, 2, 2, 2, 2, 2, 2, 2, 2, 2, 2, 2, 2, 2, 2, 2, 2, 2, 2, 2, 2, 2, 4 ),
 ( 0.02420077021543440635, 0.02572112563160185161, 0.02648130333968559333, 0.02724148104776933851, 0.02876183646393682541, 0.02952201417202056713, 0.03028219188010430885, 0.03180254729627179228, 0.03332290271243927571, 0.03408308042052300008, 0.03484325812860672444, 0.03636361354477421481, 0.03712379125285794612, 0.03788396896094166355, 0.03864414666902539486, 0.03940432437710911923, 0.04092467979327658878, 0.04244503520944406527, 0.04396539062561152789, 0.04548574604177900438, 0.04624592374986273569, 0.04700610145794646699, 0.04852645687411388797 ),
 .UNSPECIFIED. ) ;
#60133 = CARTESIAN_POINT ( 'NONE',  ( 141.0652542208218847, 47.15334271457688686, 92.80065851230959595 ) ) ;
#60134 = PLANE ( 'NONE',  #54927 ) ;
#60135 = FACE_OUTER_BOUND ( 'NONE', #30742, .T. ) ;
#60136 = ORIENTED_EDGE ( 'NONE', *, *, #15956, .F. ) ;
#60137 = CARTESIAN_POINT ( 'NONE',  ( -123.6699087229882110, 45.04696784753415528, -76.42458631566876193 ) ) ;
#60138 = ORIENTED_EDGE ( 'NONE', *, *, #44777, .T. ) ;
#60139 = ORIENTED_EDGE ( 'NONE', *, *, #62686, .F. ) ;
#60140 = CARTESIAN_POINT ( 'NONE',  ( -5.000000000000000888, 6.123233995736767268E-16, -9.500000000000000000 ) ) ;
#60141 = CARTESIAN_POINT ( 'NONE',  ( 12.99074365121421692, 21.50298515537768296, 0.000000000000000000 ) ) ;
#60142 = LINE ( 'NONE', #11959, #11661 ) ;
#60143 = CARTESIAN_POINT ( 'NONE',  ( 134.3172730033262781, 41.70277427218488953, -62.86786152285933582 ) ) ;
#60144 = CARTESIAN_POINT ( 'NONE',  ( -36.53690438256411710, 73.43472186181504924, 73.58025477438756923 ) ) ;
#60145 = ORIENTED_EDGE ( 'NONE', *, *, #62889, .T. ) ;
#60146 = CARTESIAN_POINT ( 'NONE',  ( -36.11269837220812207, -31.11269837220801193, 85.00100000000000477 ) ) ;
#60147 = ORIENTED_EDGE ( 'NONE', *, *, #23029, .F. ) ;
#60148 = LINE ( 'NONE', #33440, #21644 ) ;
#60149 = EDGE_LOOP ( 'NONE', ( #25351, #49861 ) ) ;
#60150 = VECTOR ( 'NONE', #35013, 1000.000000000000000 ) ;
#60151 = CARTESIAN_POINT ( 'NONE',  ( 126.6904219525097659, 37.26255867422720058, -95.00000000000133582 ) ) ;
#60152 = VECTOR ( 'NONE', #5932, 1000.000000000000000 ) ;
#60153 = EDGE_LOOP ( 'NONE', ( #47538, #22962, #27198, #16217, #67561 ) ) ;
#60154 = CARTESIAN_POINT ( 'NONE',  ( -144.2188519266539970, 59.82027639618912218, -74.48106321738612223 ) ) ;
#60155 = CARTESIAN_POINT ( 'NONE',  ( 5.694488332793534724, 51.35054872415687299, 26.66469066592269499 ) ) ;
#60156 = LINE ( 'NONE', #16894, #47409 ) ;
#60157 = TOROIDAL_SURFACE ( 'NONE', #43325, 20.30000000000000071, 0.3000000000000062061 ) ;
#60158 = ORIENTED_EDGE ( 'NONE', *, *, #55486, .F. ) ;
#60159 = DIRECTION ( 'NONE',  ( -0.000000000000000000, 0.000000000000000000, -1.000000000000000000 ) ) ;
#60160 = SURFACE_STYLE_USAGE ( .BOTH. , #5314 ) ;
#60161 = EDGE_CURVE ( 'NONE', #42757, #52890, #40665, .T. ) ;
#60162 = CARTESIAN_POINT ( 'NONE',  ( 32.37980458033285913, 8.611076697115702672, 40.05964868220856090 ) ) ;
#60163 = VECTOR ( 'NONE', #57345, 1000.000000000000000 ) ;
#60164 = CARTESIAN_POINT ( 'NONE',  ( -175.9864315813574649, 91.91454246454362931, -49.15589249871932509 ) ) ;
#60165 = CARTESIAN_POINT ( 'NONE',  ( -68.11501976657858393, 31.41506934893840963, 43.58025477438756923 ) ) ;
#60166 = DIRECTION ( 'NONE',  ( -1.000000000000000000, 0.000000000000000000, 0.000000000000000000 ) ) ;
#60167 = DIRECTION ( 'NONE',  ( -4.270088556250601699E-16, -0.000000000000000000, -1.000000000000000000 ) ) ;
#60168 = ORIENTED_EDGE ( 'NONE', *, *, #6455, .F. ) ;
#60169 = CARTESIAN_POINT ( 'NONE',  ( -440.1146514826276643, 395.0000000000064801, -133.9016337311479958 ) ) ;
#60170 = CARTESIAN_POINT ( 'NONE',  ( -144.2038301586456726, 61.09856042007390897, -74.48259089573751623 ) ) ;
#60171 = VERTEX_POINT ( 'NONE', #56858 ) ;
#60172 = FACE_BOUND ( 'NONE', #19330, .T. ) ;
#60173 = CARTESIAN_POINT ( 'NONE',  ( -0.3734056954813064766, 6.520221844775929476, -68.78453539205794698 ) ) ;
#60174 = CARTESIAN_POINT ( 'NONE',  ( -180.5200658187031593, 97.35517482626556784, 63.89930464416294598 ) ) ;
#60175 = DIRECTION ( 'NONE',  ( -0.7071067811865473507, 6.441404958702665783E-16, 0.7071067811865477948 ) ) ;
#60176 = FACE_OUTER_BOUND ( 'NONE', #24617, .T. ) ;
#60177 = CARTESIAN_POINT ( 'NONE',  ( 15.68296563925591514, -63.09411298019745828, 43.58025477438756923 ) ) ;
#60178 = DIRECTION ( 'NONE',  ( 0.000000000000000000, -1.000000000000000000, 0.000000000000000000 ) ) ;
#60179 = CARTESIAN_POINT ( 'NONE',  ( 114.4933711091048281, 21.89007574053286120, 2.217281872662919540 ) ) ;
#60180 = EDGE_CURVE ( 'NONE', #12136, #7089, #20249, .T. ) ;
#60181 = CARTESIAN_POINT ( 'NONE',  ( -76.98209973255083582, 21.68691446935567058, -88.98387085312982947 ) ) ;
#60182 = ADVANCED_FACE ( 'NONE', ( #46983 ), #35398, .F. ) ;
#60183 = CARTESIAN_POINT ( 'NONE',  ( -15.27594996066617661, 8.502079791899644690, 36.62617975021709071 ) ) ;
#60185 = EDGE_CURVE ( 'NONE', #42033, #14102, #56496, .T. ) ;
#60184 = CARTESIAN_POINT ( 'NONE',  ( 115.2288739107204947, 31.25773204386717197, 4.658657091807949513 ) ) ;
#60186 = CARTESIAN_POINT ( 'NONE',  ( 93.08073375333748345, 22.79826000593201840, -20.31003796707942044 ) ) ;
#60187 = ORIENTED_EDGE ( 'NONE', *, *, #15500, .T. ) ;
#60188 = CARTESIAN_POINT ( 'NONE',  ( -38.93847286785603501, 11.96870349976817494, 10.36518148543439821 ) ) ;
#60189 = ORIENTED_EDGE ( 'NONE', *, *, #30279, .T. ) ;
#60190 = FACE_OUTER_BOUND ( 'NONE', #22499, .T. ) ;
#60191 = ADVANCED_FACE ( 'NONE', ( #20939 ), #63508, .T. ) ;
#60192 = CARTESIAN_POINT ( 'NONE',  ( 79.19119222799089641, 18.06817527909834808, -69.17202811480721891 ) ) ;
#60193 = CARTESIAN_POINT ( 'NONE',  ( 103.1614067554331342, 26.83495172254625061, 88.30558029229318606 ) ) ;
#60194 = PLANE ( 'NONE',  #58210 ) ;
#60195 = DIRECTION ( 'NONE',  ( -0.000000000000000000, -0.000000000000000000, -1.000000000000000000 ) ) ;
#60196 = CARTESIAN_POINT ( 'NONE',  ( -28.81071653159242274, 10.19258396314334725, -35.78856510997613327 ) ) ;
#60197 = DIRECTION ( 'NONE',  ( 0.9839295885986295565, 0.1785568947986370392, 0.000000000000000000 ) ) ;
#60198 = DIRECTION ( 'NONE',  ( -0.000000000000000000, 0.000000000000000000, 1.000000000000000000 ) ) ;
#60199 = CARTESIAN_POINT ( 'NONE',  ( -190.6985136298602015, 109.1272424661243434, -64.50448789838189612 ) ) ;
#60200 = EDGE_LOOP ( 'NONE', ( #62645, #842 ) ) ;
#60201 = ORIENTED_EDGE ( 'NONE', *, *, #56446, .T. ) ;
#60202 = CARTESIAN_POINT ( 'NONE',  ( 32.03384598935270589, 8.576372641736000446, 65.72151599203246519 ) ) ;
#60203 = CARTESIAN_POINT ( 'NONE',  ( 177.2011275744679608, 74.76848439756739140, 57.23258176878422887 ) ) ;
#60204 = CARTESIAN_POINT ( 'NONE',  ( 46.76173513940573656, -58.63736118510165340, 43.58025477438756212 ) ) ;
#60205 = VECTOR ( 'NONE', #3955, 1000.000000000000000 ) ;
#60206 = CARTESIAN_POINT ( 'NONE',  ( -166.3205068063721228, 81.30869308872868828, 61.99160270357487690 ) ) ;
#60207 = CARTESIAN_POINT ( 'NONE',  ( -167.4844853368929307, 82.52074065752739784, -20.32144448876292842 ) ) ;
#60208 = AXIS2_PLACEMENT_3D ( 'NONE', #65750, #59058, #37956 ) ;
#60209 = CARTESIAN_POINT ( 'NONE',  ( 181.0840389613909736, -170.0000000000000000, 2.464043515047718014 ) ) ;
#60210 = VERTEX_POINT ( 'NONE', #64189 ) ;
#60211 = ADVANCED_FACE ( 'NONE', ( #53276 ), #37711, .T. ) ;
#60212 = CARTESIAN_POINT ( 'NONE',  ( 106.6322547488295385, 28.34756922280616465, -50.01364319867063557 ) ) ;
#60213 = AXIS2_PLACEMENT_3D ( 'NONE', #16700, #10382, #37817 ) ;
#60214 = CIRCLE ( 'NONE', #40990, 195.0000000000000000 ) ;
#60215 = CARTESIAN_POINT ( 'NONE',  ( 185.1660960081723033, 84.30194217633003007, -23.17644693461118877 ) ) ;
#60216 = CARTESIAN_POINT ( 'NONE',  ( 10.83521140779424030, 7.398743030771586682, 58.70627392783954690 ) ) ;
#60217 = LINE ( 'NONE', #11322, #45312 ) ;
#60218 = CARTESIAN_POINT ( 'NONE',  ( 45.49006904354233427, 9.279592366778889101, -20.66221359758136344 ) ) ;
#60219 = CARTESIAN_POINT ( 'NONE',  ( -125.8938041572051389, 47.69968343338778283, -76.75825448869764500 ) ) ;
#60220 = FACE_BOUND ( 'NONE', #61916, .T. ) ;
#60221 = AXIS2_PLACEMENT_3D ( 'NONE', #23813, #24165, #50540 ) ;
#60222 = EDGE_CURVE ( 'NONE', #55351, #44519, #872, .T. ) ;
#60223 = CARTESIAN_POINT ( 'NONE',  ( -55.54058841405663571, 14.81234591756537711, -35.21632399845985617 ) ) ;
#60224 = AXIS2_PLACEMENT_3D ( 'NONE', #55678, #7509, #59545 ) ;
#60225 = CIRCLE ( 'NONE', #47862, 65.00000000000000000 ) ;
#60226 =( REPRESENTATION_RELATIONSHIP ('NONE','NONE', #40274, #64096 ) REPRESENTATION_RELATIONSHIP_WITH_TRANSFORMATION ( #62484 )SHAPE_REPRESENTATION_RELATIONSHIP( ) );
#60227 = ORIENTED_EDGE ( 'NONE', *, *, #54469, .T. ) ;
#60228 = DIRECTION ( 'NONE',  ( 1.000000000000000000, 0.000000000000000000, 0.000000000000000000 ) ) ;
#60229 = DIRECTION ( 'NONE',  ( -0.4738686624729966379, -0.8805955318567391110, 0.000000000000000000 ) ) ;
#60230 = CARTESIAN_POINT ( 'NONE',  ( -48.34250119710924309, 14.01879126850790058, 61.30265284070986809 ) ) ;
#60231 = CARTESIAN_POINT ( 'NONE',  ( -180.4651598106648294, 97.28730001475651079, 13.02874545039772336 ) ) ;
#60232 = CARTESIAN_POINT ( 'NONE',  ( 210.9608386442062624, 117.1762372255316222, 67.68640205245998231 ) ) ;
#60233 = CARTESIAN_POINT ( 'NONE',  ( 37.92109554537579896, -5.611248133931618476, 13.32819299319724493 ) ) ;
#60234 = ORIENTED_EDGE ( 'NONE', *, *, #14696, .T. ) ;
#60235 = CARTESIAN_POINT ( 'NONE',  ( 55.56474667084419394, 11.06706367715631423, 11.46101165398160582 ) ) ;
#60236 = DIRECTION ( 'NONE',  ( 1.000000000000000000, 0.000000000000000000, 0.000000000000000000 ) ) ;
#60237 = ORIENTED_EDGE ( 'NONE', *, *, #7557, .F. ) ;
#60238 = ORIENTED_EDGE ( 'NONE', *, *, #42196, .F. ) ;
#60239 = DIRECTION ( 'NONE',  ( 0.000000000000000000, 0.000000000000000000, -1.000000000000000000 ) ) ;
#60240 = CARTESIAN_POINT ( 'NONE',  ( -27.75784438064426141, -18.62216945641829469, 6.893343212288923993 ) ) ;
#60241 = CARTESIAN_POINT ( 'NONE',  ( 87.11239765416380010, 20.65008247340817960, -62.66611478937536361 ) ) ;
#60242 = ORIENTED_EDGE ( 'NONE', *, *, #6049, .F. ) ;
#60243 = B_SPLINE_CURVE_WITH_KNOTS ( 'NONE', 3,
 ( #50481, #1593, #7223, #23056, #44505, #38175, #65984, #17780, #17056, #12501, #22003, #1960, #33266, #64921, #6525, #16717, #59617, #11431, #38527, #59972, #57149, #35699 ),
 .UNSPECIFIED., .F., .F.,
 ( 4, 2, 2, 2, 2, 2, 2, 2, 2, 2, 4 ),
 ( 8.002322828458971877E-17, 0.001318139496345214351, 0.001977209244517765148, 0.002636278992690316379, 0.003954418489035409733, 0.005272557985380503520, 0.005931627733553051715, 0.006590697481725598175, 0.007908836978070736198, 0.009226976474415874221, 0.01054511597076101224 ),
 .UNSPECIFIED. ) ;
#60244 = ORIENTED_EDGE ( 'NONE', *, *, #64471, .F. ) ;
#60245 = DIRECTION ( 'NONE',  ( -1.000000000000000000, -0.000000000000000000, -0.000000000000000000 ) ) ;
#60246 = CARTESIAN_POINT ( 'NONE',  ( 0.000000000000000000, 0.000000000000000000, 0.000000000000000000 ) ) ;
#60247 = CARTESIAN_POINT ( 'NONE',  ( -156.1477286774993729, 71.38742644140633331, -65.66038772067875584 ) ) ;
#60248 = CARTESIAN_POINT ( 'NONE',  ( 68.63585058221465829, 15.08566240483131793, 5.477619919286003558 ) ) ;
#60249 = LINE ( 'NONE', #1161, #51152 ) ;
#60250 = PRODUCT_DEFINITION_SHAPE ( 'NONE', 'NONE',  #69579 ) ;
#60251 = CARTESIAN_POINT ( 'NONE',  ( -47.79955240516188297, 13.88975739862082470, -44.68859367444699160 ) ) ;
#60252 = VECTOR ( 'NONE', #29477, 1000.000000000000000 ) ;
#60253 = ADVANCED_FACE ( 'NONE', ( #42395 ), #52931, .T. ) ;
#60254 = CARTESIAN_POINT ( 'NONE',  ( -47.61402178322637013, 13.84598486314981436, 9.983978065502588706 ) ) ;
#60255 = CARTESIAN_POINT ( 'NONE',  ( -131.3096895243911320, 51.39228038925232056, -10.35808099536435556 ) ) ;
#60256 = B_SPLINE_CURVE_WITH_KNOTS ( 'NONE', 3,
 ( #15640, #37426, #58878, #65567, #6471, #21943, #33904, #59563, #28261, #33210, #65211, #64864, #32848, #6811, #22998, #43394, #38836, #23360, #49357, #49707, #16667, #1537, #44444, #65933 ),
 .UNSPECIFIED., .F., .F.,
 ( 4, 2, 2, 2, 2, 2, 2, 2, 2, 2, 2, 4 ),
 ( 0.000000000000000000, 0.001318322376542587935, 0.002636644753085175871, 0.003954967129627763589, 0.004614128317899063303, 0.005273289506170363017, 0.006591611882712936424, 0.007250773070984224862, 0.007909934259255513300, 0.009228256635798121402, 0.009887417824069429789, 0.01054657901234073818 ),
 .UNSPECIFIED. ) ;
#60257 = CARTESIAN_POINT ( 'NONE',  ( -153.2277253043372696, 68.74531066433421245, -89.48623125317686799 ) ) ;
#60258 = DIRECTION ( 'NONE',  ( -0.000000000000000000, -0.000000000000000000, -1.000000000000000000 ) ) ;
#60259 = CARTESIAN_POINT ( 'NONE',  ( -78.66644367742111399, -170.0000000000000000, 37.91820113967311556 ) ) ;
#60260 = AXIS2_PLACEMENT_3D ( 'NONE', #59071, #68272, #31329 ) ;
#60262 = ORIENTED_EDGE ( 'NONE', *, *, #57967, .F. ) ;
#60261 = CARTESIAN_POINT ( 'NONE',  ( 0.06809871960542744629, 7.710219529346611367, -2.645508037661881584 ) ) ;
#60263 = ORIENTED_EDGE ( 'NONE', *, *, #51380, .T. ) ;
#60264 = AXIS2_PLACEMENT_3D ( 'NONE', #24521, #30140, #14302 ) ;
#60265 = ORIENTED_EDGE ( 'NONE', *, *, #68894, .T. ) ;
#60266 = DIRECTION ( 'NONE',  ( 1.000000000000000000, 0.000000000000000000, 0.000000000000000000 ) ) ;
#60267 = CARTESIAN_POINT ( 'NONE',  ( -13.32397999418070178, 63.99361958670517225, 43.58025477438756212 ) ) ;
#60268 = CARTESIAN_POINT ( 'NONE',  ( -48.99162761293257518, 13.13973062091724131, -20.29604390856045626 ) ) ;
#60269 = CARTESIAN_POINT ( 'NONE',  ( 106.6192711434718348, 27.24117154335862168, -23.14876697959396168 ) ) ;
#60270 = LINE ( 'NONE', #14745, #1335 ) ;
#60271 = VECTOR ( 'NONE', #4828, 1000.000000000000000 ) ;
#60272 = EDGE_CURVE ( 'NONE', #24929, #38551, #37115, .T. ) ;
#60273 = CARTESIAN_POINT ( 'NONE',  ( -38.92718193365331558, 11.96647478777219398, 65.05036416477805972 ) ) ;
#60274 = CARTESIAN_POINT ( 'NONE',  ( 0.000000000000000000, 0.000000000000000000, -9.474599999999998801 ) ) ;
#60275 = CARTESIAN_POINT ( 'NONE',  ( -71.16770070143908811, 19.60548673929830699, -69.98478112900720305 ) ) ;
#60276 = CARTESIAN_POINT ( 'NONE',  ( 22.81270948571149404, 6.827178363529887939, -13.53470793533548999 ) ) ;
#60277 = VERTEX_POINT ( 'NONE', #53625 ) ;
#60278 = CARTESIAN_POINT ( 'NONE',  ( 0.000000000000000000, 35.26862320190615208, 5.000000000000000000 ) ) ;
#60279 = VERTEX_POINT ( 'NONE', #6133 ) ;
#60280 = EDGE_CURVE ( 'NONE', #6453, #31099, #1782, .T. ) ;
#60281 = ORIENTED_EDGE ( 'NONE', *, *, #66197, .T. ) ;
#60282 = EDGE_CURVE ( 'NONE', #47125, #13157, #26564, .T. ) ;
#60283 = CARTESIAN_POINT ( 'NONE',  ( -4.999999999999971578, 20.55634918610402906, 85.00100000000000477 ) ) ;
#60284 = FILL_AREA_STYLE ('',( #12097 ) ) ;
#60285 = CARTESIAN_POINT ( 'NONE',  ( -24.84040467973654742, 9.616437491640137836, 87.82595348829025284 ) ) ;
#60286 = CARTESIAN_POINT ( 'NONE',  ( -94.89192151156326815, 29.18342430963128109, -43.83071791538480255 ) ) ;
#60287 = CARTESIAN_POINT ( 'NONE',  ( 0.000000000000000000, 0.000000000000000000, -10.00000000000000000 ) ) ;
#60288 = CARTESIAN_POINT ( 'NONE',  ( 14.08810621383467421, 7.458732232275138152, -50.32784852290144784 ) ) ;
#60289 = CARTESIAN_POINT ( 'NONE',  ( 141.2361973397653685, 47.26569015399785911, -15.31408827969341502 ) ) ;
#60290 = VERTEX_POINT ( 'NONE', #48001 ) ;
#60291 = EDGE_LOOP ( 'NONE', ( #50145, #15647, #607, #49702 ) ) ;
#60292 = VERTEX_POINT ( 'NONE', #69464 ) ;
#60293 = LINE ( 'NONE', #6823, #5733 ) ;
#60294 = CARTESIAN_POINT ( 'NONE',  ( -156.7435307435793845, 71.93726016406967005, -17.46061737335302766 ) ) ;
#60295 = CARTESIAN_POINT ( 'NONE',  ( 36.99625334683020128, 8.108440754877207723, -77.08499119840222136 ) ) ;
#60296 = CARTESIAN_POINT ( 'NONE',  ( 56.19211641164836379, 11.19288081156168424, -19.49878541329645287 ) ) ;
#60297 = CARTESIAN_POINT ( 'NONE',  ( -51.35181696773305760, 13.72007042346227124, 31.27555066828208297 ) ) ;
#60298 = LINE ( 'NONE', #50782, #34033 ) ;
#60299 = ORIENTED_EDGE ( 'NONE', *, *, #19872, .T. ) ;
#60300 = DIRECTION ( 'NONE',  ( -0.000000000000000000, -0.000000000000000000, -1.000000000000000000 ) ) ;
#60301 = CARTESIAN_POINT ( 'NONE',  ( -155.7433525314459075, 69.65452735858370659, 69.24046085996992872 ) ) ;
#60302 = DIRECTION ( 'NONE',  ( 0.000000000000000000, 0.000000000000000000, 1.000000000000000000 ) ) ;
#60303 = CARTESIAN_POINT ( 'NONE',  ( -165.9992860119575084, 79.53569239468048124, 9.108083402024591990 ) ) ;
#60304 = CARTESIAN_POINT ( 'NONE',  ( -83.14462298835725562, 24.07775853418030820, -48.65102209861048976 ) ) ;
#60306 = EDGE_CURVE ( 'NONE', #12451, #11248, #13038, .T. ) ;
#60305 = FACE_OUTER_BOUND ( 'NONE', #45093, .T. ) ;
#60307 = CARTESIAN_POINT ( 'NONE',  ( 0.000000000000000000, 0.000000000000000000, 0.000000000000000000 ) ) ;
#60308 = VECTOR ( 'NONE', #50684, 1000.000000000000000 ) ;
#60309 = VERTEX_POINT ( 'NONE', #16000 ) ;
#60310 = AXIS2_PLACEMENT_3D ( 'NONE', #36514, #9786, #63595 ) ;
#60311 = DIRECTION ( 'NONE',  ( -0.8532989592251507549, 0.000000000000000000, 0.5214219847544545594 ) ) ;
#60312 = CARTESIAN_POINT ( 'NONE',  ( -131.7724154034330581, 50.48821165954356616, -64.59405240136965176 ) ) ;
#60313 = CARTESIAN_POINT ( 'NONE',  ( -156.3413281584584809, 71.56573911209629557, 94.99999999999866418 ) ) ;
#60314 = CARTESIAN_POINT ( 'NONE',  ( 45.02738683369920381, 9.207938468499232698, -74.93078921836432471 ) ) ;
#60315 = CARTESIAN_POINT ( 'NONE',  ( 61.08522853873727598, 13.26388801693373232, -62.80148345061859061 ) ) ;
#60316 = EDGE_LOOP ( 'NONE', ( #3541, #56962, #45994, #43851 ) ) ;
#60317 = VECTOR ( 'NONE', #19481, 1000.000000000000000 ) ;
#60318 = VECTOR ( 'NONE', #56063, 1000.000000000000000 ) ;
#60319 = ORIENTED_EDGE ( 'NONE', *, *, #44657, .T. ) ;
#60320 = CARTESIAN_POINT ( 'NONE',  ( 0.7145311798161616545, -4.618802153517262532, -8.000000000000001776 ) ) ;
#60321 = CARTESIAN_POINT ( 'NONE',  ( 184.2892190079700754, 81.90639475741072317, 83.71060938861219825 ) ) ;
#60322 = ORIENTED_EDGE ( 'NONE', *, *, #53111, .T. ) ;
#60323 = VECTOR ( 'NONE', #68484, 1000.000000000000000 ) ;
#60324 = ORIENTED_EDGE ( 'NONE', *, *, #42321, .F. ) ;
#60325 = CARTESIAN_POINT ( 'NONE',  ( 311.9975424824652350, 20.00000000000003197, 401.6295345748407613 ) ) ;
#60326 = LINE ( 'NONE', #43781, #38054 ) ;
#60327 = ORIENTED_EDGE ( 'NONE', *, *, #11199, .T. ) ;
#60328 = CARTESIAN_POINT ( 'NONE',  ( 114.6797682035589503, 32.10876583290007602, 57.88993258366536310 ) ) ;
#60329 = CARTESIAN_POINT ( 'NONE',  ( 141.2801018238827169, 47.29457739955282847, 64.95722907669554047 ) ) ;
#60330 = CARTESIAN_POINT ( 'NONE',  ( -74.40004226286977485, 20.74218500375955543, -48.78853105593013595 ) ) ;
#60331 = LINE ( 'NONE', #33617, #11234 ) ;
#60332 = CARTESIAN_POINT ( 'NONE',  ( 92.53566308513168792, 21.52138666710686010, -38.67290711224870137 ) ) ;
#60333 = EDGE_CURVE ( 'NONE', #43731, #44813, #16693, .T. ) ;
#60334 = CARTESIAN_POINT ( 'NONE',  ( -47.61402178322638434, 13.84598486314981614, -16.86057252496108561 ) ) ;
#60335 = ADVANCED_FACE ( 'NONE', ( #48330 ), #21623, .T. ) ;
#60336 = ORIENTED_EDGE ( 'NONE', *, *, #47340, .F. ) ;
#60337 = CARTESIAN_POINT ( 'NONE',  ( 115.2288739107204663, 31.25773204386719684, -49.03044408911942753 ) ) ;
#60338 = EDGE_CURVE ( 'NONE', #50693, #30445, #10749, .T. ) ;
#60339 = CARTESIAN_POINT ( 'NONE',  ( 133.8566784816069344, -170.0000000000000000, 17.66579024853170310 ) ) ;
#60340 = CARTESIAN_POINT ( 'NONE',  ( -143.8634661037141029, 60.82480701605698670, -47.27825893513519873 ) ) ;
#60341 = DIRECTION ( 'NONE',  ( -0.000000000000000000, -0.000000000000000000, -1.000000000000000000 ) ) ;
#60343 = ORIENTED_EDGE ( 'NONE', *, *, #29789, .F. ) ;
#60342 = CARTESIAN_POINT ( 'NONE',  ( 21.98745393275193294, 71.71550996510526943, 170.0000000000000000 ) ) ;
#60344 = CARTESIAN_POINT ( 'NONE',  ( 56.52885800925551507, 12.28784885070978916, 6.671513217819436292 ) ) ;
#60345 = EDGE_CURVE ( 'NONE', #42019, #6204, #58227, .T. ) ;
#60346 = EDGE_LOOP ( 'NONE', ( #62407, #56124, #49601, #62184 ) ) ;
#60347 = CARTESIAN_POINT ( 'NONE',  ( -128.1384526288950099, 47.98891607499719925, 30.94904902096297405 ) ) ;
#60348 = VECTOR ( 'NONE', #37914, 1000.000000000000000 ) ;
#60349 = LINE ( 'NONE', #59295, #59154 ) ;
#60350 = FACE_OUTER_BOUND ( 'NONE', #69479, .T. ) ;
#60351 = DIRECTION ( 'NONE',  ( -1.000000000000000000, 0.000000000000000000, 0.000000000000000000 ) ) ;
#60352 = DIRECTION ( 'NONE',  ( -1.850371928290090422E-16, 1.000000000000000000, 1.110223024625156294E-16 ) ) ;
#60353 = VECTOR ( 'NONE', #39283, 1000.000000000000000 ) ;
#60354 = PLANE ( 'NONE',  #40995 ) ;
#60355 = CARTESIAN_POINT ( 'NONE',  ( 94.12988949694080532, 22.11811104795074812, -69.93042459641294784 ) ) ;
#60356 = DIRECTION ( 'NONE',  ( 0.000000000000000000, 0.000000000000000000, -1.000000000000000000 ) ) ;
#60357 = DIRECTION ( 'NONE',  ( 1.000000000000000000, 0.000000000000000000, 0.000000000000000000 ) ) ;
#60359 = VERTEX_POINT ( 'NONE', #11066 ) ;
#60358 = B_SPLINE_CURVE_WITH_KNOTS ( 'NONE', 3,
 ( #7583, #7918, #12855, #55756, #18471, #39919, #13201, #9294, #41650, #25489, #24103, #30757, #8263, #46929, #35342, #40270, #46575, #68392, #24452, #19155, #20193, #63106, #61718, #52205, #13543, #50821, #56439, #40609, #4021, #57832, #57147, #67705, #62060, #30405, #19498, #51524, #13875, #62419, #62767, #40960, #3329, #9647, #45541, #56801, #8618, #35696 ),
 .UNSPECIFIED., .F., .F.,
 ( 4, 2, 2, 2, 2, 2, 2, 2, 2, 2, 2, 2, 2, 2, 2, 2, 2, 2, 2, 2, 2, 2, 4 ),
 ( 0.02420077021543442022, 0.02572112563160194876, 0.02648130333968569741, 0.02724148104776944260, 0.02876183646393689827, 0.02952201417202062611, 0.03028219188010435742, 0.03180254729627184085, 0.03332290271243932428, 0.03408308042052305559, 0.03484325812860678689, 0.03636361354477425645, 0.03712379125285798775, 0.03788396896094172600, 0.03864414666902546425, 0.03940432437710919555, 0.04092467979327665123, 0.04244503520944410691, 0.04396539062561155564, 0.04548574604177901132, 0.04624592374986272181, 0.04700610145794643924, 0.04852645687411390185 ),
 .UNSPECIFIED. ) ;
#60360 = ADVANCED_FACE ( 'NONE', ( #32529 ), #38147, .F. ) ;
#60361 = ORIENTED_EDGE ( 'NONE', *, *, #31364, .F. ) ;
#60362 = ADVANCED_FACE ( 'NONE', ( #27243 ), #48677, .F. ) ;
#60363 = AXIS2_PLACEMENT_3D ( 'NONE', #13844, #46540, #46894 ) ;
#60364 = EDGE_CURVE ( 'NONE', #42365, #68939, #15321, .T. ) ;
#60365 = CARTESIAN_POINT ( 'NONE',  ( 41.09671232177015554, 8.635892912882342287, 30.10370141709571712 ) ) ;
#60366 = CARTESIAN_POINT ( 'NONE',  ( 201.9777685760379313, 102.6876480786892927, -23.98289206748827951 ) ) ;
#60367 = LINE ( 'NONE', #37863, #4253 ) ;
#60368 = FACE_OUTER_BOUND ( 'NONE', #38102, .T. ) ;
#60369 = VECTOR ( 'NONE', #1595, 1000.000000000000000 ) ;
#60370 = CARTESIAN_POINT ( 'NONE',  ( 311.9975424824652350, 170.0000000000000284, 256.6193948016162381 ) ) ;
#60371 = FACE_OUTER_BOUND ( 'NONE', #25260, .T. ) ;
#60372 = CIRCLE ( 'NONE', #57018, 63.00000000000000000 ) ;
#60373 = DIRECTION ( 'NONE',  ( 1.000000000000000000, -0.000000000000000000, 0.000000000000000000 ) ) ;
#60374 = CARTESIAN_POINT ( 'NONE',  ( -25.98312968277008039, 8.759224980175263298, -47.96912024656418794 ) ) ;
#60375 = CARTESIAN_POINT ( 'NONE',  ( 10.01137213834968165, -64.59476928204590251, 43.58025477438756212 ) ) ;
#60376 = ORIENTED_EDGE ( 'NONE', *, *, #42701, .T. ) ;
#60377 = CARTESIAN_POINT ( 'NONE',  ( -47.68562151781910785, 12.82916850665305475, -95.00000000000133582 ) ) ;
#60378 = ORIENTED_EDGE ( 'NONE', *, *, #58459, .F. ) ;
#60380 = AXIS2_PLACEMENT_3D ( 'NONE', #6540, #37496, #55062 ) ;
#60379 = DIRECTION ( 'NONE',  ( 0.000000000000000000, 1.000000000000000000, 0.000000000000000000 ) ) ;
#60381 = CARTESIAN_POINT ( 'NONE',  ( -81.95806712579563680, 23.60263724764760696, 84.86105897464825887 ) ) ;
#60382 = CARTESIAN_POINT ( 'NONE',  ( -86.06016868996614733, 25.27707703029501118, 66.04626657972286807 ) ) ;
#60383 = CARTESIAN_POINT ( 'NONE',  ( 128.0540543950622236, 39.18660671946769014, 41.78878589093363161 ) ) ;
#60384 = CARTESIAN_POINT ( 'NONE',  ( 32.29578462738146527, 8.602609172809797755, 12.98030737452486072 ) ) ;
#60385 = DIRECTION ( 'NONE',  ( 0.000000000000000000, 0.000000000000000000, -1.000000000000000000 ) ) ;
#60386 = CARTESIAN_POINT ( 'NONE',  ( -99.98584758882476820, 32.75338129098886952, -22.82608027691124519 ) ) ;
#60387 = CARTESIAN_POINT ( 'NONE',  ( 0.000000000000000000, 0.000000000000000000, 0.000000000000000000 ) ) ;
#60388 = CARTESIAN_POINT ( 'NONE',  ( 207.5654265768424693, 110.3565116837594076, 83.44490759518619427 ) ) ;
#60389 = LINE ( 'NONE', #23464, #48790 ) ;
#60390 = ORIENTED_EDGE ( 'NONE', *, *, #57432, .T. ) ;
#60391 = DIRECTION ( 'NONE',  ( -0.000000000000000000, -0.000000000000000000, -1.000000000000000000 ) ) ;
#60392 = FACE_OUTER_BOUND ( 'NONE', #62432, .T. ) ;
#60393 = CARTESIAN_POINT ( 'NONE',  ( -189.4248691432192970, 107.3461292335514656, -43.84368868221933724 ) ) ;
#60394 = DIRECTION ( 'NONE',  ( -0.000000000000000000, 0.000000000000000000, -1.000000000000000000 ) ) ;
#60395 = DIRECTION ( 'NONE',  ( -0.000000000000000000, 1.000000000000000000, -0.000000000000000000 ) ) ;
#60396 = LINE ( 'NONE', #7284, #9217 ) ;
#60397 = ORIENTED_EDGE ( 'NONE', *, *, #12819, .T. ) ;
#60398 = DIRECTION ( 'NONE',  ( 0.000000000000000000, -1.000000000000000000, 0.000000000000000000 ) ) ;
#60399 = CARTESIAN_POINT ( 'NONE',  ( -44.26023579658871654, -48.10138582123836670, 3.125053320693551875E-16 ) ) ;
#60400 = CARTESIAN_POINT ( 'NONE',  ( 410.0000000000000000, 188.0000000000000000, -90.00000000000000000 ) ) ;
#60401 = CARTESIAN_POINT ( 'NONE',  ( -166.7050147108375029, 81.70694330787516435, -38.28854392307332688 ) ) ;
#60402 = CARTESIAN_POINT ( 'NONE',  ( -188.6739852773920632, 108.2139733222100517, -40.40546001351593475 ) ) ;
#60403 = ORIENTED_EDGE ( 'NONE', *, *, #43755, .T. ) ;
#60404 = CARTESIAN_POINT ( 'NONE',  ( -102.2801239173131052, 32.78103895658058065, 3.674523915951417141 ) ) ;
#60405 = DIRECTION ( 'NONE',  ( 0.000000000000000000, 1.000000000000000000, 0.000000000000000000 ) ) ;
#60406 = AXIS2_PLACEMENT_3D ( 'NONE', #29033, #50474, #2295 ) ;
#60407 = CARTESIAN_POINT ( 'NONE',  ( -143.8794621588508562, 59.54894433207191184, -20.43180592025295894 ) ) ;
#60408 = CARTESIAN_POINT ( 'NONE',  ( -5.417282889646083177, 7.753782747238989970, -62.65547924408967617 ) ) ;
#60409 = SHAPE_REPRESENTATION ( 'hex bolt gradeb_iso_ISO 4015 - M10 x 40 x 26-N', ( #66832 ), #10752 ) ;
#60410 = CIRCLE ( 'NONE', #55944, 5.000000000000004441 ) ;
#60411 = DIRECTION ( 'NONE',  ( 0.9839295885986295565, 0.1785568947986370392, 0.000000000000000000 ) ) ;
#60412 = ORIENTED_EDGE ( 'NONE', *, *, #31275, .F. ) ;
#60413 = CARTESIAN_POINT ( 'NONE',  ( -61.10880364359509542, 17.43879918625642844, 6.541553347541163355 ) ) ;
#60414 = CARTESIAN_POINT ( 'NONE',  ( 201.5903370237275283, 102.1785392640257868, -50.66542380412518298 ) ) ;
#60415 = CARTESIAN_POINT ( 'NONE',  ( -150.5993571094983281, 66.43939758484178526, 30.79752979960735715 ) ) ;
#60416 = CARTESIAN_POINT ( 'NONE',  ( 18.66025561752211104, 6.609375019058820300, -49.96014427081493636 ) ) ;
#60417 = VECTOR ( 'NONE', #61036, 1000.000000000000227 ) ;
#60419 = VERTEX_POINT ( 'NONE', #39897 ) ;
#60418 = CARTESIAN_POINT ( 'NONE',  ( -15.55634918610400597, 15.55634918610405748, 85.00100000000000477 ) ) ;
#60420 = DIRECTION ( 'NONE',  ( 0.000000000000000000, 0.000000000000000000, 1.000000000000000000 ) ) ;
#60421 = EDGE_CURVE ( 'NONE', #36461, #4465, #19749, .T. ) ;
#60422 = ORIENTED_EDGE ( 'NONE', *, *, #52864, .F. ) ;
#60423 = VERTEX_POINT ( 'NONE', #44478 ) ;
#60424 = AXIS2_PLACEMENT_3D ( 'NONE', #62350, #30342, #51794 ) ;
#60425 = CARTESIAN_POINT ( 'NONE',  ( 177.0110682437507990, 75.98481089748379702, 30.49479835804475059 ) ) ;
#60426 = ADVANCED_FACE ( 'NONE', ( #45166 ), #50456, .T. ) ;
#60427 = DIRECTION ( 'NONE',  ( -0.000000000000000000, -1.000000000000000000, -0.000000000000000000 ) ) ;
#60429 = ORIENTED_EDGE ( 'NONE', *, *, #871, .F. ) ;
#60428 = CARTESIAN_POINT ( 'NONE',  ( -12.78319349481552258, 8.274445259016799170, -64.11374738978491905 ) ) ;
#60430 = DIRECTION ( 'NONE',  ( -1.000000000000000000, 0.000000000000000000, 0.000000000000000000 ) ) ;
#60431 = ADVANCED_FACE ( 'NONE', ( #50793 ), #23027, .F. ) ;
#60432 = PLANE ( 'NONE',  #45170 ) ;
#60433 = DIRECTION ( 'NONE',  ( 3.835731315158922607E-15, 1.000000000000000000, 5.551115123125782702E-17 ) ) ;
#60434 = VERTEX_POINT ( 'NONE', #34641 ) ;
#60435 = CARTESIAN_POINT ( 'NONE',  ( -63.89980896331448434, -18.93195718737547750, 34.48241823982459664 ) ) ;
#60436 = CARTESIAN_POINT ( 'NONE',  ( -38.69408084385330682, 10.89529537250242974, -14.00704445308265633 ) ) ;
#60437 = CARTESIAN_POINT ( 'NONE',  ( -34.39004539972345498, 0.000000000000000000, -5.000000000000000000 ) ) ;
#60438 = CARTESIAN_POINT ( 'NONE',  ( 129.1052153257903967, 39.78893484542955150, 69.67837425836049192 ) ) ;
#60439 = PLANE ( 'NONE',  #19410 ) ;
#60440 = EDGE_CURVE ( 'NONE', #10658, #26520, #43763, .T. ) ;
#60441 = ORIENTED_EDGE ( 'NONE', *, *, #23205, .F. ) ;
#60442 = ORIENTED_EDGE ( 'NONE', *, *, #60161, .T. ) ;
#60443 = ORIENTED_EDGE ( 'NONE', *, *, #42697, .T. ) ;
#60444 = DIRECTION ( 'NONE',  ( 1.261617073437677999E-16, 0.000000000000000000, 1.000000000000000000 ) ) ;
#60445 = CARTESIAN_POINT ( 'NONE',  ( -105.8683518445188554, 35.77995342500076248, 4.571401378338662447 ) ) ;
#60446 = LINE ( 'NONE', #39685, #12218 ) ;
#60447 = CARTESIAN_POINT ( 'NONE',  ( -36.37663950036512261, 10.45389057208229033, -37.15064349336959282 ) ) ;
#60448 = CARTESIAN_POINT ( 'NONE',  ( -94.77657963819960685, 29.12969147113658153, 91.47122548580749424 ) ) ;
#60449 = CARTESIAN_POINT ( 'NONE',  ( -143.2471548081022661, 59.04577938365764567, 34.05900480430268829 ) ) ;
#60450 = CARTESIAN_POINT ( 'NONE',  ( -131.3154845336012500, 50.16828105866952114, 59.75965407406295782 ) ) ;
#60451 = CARTESIAN_POINT ( 'NONE',  ( -72.35078170365746075, 21.08176362823952843, -19.82354011342815880 ) ) ;
#60452 = VERTEX_POINT ( 'NONE', #61005 ) ;
#60453 = CARTESIAN_POINT ( 'NONE',  ( 82.14449817946436383, 17.93919511903895625, 70.07299682206928537 ) ) ;
#60455 = ORIENTED_EDGE ( 'NONE', *, *, #23919, .F. ) ;
#60454 = B_SPLINE_CURVE_WITH_KNOTS ( 'NONE', 3,
 ( #50591, #8737, #19978, #20306, #3447, #62180, #47043, #51639, #24909, #3109, #24571, #61826, #15038, #67473, #14000, #52320, #63228, #40722, #57945, #41771, #31227, #41429, #46341, #52658, #57609, #4483, #13650, #30526, #56559, #9420, #9765, #56920, #9073, #36494, #25609, #25941, #36150, #8385, #35104, #47373, #19620, #18934, #40383, #35456, #29829, #62541 ),
 .UNSPECIFIED., .F., .F.,
 ( 4, 2, 2, 2, 2, 2, 2, 2, 2, 2, 2, 2, 2, 2, 2, 2, 2, 2, 2, 2, 2, 2, 4 ),
 ( 0.02989107162308287519, 0.03170280136394029724, 0.03351453110479772624, 0.03532626084565514829, 0.03713799058651257035, 0.03894972032736999934, 0.03985558519779868608, 0.04076145006822737282, 0.04166731493865606650, 0.04257317980908476018, 0.04347904467951344692, 0.04438490954994213367, 0.04529077442037082735, 0.04619663929079951409, 0.04710250416122820777, 0.04800836903165689451, 0.04891423390208558819, 0.04982009877251427493, 0.05163182851337158596, 0.05344355825422892475, 0.05525528799508625660, 0.05706701773594359539, 0.05887874747680092724 ),
 .UNSPECIFIED. ) ;
#60456 = VECTOR ( 'NONE', #59865, 1000.000000000000000 ) ;
#60457 = CARTESIAN_POINT ( 'NONE',  ( 34.45500533947589616, 7.817363290423890554, 43.07223163450435521 ) ) ;
#60458 = LINE ( 'NONE', #48476, #30755 ) ;
#60459 = DIRECTION ( 'NONE',  ( 0.000000000000000000, 1.000000000000000000, 0.000000000000000000 ) ) ;
#60460 = FACE_OUTER_BOUND ( 'NONE', #5967, .T. ) ;
#60461 = LINE ( 'NONE', #28810, #19007 ) ;
#60462 = CARTESIAN_POINT ( 'NONE',  ( -124.1007047332778228, 46.52282960291165637, 57.66784334201018680 ) ) ;
#60463 = DIRECTION ( 'NONE',  ( 0.000000000000000000, 0.000000000000000000, -1.000000000000000000 ) ) ;
#60464 = CARTESIAN_POINT ( 'NONE',  ( 150.0973882686025433, 52.13852366454153042, -42.22282177753791643 ) ) ;
#60465 = AXIS2_PLACEMENT_3D ( 'NONE', #19518, #18139, #67379 ) ;
#60466 = CARTESIAN_POINT ( 'NONE',  ( -0.6543471694412733575, -8.859816792613656844, -9.003584543331200507 ) ) ;
#60467 = ORIENTED_EDGE ( 'NONE', *, *, #46843, .T. ) ;
#60468 = CARTESIAN_POINT ( 'NONE',  ( -447.6627218934889925, 395.0000000000064801, -141.4497041420092387 ) ) ;
#60469 = DIRECTION ( 'NONE',  ( 0.9909497617679352555, -0.1342332658176522697, 5.102127870520022769E-18 ) ) ;
#60470 = ORIENTED_EDGE ( 'NONE', *, *, #790, .T. ) ;
#60471 = CYLINDRICAL_SURFACE ( 'NONE', #65713, 7.500000000000013323 ) ;
#60472 = CARTESIAN_POINT ( 'NONE',  ( -149.5074843970971017, 65.50121172469319220, -49.81283053149199702 ) ) ;
#60473 = ORIENTED_EDGE ( 'NONE', *, *, #49395, .F. ) ;
#60474 = CARTESIAN_POINT ( 'NONE',  ( -85.46258339457286013, 25.02772366257408265, 34.73610256809621433 ) ) ;
#60475 = CARTESIAN_POINT ( 'NONE',  ( 152.8672128926848188, 55.41186463791517269, -76.39475647682806425 ) ) ;
#60476 = CARTESIAN_POINT ( 'NONE',  ( 43.96062659677686213, 10.06332325923986204, 43.38939548662082046 ) ) ;
#60477 = SURFACE_SIDE_STYLE ('',( #14239 ) ) ;
#60478 = ORIENTED_EDGE ( 'NONE', *, *, #24012, .T. ) ;
#60479 = ORIENTED_EDGE ( 'NONE', *, *, #30665, .T. ) ;
#60480 = CYLINDRICAL_SURFACE ( 'NONE', #47987, 5.000000000000004441 ) ;
#60481 = ORIENTED_EDGE ( 'NONE', *, *, #5871, .T. ) ;
#60482 = CARTESIAN_POINT ( 'NONE',  ( -189.2776534485022069, 107.1424877329940841, -95.00000000000133582 ) ) ;
#60483 = CARTESIAN_POINT ( 'NONE',  ( -23.14886993799567705, -9.760512885997105315, 0.000000000000000000 ) ) ;
#60484 = LINE ( 'NONE', #6671, #450 ) ;
#60485 = EDGE_CURVE ( 'NONE', #52661, #43797, #18443, .T. ) ;
#60486 = CARTESIAN_POINT ( 'NONE',  ( 138.0620293754376178, 45.21335672767177272, 84.48092758364141730 ) ) ;
#60487 = DIRECTION ( 'NONE',  ( 0.000000000000000000, 0.000000000000000000, 1.000000000000000000 ) ) ;
#60488 = CARTESIAN_POINT ( 'NONE',  ( -72.62976060914745347, 18.74780984163036024, 170.0000000000000000 ) ) ;
#60489 = EDGE_CURVE ( 'NONE', #34313, #50651, #59041, .T. ) ;
#60490 = VERTEX_POINT ( 'NONE', #27945 ) ;
#60491 = CARTESIAN_POINT ( 'NONE',  ( -120.4816138481825192, 43.03185659245512085, -74.47313363230125560 ) ) ;
#60492 = ORIENTED_EDGE ( 'NONE', *, *, #45473, .T. ) ;
#60493 = ORIENTED_EDGE ( 'NONE', *, *, #54760, .T. ) ;
#60494 = DIRECTION ( 'NONE',  ( 0.000000000000000000, 1.000000000000000000, -0.000000000000000000 ) ) ;
#60495 = DIRECTION ( 'NONE',  ( -0.000000000000000000, -0.000000000000000000, 1.000000000000000000 ) ) ;
#60496 = CARTESIAN_POINT ( 'NONE',  ( 0.000000000000000000, 0.000000000000000000, 26.24939009510892518 ) ) ;
#60497 = CARTESIAN_POINT ( 'NONE',  ( 139.2794027252094509, 45.99190465195508892, 15.36930535624699523 ) ) ;
#60498 = LINE ( 'NONE', #33434, #41958 ) ;
#60499 = ORIENTED_EDGE ( 'NONE', *, *, #15034, .F. ) ;
#60500 = ADVANCED_FACE ( 'NONE', ( #6839 ), #61354, .T. ) ;
#60501 = VERTEX_POINT ( 'NONE', #28653 ) ;
#60502 = EDGE_CURVE ( 'NONE', #42281, #60658, #66973, .T. ) ;
#60503 = CARTESIAN_POINT ( 'NONE',  ( 15.29293866748104769, 6.484959508098437020, 45.01470767270525641 ) ) ;
#60504 = ORIENTED_EDGE ( 'NONE', *, *, #32565, .T. ) ;
#60505 = CARTESIAN_POINT ( 'NONE',  ( 133.8566784816069344, 41.42467568809808398, -89.71241211332301191 ) ) ;
#60506 = CIRCLE ( 'NONE', #36912, 5.000000000000004441 ) ;
#60507 = ORIENTED_EDGE ( 'NONE', *, *, #61770, .F. ) ;
#60508 = CARTESIAN_POINT ( 'NONE',  ( -124.1007047332778512, 46.52282960291164216, 3.978742161082801321 ) ) ;
#60509 = EDGE_CURVE ( 'NONE', #29802, #13226, #36628, .T. ) ;
#60510 = CARTESIAN_POINT ( 'NONE',  ( 88.52345267551652341, 20.07594890262054932, 3.106688155335522339 ) ) ;
#60511 = AXIS2_PLACEMENT_3D ( 'NONE', #56205, #40035, #22810 ) ;
#60512 = DIRECTION ( 'NONE',  ( -0.000000000000000000, 1.000000000000000000, -0.000000000000000000 ) ) ;
#60513 = ORIENTED_EDGE ( 'NONE', *, *, #9005, .T. ) ;
#60514 = DIRECTION ( 'NONE',  ( -1.000000000000000000, -2.465190328815660250E-32, -1.671219923253722421E-63 ) ) ;
#60515 = LINE ( 'NONE', #28867, #32350 ) ;
#60516 = CARTESIAN_POINT ( 'NONE',  ( 156.5977259323288990, 56.97512126940429056, 29.44731887063822739 ) ) ;
#60517 = CARTESIAN_POINT ( 'NONE',  ( 65.40383840050414221, 14.27443447873231719, 30.18673279204580595 ) ) ;
#60518 = CARTESIAN_POINT ( 'NONE',  ( -126.7989199172159829, 47.09198523267867387, -23.02839162617069491 ) ) ;
#60519 = CARTESIAN_POINT ( 'NONE',  ( -142.8209151613836241, 58.70887234856630243, -92.57052796546220463 ) ) ;
#60520 = CARTESIAN_POINT ( 'NONE',  ( 126.6395826915640015, 37.23416510613625974, -72.42523722532835961 ) ) ;
#60521 = EDGE_CURVE ( 'NONE', #30354, #39251, #7895, .T. ) ;
#60522 = ORIENTED_EDGE ( 'NONE', *, *, #22471, .T. ) ;
#60523 = CARTESIAN_POINT ( 'NONE',  ( 140.2200249818745021, 46.60103563593128229, -74.34575589100958837 ) ) ;
#60524 = DIRECTION ( 'NONE',  ( 0.000000000000000000, 0.000000000000000000, 1.000000000000000000 ) ) ;
#60525 = ORIENTED_EDGE ( 'NONE', *, *, #24760, .F. ) ;
#60526 = ADVANCED_FACE ( 'NONE', ( #44111 ), #43377, .T. ) ;
#60527 = EDGE_CURVE ( 'NONE', #57935, #57426, #43302, .T. ) ;
#60528 = DIRECTION ( 'NONE',  ( 0.000000000000000000, 0.000000000000000000, 1.000000000000000000 ) ) ;
#60529 = EDGE_CURVE ( 'NONE', #6992, #40870, #46903, .T. ) ;
#60530 = FACE_OUTER_BOUND ( 'NONE', #60626, .T. ) ;
#60531 = CARTESIAN_POINT ( 'NONE',  ( -34.74023699876256899, 11.17830703027882677, 30.96454232188382605 ) ) ;
#60532 = CARTESIAN_POINT ( 'NONE',  ( -142.5087559769085317, 59.74468185400779419, -12.71953806562390810 ) ) ;
#60533 = LINE ( 'NONE', #19260, #54787 ) ;
#60534 = DIRECTION ( 'NONE',  ( 0.000000000000000000, 0.000000000000000000, 1.000000000000000000 ) ) ;
#60535 = FACE_OUTER_BOUND ( 'NONE', #45719, .T. ) ;
#60536 = CARTESIAN_POINT ( 'NONE',  ( 113.3080539574503263, 21.67699184046404781, 3.763267418054582869 ) ) ;
#60537 = CARTESIAN_POINT ( 'NONE',  ( -72.09647865251525900, 19.92687487589685702, -92.68025296393560097 ) ) ;
#60538 = DIRECTION ( 'NONE',  ( 0.000000000000000000, -0.8660254037844380415, 0.5000000000000009992 ) ) ;
#60539 = CARTESIAN_POINT ( 'NONE',  ( 117.6916924104495763, 32.48309187151380684, 11.28248544281732002 ) ) ;
#60540 = DIRECTION ( 'NONE',  ( 1.000000000000000000, -4.565061778886334783E-18, 0.000000000000000000 ) ) ;
#60541 = ORIENTED_EDGE ( 'NONE', *, *, #4123, .T. ) ;
#60542 = CARTESIAN_POINT ( 'NONE',  ( -95.63694837622348643, 30.64472169584719907, -39.02429480595472455 ) ) ;
#60543 = VERTEX_POINT ( 'NONE', #61692 ) ;
#60544 = CARTESIAN_POINT ( 'NONE',  ( 26.11269837220803325, -15.55634918610409656, 2.000000000000001776 ) ) ;
#60545 = CARTESIAN_POINT ( 'NONE',  ( 35.00000000000000000, 4.286263797015736496E-15, 30.00000000000000000 ) ) ;
#60546 = CARTESIAN_POINT ( 'NONE',  ( 109.6443462180100425, 29.71354171299205049, 83.31739449737001735 ) ) ;
#60547 = CARTESIAN_POINT ( 'NONE',  ( 181.0840389613909736, -170.0000000000000000, -16.88050707541594164 ) ) ;
#60548 = LINE ( 'NONE', #49630, #32238 ) ;
#60549 = CARTESIAN_POINT ( 'NONE',  ( -15.55634918610408945, -31.11269837220804035, 2.000000000000001776 ) ) ;
#60550 = DIRECTION ( 'NONE',  ( 0.000000000000000000, 0.7071067811865474617, -0.7071067811865474617 ) ) ;
#60551 = CARTESIAN_POINT ( 'NONE',  ( -188.6739852773920632, 108.2139733222100375, -70.66125817296374123 ) ) ;
#60552 = VERTEX_POINT ( 'NONE', #13853 ) ;
#60553 = ORIENTED_EDGE ( 'NONE', *, *, #40963, .F. ) ;
#60554 = LINE ( 'NONE', #1827, #48885 ) ;
#60555 = CARTESIAN_POINT ( 'NONE',  ( 178.4027079424739384, 75.93756746109792743, 70.66078313421148493 ) ) ;
#60556 = DIRECTION ( 'NONE',  ( 0.000000000000000000, 0.000000000000000000, -1.000000000000000000 ) ) ;
#60557 = CARTESIAN_POINT ( 'NONE',  ( -167.6566265204789943, 82.70140535081092992, 70.30913300738275495 ) ) ;
#60558 = LINE ( 'NONE', #66215, #411 ) ;
#60559 = VECTOR ( 'NONE', #42427, 1000.000000000000000 ) ;
#60560 = CARTESIAN_POINT ( 'NONE',  ( -125.8938041572051389, -170.0000000000000000, -69.25825448869763079 ) ) ;
#60561 = ORIENTED_EDGE ( 'NONE', *, *, #20097, .T. ) ;
#60562 = CIRCLE ( 'NONE', #65027, 5.000000000000170530 ) ;
#60563 = CARTESIAN_POINT ( 'NONE',  ( 93.87650740736114585, 23.09802612281734469, 8.371155946943980908 ) ) ;
#60564 = CARTESIAN_POINT ( 'NONE',  ( 17.48988570800758424, 7.568061572928497682, -35.71044138032643644 ) ) ;
#60565 = DIRECTION ( 'NONE',  ( 0.000000000000000000, 1.224646799147357891E-16, 1.000000000000000000 ) ) ;
#60566 = FACE_OUTER_BOUND ( 'NONE', #44955, .T. ) ;
#60567 = CARTESIAN_POINT ( 'NONE',  ( 212.1700216741375300, 117.1889356120871639, -17.70906844655045376 ) ) ;
#60568 = EDGE_CURVE ( 'NONE', #28396, #54939, #63079, .T. ) ;
#60569 = FACE_BOUND ( 'NONE', #7847, .T. ) ;
#60570 = CARTESIAN_POINT ( 'NONE',  ( -58.33245019990695823, 15.58496056636070115, -35.95393952762761813 ) ) ;
#60571 = EDGE_CURVE ( 'NONE', #51895, #2171, #8933, .T. ) ;
#60572 = VERTEX_POINT ( 'NONE', #56772 ) ;
#60573 = LINE ( 'NONE', #25387, #28932 ) ;
#60574 = CARTESIAN_POINT ( 'NONE',  ( 88.98820631332499431, 21.30618275724810218, -50.45717736827222666 ) ) ;
#60575 = CARTESIAN_POINT ( 'NONE',  ( -49.12372073857199695, 14.20664392157176437, 60.04245956566853692 ) ) ;
#60576 = DIRECTION ( 'NONE',  ( -0.000000000000000000, 1.000000000000000000, -0.000000000000000000 ) ) ;
#60577 = LINE ( 'NONE', #55293, #23986 ) ;
#60578 = CONICAL_SURFACE ( 'NONE', #42645, 65.00000000000000000, 0.7853981633974497223 ) ;
#60579 = CYLINDRICAL_SURFACE ( 'NONE', #22099, 7.500000000000020428 ) ;
#60580 = ORIENTED_EDGE ( 'NONE', *, *, #59918, .T. ) ;
#60582 = EDGE_CURVE ( 'NONE', #37469, #34631, #33242, .T. ) ;
#60581 = CARTESIAN_POINT ( 'NONE',  ( 55.51597771111714508, 11.05737652677078664, 10.96812083458806697 ) ) ;
#60583 = CARTESIAN_POINT ( 'NONE',  ( -58.33959211651038146, 29.48226216511319464, 41.38025477438755928 ) ) ;
#60584 = ORIENTED_EDGE ( 'NONE', *, *, #66115, .T. ) ;
#60585 = EDGE_CURVE ( 'NONE', #59881, #4077, #68026, .T. ) ;
#60586 = CARTESIAN_POINT ( 'NONE',  ( 106.5030061485517763, 28.28936250057212476, -90.56079799092418625 ) ) ;
#60587 = ORIENTED_EDGE ( 'NONE', *, *, #26295, .T. ) ;
#60588 = DIRECTION ( 'NONE',  ( 1.000000000000000000, 0.000000000000000000, 0.000000000000000000 ) ) ;
#60589 = CARTESIAN_POINT ( 'NONE',  ( -58.75378739419586793, 16.75118858561006974, -22.41342698957060620 ) ) ;
#60590 = CARTESIAN_POINT ( 'NONE',  ( -417.6627218934913230, 1.665334536937734811E-13, 113.5502958579881749 ) ) ;
#60591 = ORIENTED_EDGE ( 'NONE', *, *, #63859, .F. ) ;
#60592 = ADVANCED_FACE ( 'NONE', ( #57459 ), #63640, .T. ) ;
#60593 = ORIENTED_EDGE ( 'NONE', *, *, #3880, .F. ) ;
#60594 = LINE ( 'NONE', #23325, #41983 ) ;
#60595 = VECTOR ( 'NONE', #52981, 999.9999999999998863 ) ;
#60596 = CARTESIAN_POINT ( 'NONE',  ( 164.6598737201888127, 64.78038692612518901, 34.70323317510625571 ) ) ;
#60597 = CARTESIAN_POINT ( 'NONE',  ( 106.6322547488295527, 28.34756922280617530, 3.675457982256730372 ) ) ;
#60598 = CARTESIAN_POINT ( 'NONE',  ( 69.83617901654358207, 15.39919709983077389, 7.339238517795263483 ) ) ;
#60599 = LINE ( 'NONE', #54252, #16282 ) ;
#60600 = DIRECTION ( 'NONE',  ( -0.000000000000000000, -0.000000000000000000, -1.000000000000000000 ) ) ;
#60601 = LINE ( 'NONE', #18383, #2822 ) ;
#60602 = CARTESIAN_POINT ( 'NONE',  ( -14.65000983264446788, 8.442132792737769620, -93.38135813376521810 ) ) ;
#60603 = CYLINDRICAL_SURFACE ( 'NONE', #2643, 4.999999999999997335 ) ;
#60604 = FACE_OUTER_BOUND ( 'NONE', #10345, .T. ) ;
#60605 = VECTOR ( 'NONE', #36648, 1000.000000000000000 ) ;
#60606 = CARTESIAN_POINT ( 'NONE',  ( 93.32455161385975373, 21.81511294875801710, 87.50465937977445208 ) ) ;
#60608 = ORIENTED_EDGE ( 'NONE', *, *, #32463, .F. ) ;
#60607 = CARTESIAN_POINT ( 'NONE',  ( 64.08056813503694116, 12.89932471814516290, 43.58025477438756212 ) ) ;
#60609 = EDGE_LOOP ( 'NONE', ( #12511, #62761, #14585, #41825 ) ) ;
#60610 = EDGE_CURVE ( 'NONE', #24540, #20416, #61376, .T. ) ;
#60611 = EDGE_CURVE ( 'NONE', #59231, #16988, #24473, .T. ) ;
#60612 = VECTOR ( 'NONE', #47246, 1000.000000000000000 ) ;
#60613 = ORIENTED_EDGE ( 'NONE', *, *, #63779, .F. ) ;
#60614 = CARTESIAN_POINT ( 'NONE',  ( -7.825402957745083654, 6.891034867348163395, -23.57352014148015584 ) ) ;
#60615 = CARTESIAN_POINT ( 'NONE',  ( -167.1306301799594110, 82.15042288607379817, 87.48651795901140815 ) ) ;
#60616 = CARTESIAN_POINT ( 'NONE',  ( -47.55360235114366674, 12.79819361309568926, -16.38438511314839374 ) ) ;
#60617 = CARTESIAN_POINT ( 'NONE',  ( 103.8102216002272939, -165.0710086335687379, 10.00000000000000000 ) ) ;
#60618 = EDGE_CURVE ( 'NONE', #67945, #13204, #21538, .T. ) ;
#60619 = CARTESIAN_POINT ( 'NONE',  ( -56.97556689808915564, 16.24958672959845885, -35.46295881559763075 ) ) ;
#60620 = CARTESIAN_POINT ( 'NONE',  ( 450.2085304802404835, 190.0000000000000000, -219.9999999999999147 ) ) ;
#60621 = CYLINDRICAL_SURFACE ( 'NONE', #63486, 5.000000000000170530 ) ;
#60622 = CARTESIAN_POINT ( 'NONE',  ( -14.32241591711282247, 7.401556312061832621, 41.37047100563557933 ) ) ;
#60623 = VERTEX_POINT ( 'NONE', #42315 ) ;
#60624 = CARTESIAN_POINT ( 'NONE',  ( -21.27554331372908081, -61.43430442924895374, 170.0000000000000000 ) ) ;
#60625 = ORIENTED_EDGE ( 'NONE', *, *, #20097, .F. ) ;
#60626 = EDGE_LOOP ( 'NONE', ( #33679, #29352, #67828, #41258 ) ) ;
#60627 = CARTESIAN_POINT ( 'NONE',  ( -142.8556048422594813, 60.01994222009839319, 14.85110067941132961 ) ) ;
#60628 = DIRECTION ( 'NONE',  ( -0.8090169943749507819, 0.5877852522924685852, 0.000000000000000000 ) ) ;
#60629 = CARTESIAN_POINT ( 'NONE',  ( -32.72965438883313993, 10.82661681132672093, 83.98928369309581399 ) ) ;
#60630 = AXIS2_PLACEMENT_3D ( 'NONE', #63725, #26437, #58767 ) ;
#60631 = CARTESIAN_POINT ( 'NONE',  ( 73.95984195137799588, -12.15131637179793955, 41.38025477438755928 ) ) ;
#60632 = DIRECTION ( 'NONE',  ( 0.3930250316539278255, -0.9195277725514487965, 0.000000000000000000 ) ) ;
#60633 = CARTESIAN_POINT ( 'NONE',  ( -190.6985136298601731, 109.1272424661242582, 94.99999999999866418 ) ) ;
#60634 = CARTESIAN_POINT ( 'NONE',  ( 138.5943620234099001, 45.55242290395134575, -22.51329138269814578 ) ) ;
#60635 = ORIENTED_EDGE ( 'NONE', *, *, #34347, .T. ) ;
#60636 = VERTEX_POINT ( 'NONE', #15238 ) ;
#60637 = EDGE_LOOP ( 'NONE', ( #40975, #40629, #9708, #13277 ) ) ;
#60638 = DIRECTION ( 'NONE',  ( 1.000000000000000000, 0.000000000000000000, 0.000000000000000000 ) ) ;
#60639 = CARTESIAN_POINT ( 'NONE',  ( -11.57808265946730231, 7.164483090579921054, 4.272735484984936605 ) ) ;
#60640 = CARTESIAN_POINT ( 'NONE',  ( 33.44983424733139543, 7.709709042132400825, -65.37461540421082873 ) ) ;
#60641 = LINE ( 'NONE', #22311, #61080 ) ;
#60642 =( REPRESENTATION_RELATIONSHIP ('NONE','NONE', #40274, #32051 ) REPRESENTATION_RELATIONSHIP_WITH_TRANSFORMATION ( #614 )SHAPE_REPRESENTATION_RELATIONSHIP( ) );
#60643 = UNCERTAINTY_MEASURE_WITH_UNIT (LENGTH_MEASURE( 1.000000000000000082E-05 ), #59043, 'distance_accuracy_value', 'NONE');
#60644 = CARTESIAN_POINT ( 'NONE',  ( 0.000000000000000000, 0.000000000000000000, 41.38025477438755928 ) ) ;
#60645 = AXIS2_PLACEMENT_3D ( 'NONE', #40038, #59731, #16829 ) ;
#60646 = CARTESIAN_POINT ( 'NONE',  ( -8.000000000000000000, -1.555946510856147880, -9.432911297836646725 ) ) ;
#60647 = ORIENTED_EDGE ( 'NONE', *, *, #11103, .T. ) ;
#60648 = CARTESIAN_POINT ( 'NONE',  ( -452.6627218934913799, 0.000000000000000000, -116.4497041420118393 ) ) ;
#60649 = CARTESIAN_POINT ( 'NONE',  ( 198.8732368717151644, 100.3103976497390590, -65.93875134692073914 ) ) ;
#60650 = SHAPE_REPRESENTATION_RELATIONSHIP ( 'NONE' , 'NONE' ,  #48255, #50824 ) ;
#60651 = CARTESIAN_POINT ( 'NONE',  ( -5.183193881612056408, 7.740932022135016410, -35.89460273968080628 ) ) ;
#60652 = CARTESIAN_POINT ( 'NONE',  ( 110.2429982417149290, 28.88204397445231209, 2.766663615273646570 ) ) ;
#60653 = CARTESIAN_POINT ( 'NONE',  ( 21.96921518829288900, -71.65937688154161833, 41.38025477438755928 ) ) ;
#60654 = DIRECTION ( 'NONE',  ( -0.000000000000000000, -0.000000000000000000, -1.000000000000000000 ) ) ;
#60655 = FACE_BOUND ( 'NONE', #14101, .T. ) ;
#60656 = DIRECTION ( 'NONE',  ( -0.8496664383351307803, 0.000000000000000000, 0.5273205320930463014 ) ) ;
#60657 = ADVANCED_FACE ( 'NONE', ( #5704 ), #41969, .F. ) ;
#60658 = VERTEX_POINT ( 'NONE', #58476 ) ;
#60659 = CARTESIAN_POINT ( 'NONE',  ( 280.0000000000000000, 21.42428528562853529, 4.999999999999990230 ) ) ;
#60660 = DIRECTION ( 'NONE',  ( -0.000000000000000000, 0.000000000000000000, -1.000000000000000000 ) ) ;
#60661 = LINE ( 'NONE', #18104, #9615 ) ;
#60662 = CARTESIAN_POINT ( 'NONE',  ( 3.000000000000002665, 0.000000000000000000, -50.00000000000000000 ) ) ;
#60663 = CARTESIAN_POINT ( 'NONE',  ( 125.0000000000000000, 1.530808498934191561E-14, -5.000000000000000000 ) ) ;
#60664 = ORIENTED_EDGE ( 'NONE', *, *, #50014, .T. ) ;
#60665 = VERTEX_POINT ( 'NONE', #15589 ) ;
#60667 = EDGE_CURVE ( 'NONE', #36599, #34263, #4095, .T. ) ;
#60666 = DIRECTION ( 'NONE',  ( 0.000000000000000000, 0.000000000000000000, 1.000000000000000000 ) ) ;
#60668 = CARTESIAN_POINT ( 'NONE',  ( 186.2914852210160461, 84.03335794683924576, 85.09093861525570901 ) ) ;
#60669 = VERTEX_POINT ( 'NONE', #11326 ) ;
#60670 = VERTEX_POINT ( 'NONE', #20506 ) ;
#60671 = B_SPLINE_CURVE_WITH_KNOTS ( 'NONE', 3,
 ( #1406, #27789, #1063, #43953, #17224, #33433, #54859, #6685, #17589, #28131, #39054, #60497, #20024, #30575, #3840, #14046, #3488, #35505, #62930, #40773, #40089, #45713, #41478, #52025, #4187, #56966, #30233, #61544, #62590, #24267, #61872, #25310, #51682, #41126, #8074, #40429, #19318, #29523, #14403, #13700, #35152, #9117, #13363, #50990, #2805, #67190, #8786, #24960 ),
 .UNSPECIFIED., .F., .F.,
 ( 4, 2, 2, 2, 2, 2, 2, 2, 2, 2, 2, 2, 2, 2, 2, 2, 2, 2, 2, 2, 2, 2, 2, 4 ),
 ( 0.000000000000000000, 0.001591515129442203210, 0.003183030258884406421, 0.003978787823605504231, 0.004774545388326602476, 0.006366060517768851006, 0.007957575647211098668, 0.009549090776653347198, 0.01034484834137447580, 0.01114060590609560440, 0.01193636347081673300, 0.01273212103553786334, 0.01432363616498011881, 0.01591515129442237775, 0.01671090885914350288, 0.01750666642386462801, 0.01830242398858576008, 0.01909818155330688522, 0.02068969668274918405, 0.02148545424747034041, 0.02228121181219149330, 0.02387272694163372622, 0.02466848450635488951, 0.02546424207107604240 ),
 .UNSPECIFIED. ) ;
#60672 = FACE_OUTER_BOUND ( 'NONE', #27584, .T. ) ;
#60673 = CARTESIAN_POINT ( 'NONE',  ( -176.3791001330698975, 90.82833141237287577, -62.28654758217901843 ) ) ;
#60674 = EDGE_CURVE ( 'NONE', #27330, #31531, #31756, .T. ) ;
#60675 = PLANE ( 'NONE',  #12211 ) ;
#60676 = ORIENTED_EDGE ( 'NONE', *, *, #51937, .F. ) ;
#60677 = CARTESIAN_POINT ( 'NONE',  ( -439.4229916354183274, 400.0000000000064801, 96.05029585798874336 ) ) ;
#60678 = ADVANCED_FACE ( 'NONE', ( #69388 ), #59510, .F. ) ;
#60679 = CARTESIAN_POINT ( 'NONE',  ( 0.000000000000000000, 0.000000000000000000, 85.00000000000000000 ) ) ;
#60680 = DIRECTION ( 'NONE',  ( 0.000000000000000000, 0.000000000000000000, 1.000000000000000000 ) ) ;
#60681 = VECTOR ( 'NONE', #57689, 1000.000000000000000 ) ;
#60682 = LINE ( 'NONE', #65982, #55076 ) ;
#60683 = CARTESIAN_POINT ( 'NONE',  ( -5.000000000000058620, -26.11269837220806522, 0.000000000000000000 ) ) ;
#60684 = CARTESIAN_POINT ( 'NONE',  ( -49.12372073857197563, 14.20664392157176259, -20.49119220572248423 ) ) ;
#60685 = EDGE_LOOP ( 'NONE', ( #42411, #12165, #47521, #47423 ) ) ;
#60686 = CARTESIAN_POINT ( 'NONE',  ( -124.3250225421925848, 45.46958056770282752, -8.231571376810528307 ) ) ;
#60687 = DIRECTION ( 'NONE',  ( -0.000000000000000000, -0.000000000000000000, -1.000000000000000000 ) ) ;
#60688 = CARTESIAN_POINT ( 'NONE',  ( -149.5074843970971017, 65.50121172469319220, -49.81283053149199702 ) ) ;
#60689 = FACE_OUTER_BOUND ( 'NONE', #43650, .T. ) ;
#60691 = ORIENTED_EDGE ( 'NONE', *, *, #18986, .F. ) ;
#60690 = CARTESIAN_POINT ( 'NONE',  ( -130.2601666248127401, 49.43645820311487427, 85.70393383863903125 ) ) ;
#60692 = CARTESIAN_POINT ( 'NONE',  ( 86.14852828165525978, 19.25704475759650336, -35.82156419891170884 ) ) ;
#60693 = AXIS2_PLACEMENT_3D ( 'NONE', #46611, #19890, #68748 ) ;
#60694 = ORIENTED_EDGE ( 'NONE', *, *, #37368, .T. ) ;
#60695 = B_SPLINE_CURVE_WITH_KNOTS ( 'NONE', 3,
 ( #68487, #37501, #16399, #57931, #47030, #210, #20292, #47704, #69505, #69165, #4126, #53674, #41757, #37855, #30862, #42096, #42772, #63214, #20991, #15366 ),
 .UNSPECIFIED., .F., .F.,
 ( 4, 2, 2, 2, 2, 2, 2, 2, 2, 4 ),
 ( 0.009977836299145791815, 0.01121959191743023346, 0.01246134753571467683, 0.01308222534485689766, 0.01370310315399911848, 0.01494485877228356185, 0.01618661439056800350, 0.01742837000885244861, 0.01867012562713689372, 0.01991188124542133536 ),
 .UNSPECIFIED. ) ;
#60696 = CARTESIAN_POINT ( 'NONE',  ( -132.6161619568759136, 51.08240647571224002, 34.78398694684950243 ) ) ;
#60697 = CARTESIAN_POINT ( 'NONE',  ( 82.94816950786172072, 19.25538918181909054, 43.75103483649611036 ) ) ;
#60698 = DIRECTION ( 'NONE',  ( -1.000000000000000000, 0.000000000000000000, 0.000000000000000000 ) ) ;
#60699 = EDGE_CURVE ( 'NONE', #34184, #32490, #22392, .T. ) ;
#60700 = CARTESIAN_POINT ( 'NONE',  ( 187.8959968237854241, 85.77553094678179946, -20.03028080268358835 ) ) ;
#60701 = CARTESIAN_POINT ( 'NONE',  ( 141.0645618855931218, 45.95036951196543384, -18.81836596334719047 ) ) ;
#60702 = LINE ( 'NONE', #28703, #2834 ) ;
#60703 = CARTESIAN_POINT ( 'NONE',  ( 93.85846834761629509, 22.01563781856519952, -72.17934525255718370 ) ) ;
#60704 = CARTESIAN_POINT ( 'NONE',  ( 73.57152302639913444, -14.62167909564502821, 43.58025477438756212 ) ) ;
#60705 = VERTEX_POINT ( 'NONE', #17668 ) ;
#60706 = ORIENTED_EDGE ( 'NONE', *, *, #9454, .T. ) ;
#60707 = CARTESIAN_POINT ( 'NONE',  ( 39.40195752203892710, 8.409560354027400209, 29.91383430596324899 ) ) ;
#60708 = DIRECTION ( 'NONE',  ( -0.000000000000000000, -0.000000000000000000, -1.000000000000000000 ) ) ;
#60709 = DIRECTION ( 'NONE',  ( -0.000000000000000000, 1.000000000000000000, -0.000000000000000000 ) ) ;
#60710 = PLANE ( 'NONE',  #31800 ) ;
#60711 = VECTOR ( 'NONE', #10398, 1000.000000000000000 ) ;
#60712 = CARTESIAN_POINT ( 'NONE',  ( 208.5884523568771840, 113.6152425727544824, -37.40009660611077891 ) ) ;
#60713 = CARTESIAN_POINT ( 'NONE',  ( -71.26746920569853216, 20.70422440535243069, -70.71288310661476828 ) ) ;
#60714 = CARTESIAN_POINT ( 'NONE',  ( -78.66644367742111399, 22.32174330031318377, -76.96000122218160300 ) ) ;
#60715 = CARTESIAN_POINT ( 'NONE',  ( -26.50364027666004318, 8.832969329054181529, -48.48556182960913219 ) ) ;
#60716 = PLANE ( 'NONE',  #68858 ) ;
#60717 = EDGE_LOOP ( 'NONE', ( #49519, #63915, #33077, #35406 ) ) ;
#60718 = ORIENTED_EDGE ( 'NONE', *, *, #716, .T. ) ;
#60719 = CARTESIAN_POINT ( 'NONE',  ( -9.771516655894561865, 7.025139475821124080, -50.17770668640199716 ) ) ;
#60720 = FACE_OUTER_BOUND ( 'NONE', #68243, .T. ) ;
#60721 = CARTESIAN_POINT ( 'NONE',  ( -8.000000000000000000, 3.115336682267014989, -9.180606868608490956 ) ) ;
#60722 = CARTESIAN_POINT ( 'NONE',  ( 126.4318266066171645, 38.27072266789463839, 35.91859280786284359 ) ) ;
#60723 = LINE ( 'NONE', #61757, #38938 ) ;
#60724 = DIRECTION ( 'NONE',  ( 0.000000000000000000, 1.000000000000000000, -0.000000000000000000 ) ) ;
#60725 = CONICAL_SURFACE ( 'NONE', #50584, 8.000000000000000000, 1.047197551196600296 ) ;
#60726 = CARTESIAN_POINT ( 'NONE',  ( 44.99999999999995737, -22.99999999999998579, 0.000000000000000000 ) ) ;
#60727 = CARTESIAN_POINT ( 'NONE',  ( 61.09977118998601497, 13.26754120022605932, 30.05771525600105321 ) ) ;
#60728 = CARTESIAN_POINT ( 'NONE',  ( 61.91366885787816443, -28.42865614898931881, 43.58025477438756923 ) ) ;
#60729 = CARTESIAN_POINT ( 'NONE',  ( -4.164416015345870470, 64.86646004871185767, 170.0000000000000000 ) ) ;
#60730 = VERTEX_POINT ( 'NONE', #38777 ) ;
#60731 = CARTESIAN_POINT ( 'NONE',  ( 63.01563776193090405, 13.70579113808098271, 71.65751152968501003 ) ) ;
#60732 = DIRECTION ( 'NONE',  ( -0.000000000000000000, -1.000000000000000000, -0.000000000000000000 ) ) ;
#60733 = CARTESIAN_POINT ( 'NONE',  ( -189.8071159312682710, 107.8771087123620163, -44.99094141979524863 ) ) ;
#60735 = ADVANCED_FACE ( 'NONE', ( #67179 ), #28206, .T. ) ;
#60734 = DIRECTION ( 'NONE',  ( -0.000000000000000000, -0.000000000000000000, -1.000000000000000000 ) ) ;
#60736 = CARTESIAN_POINT ( 'NONE',  ( 204.6977192012829789, 106.3443248447423315, 71.05227132923315025 ) ) ;
#60737 = CARTESIAN_POINT ( 'NONE',  ( 132.0249343950657135, 41.49728247212332377, -9.346915333156639250 ) ) ;
#60738 = EDGE_CURVE ( 'NONE', #16384, #9825, #21511, .T. ) ;
#60739 = ORIENTED_EDGE ( 'NONE', *, *, #45473, .F. ) ;
#60740 = APPLICATION_PROTOCOL_DEFINITION ( 'draft international standard', 'automotive_design', 1998, #53830 ) ;
#60741 = AXIS2_PLACEMENT_3D ( 'NONE', #2085, #23538, #55888 ) ;
#60742 = CARTESIAN_POINT ( 'NONE',  ( 35.16506403794528524, -22.46626249432251399, 13.79046340968178264 ) ) ;
#60743 = CARTESIAN_POINT ( 'NONE',  ( -36.38071096718370256, 11.47804921491337637, -37.15419882060332668 ) ) ;
#60744 = DIRECTION ( 'NONE',  ( -0.000000000000000000, -0.000000000000000000, -1.000000000000000000 ) ) ;
#60745 = ITEM_DEFINED_TRANSFORMATION ( 'NONE', 'NONE', #29898,  #66832 ) ;
#60746 = CARTESIAN_POINT ( 'NONE',  ( -173.7825098940164992, 87.86624138172392406, 84.52333946395306441 ) ) ;
#60747 = EDGE_LOOP ( 'NONE', ( #18678, #41365, #12867, #36404 ) ) ;
#60748 = CARTESIAN_POINT ( 'NONE',  ( -121.2008155373973750, 43.48033530165983507, -48.28419163247083645 ) ) ;
#60749 = LINE ( 'NONE', #6236, #30764 ) ;
#60750 = CARTESIAN_POINT ( 'NONE',  ( 140.0012045870120687, -170.0000000000000000, 94.99999999999866418 ) ) ;
#60751 = CARTESIAN_POINT ( 'NONE',  ( -5.412684891282534494, 7.753215344827985689, -76.88094471104368210 ) ) ;
#60752 = EDGE_CURVE ( 'NONE', #47772, #65564, #25779, .T. ) ;
#60753 = DIRECTION ( 'NONE',  ( 1.000000000000000000, 0.000000000000000000, 0.000000000000000000 ) ) ;
#60754 = ORIENTED_EDGE ( 'NONE', *, *, #34405, .F. ) ;
#60755 = CARTESIAN_POINT ( 'NONE',  ( 162.2792973920977317, 62.79117098392629259, -91.54424637048310842 ) ) ;
#60756 = CARTESIAN_POINT ( 'NONE',  ( 197.2200752504832053, 96.62072041958364821, -43.16169500306578044 ) ) ;
#60757 = ADVANCED_FACE ( 'NONE', ( #56952 ), #52010, .F. ) ;
#60758 = CARTESIAN_POINT ( 'NONE',  ( 15.55634918610397399, -31.11269837220809364, 0.000000000000000000 ) ) ;
#60759 = LINE ( 'NONE', #66756, #44945 ) ;
#60761 = VERTEX_POINT ( 'NONE', #9107 ) ;
#60760 = CARTESIAN_POINT ( 'NONE',  ( 1.667562369266826661, 64.99262834925669097, 41.38025477438755928 ) ) ;
#60762 = CARTESIAN_POINT ( 'NONE',  ( 55.90536342106781120, 11.13510150712953717, 34.87586743684235557 ) ) ;
#60763 = EDGE_LOOP ( 'NONE', ( #13309, #63714, #61151, #68456 ) ) ;
#60764 = ORIENTED_EDGE ( 'NONE', *, *, #25747, .F. ) ;
#60765 = CARTESIAN_POINT ( 'NONE',  ( -73.09185868250601459, 20.27574131633382848, -10.72959749028603049 ) ) ;
#60766 = CARTESIAN_POINT ( 'NONE',  ( -38.57591613063113556, 11.89740419135774196, -94.16128332851744176 ) ) ;
#60768 = VERTEX_POINT ( 'NONE', #4173 ) ;
#60767 = CARTESIAN_POINT ( 'NONE',  ( -9.765753193741732119, 8.033970690975921869, -77.01142990352218476 ) ) ;
#60769 = CARTESIAN_POINT ( 'NONE',  ( -101.1578861705715724, 33.34056307617599657, 84.28663787432705590 ) ) ;
#60770 = CARTESIAN_POINT ( 'NONE',  ( 50.97490815085634352, 6.000000000000000000, -9.435653166495500344 ) ) ;
#60771 = FACE_BOUND ( 'NONE', #17932, .T. ) ;
#60772 = ORIENTED_EDGE ( 'NONE', *, *, #34254, .F. ) ;
#60773 = CIRCLE ( 'NONE', #50690, 125.0000000000000000 ) ;
#60774 = CARTESIAN_POINT ( 'NONE',  ( 208.0306608271317259, 112.7988899307264887, -77.39258503760095209 ) ) ;
#60775 = AXIS2_PLACEMENT_3D ( 'NONE', #65718, #55134, #43535 ) ;
#60776 = CARTESIAN_POINT ( 'NONE',  ( -38.87848244732137459, 10.93141945332450504, -16.95606301243583758 ) ) ;
#60777 = CARTESIAN_POINT ( 'NONE',  ( 156.0322512485978450, 56.54107760830848406, -89.94358864157470634 ) ) ;
#60778 = CARTESIAN_POINT ( 'NONE',  ( -131.6253556217204732, 51.61436399519942597, 6.412036120678384243 ) ) ;
#60779 = CARTESIAN_POINT ( 'NONE',  ( 17.73567516211397432, 7.577454475141602863, 57.09994424157939363 ) ) ;
#60780 = VERTEX_POINT ( 'NONE', #42143 ) ;
#60781 = ORIENTED_EDGE ( 'NONE', *, *, #68893, .F. ) ;
#60782 = ORIENTED_EDGE ( 'NONE', *, *, #69174, .T. ) ;
#60783 = CIRCLE ( 'NONE', #52892, 5.000000000000004441 ) ;
#60784 = CARTESIAN_POINT ( 'NONE',  ( 204.6977192012829789, 106.3443248447423315, -90.01503221354893469 ) ) ;
#60785 = CARTESIAN_POINT ( 'NONE',  ( -108.9145525555662033, 37.42858360505776005, 7.667561549411721522 ) ) ;
#60786 = DIRECTION ( 'NONE',  ( 1.000000000000000000, 0.000000000000000000, 0.000000000000000000 ) ) ;
#60787 = CARTESIAN_POINT ( 'NONE',  ( -37.07602570886410120, 10.58457435034603300, -47.78910661960291861 ) ) ;
#60788 = CARTESIAN_POINT ( 'NONE',  ( -97.82004213277211591, 30.57222530530879823, 85.67048935340082494 ) ) ;
#60789 = CARTESIAN_POINT ( 'NONE',  ( 64.98797965777978902, -1.250000000000021094, 170.0000000000000000 ) ) ;
#60790 = CYLINDRICAL_SURFACE ( 'NONE', #17075, 10.00000000000000000 ) ;
#60791 = CARTESIAN_POINT ( 'NONE',  ( -77.71490760329790248, 23.03637365463982434, -23.22547527094106812 ) ) ;
#60792 = ORIENTED_EDGE ( 'NONE', *, *, #31278, .F. ) ;
#60793 = CARTESIAN_POINT ( 'NONE',  ( 79.11678589158262298, 16.99307320450158443, 64.06522735529883050 ) ) ;
#60794 = ORIENTED_EDGE ( 'NONE', *, *, #46887, .F. ) ;
#60795 = CARTESIAN_POINT ( 'NONE',  ( 39.40195752203892710, 8.409560354027400209, 29.91383430596324899 ) ) ;
#60796 = B_SPLINE_CURVE_WITH_KNOTS ( 'NONE', 3,
 ( #14299, #57207, #25211, #46642, #68118, #41379, #62834, #14635, #9360, #30825, #6505, #59593, #11413, #54677, #27599, #5795, #37122, #53965, #5110, #32535, #49040, #43424, #881, #16698, #6141, #64549, #22329, #53281, #26912, #32884, #22678, #26571, #58914, #37813, #48009, #54318, #10727, #32201, #59260, #27249, #44115, #69472, #48684, #49394, #11072, #5456 ),
 .UNSPECIFIED., .F., .F.,
 ( 4, 2, 2, 2, 2, 2, 2, 2, 2, 2, 2, 2, 2, 2, 2, 2, 2, 2, 2, 2, 2, 2, 4 ),
 ( 0.000000000000000000, 0.001615199098318927107, 0.003230398196637854213, 0.004037997745797326440, 0.004845597294956798667, 0.006460796393275733580, 0.007268395942435232696, 0.008075995491594732678, 0.009691194589913694479, 0.01049879413907319099, 0.01130639368823268751, 0.01211399323739218402, 0.01292159278655168227, 0.01453679188487069784, 0.01615199098318971516, 0.01695959053234921340, 0.01776719008150871512, 0.01938238917982775325, 0.02099758827814678791, 0.02180518782730633820, 0.02261278737646588849, 0.02422798647478491274, 0.02584318557310393699 ),
 .UNSPECIFIED. ) ;
#60797 = CARTESIAN_POINT ( 'NONE',  ( 50.97490815085634352, 0.000000000000000000, -41.68900338898716740 ) ) ;
#60798 = LINE ( 'NONE', #66804, #54574 ) ;
#60799 = FACE_OUTER_BOUND ( 'NONE', #67939, .T. ) ;
#60800 = LINE ( 'NONE', #28450, #8670 ) ;
#60801 = CARTESIAN_POINT ( 'NONE',  ( -48.32993240732255913, 12.98137013984325350, 14.33474380245380431 ) ) ;
#60802 = FACE_BOUND ( 'NONE', #45578, .T. ) ;
#60803 = ADVANCED_FACE ( 'NONE', ( #14391 ), #41465, .F. ) ;
#60804 = CARTESIAN_POINT ( 'NONE',  ( 422.4999999999999432, -18.06806526123148160, 380.0000000000000000 ) ) ;
#60805 = ORIENTED_EDGE ( 'NONE', *, *, #27524, .T. ) ;
#60806 = LINE ( 'NONE', #24239, #46612 ) ;
#60807 = CARTESIAN_POINT ( 'NONE',  ( -152.9121563765243650, 67.12206067149027433, -8.781803752322767664 ) ) ;
#60808 = ORIENTED_EDGE ( 'NONE', *, *, #41454, .F. ) ;
#60809 = CARTESIAN_POINT ( 'NONE',  ( 112.3013380801408658, 388.0000000000065938, -133.9497041420121377 ) ) ;
#60810 = DIRECTION ( 'NONE',  ( 0.9195277725514489076, 0.3930250316539278810, -0.000000000000000000 ) ) ;
#60811 = CARTESIAN_POINT ( 'NONE',  ( -84.49322488516129681, 0.000000000000000000, 43.58025477438756212 ) ) ;
#60812 = VERTEX_POINT ( 'NONE', #47753 ) ;
#60813 = DIRECTION ( 'NONE',  ( 0.000000000000000000, 0.000000000000000000, -1.000000000000000000 ) ) ;
#60815 = EDGE_CURVE ( 'NONE', #63697, #33686, #45661, .T. ) ;
#60814 = CARTESIAN_POINT ( 'NONE',  ( 150.5744176759382924, 53.72473166688033075, -73.42946358852339017 ) ) ;
#60816 = CARTESIAN_POINT ( 'NONE',  ( 42.71247067544612719, 9.879726907348450382, 30.67953867783917232 ) ) ;
#60817 =( BOUNDED_CURVE ( )  B_SPLINE_CURVE ( 3, ( #25472, #30739, #62043, #36012 ),
 .UNSPECIFIED., .F., .F. ) 
 B_SPLINE_CURVE_WITH_KNOTS ( ( 4, 4 ),
 ( 3.140184917367546389E-16, 1.570796326794907882 ),
 .UNSPECIFIED. ) 
 CURVE ( )  GEOMETRIC_REPRESENTATION_ITEM ( )  RATIONAL_B_SPLINE_CURVE ( ( 1.000000000000000000, 0.8047378541243622729, 0.8047378541243622729, 1.000000000000000000 ) ) 
 REPRESENTATION_ITEM ( '' )  );
#60818 = CARTESIAN_POINT ( 'NONE',  ( 138.1919700334460401, 44.10401742531044533, -49.66122531802075457 ) ) ;
#60819 = EDGE_CURVE ( 'NONE', #53439, #24494, #47851, .T. ) ;
#60820 = ORIENTED_EDGE ( 'NONE', *, *, #41787, .T. ) ;
#60821 = ADVANCED_FACE ( 'NONE', ( #69215 ), #46378, .T. ) ;
#60822 = VECTOR ( 'NONE', #38503, 1000.000000000000000 ) ;
#60823 = CARTESIAN_POINT ( 'NONE',  ( 290.0000000000000568, -5.000000000000000888, 18.50000000000000000 ) ) ;
#60824 = ORIENTED_EDGE ( 'NONE', *, *, #9847, .F. ) ;
#60825 = CARTESIAN_POINT ( 'NONE',  ( 33.77444274891858811, 8.756048688386680823, -21.23933397304090676 ) ) ;
#60826 = DIRECTION ( 'NONE',  ( -0.7530714660036099684, -0.6579387259397136978, 0.000000000000000000 ) ) ;
#60827 = CIRCLE ( 'NONE', #59701, 75.31295361348102801 ) ;
#60828 = DIRECTION ( 'NONE',  ( 0.000000000000000000, 0.000000000000000000, -1.000000000000000000 ) ) ;
#60829 = CARTESIAN_POINT ( 'NONE',  ( 139.3117261255414121, 46.01296213310618555, 85.54168116855211679 ) ) ;
#60830 = PRODUCT_DEFINITION_SHAPE ( 'NONE', 'NONE',  #69593 ) ;
#60831 = DIRECTION ( 'NONE',  ( -0.000000000000000000, 1.000000000000000000, -0.000000000000000000 ) ) ;
#60832 = AXIS2_PLACEMENT_3D ( 'NONE', #66355, #1261, #7241 ) ;
#60834 = AXIS2_PLACEMENT_3D ( 'NONE', #26300, #65942, #65578 ) ;
#60833 = DIRECTION ( 'NONE',  ( -1.000000000000000000, -2.922263668027335568E-20, -3.557538378468060822E-20 ) ) ;
#60835 = ORIENTED_EDGE ( 'NONE', *, *, #19522, .F. ) ;
#60836 = EDGE_CURVE ( 'NONE', #40116, #41223, #21040, .T. ) ;
#60837 = CARTESIAN_POINT ( 'NONE',  ( 99.99999999999997158, 6.000000000000000000, -25.00000000000000000 ) ) ;
#60838 = ORIENTED_EDGE ( 'NONE', *, *, #38118, .F. ) ;
#60839 = CARTESIAN_POINT ( 'NONE',  ( 163.7464701930789204, 62.69993100427426214, -20.91664329413919887 ) ) ;
#60840 = CARTESIAN_POINT ( 'NONE',  ( 0.000000000000000000, 0.000000000000000000, 41.38025477438755928 ) ) ;
#60841 = DIRECTION ( 'NONE',  ( -1.000000000000000000, 0.000000000000000000, 0.000000000000000000 ) ) ;
#60842 = CARTESIAN_POINT ( 'NONE',  ( -129.1212007313910988, 49.87404947283614121, -89.31921607445420364 ) ) ;
#60843 = DIRECTION ( 'NONE',  ( -1.000000000000000000, 0.000000000000000000, 0.000000000000000000 ) ) ;
#60844 = AXIS2_PLACEMENT_3D ( 'NONE', #41176, #41865, #9860 ) ;
#60845 = VERTEX_POINT ( 'NONE', #25976 ) ;
#60846 = DIRECTION ( 'NONE',  ( -0.000000000000000000, 1.000000000000000000, -0.000000000000000000 ) ) ;
#60847 = CARTESIAN_POINT ( 'NONE',  ( 12.03194517566456234, 6.409266703743585758, 44.02472010739144537 ) ) ;
#60848 = ORIENTED_EDGE ( 'NONE', *, *, #8483, .F. ) ;
#60849 = CARTESIAN_POINT ( 'NONE',  ( -59.57733000654214095, 15.94108165424591661, -75.56201074176625809 ) ) ;
#60850 = CARTESIAN_POINT ( 'NONE',  ( 63.01563776193091826, -170.0000000000000000, 2.968410348757589023 ) ) ;
#60851 = VERTEX_POINT ( 'NONE', #63607 ) ;
#60852 = CARTESIAN_POINT ( 'NONE',  ( -142.3393481102175429, 58.33014244976923379, -71.38071900410970727 ) ) ;
#60853 = CARTESIAN_POINT ( 'NONE',  ( 93.71772995179817656, 21.96265635001559957, 12.83079813077724118 ) ) ;
#60854 = DIRECTION ( 'NONE',  ( 1.000000000000000000, 0.000000000000000000, 0.000000000000000000 ) ) ;
#60855 = ORIENTED_EDGE ( 'NONE', *, *, #34158, .F. ) ;
#60856 = LINE ( 'NONE', #371, #32305 ) ;
#60857 = CARTESIAN_POINT ( 'NONE',  ( 56.32277010625402625, 12.24595634619651641, 87.60108806781256874 ) ) ;
#60858 = CARTESIAN_POINT ( 'NONE',  ( 38.43102714813441878, 9.298961820315049920, 29.96078491149901524 ) ) ;
#60859 = CARTESIAN_POINT ( 'NONE',  ( 63.49941241090382960, 13.81848793187417535, 29.81296093922127000 ) ) ;
#60860 = CARTESIAN_POINT ( 'NONE',  ( -131.6133495896317243, 50.37677745548732133, -10.71135871446110954 ) ) ;
#60861 = CARTESIAN_POINT ( 'NONE',  ( 154.6667526376337207, 55.50347409140649546, 70.71395942990847061 ) ) ;
#60862 = CARTESIAN_POINT ( 'NONE',  ( 128.0568017572568635, 38.03085713813909052, -75.14985521657804668 ) ) ;
#60863 = VERTEX_POINT ( 'NONE', #8774 ) ;
#60864 = CARTESIAN_POINT ( 'NONE',  ( 141.3400002717723396, 47.33399859146519617, -69.80018433290322832 ) ) ;
#60865 = CARTESIAN_POINT ( 'NONE',  ( -145.5195986658808920, 62.16746116576787529, -75.51344088246251829 ) ) ;
#60866 = ORIENTED_EDGE ( 'NONE', *, *, #5150, .F. ) ;
#60867 = AXIS2_PLACEMENT_3D ( 'NONE', #5023, #37042, #67685 ) ;
#60868 = CARTESIAN_POINT ( 'NONE',  ( -150.3850953947692233, 66.25368649589884740, -34.85138302416307710 ) ) ;
#60869 = CARTESIAN_POINT ( 'NONE',  ( 205.5130322755755117, 109.1888880665735684, -9.481380442157899324 ) ) ;
#60870 = CARTESIAN_POINT ( 'NONE',  ( -37.05762690088740641, 11.60527003175541338, 32.74225044994760481 ) ) ;
#60871 = VECTOR ( 'NONE', #37929, 1000.000000000000000 ) ;
#60872 = DIRECTION ( 'NONE',  ( 0.000000000000000000, -0.000000000000000000, -1.000000000000000000 ) ) ;
#60873 = EDGE_CURVE ( 'NONE', #58260, #62528, #62574, .T. ) ;
#60874 = CARTESIAN_POINT ( 'NONE',  ( -5.888165822225389867, 7.780336669456523246, 44.86524469126863579 ) ) ;
#60875 = DIRECTION ( 'NONE',  ( 1.000000000000000000, 0.000000000000000000, 0.000000000000000000 ) ) ;
#60876 = CARTESIAN_POINT ( 'NONE',  ( -48.04019567818505010, 12.91272349839804789, -66.88950554398400072 ) ) ;
#60877 = CARTESIAN_POINT ( 'NONE',  ( -5.412684891282529165, 7.753215344827987465, -23.19184353011629796 ) ) ;
#60879 = CARTESIAN_POINT ( 'NONE',  ( -8.314488422519703548, 7.931352979988681717, 30.11558103944717857 ) ) ;
#60878 = AXIS2_PLACEMENT_3D ( 'NONE', #9928, #62707, #42277 ) ;
#60880 = AXIS2_PLACEMENT_3D ( 'NONE', #17564, #27763, #22142 ) ;
#60881 = CARTESIAN_POINT ( 'NONE',  ( 115.7746371641014775, 31.52600568297706118, 15.35476345625890460 ) ) ;
#60882 = CARTESIAN_POINT ( 'NONE',  ( 46.10482416129922001, 10.39500475043931083, -93.43768358713884936 ) ) ;
#60883 = ORIENTED_EDGE ( 'NONE', *, *, #25985, .T. ) ;
#60884 = CYLINDRICAL_SURFACE ( 'NONE', #7106, 72.99999999999998579 ) ;
#60885 = ORIENTED_EDGE ( 'NONE', *, *, #59522, .T. ) ;
#60886 = CARTESIAN_POINT ( 'NONE',  ( 2.700000000000004619, 3.061616997868383437E-15, 25.00000000000000355 ) ) ;
#60887 = CONICAL_SURFACE ( 'NONE', #9223, 74.95140232871122521, 0.8777644062502172329 ) ;
#60888 = CARTESIAN_POINT ( 'NONE',  ( 82.12277968641505765, 18.98848723477810907, -64.15117521669343148 ) ) ;
#60889 = LINE ( 'NONE', #3206, #21517 ) ;
#60890 = FACE_OUTER_BOUND ( 'NONE', #33593, .T. ) ;
#60891 = CARTESIAN_POINT ( 'NONE',  ( -55.05276343752909440, 14.68156374112637508, 18.47277718246750311 ) ) ;
#60892 = CLOSED_SHELL ( 'NONE', ( #15598, #9796, #39080, #22866, #42316, #39159, #217, #9886, #64903, #7204, #41636, #37066, #14669, #19672, #20710, #39939, #35019, #52790, #11668, #7698, #41625, #38406, #60182, #48025, #23904, #5956, #32236, #55659, #46880, #40279, #39969, #7341, #42719, #39163, #7880, #25575, #37787, #20619, #59669, #63463, #21646, #65018, #62342, #2973, #2384, #28111, #37958, #46289, #30093, #50661, #15639, #36170, #25411, #9913, #26120, #7136, #26375, #25206, #49943, #57521, #36466, #21839, #34239, #9090, #44048, #25096, #11082, #34409, #67664, #4291, #6162, #25570, #32948, #33055, #11512, #51327, #49078, #26847, #23756, #17511, #38990, #4009, #19272, #57989, #2158, #13734, #9456, #50244, #45652, #45192, #58990, #48707, #34642, #34228, #38917, #45503, #27447, #4707, #65246, #54026, #55363, #53843, #14309, #10147, #46744, #39323, #21259, #8576, #2630, #50687, #64409, #37564, #14157, #57273, #31512, #49512, #4535, #2784, #25262, #14378, #8922, #38672, #45091, #11410, #47631, #55453, #48962, #51444, #34518, #22687, #35600, #37932, #48242, #64467, #23817, #29001, #57208, #36925, #54523, #61853, #6765, #5094, #56815, #20933, #63306, #61407, #49881, #46053, #48162, #12322, #40243, #46775, #42913, #4207, #23293, #23539, #6940, #24934, #17539, #65421, #10730, #49748, #45501, #42249, #43416, #27541, #28095, #25495, #57903, #55106, #67661, #28322, #29535, #11345, #23586, #42557, #13105, #45526, #50301, #59338, #62247, #53284, #63444, #25466, #8501, #30987, #61554, #46453, #59600, #21444, #24413, #26833, #42010, #1205, #18907, #63520, #55414, #10247, #8533, #8186, #2623, #51296, #54771, #42504, #31536, #40499, #59445, #44216, #50637, #9768, #19298, #19434, #69351, #52787, #2136, #40326, #44943, #39869, #24158, #40181, #54153, #20492, #58422, #4056, #45925, #7958, #68323, #32069, #42484, #35377, #56415, #3404, #42647, #33548, #27610, #61408, #57183, #48423, #58909, #2966, #51530, #40317, #53484, #46844, #65362, #60757, #8100, #4615, #29944, #68731, #69080, #25739, #58427, #58047, #57794, #61617, #52956, #2244, #62160, #39618, #4068, #10, #5306, #56002, #43262, #32719, #12985, #40339, #23620, #16036, #20380, #14751, #24797, #14548, #8820, #68751, #13031, #21655, #24387, #64160, #9878, #20032, #43106, #685, #11108, #28922, #48405, #25185, #57190, #1179, #56082, #21622, #67377, #8276, #51954, #8180, #36281, #57662, #17724, #58592, #40064, #33506, #61012 ) ) ;
#60893 = CARTESIAN_POINT ( 'NONE',  ( 183.2136430849848239, 0.000000000000000000, -4.435653166495524324 ) ) ;
#60894 = CARTESIAN_POINT ( 'NONE',  ( -7.825402957745087207, -170.0000000000000000, 10.77103044898353090 ) ) ;
#60895 = CARTESIAN_POINT ( 'NONE',  ( -118.5151419614604436, 43.00218563933585614, -14.19961787797135422 ) ) ;
#60896 = ORIENTED_EDGE ( 'NONE', *, *, #55044, .F. ) ;
#60897 = ORIENTED_EDGE ( 'NONE', *, *, #18364, .T. ) ;
#60899 = EDGE_CURVE ( 'NONE', #9934, #18701, #46730, .T. ) ;
#60898 = CARTESIAN_POINT ( 'NONE',  ( 39.40195752203892710, 8.409560354027387774, -89.30891864635511013 ) ) ;
#60900 = CARTESIAN_POINT ( 'NONE',  ( 173.6012773665504483, 71.36035397668607061, 63.06485450500365175 ) ) ;
#60901 = CARTESIAN_POINT ( 'NONE',  ( 0.000000000000000000, 0.000000000000000000, 5.000000000000000000 ) ) ;
#60902 = CARTESIAN_POINT ( 'NONE',  ( -169.1122507277982550, 84.24359299875004581, 58.81210775617142872 ) ) ;
#60903 = PLANE ( 'NONE',  #52091 ) ;
#60904 = B_SPLINE_CURVE_WITH_KNOTS ( 'NONE', 3,
 ( #29116, #3083, #62515, #3421, #35082, #35785, #24197, #8360, #40695, #45640, #30163, #56533, #24881, #46318, #51272, #56895, #18216, #13623, #56185, #66767, #67794, #29810, #39666, #51612, #23845, #67118, #7671, #8710, #50566, #19241, #45982, #45285, #19592, #2385, #40357, #61120, #57234, #41056, #18910, #67450, #34408, #9049, #62153, #55851, #61805 ),
 .UNSPECIFIED., .F., .F.,
 ( 4, 2, 2, 1, 2, 2, 2, 2, 2, 2, 2, 2, 2, 2, 2, 2, 2, 2, 2, 2, 2, 2, 4 ),
 ( 0.02345095402629350165, 0.02491692321306680433, 0.02564990780645345914, 0.02638289239984011048, 0.02711587699322676182, 0.02784886158661341315, 0.02931483077338671930, 0.03004781536677335330, 0.03078079996015998382, 0.03224676914693325180, 0.03297975374031988927, 0.03371273833370651979, 0.03517870752047982941, 0.03664467670725313903, 0.03737766130063981118, 0.03811064589402649028, 0.03957661508079979990, 0.04104258426757310951, 0.04250855345434641913, 0.04324153804773307741, 0.04397452264111972875, 0.04544049182789304531, 0.04690646101466636186 ),
 .UNSPECIFIED. ) ;
#60905 = EDGE_CURVE ( 'NONE', #8320, #15127, #57294, .T. ) ;
#60906 = DIRECTION ( 'NONE',  ( 0.000000000000000000, 0.000000000000000000, 1.000000000000000000 ) ) ;
#60907 = ORIENTED_EDGE ( 'NONE', *, *, #48949, .F. ) ;
#60908 = CARTESIAN_POINT ( 'NONE',  ( 102.7446498997620097, 26.65764321315730356, -43.95904520983128094 ) ) ;
#60909 = CARTESIAN_POINT ( 'NONE',  ( 173.9832054143776077, 71.71542822834034325, -95.00000000000133582 ) ) ;
#60910 = CARTESIAN_POINT ( 'NONE',  ( -78.66644367742111399, 22.32174330031318021, -23.27090004125422595 ) ) ;
#60911 = DIRECTION ( 'NONE',  ( 0.000000000000000000, -1.000000000000000000, 0.000000000000000000 ) ) ;
#60912 = CARTESIAN_POINT ( 'NONE',  ( 212.0850679406004247, 117.0583048437722056, -15.64194342746143640 ) ) ;
#60913 = FACE_BOUND ( 'NONE', #29133, .T. ) ;
#60914 = ADVANCED_BREP_SHAPE_REPRESENTATION ( '', ( #18268, #66832 ), #2840 ) ;
#60915 = ADVANCED_FACE ( 'NONE', ( #14719 ), #35491, .T. ) ;
#60916 = B_SPLINE_CURVE_WITH_KNOTS ( 'NONE', 3,
 ( #58520, #3348, #24808, #46243, #62785, #20212 ),
 .UNSPECIFIED., .F., .F.,
 ( 4, 2, 4 ),
 ( 1.095770181118598899E-06, 0.03239442681617712289, 0.06478775786217312593 ),
 .UNSPECIFIED. ) ;
#60917 = ORIENTED_EDGE ( 'NONE', *, *, #65, .F. ) ;
#60918 = CARTESIAN_POINT ( 'NONE',  ( 0.000000000000000000, 0.000000000000000000, 41.38025477438755928 ) ) ;
#60919 = CARTESIAN_POINT ( 'NONE',  ( 87.59078297315397776, 20.81577753000345510, -50.77505834181354061 ) ) ;
#60920 = CIRCLE ( 'NONE', #24989, 245.3095347406802773 ) ;
#60921 = DIRECTION ( 'NONE',  ( 1.000000000000000000, 7.993605777301127091E-15, 0.000000000000000000 ) ) ;
#60922 = CARTESIAN_POINT ( 'NONE',  ( -174.7817412490652771, 90.52199442492062076, 4.151215324986693211 ) ) ;
#60923 = CARTESIAN_POINT ( 'NONE',  ( 207.4566510040494620, 111.9649643341356011, 56.57504234372401442 ) ) ;
#60924 = EDGE_CURVE ( 'NONE', #19164, #31197, #8950, .T. ) ;
#60925 = EDGE_CURVE ( 'NONE', #45135, #28312, #14182, .T. ) ;
#60926 = FACE_OUTER_BOUND ( 'NONE', #65170, .T. ) ;
#60927 = AXIS2_PLACEMENT_3D ( 'NONE', #68482, #9398, #30855 ) ;
#60928 = ORIENTED_EDGE ( 'NONE', *, *, #41241, .F. ) ;
#60929 = DIRECTION ( 'NONE',  ( -0.000000000000000000, 0.000000000000000000, -1.000000000000000000 ) ) ;
#60930 = CARTESIAN_POINT ( 'NONE',  ( -62.54085973597666026, 16.81797209566546769, 64.17062851049894334 ) ) ;
#60931 = ORIENTED_EDGE ( 'NONE', *, *, #3813, .T. ) ;
#60932 = VECTOR ( 'NONE', #52319, 1000.000000000000000 ) ;
#60933 = CARTESIAN_POINT ( 'NONE',  ( -89.99999999999998579, 1.102182119232617596E-14, -10.00000000000000000 ) ) ;
#60934 = ORIENTED_EDGE ( 'NONE', *, *, #42307, .T. ) ;
#60935 = CARTESIAN_POINT ( 'NONE',  ( -27.00000000000000355, 29.99999999999999645, 15.00000000000000000 ) ) ;
#60936 = CARTESIAN_POINT ( 'NONE',  ( -34.47910271558636452, -23.50544947846431043, 13.79046340968177020 ) ) ;
#60937 = CARTESIAN_POINT ( 'NONE',  ( 93.32228019177716760, 22.88890999585039410, -73.55979981550770219 ) ) ;
#60938 = VERTEX_POINT ( 'NONE', #5878 ) ;
#60939 = VECTOR ( 'NONE', #36548, 1000.000000000000000 ) ;
#60940 = VERTEX_POINT ( 'NONE', #22071 ) ;
#60941 = CARTESIAN_POINT ( 'NONE',  ( 41.09759788073309039, 9.651672055033845510, 71.56824425796526157 ) ) ;
#60942 = CARTESIAN_POINT ( 'NONE',  ( 158.3516718297675823, 59.61984652322053080, 29.44820441190890037 ) ) ;
#60943 = CARTESIAN_POINT ( 'NONE',  ( -152.9143627383494959, 68.46626892668652431, -62.46033273451909196 ) ) ;
#60944 = CARTESIAN_POINT ( 'NONE',  ( 65.40383840050414221, 14.27443447873230120, 3.342182201582107659 ) ) ;
#60945 = DIRECTION ( 'NONE',  ( -0.000000000000000000, -0.000000000000000000, 1.000000000000000000 ) ) ;
#60946 = ORIENTED_EDGE ( 'NONE', *, *, #11182, .F. ) ;
#60947 = CARTESIAN_POINT ( 'NONE',  ( -54.08488990389049889, 15.46443908526321742, -50.16924448875967357 ) ) ;
#60948 = CARTESIAN_POINT ( 'NONE',  ( 60.61895554631703220, 13.15982272268128384, -36.09744376541886623 ) ) ;
#60949 = CARTESIAN_POINT ( 'NONE',  ( -133.3944793432480083, 52.87251459353621641, -15.31422958618754748 ) ) ;
#60950 = CARTESIAN_POINT ( 'NONE',  ( -39.29440389294403246, -17.09499999999999886, 4.000000000000000000 ) ) ;
#60951 = CARTESIAN_POINT ( 'NONE',  ( 116.9200705848630548, 32.09536795999726166, -13.12392903560524005 ) ) ;
#60952 = CARTESIAN_POINT ( 'NONE',  ( 83.49107459963974520, 18.37327588711363191, 84.05685319569637670 ) ) ;
#60954 = ORIENTED_EDGE ( 'NONE', *, *, #41836, .T. ) ;
#60953 = DIRECTION ( 'NONE',  ( -1.000000000000000000, 0.000000000000000000, 0.000000000000000000 ) ) ;
#60955 = VERTEX_POINT ( 'NONE', #43857 ) ;
#60956 = VERTEX_POINT ( 'NONE', #38243 ) ;
#60957 = CARTESIAN_POINT ( 'NONE',  ( 45.49006904354232006, 9.279592366778883772, 6.182336992882302873 ) ) ;
#60958 = CARTESIAN_POINT ( 'NONE',  ( -180.4741487479101352, 97.29837986977219089, 93.66950218727245669 ) ) ;
#60959 = DIRECTION ( 'NONE',  ( 0.000000000000000000, 0.000000000000000000, 1.000000000000000000 ) ) ;
#60960 = EDGE_CURVE ( 'NONE', #56594, #14354, #50929, .T. ) ;
#60961 = CARTESIAN_POINT ( 'NONE',  ( 103.0103829243728910, 25.67737053862327556, -14.52816394246318055 ) ) ;
#60962 = CARTESIAN_POINT ( 'NONE',  ( 198.8687991397275994, 98.67887821384411495, 5.136872697827199019 ) ) ;
#60963 = FACE_OUTER_BOUND ( 'NONE', #53127, .T. ) ;
#60964 = DIRECTION ( 'NONE',  ( 0.000000000000000000, -1.000000000000000000, 0.000000000000000000 ) ) ;
#60965 = DIRECTION ( 'NONE',  ( -1.000000000000000000, 0.000000000000000000, 0.000000000000000000 ) ) ;
#60966 = CARTESIAN_POINT ( 'NONE',  ( -14.55390976651257162, 7.422979442794212623, 34.29323620107704329 ) ) ;
#60968 = ORIENTED_EDGE ( 'NONE', *, *, #47513, .F. ) ;
#60967 = EDGE_CURVE ( 'NONE', #47893, #48012, #38959, .T. ) ;
#60969 = LINE ( 'NONE', #22292, #59813 ) ;
#60970 = EDGE_LOOP ( 'NONE', ( #46240, #39478, #44759, #67136 ) ) ;
#60971 = ORIENTED_EDGE ( 'NONE', *, *, #27211, .F. ) ;
#60972 = CARTESIAN_POINT ( 'NONE',  ( -149.5074843970971017, 64.17983161892348676, 3.876270649435373361 ) ) ;
#60973 = CARTESIAN_POINT ( 'NONE',  ( 184.3966782763552033, 83.48172388049823667, -77.31299941553588440 ) ) ;
#60974 = CARTESIAN_POINT ( 'NONE',  ( -169.1116812882275724, 84.24296059722693997, 44.67583165595225125 ) ) ;
#60975 = CARTESIAN_POINT ( 'NONE',  ( -101.8191498210054675, 32.54686850610960391, -50.01457726497592660 ) ) ;
#60976 = CIRCLE ( 'NONE', #62131, 25.12245591505646303 ) ;
#60977 = CARTESIAN_POINT ( 'NONE',  ( 0.000000000000000000, 6.000000000000000000, -46.99999999999997158 ) ) ;
#60978 = DIRECTION ( 'NONE',  ( 0.000000000000000000, -1.000000000000000000, 0.000000000000000000 ) ) ;
#60979 = CARTESIAN_POINT ( 'NONE',  ( 136.1037846510193106, 43.98155406734452555, -9.508421591050250754 ) ) ;
#60980 = VERTEX_POINT ( 'NONE', #23122 ) ;
#60981 = EDGE_CURVE ( 'NONE', #34764, #41788, #56165, .T. ) ;
#60982 = ORIENTED_EDGE ( 'NONE', *, *, #5444, .F. ) ;
#60983 = ORIENTED_EDGE ( 'NONE', *, *, #16012, .F. ) ;
#60984 = CIRCLE ( 'NONE', #29505, 74.95140232871122521 ) ;
#60985 = EDGE_CURVE ( 'NONE', #66758, #22108, #39301, .T. ) ;
#60986 = DIRECTION ( 'NONE',  ( 0.000000000000000000, 0.000000000000000000, 1.000000000000000000 ) ) ;
#60987 = CARTESIAN_POINT ( 'NONE',  ( -14.55390976651258050, 7.422979442794215288, 7.448685610613371644 ) ) ;
#60988 = CARTESIAN_POINT ( 'NONE',  ( -36.59702023225411693, 36.46867370448659784, 26.66469066592269144 ) ) ;
#60989 = AXIS2_PLACEMENT_3D ( 'NONE', #65585, #17377, #38857 ) ;
#60990 = CARTESIAN_POINT ( 'NONE',  ( 60.62939143133410624, 12.13148391928980807, -23.50308998565268936 ) ) ;
#60991 = EDGE_CURVE ( 'NONE', #26264, #32665, #61102, .T. ) ;
#60992 = VECTOR ( 'NONE', #63133, 1000.000000000000000 ) ;
#60993 = EDGE_CURVE ( 'NONE', #52661, #12758, #56505, .T. ) ;
#60994 = CARTESIAN_POINT ( 'NONE',  ( -48.99162761293256807, 13.13973062091723776, 33.39305727236687460 ) ) ;
#60995 = LINE ( 'NONE', #59933, #52003 ) ;
#60996 = EDGE_LOOP ( 'NONE', ( #53644, #63651, #33250, #5849 ) ) ;
#60997 = CARTESIAN_POINT ( 'NONE',  ( -55.05276343752909440, 15.72344139423348786, -77.06087458892358200 ) ) ;
#60998 = CARTESIAN_POINT ( 'NONE',  ( -20.00000000000002842, -6.319444444444441089, 4.000000000000000000 ) ) ;
#60999 = DIRECTION ( 'NONE',  ( 1.000000000000000000, 0.000000000000000000, 0.000000000000000000 ) ) ;
#61000 = CARTESIAN_POINT ( 'NONE',  ( 280.0000000000000000, -21.42428528562853884, 4.999999999999990230 ) ) ;
#61001 = CARTESIAN_POINT ( 'NONE',  ( 4.590321433069001422, -24.57496590315233931, 0.000000000000000000 ) ) ;
#61002 = CARTESIAN_POINT ( 'NONE',  ( -173.1211646369891639, 87.12891641440852197, -88.40105834567665966 ) ) ;
#61003 = DIRECTION ( 'NONE',  ( -0.000000000000000000, -0.000000000000000000, -1.000000000000000000 ) ) ;
#61004 = FACE_BOUND ( 'NONE', #14272, .T. ) ;
#61005 = CARTESIAN_POINT ( 'NONE',  ( 259.2042601260359334, 188.0000000000000000, -91.27944787107685443 ) ) ;
#61006 = EDGE_CURVE ( 'NONE', #10264, #52549, #58150, .T. ) ;
#61007 = CARTESIAN_POINT ( 'NONE',  ( -4.504169684898452708, 6.697401007565304099, 71.18915580831600209 ) ) ;
#61008 = ORIENTED_EDGE ( 'NONE', *, *, #52551, .T. ) ;
#61009 = DIRECTION ( 'NONE',  ( 0.04486483035050447404, 0.9989930665413151445, -0.000000000000000000 ) ) ;
#61010 = CARTESIAN_POINT ( 'NONE',  ( 180.6710448012268841, 78.18844465372406205, 29.30859410551140698 ) ) ;
#61011 = CARTESIAN_POINT ( 'NONE',  ( 68.07999999999999829, -26.09918303830819397, 0.000000000000000000 ) ) ;
#61012 = ADVANCED_FACE ( 'NONE', ( #50887 ), #28746, .F. ) ;
#61013 = CARTESIAN_POINT ( 'NONE',  ( 0.000000000000000000, 70.00000000000000000, -60.00000000000000000 ) ) ;
#61014 = ADVANCED_FACE ( 'NONE', ( #25213 ), #19571, .F. ) ;
#61015 = CARTESIAN_POINT ( 'NONE',  ( 110.2429982417149574, -170.0000000000000000, 17.76666361527367499 ) ) ;
#61016 = EDGE_LOOP ( 'NONE', ( #56634, #66277, #16353, #2127 ) ) ;
#61017 = CARTESIAN_POINT ( 'NONE',  ( 39.40195752203891999, 9.424259417798147354, -35.61981746542776506 ) ) ;
#61018 = CARTESIAN_POINT ( 'NONE',  ( 187.7243171268374056, 85.58745653499732953, 86.99151838653519064 ) ) ;
#61019 = ORIENTED_EDGE ( 'NONE', *, *, #2875, .T. ) ;
#61020 = VERTEX_POINT ( 'NONE', #51591 ) ;
#61021 = CARTESIAN_POINT ( 'NONE',  ( 177.0075766083211875, 74.58167636505947939, -50.02476627610127480 ) ) ;
#61022 = CARTESIAN_POINT ( 'NONE',  ( -180.2252811616041868, 95.40045830523435200, -66.63472952968756147 ) ) ;
#61023 = FACE_OUTER_BOUND ( 'NONE', #19933, .T. ) ;
#61024 = EDGE_LOOP ( 'NONE', ( #47736, #44641, #57161, #32648 ) ) ;
#61025 = CARTESIAN_POINT ( 'NONE',  ( 117.7442255600442849, 33.63739995216996448, 63.45684847541002682 ) ) ;
#61026 = LINE ( 'NONE', #13198, #19906 ) ;
#61027 = CARTESIAN_POINT ( 'NONE',  ( -3.868882431147346868, 6.665575841812235502, 4.394750620680583530 ) ) ;
#61028 = VECTOR ( 'NONE', #65650, 1000.000000000000000 ) ;
#61029 = DIRECTION ( 'NONE',  ( -0.000000000000000000, 1.000000000000000000, -0.000000000000000000 ) ) ;
#61030 = CARTESIAN_POINT ( 'NONE',  ( 22.89837001126011984, 6.832355714161187699, -94.17556532809329894 ) ) ;
#61031 = VECTOR ( 'NONE', #56392, 1000.000000000000000 ) ;
#61032 = CARTESIAN_POINT ( 'NONE',  ( -47.56466076048272384, 13.83435953640667293, -16.36260880930676720 ) ) ;
#61033 = VECTOR ( 'NONE', #33480, 1000.000000000000000 ) ;
#61034 = ORIENTED_EDGE ( 'NONE', *, *, #58848, .F. ) ;
#61035 = AXIS2_PLACEMENT_3D ( 'NONE', #68534, #18963, #40757 ) ;
#61036 = DIRECTION ( 'NONE',  ( -0.2225209339563184452, 0.9749279121818226201, 5.146830507070804164E-17 ) ) ;
#61037 = CARTESIAN_POINT ( 'NONE',  ( -72.77296415263758433, 21.23032531836538084, 6.408587851164161187 ) ) ;
#61038 = CARTESIAN_POINT ( 'NONE',  ( 0.000000000000000000, 9.797174393178825657E-16, -8.000000000000000000 ) ) ;
#61039 = CARTESIAN_POINT ( 'NONE',  ( -173.1211646369891355, 88.63826465341151106, -76.55650775521370122 ) ) ;
#61041 = ORIENTED_EDGE ( 'NONE', *, *, #31048, .T. ) ;
#61040 = CARTESIAN_POINT ( 'NONE',  ( -123.7039169285859828, 45.06792368978931052, 84.61315978542810967 ) ) ;
#61042 = CARTESIAN_POINT ( 'NONE',  ( 80.73012746365749592, 17.49169339352364361, -38.66384684947503558 ) ) ;
#61043 = AXIS2_PLACEMENT_3D ( 'NONE', #25094, #30364, #51816 ) ;
#61044 = ORIENTED_EDGE ( 'NONE', *, *, #51765, .F. ) ;
#61045 = FACE_OUTER_BOUND ( 'NONE', #53303, .T. ) ;
#61046 = CARTESIAN_POINT ( 'NONE',  ( 79.14113188808480004, 18.05280674635442750, 37.70299700396097364 ) ) ;
#61047 = DIRECTION ( 'NONE',  ( 0.000000000000000000, 0.000000000000000000, 1.000000000000000000 ) ) ;
#61048 = DIRECTION ( 'NONE',  ( -1.000000000000000000, 0.000000000000000000, 0.000000000000000000 ) ) ;
#61049 = CARTESIAN_POINT ( 'NONE',  ( 140.5781926063689298, 45.63383190293698988, -20.01610080164386929 ) ) ;
#61050 = CARTESIAN_POINT ( 'NONE',  ( 412.3372781065086770, 0.000000000000000000, -146.4497041420118251 ) ) ;
#61051 = CARTESIAN_POINT ( 'NONE',  ( -173.1211646369891355, 88.63826465341152527, -7.867406574286299303 ) ) ;
#61052 = EDGE_CURVE ( 'NONE', #23096, #13308, #11962, .T. ) ;
#61053 = DIRECTION ( 'NONE',  ( -1.000000000000000000, -0.000000000000000000, -0.000000000000000000 ) ) ;
#61054 = ORIENTED_EDGE ( 'NONE', *, *, #4456, .F. ) ;
#61055 = APPLICATION_CONTEXT ( 'automotive_design' ) ;
#61056 = VERTEX_POINT ( 'NONE', #57555 ) ;
#61057 = CARTESIAN_POINT ( 'NONE',  ( 311.9975424824652350, 296.0000000000000000, 420.0000000000000000 ) ) ;
#61058 = CARTESIAN_POINT ( 'NONE',  ( -72.62976060914719767, -18.74780984163136566, 170.0000000000000000 ) ) ;
#61059 = DIRECTION ( 'NONE',  ( -0.000000000000000000, -0.000000000000000000, 1.000000000000000000 ) ) ;
#61060 = CARTESIAN_POINT ( 'NONE',  ( -24.53636015449790264, 60.58612729876396941, 6.377659838150179840E-18 ) ) ;
#61061 = DIRECTION ( 'NONE',  ( -1.000000000000000000, 0.000000000000000000, 0.000000000000000000 ) ) ;
#61062 = CARTESIAN_POINT ( 'NONE',  ( -102.7502407665687230, 33.01985383847077316, 72.36362509687882039 ) ) ;
#61063 = CARTESIAN_POINT ( 'NONE',  ( -24.41864932425148282, 8.543938959778818898, -40.16677908042758105 ) ) ;
#61064 = CARTESIAN_POINT ( 'NONE',  ( 164.8407099662995279, 63.61629583487390960, -71.88438285980473097 ) ) ;
#61065 = VERTEX_POINT ( 'NONE', #15333 ) ;
#61066 = EDGE_CURVE ( 'NONE', #9408, #58973, #65864, .T. ) ;
#61067 = VERTEX_POINT ( 'NONE', #35761 ) ;
#61069 = ORIENTED_EDGE ( 'NONE', *, *, #32224, .T. ) ;
#61068 = B_SPLINE_CURVE_WITH_KNOTS ( 'NONE', 3,
 ( #20087, #3557, #25028, #41542, #8148, #40497, #56682, #67943, #62995, #29952, #62659, #36264, #57722, #2528, #45432, #66912, #18707, #61613 ),
 .UNSPECIFIED., .F., .F.,
 ( 4, 2, 2, 2, 2, 2, 2, 2, 4 ),
 ( 0.01001677236965714708, 0.01126784864425927138, 0.01251892491886139568, 0.01377000119346351997, 0.01502107746806564254, 0.01627215374266776857, 0.01752323001726989113, 0.01877430629187201716, 0.02002538256647413972 ),
 .UNSPECIFIED. ) ;
#61070 = DIRECTION ( 'NONE',  ( -2.692596297684568294E-16, -1.000000000000000000, 1.133976529980832822E-16 ) ) ;
#61071 = AXIS2_PLACEMENT_3D ( 'NONE', #431, #5368, #16606 ) ;
#61072 = CARTESIAN_POINT ( 'NONE',  ( -77.47632222052990869, 21.87111359341350791, 84.17632590412091531 ) ) ;
#61073 = CARTESIAN_POINT ( 'NONE',  ( -79.61931371420115511, 22.68640080971621487, 72.21703544022015819 ) ) ;
#61074 = CARTESIAN_POINT ( 'NONE',  ( 98.48662049252141060, -156.6058287036421177, 0.000000000000000000 ) ) ;
#61075 = CARTESIAN_POINT ( 'NONE',  ( 10.55634918610400419, -15.55634918610406103, 2.000000000000001776 ) ) ;
#61076 = EDGE_CURVE ( 'NONE', #5356, #15020, #40673, .T. ) ;
#61077 = DIRECTION ( 'NONE',  ( -0.000000000000000000, 0.000000000000000000, -1.000000000000000000 ) ) ;
#61078 = AXIS2_PLACEMENT_3D ( 'NONE', #39012, #43910, #49532 ) ;
#61079 = CARTESIAN_POINT ( 'NONE',  ( -95.05323930133207000, 30.36974142673411237, -13.59935561858418396 ) ) ;
#61080 = VECTOR ( 'NONE', #2261, 999.9999999999998863 ) ;
#61081 = CARTESIAN_POINT ( 'NONE',  ( 55.76255201544533691, 12.13275766515751997, 35.34123246681144082 ) ) ;
#61082 = CARTESIAN_POINT ( 'NONE',  ( 35.34747263975754805, 7.916651221204775268, 84.78471632296681548 ) ) ;
#61083 = DIRECTION ( 'NONE',  ( 0.000000000000000000, 1.000000000000000000, 0.000000000000000000 ) ) ;
#61084 = ORIENTED_EDGE ( 'NONE', *, *, #64555, .F. ) ;
#61085 = CARTESIAN_POINT ( 'NONE',  ( 197.6319840686292082, 97.13072366387987699, -95.00000000000133582 ) ) ;
#61086 = FACE_BOUND ( 'NONE', #19919, .T. ) ;
#61087 = CARTESIAN_POINT ( 'NONE',  ( -14.92860730136983705, 8.468845235798738713, 8.351230680223016734 ) ) ;
#61088 = AXIS2_PLACEMENT_3D ( 'NONE', #31402, #41950, #26117 ) ;
#61089 = CYLINDRICAL_SURFACE ( 'NONE', #6276, 65.00000000000000000 ) ;
#61090 = CARTESIAN_POINT ( 'NONE',  ( 197.6316695787931508, 97.13022718399028577, 66.08436601712787706 ) ) ;
#61091 = VECTOR ( 'NONE', #8154, 1000.000000000000000 ) ;
#61092 = CARTESIAN_POINT ( 'NONE',  ( 133.4058733589413350, 42.32720528873925758, -24.17876034193200852 ) ) ;
#61093 = AXIS2_PLACEMENT_3D ( 'NONE', #10298, #11335, #10994 ) ;
#61094 = ORIENTED_EDGE ( 'NONE', *, *, #29125, .F. ) ;
#61096 = VECTOR ( 'NONE', #30804, 1000.000000000000000 ) ;
#61095 = PRODUCT_CONTEXT ( 'NONE', #46670, 'mechanical' ) ;
#61097 = CYLINDRICAL_SURFACE ( 'NONE', #11604, 65.36598343705435354 ) ;
#61098 = CARTESIAN_POINT ( 'NONE',  ( -32.41898580403142205, 10.77423026598439471, -35.36526679678951979 ) ) ;
#61099 = EDGE_CURVE ( 'NONE', #67205, #17944, #12306, .T. ) ;
#61100 = DIRECTION ( 'NONE',  ( -0.000000000000000000, -0.000000000000000000, 1.000000000000000000 ) ) ;
#61101 = ITEM_DEFINED_TRANSFORMATION ( 'NONE', 'NONE', #1845,  #66832 ) ;
#61102 = LINE ( 'NONE', #61448, #67024 ) ;
#61103 = ORIENTED_EDGE ( 'NONE', *, *, #58160, .F. ) ;
#61104 = CARTESIAN_POINT ( 'NONE',  ( -118.5043919384111604, 41.81711884544880320, -41.10325547692050918 ) ) ;
#61105 = ADVANCED_FACE ( 'NONE', ( #26573 ), #175, .T. ) ;
#61106 = CARTESIAN_POINT ( 'NONE',  ( -142.0902782307735208, 58.13494170556001706, -16.61472388644448372 ) ) ;
#61107 = CARTESIAN_POINT ( 'NONE',  ( -1.862553927312061042, 7.582910205528087033, -74.33794145251196994 ) ) ;
#61108 = DIRECTION ( 'NONE',  ( 1.000000000000000000, 0.000000000000000000, 0.000000000000000000 ) ) ;
#61109 = ORIENTED_EDGE ( 'NONE', *, *, #46122, .T. ) ;
#61110 = DIRECTION ( 'NONE',  ( 0.000000000000000000, -1.000000000000000000, -2.184185950696548891E-33 ) ) ;
#61111 = CARTESIAN_POINT ( 'NONE',  ( 203.9181091394787586, 105.2759068139671115, -36.32593103262158252 ) ) ;
#61112 = DIRECTION ( 'NONE',  ( 1.000000000000000000, 0.000000000000000000, 0.000000000000000000 ) ) ;
#61113 = CARTESIAN_POINT ( 'NONE',  ( 23.09541709302173018, 6.844586979481618982, -44.72642228744273041 ) ) ;
#61115 = VERTEX_POINT ( 'NONE', #15676 ) ;
#61114 = CARTESIAN_POINT ( 'NONE',  ( -55.05276343752910151, 14.68156374112636620, 3.472777182467474244 ) ) ;
#61116 = DIRECTION ( 'NONE',  ( 0.000000000000000000, -1.000000000000000000, -0.000000000000000000 ) ) ;
#61117 = VERTEX_POINT ( 'NONE', #21978 ) ;
#61118 = ORIENTED_EDGE ( 'NONE', *, *, #44854, .T. ) ;
#61119 = CARTESIAN_POINT ( 'NONE',  ( -173.1211646369891071, 88.63826465341152527, 18.97714401617737323 ) ) ;
#61120 = CARTESIAN_POINT ( 'NONE',  ( 20.37135563017390893, 6.690359945346061821, -63.90633550731507029 ) ) ;
#61121 = AXIS2_PLACEMENT_3D ( 'NONE', #56139, #8658, #61421 ) ;
#61123 = ORIENTED_EDGE ( 'NONE', *, *, #43505, .F. ) ;
#61122 = CARTESIAN_POINT ( 'NONE',  ( -15.32495246574475090, 8.506829480038508251, -70.26458035401391555 ) ) ;
#61124 = CARTESIAN_POINT ( 'NONE',  ( -94.85411614066488539, 30.27638713119805303, 92.81031322454776955 ) ) ;
#61125 = CARTESIAN_POINT ( 'NONE',  ( -23.93933407965395332, 9.495050561681672718, 38.21205357566448413 ) ) ;
#61126 = CARTESIAN_POINT ( 'NONE',  ( -78.66644367742111399, 23.39876645725287219, -50.11545063171791270 ) ) ;
#61127 = PRODUCT_RELATED_PRODUCT_CATEGORY ( 'part', '', ( #34472 ) ) ;
#61128 = AXIS2_PLACEMENT_3D ( 'NONE', #60811, #29162, #50612 ) ;
#61129 = ORIENTED_EDGE ( 'NONE', *, *, #7474, .F. ) ;
#61130 = CARTESIAN_POINT ( 'NONE',  ( 212.0803491126036988, 118.9047894217573287, -69.30594524286756553 ) ) ;
#61131 = AXIS2_PLACEMENT_3D ( 'NONE', #55268, #38396, #21866 ) ;
#61132 = ADVANCED_FACE ( 'NONE', ( #5112 ), #54320, .F. ) ;
#61133 = VECTOR ( 'NONE', #40261, 1000.000000000000000 ) ;
#61134 = CARTESIAN_POINT ( 'NONE',  ( 140.4641697461912884, 46.75994457266055093, 40.59688181447199185 ) ) ;
#61135 = ADVANCED_FACE ( 'NONE', ( #65243 ), #26232, .T. ) ;
#61136 = CARTESIAN_POINT ( 'NONE',  ( -173.5422248620772052, 89.11126078969412845, 45.82169460664104577 ) ) ;
#61137 = VECTOR ( 'NONE', #67520, 1000.000000000000000 ) ;
#61138 = CARTESIAN_POINT ( 'NONE',  ( 110.2429982417149574, -170.0000000000000000, -43.42243756565370205 ) ) ;
#61139 = DIRECTION ( 'NONE',  ( 0.000000000000000000, 0.000000000000000000, 1.000000000000000000 ) ) ;
#61140 = ORIENTED_EDGE ( 'NONE', *, *, #58570, .F. ) ;
#61141 = ORIENTED_EDGE ( 'NONE', *, *, #34429, .F. ) ;
#61142 = ORIENTED_EDGE ( 'NONE', *, *, #65288, .F. ) ;
#61143 = DIRECTION ( 'NONE',  ( -0.000000000000000000, -0.000000000000000000, -1.000000000000000000 ) ) ;
#61144 =( NAMED_UNIT ( * ) SI_UNIT ( $, .STERADIAN. ) SOLID_ANGLE_UNIT ( ) );
#61145 = CARTESIAN_POINT ( 'NONE',  ( -33.37566357177429666, 9.916833145467597532, -50.07922491613769012 ) ) ;
#61146 = DIRECTION ( 'NONE',  ( 1.000000000000000000, 0.000000000000000000, 0.000000000000000000 ) ) ;
#61147 = CARTESIAN_POINT ( 'NONE',  ( -142.3178993725749137, 58.31327888234797285, 40.42933480981873373 ) ) ;
#61148 = CARTESIAN_POINT ( 'NONE',  ( 43.10136218933562446, -39.31639513875150982, 27.58472315868180402 ) ) ;
#61149 = CYLINDRICAL_SURFACE ( 'NONE', #29555, 299.9999999999999432 ) ;
#61150 = EDGE_CURVE ( 'NONE', #32488, #9160, #42740, .T. ) ;
#61151 = ORIENTED_EDGE ( 'NONE', *, *, #56333, .T. ) ;
#61152 = DIRECTION ( 'NONE',  ( -0.000000000000000000, -0.000000000000000000, 1.000000000000000000 ) ) ;
#61153 = VERTEX_POINT ( 'NONE', #53967 ) ;
#61154 = CARTESIAN_POINT ( 'NONE',  ( 38.42384008295177722, 8.283891555743464252, 44.86569254733282008 ) ) ;
#61155 = DIRECTION ( 'NONE',  ( -1.000000000000000000, 0.000000000000000000, 0.000000000000000000 ) ) ;
#61156 = EDGE_CURVE ( 'NONE', #5523, #56201, #64551, .T. ) ;
#61157 = CARTESIAN_POINT ( 'NONE',  ( 133.8566784816069060, 42.60093787723655367, 17.66579024853170310 ) ) ;
#61158 = DIRECTION ( 'NONE',  ( -0.000000000000000000, -0.000000000000000000, -1.000000000000000000 ) ) ;
#61159 = EDGE_CURVE ( 'NONE', #33533, #60292, #2223, .T. ) ;
#61160 = SURFACE_SIDE_STYLE ('',( #61508 ) ) ;
#61161 = CARTESIAN_POINT ( 'NONE',  ( -118.4709174626548531, 42.97515378817185194, 66.07066160974568447 ) ) ;
#61162 = CARTESIAN_POINT ( 'NONE',  ( -102.2801239173131194, -170.0000000000000000, 3.674523915951417141 ) ) ;
#61163 = CARTESIAN_POINT ( 'NONE',  ( 73.57152302639893549, 14.62167909564604429, 170.0000000000000000 ) ) ;
#61164 = CARTESIAN_POINT ( 'NONE',  ( 47.73902449248994628, 57.85799893277891215, 170.0000000000000000 ) ) ;
#61165 = ORIENTED_EDGE ( 'NONE', *, *, #17807, .F. ) ;
#61166 = FACE_OUTER_BOUND ( 'NONE', #34894, .T. ) ;
#61167 = CARTESIAN_POINT ( 'NONE',  ( -149.5074843970971017, 64.17983161892347255, -7.968279941028269420 ) ) ;
#61168 = ORIENTED_EDGE ( 'NONE', *, *, #26104, .T. ) ;
#61169 = LINE ( 'NONE', #12994, #64542 ) ;
#61170 = CARTESIAN_POINT ( 'NONE',  ( -62.54086041493280135, 17.86944394914988976, 65.15299748377630351 ) ) ;
#61171 = CARTESIAN_POINT ( 'NONE',  ( 86.62931800182293784, -170.0000000000000000, -62.66611478937537782 ) ) ;
#61172 = ORIENTED_EDGE ( 'NONE', *, *, #3482, .T. ) ;
#61173 = DIRECTION ( 'NONE',  ( 0.6910626489868685329, -0.7227948638273878901, 0.000000000000000000 ) ) ;
#61174 = CARTESIAN_POINT ( 'NONE',  ( 150.5538013146980347, 53.70974888488127874, -67.55639953143700893 ) ) ;
#61175 = CARTESIAN_POINT ( 'NONE',  ( -38.93922791710217979, 10.94334660650242341, 37.47454328655717148 ) ) ;
#61176 = CARTESIAN_POINT ( 'NONE',  ( 140.4586216751745269, 45.55624550472995793, -47.09120538612899765 ) ) ;
#61177 = VECTOR ( 'NONE', #37151, 1000.000000000000000 ) ;
#61178 = ORIENTED_EDGE ( 'NONE', *, *, #11347, .F. ) ;
#61179 = DIRECTION ( 'NONE',  ( 1.015474350197485566E-14, -0.9999999999999998890, -4.104355744161124008E-15 ) ) ;
#61180 = CARTESIAN_POINT ( 'NONE',  ( -122.7930600691577752, 44.48546375740916403, 44.96461390212944309 ) ) ;
#61181 = ORIENTED_EDGE ( 'NONE', *, *, #32554, .F. ) ;
#61182 = CARTESIAN_POINT ( 'NONE',  ( 38.90907126433565111, 9.359889524363177671, -8.775266874964067654 ) ) ;
#61183 = LINE ( 'NONE', #43937, #47300 ) ;
#61184 = AXIS2_PLACEMENT_3D ( 'NONE', #5103, #43415, #47658 ) ;
#61185 = PLANE ( 'NONE',  #40878 ) ;
#61186 = CARTESIAN_POINT ( 'NONE',  ( 127.3308700373269886, 38.77640327688543209, 86.99888605803015196 ) ) ;
#61187 = VECTOR ( 'NONE', #6215, 1000.000000000000000 ) ;
#61188 = EDGE_CURVE ( 'NONE', #34341, #48842, #17397, .T. ) ;
#61189 = CARTESIAN_POINT ( 'NONE',  ( 199.6029099983328479, 101.2457601186893612, -91.99728860495294214 ) ) ;
#61190 = AXIS2_PLACEMENT_3D ( 'NONE', #41400, #14654, #4109 ) ;
#61191 = LINE ( 'NONE', #60488, #23680 ) ;
#61192 = CIRCLE ( 'NONE', #3944, 10.00000000000000000 ) ;
#61193 = CARTESIAN_POINT ( 'NONE',  ( 76.57571471437145760, 10.00000000000000000, -20.00000000000000000 ) ) ;
#61194 = EDGE_LOOP ( 'NONE', ( #48299, #55966, #68599, #45605 ) ) ;
#61195 = CARTESIAN_POINT ( 'NONE',  ( 160.9069879467681403, 60.37290772564308128, -23.46207914634777936 ) ) ;
#61196 = CARTESIAN_POINT ( 'NONE',  ( -31.43908319763709969, 10.61114334766716638, -77.16174795566554678 ) ) ;
#61197 = DIRECTION ( 'NONE',  ( 0.9362348706397417564, -0.3513748240813305279, 0.000000000000000000 ) ) ;
#61198 = CARTESIAN_POINT ( 'NONE',  ( -133.3122825023497171, 52.81354457049841500, -95.00000000000133582 ) ) ;
#61199 = PLANE ( 'NONE',  #35282 ) ;
#61200 = ORIENTED_EDGE ( 'NONE', *, *, #16818, .F. ) ;
#61201 = CARTESIAN_POINT ( 'NONE',  ( 164.1338586910085837, 64.33646242148854810, -13.32728364527724807 ) ) ;
#61202 = LINE ( 'NONE', #22870, #9309 ) ;
#61203 = VERTEX_POINT ( 'NONE', #12135 ) ;
#61204 = CARTESIAN_POINT ( 'NONE',  ( -61.39252081892700375, 16.47343302442957835, -73.57560269778032591 ) ) ;
#61205 = CARTESIAN_POINT ( 'NONE',  ( 133.4819570657469683, 41.19842572144921178, -89.71241211332299770 ) ) ;
#61206 = ORIENTED_EDGE ( 'NONE', *, *, #50686, .F. ) ;
#61207 = CARTESIAN_POINT ( 'NONE',  ( -142.0251973982164486, 58.08401473564114070, -69.74446058856305797 ) ) ;
#61208 = DIRECTION ( 'NONE',  ( -0.000000000000000000, 1.000000000000000000, -0.000000000000000000 ) ) ;
#61209 = EDGE_CURVE ( 'NONE', #28546, #16482, #44485, .T. ) ;
#61210 = CARTESIAN_POINT ( 'NONE',  ( 164.3577270662354124, 63.21061577643033758, -46.60488526209466187 ) ) ;
#61211 = EDGE_CURVE ( 'NONE', #14663, #17465, #28302, .T. ) ;
#61212 = ORIENTED_EDGE ( 'NONE', *, *, #19516, .F. ) ;
#61213 = CARTESIAN_POINT ( 'NONE',  ( 0.000000000000000000, 0.000000000000000000, 0.000000000000000000 ) ) ;
#61214 = EDGE_CURVE ( 'NONE', #36547, #18072, #49741, .T. ) ;
#61215 = CARTESIAN_POINT ( 'NONE',  ( -102.2801239173131194, 33.91021738430207932, 45.51907450641513009 ) ) ;
#61216 = CARTESIAN_POINT ( 'NONE',  ( 74.62299871641508275, -5.461138973197949831, 170.0000000000000000 ) ) ;
#61217 = CARTESIAN_POINT ( 'NONE',  ( 79.54836217416615796, 18.17815803851261336, -18.96166302950352645 ) ) ;
#61218 = EDGE_CURVE ( 'NONE', #64743, #10732, #8565, .T. ) ;
#61219 = CARTESIAN_POINT ( 'NONE',  ( -132.0958200534848004, 50.71531800824801195, -19.79385869415553856 ) ) ;
#61220 = CARTESIAN_POINT ( 'NONE',  ( 39.40195752203892710, 9.424259417798138472, -89.30891864635511013 ) ) ;
#61221 = CARTESIAN_POINT ( 'NONE',  ( 149.0250918491436494, 6.000000000000000000, -41.68900338898718871 ) ) ;
#61222 = ORIENTED_EDGE ( 'NONE', *, *, #24163, .F. ) ;
#61223 = CARTESIAN_POINT ( 'NONE',  ( -15.67984581960975632, -63.08044415722883969, 40.00000000000003553 ) ) ;
#61224 = FACE_OUTER_BOUND ( 'NONE', #8999, .T. ) ;
#61225 = VERTEX_POINT ( 'NONE', #65965 ) ;
#61226 = VECTOR ( 'NONE', #49608, 1000.000000000000000 ) ;
#61227 = EDGE_CURVE ( 'NONE', #63672, #59242, #17763, .T. ) ;
#61228 = CARTESIAN_POINT ( 'NONE',  ( -149.9475539515598257, 65.87716206616009629, -34.81283053149195439 ) ) ;
#61229 = FACE_OUTER_BOUND ( 'NONE', #13156, .T. ) ;
#61230 = CIRCLE ( 'NONE', #32003, 5.000000000000004441 ) ;
#61231 = VECTOR ( 'NONE', #14962, 1000.000000000000000 ) ;
#61232 = CARTESIAN_POINT ( 'NONE',  ( -447.6627218934913799, 389.9999999999998295, -141.4497041420118535 ) ) ;
#61233 = CARTESIAN_POINT ( 'NONE',  ( 211.9972138934681425, 190.0000000000000000, 276.7374251518728556 ) ) ;
#61234 = DIRECTION ( 'NONE',  ( -0.000000000000000000, 1.000000000000000000, -0.000000000000000000 ) ) ;
#61235 = CARTESIAN_POINT ( 'NONE',  ( -49.11825192196926793, 13.17012322555987858, -64.94842763682078157 ) ) ;
#61236 = DIRECTION ( 'NONE',  ( -0.7071067811865474617, -9.058225723175622340E-16, 0.7071067811865474617 ) ) ;
#61237 = AXIS2_PLACEMENT_3D ( 'NONE', #21395, #48446, #11183 ) ;
#61238 = CARTESIAN_POINT ( 'NONE',  ( -14.92860730136983882, 8.468845235798742266, 35.19578127068669460 ) ) ;
#61239 = CARTESIAN_POINT ( 'NONE',  ( -59.94781924509479865, 16.04872117907065032, 16.66037302724637925 ) ) ;
#61240 = ORIENTED_EDGE ( 'NONE', *, *, #49938, .T. ) ;
#61242 = VECTOR ( 'NONE', #557, 1000.000000000000000 ) ;
#61241 = CARTESIAN_POINT ( 'NONE',  ( -12.77952633087691403, 21.62918162951106993, 0.000000000000000000 ) ) ;
#61243 = ORIENTED_EDGE ( 'NONE', *, *, #25435, .T. ) ;
#61244 = CARTESIAN_POINT ( 'NONE',  ( 60.58000000000000540, -26.09918303830819397, 15.41169613715280562 ) ) ;
#61245 = EDGE_CURVE ( 'NONE', #54323, #27270, #37759, .T. ) ;
#61246 = CARTESIAN_POINT ( 'NONE',  ( 42.71680114082826663, 9.880016734137544887, -9.529744981248345681 ) ) ;
#61247 = EDGE_CURVE ( 'NONE', #10412, #27437, #44117, .T. ) ;
#61248 = DIRECTION ( 'NONE',  ( -0.9989930665413143673, -0.04486483035051862939, 0.000000000000000000 ) ) ;
#61249 = PLANE ( 'NONE',  #45717 ) ;
#61250 = CARTESIAN_POINT ( 'NONE',  ( 61.94551923608091926, -24.58367728653112039, 34.48241795236666718 ) ) ;
#61251 = CARTESIAN_POINT ( 'NONE',  ( 5.799999999999999822, 9.237604307034018802, 0.000000000000000000 ) ) ;
#61252 = CARTESIAN_POINT ( 'NONE',  ( -77.02372450489328060, 21.70271995013164101, 57.44099635086979561 ) ) ;
#61253 = CARTESIAN_POINT ( 'NONE',  ( -169.1005390226460179, 82.76152663947084420, 71.51309903033511262 ) ) ;
#61254 = VERTEX_POINT ( 'NONE', #50464 ) ;
#61255 = ORIENTED_EDGE ( 'NONE', *, *, #13823, .T. ) ;
#61256 = FACE_BOUND ( 'NONE', #30617, .T. ) ;
#61257 = DIRECTION ( 'NONE',  ( 1.000000000000000000, 0.000000000000000000, 0.000000000000000000 ) ) ;
#61258 = CARTESIAN_POINT ( 'NONE',  ( -20.55634918610408945, -31.11269837220804035, 85.00100000000000477 ) ) ;
#61259 = CARTESIAN_POINT ( 'NONE',  ( 105.4134760436918583, 27.80903124201758558, 69.71480060533734502 ) ) ;
#61260 = DIRECTION ( 'NONE',  ( -0.000000000000000000, -0.000000000000000000, -1.000000000000000000 ) ) ;
#61261 = LINE ( 'NONE', #44737, #22931 ) ;
#61262 = VERTEX_POINT ( 'NONE', #66657 ) ;
#61263 = CARTESIAN_POINT ( 'NONE',  ( 88.53025347111699261, 21.14438024052373422, 3.096674985598131258 ) ) ;
#61264 = CARTESIAN_POINT ( 'NONE',  ( 22.15926701483428474, 7.796117250416237709, -39.05393624471034286 ) ) ;
#61265 = DIRECTION ( 'NONE',  ( -0.7071067811865474617, 0.000000000000000000, 0.7071067811865475727 ) ) ;
#61266 = DIRECTION ( 'NONE',  ( 0.000000000000000000, 0.000000000000000000, -1.000000000000000000 ) ) ;
#61267 = CARTESIAN_POINT ( 'NONE',  ( 210.9747454890631388, 115.3673079504856105, -12.86836890806030276 ) ) ;
#61268 = FACE_BOUND ( 'NONE', #14442, .T. ) ;
#61269 = VECTOR ( 'NONE', #20802, 1000.000000000000227 ) ;
#61270 = VERTEX_POINT ( 'NONE', #13528 ) ;
#61271 = DIRECTION ( 'NONE',  ( -0.000000000000000000, -0.000000000000000000, -1.000000000000000000 ) ) ;
#61272 = CARTESIAN_POINT ( 'NONE',  ( 86.62931800182293784, 20.48449268398422873, -50.82156419891174437 ) ) ;
#61273 = CARTESIAN_POINT ( 'NONE',  ( 38.91512155099545112, 9.360679678889628264, -77.46436805589146957 ) ) ;
#61274 = LINE ( 'NONE', #34564, #55703 ) ;
#61275 = CARTESIAN_POINT ( 'NONE',  ( 211.8382652195005846, 118.5282575235989384, 65.86877708187445535 ) ) ;
#61276 = LINE ( 'NONE', #33518, #41193 ) ;
#61277 = VECTOR ( 'NONE', #21115, 1000.000000000000000 ) ;
#61278 = VECTOR ( 'NONE', #31506, 1000.000000000000114 ) ;
#61279 = ORIENTED_EDGE ( 'NONE', *, *, #64959, .F. ) ;
#61280 = AXIS2_PLACEMENT_3D ( 'NONE', #9103, #21035, #41800 ) ;
#61281 = DIRECTION ( 'NONE',  ( 1.000000000000000000, 0.000000000000000000, 0.000000000000000000 ) ) ;
#61282 = VECTOR ( 'NONE', #15009, 1000.000000000000000 ) ;
#61283 = CARTESIAN_POINT ( 'NONE',  ( -8.000000000000000000, -4.618802153517024500, -8.785468820183664818 ) ) ;
#61284 = EDGE_LOOP ( 'NONE', ( #36811, #46695, #8535, #55483 ) ) ;
#61285 = DIRECTION ( 'NONE',  ( 0.000000000000000000, 0.000000000000000000, -1.000000000000000000 ) ) ;
#61286 = EDGE_LOOP ( 'NONE', ( #27092, #60591 ) ) ;
#61287 = AXIS2_PLACEMENT_3D ( 'NONE', #43979, #17253, #38724 ) ;
#61288 = CARTESIAN_POINT ( 'NONE',  ( -83.52505811737952968, 24.23179517241435832, -75.19473686439705773 ) ) ;
#61289 = CARTESIAN_POINT ( 'NONE',  ( -62.55184817504198946, 17.87278652436698323, -16.38738335002791047 ) ) ;
#61290 = CARTESIAN_POINT ( 'NONE',  ( 93.43270425363547815, 22.93046121381055968, -73.33260761053102783 ) ) ;
#61291 = ORIENTED_EDGE ( 'NONE', *, *, #10134, .T. ) ;
#61292 = ORIENTED_EDGE ( 'NONE', *, *, #66988, .F. ) ;
#61293 = CARTESIAN_POINT ( 'NONE',  ( 8.683531412707429453, 6.377173148747127485, -40.60382404160758796 ) ) ;
#61294 = CARTESIAN_POINT ( 'NONE',  ( -105.7402726937670678, 35.71226297334109034, -89.54607016031067701 ) ) ;
#61295 = CARTESIAN_POINT ( 'NONE',  ( 19.10216788411014122, 6.629360741291161041, 3.937534161706087943 ) ) ;
#61296 = ORIENTED_EDGE ( 'NONE', *, *, #34141, .F. ) ;
#61297 = B_SPLINE_CURVE_WITH_KNOTS ( 'NONE', 3,
 ( #58812, #422, #5008, #20491, #26473, #10623, #11312, #41959, #31409, #52838, #4662, #7095, #6744, #48935, #28555, #49289, #39805, #27496, #23632, #17655, #39454, #50362, #28193, #16939, #49642, #50000, #45070, #43665, #65856, #34193, #12028, #6036, #1470, #60207, #2177, #32784, #1833, #6400, #66555, #44018, #18342, #22930, #23291, #54573, #44736, #12725 ),
 .UNSPECIFIED., .F., .F.,
 ( 4, 2, 2, 2, 2, 2, 2, 2, 2, 2, 2, 2, 2, 2, 2, 2, 2, 2, 2, 2, 2, 2, 4 ),
 ( 1.398578778534940505E-17, 0.003635178948345853429, 0.005452768422518746751, 0.007270357896691640072, 0.008179152633778073722, 0.009087947370864508240, 0.01090553684503742064, 0.01181433158212388812, 0.01272312631921035907, 0.01363192105629682828, 0.01454071579338329749, 0.01544951053046976670, 0.01635830526755623418, 0.01726710000464270686, 0.01817589474172917607, 0.01908468947881564529, 0.01999348421590211450, 0.02090227895298858718, 0.02181107369007505639, 0.02362866316424793930, 0.02544625263842082916, 0.02726384211259371554, 0.02908143158676660192 ),
 .UNSPECIFIED. ) ;
#61298 = EDGE_CURVE ( 'NONE', #54364, #44335, #21001, .T. ) ;
#61299 = DIRECTION ( 'NONE',  ( -0.000000000000000000, -0.000000000000000000, -1.000000000000000000 ) ) ;
#61300 = DIRECTION ( 'NONE',  ( 0.000000000000000000, 0.000000000000000000, 1.000000000000000000 ) ) ;
#61301 = CARTESIAN_POINT ( 'NONE',  ( -132.9126122820979390, 52.52752252041129566, -18.22572883211020311 ) ) ;
#61302 = CARTESIAN_POINT ( 'NONE',  ( 110.2429982417149290, 28.88204397445231209, -24.07788697519002596 ) ) ;
#61303 = CARTESIAN_POINT ( 'NONE',  ( 86.01819737891891293, 19.21322810362191902, 83.41904106266301255 ) ) ;
#61305 = ORIENTED_EDGE ( 'NONE', *, *, #64499, .F. ) ;
#61304 = CARTESIAN_POINT ( 'NONE',  ( 70.21761529798065737, -26.35311180609978976, 43.58025477438756212 ) ) ;
#61306 = ORIENTED_EDGE ( 'NONE', *, *, #63510, .T. ) ;
#61307 = EDGE_CURVE ( 'NONE', #36964, #39147, #40255, .T. ) ;
#61308 = ORIENTED_EDGE ( 'NONE', *, *, #18891, .T. ) ;
#61309 = CARTESIAN_POINT ( 'NONE',  ( 45.02738683369921802, 9.207938468499234475, 5.602862553026719539 ) ) ;
#61310 = CARTESIAN_POINT ( 'NONE',  ( -180.3444197309645176, 97.13822914721130530, 89.96127970653128614 ) ) ;
#61311 = CARTESIAN_POINT ( 'NONE',  ( 0.3167204509598223194, -5.377136764700217064, -6.686525924292710421 ) ) ;
#61312 = CARTESIAN_POINT ( 'NONE',  ( 104.7034219878851928, 26.40210929103715642, -21.65807146565094143 ) ) ;
#61313 = CARTESIAN_POINT ( 'NONE',  ( 203.9181091394787870, 105.2759068139671257, 17.36317014830576611 ) ) ;
#61314 = CARTESIAN_POINT ( 'NONE',  ( 198.5841913839438746, 99.94205862921178607, 86.03763448066921171 ) ) ;
#61315 = CYLINDRICAL_SURFACE ( 'NONE', #13044, 7.500000000000020428 ) ;
#61316 = CARTESIAN_POINT ( 'NONE',  ( -71.59086462055189770, 19.75139532313339430, -71.95998834529184762 ) ) ;
#61317 = DIRECTION ( 'NONE',  ( -1.000000000000000000, 1.232595164407830946E-32, 7.703719777548943412E-34 ) ) ;
#61318 = EDGE_LOOP ( 'NONE', ( #27004, #29040, #32042, #21711 ) ) ;
#61319 = AXIS2_PLACEMENT_3D ( 'NONE', #835, #33195, #125 ) ;
#61320 = CARTESIAN_POINT ( 'NONE',  ( 10.31616749326173554, 7.393414706728908214, -21.30915619223937085 ) ) ;
#61321 = VERTEX_POINT ( 'NONE', #1943 ) ;
#61322 = ORIENTED_EDGE ( 'NONE', *, *, #67591, .F. ) ;
#61323 = EDGE_CURVE ( 'NONE', #48110, #14951, #23400, .T. ) ;
#61324 = DIRECTION ( 'NONE',  ( 1.000000000000000000, 0.000000000000000000, 0.000000000000000000 ) ) ;
#61325 = CARTESIAN_POINT ( 'NONE',  ( 188.5842358232185916, 88.03712271786932320, -70.86903138220263543 ) ) ;
#61326 = CARTESIAN_POINT ( 'NONE',  ( -37.51960690572916235, 11.69306339258380056, 87.00308991710100770 ) ) ;
#61327 = CARTESIAN_POINT ( 'NONE',  ( 207.8484262634767390, 110.7633525054913974, -77.48949184225725162 ) ) ;
#61328 = VECTOR ( 'NONE', #6498, 1000.000000000000114 ) ;
#61329 = VECTOR ( 'NONE', #43686, 999.9999999999998863 ) ;
#61330 = DIRECTION ( 'NONE',  ( 0.000000000000000000, -1.000000000000000000, 0.000000000000000000 ) ) ;
#61331 = CARTESIAN_POINT ( 'NONE',  ( -26.83517958587657404, 59.60356471962912650, 3.125053320693570118E-16 ) ) ;
#61332 = AXIS2_PLACEMENT_3D ( 'NONE', #19648, #36178, #47402 ) ;
#61333 = CARTESIAN_POINT ( 'NONE',  ( 128.4224537826254107, 38.23837035195744960, -38.33144164633024076 ) ) ;
#61334 = VERTEX_POINT ( 'NONE', #66319 ) ;
#61335 = ORIENTED_EDGE ( 'NONE', *, *, #50020, .F. ) ;
#61336 = VECTOR ( 'NONE', #21834, 1000.000000000000114 ) ;
#61337 = CARTESIAN_POINT ( 'NONE',  ( 329.1355598199467636, 188.0000000000000000, -129.5087625010780812 ) ) ;
#61338 = VECTOR ( 'NONE', #51462, 1000.000000000000000 ) ;
#61339 = CARTESIAN_POINT ( 'NONE',  ( -44.99999999999998579, -25.00000000000000000, 2.000000000000015543 ) ) ;
#61340 = FACE_BOUND ( 'NONE', #47767, .T. ) ;
#61341 = CARTESIAN_POINT ( 'NONE',  ( 58.48209831743720599, 11.66636741727081628, -10.38159958421693574 ) ) ;
#61342 = UNCERTAINTY_MEASURE_WITH_UNIT (LENGTH_MEASURE( 1.000000000000000082E-05 ), #17832, 'distance_accuracy_value', 'NONE');
#61343 = CARTESIAN_POINT ( 'NONE',  ( -50.14771795543006050, 13.42081263859820872, 32.12267660860144503 ) ) ;
#61344 = DIRECTION ( 'NONE',  ( -0.000000000000000000, -0.000000000000000000, -1.000000000000000000 ) ) ;
#61345 = ORIENTED_EDGE ( 'NONE', *, *, #40726, .T. ) ;
#61346 = CYLINDRICAL_SURFACE ( 'NONE', #44652, 7.500000000000020428 ) ;
#61347 = CARTESIAN_POINT ( 'NONE',  ( -74.58602291351357394, -7.967916035252126328, 43.58025477438756923 ) ) ;
#61348 = CARTESIAN_POINT ( 'NONE',  ( 198.4059165548112560, 99.71594270191990006, -66.57968520498842224 ) ) ;
#61349 = CARTESIAN_POINT ( 'NONE',  ( 277.7840330814955792, -21.53650026154319619, 4.493931093091628526 ) ) ;
#61350 = CARTESIAN_POINT ( 'NONE',  ( 107.9301116202192077, 27.82606182274595596, 3.116396251667963746 ) ) ;
#61351 = CARTESIAN_POINT ( 'NONE',  ( -169.8842709557924593, 83.59602878049473418, 4.696942425479066152 ) ) ;
#61352 = LINE ( 'NONE', #24070, #35176 ) ;
#61353 = FACE_BOUND ( 'NONE', #40396, .T. ) ;
#61354 = CYLINDRICAL_SURFACE ( 'NONE', #2937, 65.36598343705435354 ) ;
#61355 = CARTESIAN_POINT ( 'NONE',  ( -101.2355754230665781, 32.25344808697845167, -88.77378729876801344 ) ) ;
#61356 = ORIENTED_EDGE ( 'NONE', *, *, #9778, .F. ) ;
#61357 = CARTESIAN_POINT ( 'NONE',  ( 276.2339232178673001, 21.75159641080505679, 3.304888597515802218 ) ) ;
#61358 = CARTESIAN_POINT ( 'NONE',  ( 153.2523375521184050, 55.69936538551846894, 57.54797417081107369 ) ) ;
#61359 = CARTESIAN_POINT ( 'NONE',  ( 0.000000000000000000, 0.000000000000000000, 40.00000000000003553 ) ) ;
#61360 = CARTESIAN_POINT ( 'NONE',  ( -9.291678301352696678, 76.94361032721405991, 133.5802547743875550 ) ) ;
#61361 = CARTESIAN_POINT ( 'NONE',  ( 99.71998884745383407, 190.0000000000000000, 7.478223336038896996 ) ) ;
#61362 = EDGE_CURVE ( 'NONE', #32365, #29569, #18106, .T. ) ;
#61363 = ORIENTED_EDGE ( 'NONE', *, *, #49597, .F. ) ;
#61364 = ORIENTED_EDGE ( 'NONE', *, *, #30355, .T. ) ;
#61365 = EDGE_CURVE ( 'NONE', #52338, #8192, #18796, .T. ) ;
#61366 = ORIENTED_EDGE ( 'NONE', *, *, #28054, .T. ) ;
#61367 = DIRECTION ( 'NONE',  ( -1.000000000000000000, 0.000000000000000000, 0.000000000000000000 ) ) ;
#61368 = CARTESIAN_POINT ( 'NONE',  ( -177.5271152834791337, 92.16916858125017598, -62.96948660494962269 ) ) ;
#61369 = CARTESIAN_POINT ( 'NONE',  ( -7.329206686002009974E-14, -41.66904755831212270, 85.00100000000000477 ) ) ;
#61370 = ORIENTED_EDGE ( 'NONE', *, *, #51926, .T. ) ;
#61371 = DIRECTION ( 'NONE',  ( 1.000000000000000000, 0.000000000000000000, 0.000000000000000000 ) ) ;
#61372 = AXIS2_PLACEMENT_3D ( 'NONE', #24328, #19032, #7795 ) ;
#61373 = CARTESIAN_POINT ( 'NONE',  ( -180.0175713311536754, 95.14770835574076102, 8.515290778967939289 ) ) ;
#61374 = CARTESIAN_POINT ( 'NONE',  ( -0.5751131641471384226, 6.527254166626918597, 12.70591576700029890 ) ) ;
#61375 = LINE ( 'NONE', #18127, #34871 ) ;
#61376 = CIRCLE ( 'NONE', #35521, 65.00000000000000000 ) ;
#61377 = LINE ( 'NONE', #7222, #9168 ) ;
#61378 = CARTESIAN_POINT ( 'NONE',  ( 139.7928618793172859, 45.12615179300589574, 14.75651092525571784 ) ) ;
#61379 = CARTESIAN_POINT ( 'NONE',  ( -180.6209440844957896, 95.88392769199009535, 38.64167446930188987 ) ) ;
#61380 = ADVANCED_FACE ( 'NONE', ( #29023 ), #45178, .T. ) ;
#61381 = ORIENTED_EDGE ( 'NONE', *, *, #69057, .T. ) ;
#61382 = EDGE_CURVE ( 'NONE', #33141, #30832, #2620, .T. ) ;
#61383 = CARTESIAN_POINT ( 'NONE',  ( 18.89356949897907967, -62.19351277735683681, 40.00000000000003553 ) ) ;
#61384 = AXIS2_PLACEMENT_3D ( 'NONE', #31560, #9423, #64258 ) ;
#61385 = CARTESIAN_POINT ( 'NONE',  ( -74.20136529587826146, 21.74007521413449950, 17.10464239477820669 ) ) ;
#61386 = CARTESIAN_POINT ( 'NONE',  ( 46.90222083990963853, 9.503928413859233260, -42.87962864881881586 ) ) ;
#61387 = CARTESIAN_POINT ( 'NONE',  ( -172.3127615181935539, 87.73358064377643473, -76.52411096701514737 ) ) ;
#61389 = ORIENTED_EDGE ( 'NONE', *, *, #38208, .F. ) ;
#61388 = CARTESIAN_POINT ( 'NONE',  ( -120.0202139357153186, 42.74628011209018297, 87.13439761332067235 ) ) ;
#61390 = CARTESIAN_POINT ( 'NONE',  ( 79.93126905972556528, 17.24332478304277316, -46.70519100763757336 ) ) ;
#61391 = EDGE_CURVE ( 'NONE', #12220, #21613, #54679, .T. ) ;
#61392 = ORIENTED_EDGE ( 'NONE', *, *, #17023, .F. ) ;
#61393 = CARTESIAN_POINT ( 'NONE',  ( 99.71998884745383407, 188.0000000000000000, -91.27944787107685443 ) ) ;
#61394 = CARTESIAN_POINT ( 'NONE',  ( 79.12879321038292346, 18.04902206524926811, 37.44799338594253868 ) ) ;
#61395 = CARTESIAN_POINT ( 'NONE',  ( -35.00000000000000000, -35.00000000000000000, 2.000000000000000000 ) ) ;
#61396 = CARTESIAN_POINT ( 'NONE',  ( 39.40195752203892710, -170.0000000000000000, -50.61981746542779348 ) ) ;
#61397 = CARTESIAN_POINT ( 'NONE',  ( 139.3067271572849677, 44.81402783181197691, -11.52040805170238791 ) ) ;
#61398 = CARTESIAN_POINT ( 'NONE',  ( -41.50537345350635121, -50.04124777106355282, 43.58025477438756923 ) ) ;
#61399 = CARTESIAN_POINT ( 'NONE',  ( -180.4614954900547161, 97.28277348252829881, -16.93614783883196750 ) ) ;
#61400 = CARTESIAN_POINT ( 'NONE',  ( -153.7005182577090068, 67.81869626254727734, -36.07780814487768595 ) ) ;
#61401 = VERTEX_POINT ( 'NONE', #25813 ) ;
#61402 = VERTEX_POINT ( 'NONE', #9634 ) ;
#61403 = ADVANCED_FACE ( 'NONE', ( #8602 ), #4007, .F. ) ;
#61404 = CARTESIAN_POINT ( 'NONE',  ( 105.2506154496929582, 26.63995206619729927, 69.55816789470473793 ) ) ;
#61405 = CARTESIAN_POINT ( 'NONE',  ( 164.7167608259061637, 63.51199216609071385, 61.80061252660392057 ) ) ;
#61407 = ADVANCED_FACE ( 'NONE', ( #40943 ), #62753, .T. ) ;
#61406 = CYLINDRICAL_SURFACE ( 'NONE', #39647, 75.00000000000001421 ) ;
#61408 = ADVANCED_FACE ( 'NONE', ( #51511 ), #8245, .F. ) ;
#61409 = EDGE_CURVE ( 'NONE', #20810, #37937, #3313, .T. ) ;
#61410 = LINE ( 'NONE', #37016, #9748 ) ;
#61411 = CARTESIAN_POINT ( 'NONE',  ( 186.2651679807462415, 84.00458780104320056, -49.16829926748396673 ) ) ;
#61412 = CARTESIAN_POINT ( 'NONE',  ( -105.4589068214114178, 34.42476264325677704, 58.05430461866929903 ) ) ;
#61413 = CARTESIAN_POINT ( 'NONE',  ( -31.43908319763709258, 9.591432048623767415, -35.31719736520183517 ) ) ;
#61414 = DIRECTION ( 'NONE',  ( 1.000000000000000000, 0.000000000000000000, 0.000000000000000000 ) ) ;
#61415 = VERTEX_POINT ( 'NONE', #19838 ) ;
#61416 = PRODUCT_DEFINITION_SHAPE ( 'NONE', 'NONE',  #69578 ) ;
#61417 = ORIENTED_EDGE ( 'NONE', *, *, #20577, .T. ) ;
#61418 = ORIENTED_EDGE ( 'NONE', *, *, #47687, .T. ) ;
#61419 = CONICAL_SURFACE ( 'NONE', #24369, 74.95140232871122521, 0.8777644062502172329 ) ;
#61420 = LINE ( 'NONE', #29410, #67816 ) ;
#61421 = DIRECTION ( 'NONE',  ( 0.000000000000000000, 0.000000000000000000, -1.000000000000000000 ) ) ;
#61422 = CARTESIAN_POINT ( 'NONE',  ( 15.68296563925591869, -63.09411298019745828, 0.000000000000000000 ) ) ;
#61423 = CARTESIAN_POINT ( 'NONE',  ( -452.6627218934913799, 364.9999999999998295, -146.4497041420117966 ) ) ;
#61424 = CARTESIAN_POINT ( 'NONE',  ( 121.4242852856285140, 6.000000000000000000, -20.00000000000000000 ) ) ;
#61425 = VECTOR ( 'NONE', #40066, 1000.000000000000000 ) ;
#61426 = CARTESIAN_POINT ( 'NONE',  ( -62.06231780744545290, 17.72446026058426938, 40.49660573368029048 ) ) ;
#61427 = CARTESIAN_POINT ( 'NONE',  ( -96.77705718164442317, 31.18700926299570853, -10.55039380601694710 ) ) ;
#61428 = AXIS2_PLACEMENT_3D ( 'NONE', #35818, #15047, #57616 ) ;
#61429 = CARTESIAN_POINT ( 'NONE',  ( 57.07246224906425880, 12.39953617563783084, 41.91415364038640945 ) ) ;
#61430 = CARTESIAN_POINT ( 'NONE',  ( 31.90811916295598039, 7.552800146120133284, 91.55187592262117846 ) ) ;
#61431 =( LENGTH_UNIT ( ) NAMED_UNIT ( * ) SI_UNIT ( .MILLI., .METRE. ) );
#61432 = ORIENTED_EDGE ( 'NONE', *, *, #12862, .T. ) ;
#61433 = VECTOR ( 'NONE', #12885, 1000.000000000000000 ) ;
#61434 = CARTESIAN_POINT ( 'NONE',  ( -7.825402957745083654, 6.891034867348166060, -50.41807073194384259 ) ) ;
#61435 = CARTESIAN_POINT ( 'NONE',  ( -450.6627218934913230, 177.8591479523843475, -111.4497041420117966 ) ) ;
#61436 = CARTESIAN_POINT ( 'NONE',  ( -14.84903512415885274, 8.461292896365064209, 13.41286030492582348 ) ) ;
#61437 = CARTESIAN_POINT ( 'NONE',  ( -142.4991775570125583, 58.45550857435405590, 14.10091869410458010 ) ) ;
#61438 = CARTESIAN_POINT ( 'NONE',  ( 283.0494652463580678, -21.63856170200817530, -3.975743201777058200 ) ) ;
#61439 = CARTESIAN_POINT ( 'NONE',  ( 197.3054165770396366, 96.72615186924561215, 62.24439187461354095 ) ) ;
#61440 = CARTESIAN_POINT ( 'NONE',  ( 128.0882145863933772, 39.20607399008168414, -21.49800594817171273 ) ) ;
#61441 = AXIS2_PLACEMENT_3D ( 'NONE', #37232, #58342, #9831 ) ;
#61442 = ORIENTED_EDGE ( 'NONE', *, *, #68240, .T. ) ;
#61443 = DIRECTION ( 'NONE',  ( -0.9998063756620102493, -0.01967768242440563753, 8.641437467987462711E-15 ) ) ;
#61444 = FACE_OUTER_BOUND ( 'NONE', #65089, .T. ) ;
#61445 = CARTESIAN_POINT ( 'NONE',  ( -35.17296606710973350, 11.25626711331309515, -49.34029585684413632 ) ) ;
#61446 = FACE_OUTER_BOUND ( 'NONE', #9437, .T. ) ;
#61447 = CONTEXT_DEPENDENT_SHAPE_REPRESENTATION ( #64223, #16362 ) ;
#61448 = CARTESIAN_POINT ( 'NONE',  ( 39.40195752203892710, -170.0000000000000000, -77.46436805589148378 ) ) ;
#61449 = ORIENTED_EDGE ( 'NONE', *, *, #2073, .T. ) ;
#61450 = CARTESIAN_POINT ( 'NONE',  ( -122.7930600691578036, 44.48546375740917114, -35.56903786926160649 ) ) ;
#61451 = LINE ( 'NONE', #34731, #48186 ) ;
#61452 = DIRECTION ( 'NONE',  ( -0.000000000000000000, -0.000000000000000000, 1.000000000000000000 ) ) ;
#61453 = ADVANCED_FACE ( 'NONE', ( #30053 ), #29696, .T. ) ;
#61454 = CARTESIAN_POINT ( 'NONE',  ( 150.3392635816054508, 53.55403001380570771, 88.24482449747890200 ) ) ;
#61455 = VERTEX_POINT ( 'NONE', #30741 ) ;
#61456 = DIRECTION ( 'NONE',  ( -0.000000000000000000, 0.5000000000000008882, -0.8660254037844381525 ) ) ;
#61457 = DIRECTION ( 'NONE',  ( 1.000000000000000000, 0.000000000000000000, 0.000000000000000000 ) ) ;
#61458 = CARTESIAN_POINT ( 'NONE',  ( -154.7826623253029936, 70.14150242829515491, 32.88389497768243075 ) ) ;
#61459 = CARTESIAN_POINT ( 'NONE',  ( -84.49322488516129681, 0.000000000000000000, 43.58025477438756212 ) ) ;
#61460 = CARTESIAN_POINT ( 'NONE',  ( 79.82127737190243977, 17.20935440217364487, 7.211099181453766604 ) ) ;
#61462 = ORIENTED_EDGE ( 'NONE', *, *, #11176, .T. ) ;
#61461 = DIRECTION ( 'NONE',  ( 0.000000000000000000, 0.000000000000000000, 1.000000000000000000 ) ) ;
#61463 = AXIS2_PLACEMENT_3D ( 'NONE', #87, #32454, #21887 ) ;
#61464 = EDGE_CURVE ( 'NONE', #10168, #8516, #13861, .T. ) ;
#61465 = CARTESIAN_POINT ( 'NONE',  ( -1.928775478690862188, 7.585606196872214824, -91.95340218108046315 ) ) ;
#61466 = ADVANCED_FACE ( 'NONE', ( #41976 ), #14893, .F. ) ;
#61467 = ORIENTED_EDGE ( 'NONE', *, *, #48585, .T. ) ;
#61469 = ORIENTED_EDGE ( 'NONE', *, *, #48479, .F. ) ;
#61468 = ADVANCED_FACE ( 'NONE', ( #46557 ), #46210, .F. ) ;
#61470 = AXIS2_PLACEMENT_3D ( 'NONE', #58980, #47386, #5181 ) ;
#61471 = CARTESIAN_POINT ( 'NONE',  ( 173.5836858989432301, 72.71885240881778145, 37.09537031985573208 ) ) ;
#61472 = CARTESIAN_POINT ( 'NONE',  ( -31.65307660562752901, 10.64641742089424703, -89.00629854612921577 ) ) ;
#61473 = EDGE_CURVE ( 'NONE', #60060, #69323, #67691, .T. ) ;
#61474 = AXIS2_PLACEMENT_3D ( 'NONE', #48938, #47565, #77 ) ;
#61476 = ORIENTED_EDGE ( 'NONE', *, *, #22732, .T. ) ;
#61475 = CARTESIAN_POINT ( 'NONE',  ( -10.69547592951790804, 8.103864096836391084, -76.70459122694524012 ) ) ;
#61477 = CYLINDRICAL_SURFACE ( 'NONE', #63376, 7.500000000000013323 ) ;
#61478 = CARTESIAN_POINT ( 'NONE',  ( -25.07735481787161902, 9.648965052008779963, 33.73669382820916951 ) ) ;
#61479 = CARTESIAN_POINT ( 'NONE',  ( -72.35078170365747496, 21.08176362823951777, -46.66809070389184200 ) ) ;
#61480 = CIRCLE ( 'NONE', #28899, 24.99999999999985434 ) ;
#61481 = ORIENTED_EDGE ( 'NONE', *, *, #22731, .F. ) ;
#61482 = CARTESIAN_POINT ( 'NONE',  ( 175.1380114663270149, 74.18445479419006006, -92.83823291830314872 ) ) ;
#61483 = AXIS2_PLACEMENT_3D ( 'NONE', #54632, #59552, #43720 ) ;
#61484 = CARTESIAN_POINT ( 'NONE',  ( 141.0792860804899647, 47.16255757051796138, 34.91922768290986312 ) ) ;
#61485 = CARTESIAN_POINT ( 'NONE',  ( 0.000000000000000000, 0.000000000000000000, 0.000000000000000000 ) ) ;
#61486 = CARTESIAN_POINT ( 'NONE',  ( -130.1938957973835613, 50.61368074696266461, 5.112861415500842277 ) ) ;
#61487 = LINE ( 'NONE', #23858, #55356 ) ;
#61488 = EDGE_LOOP ( 'NONE', ( #9283, #38846 ) ) ;
#61489 = VERTEX_POINT ( 'NONE', #57468 ) ;
#61490 = ORIENTED_EDGE ( 'NONE', *, *, #19462, .T. ) ;
#61492 = EDGE_CURVE ( 'NONE', #1617, #63246, #68376, .T. ) ;
#61491 = DIRECTION ( 'NONE',  ( 0.000000000000000000, -0.1086713087885527451, -0.9940777367219241212 ) ) ;
#61493 = EDGE_CURVE ( 'NONE', #1734, #58973, #9278, .T. ) ;
#61494 = DIRECTION ( 'NONE',  ( 0.000000000000000000, 1.224646799147344826E-16, 1.000000000000000000 ) ) ;
#61495 = LINE ( 'NONE', #13645, #60252 ) ;
#61496 = DIRECTION ( 'NONE',  ( 1.000000000000000000, 0.000000000000000000, 0.000000000000000000 ) ) ;
#61497 = EDGE_CURVE ( 'NONE', #13782, #63246, #67347, .T. ) ;
#61498 = CARTESIAN_POINT ( 'NONE',  ( 50.98853755884145755, 400.0000000000065938, -123.9497041420120382 ) ) ;
#61499 = LINE ( 'NONE', #57259, #23892 ) ;
#61500 = CARTESIAN_POINT ( 'NONE',  ( -74.39861643904067989, 21.81123504700006777, -9.598885444783787690 ) ) ;
#61501 = ORIENTED_EDGE ( 'NONE', *, *, #23437, .F. ) ;
#61502 = CARTESIAN_POINT ( 'NONE',  ( -105.4642082819536029, 35.56541171990216554, 44.82579570833843974 ) ) ;
#61503 = ORIENTED_EDGE ( 'NONE', *, *, #20577, .F. ) ;
#61504 = DIRECTION ( 'NONE',  ( -0.000000000000000000, -0.000000000000000000, -1.000000000000000000 ) ) ;
#61505 = ORIENTED_EDGE ( 'NONE', *, *, #36076, .T. ) ;
#61506 = CARTESIAN_POINT ( 'NONE',  ( 209.3223706822284100, 172.0000000000000284, 277.8007638641562380 ) ) ;
#61507 = CARTESIAN_POINT ( 'NONE',  ( 110.2429982417149574, -170.0000000000000000, 37.11121420573731911 ) ) ;
#61508 = SURFACE_STYLE_FILL_AREA ( #43914 ) ;
#61509 = CARTESIAN_POINT ( 'NONE',  ( -4.613603609464500543, -74.86839895266049894, 43.58025477438756212 ) ) ;
#61510 = CARTESIAN_POINT ( 'NONE',  ( -54.56693200831794144, 14.55131601960339083, 18.47277718246750666 ) ) ;
#61511 = FACE_OUTER_BOUND ( 'NONE', #35731, .T. ) ;
#61512 = VERTEX_POINT ( 'NONE', #20179 ) ;
#61513 = VECTOR ( 'NONE', #26751, 1000.000000000000000 ) ;
#61514 = LINE ( 'NONE', #60468, #27468 ) ;
#61515 = CARTESIAN_POINT ( 'NONE',  ( -155.5978531700836527, 69.52241200678679434, -11.08417929211540276 ) ) ;
#61516 = ORIENTED_EDGE ( 'NONE', *, *, #63282, .T. ) ;
#61517 = CARTESIAN_POINT ( 'NONE',  ( -55.53469534616547776, 14.81076603075804066, 30.31732777293112946 ) ) ;
#61518 = CARTESIAN_POINT ( 'NONE',  ( -56.72676045871357786, 16.18052435693488533, 57.34706834696837774 ) ) ;
#61519 = FACE_OUTER_BOUND ( 'NONE', #3979, .T. ) ;
#61520 = ORIENTED_EDGE ( 'NONE', *, *, #29557, .F. ) ;
#61521 = PLANE ( 'NONE',  #19902 ) ;
#61522 = CARTESIAN_POINT ( 'NONE',  ( 154.0281735872262061, 56.28213428456459155, -63.80132600415307564 ) ) ;
#61523 = CARTESIAN_POINT ( 'NONE',  ( -35.38560449531986052, 10.27249159032102277, 31.33411146270130487 ) ) ;
#61524 = AXIS2_PLACEMENT_3D ( 'NONE', #45937, #19548, #41010 ) ;
#61525 = CARTESIAN_POINT ( 'NONE',  ( 140.2332932573541484, 45.41010019581506185, -39.54326788570185869 ) ) ;
#61526 = VECTOR ( 'NONE', #67346, 1000.000000000000114 ) ;
#61527 = EDGE_LOOP ( 'NONE', ( #37129, #46977, #25843, #2096 ) ) ;
#61528 = DIRECTION ( 'NONE',  ( -0.000000000000000000, 1.000000000000000000, -0.000000000000000000 ) ) ;
#61529 = CARTESIAN_POINT ( 'NONE',  ( -1.224646799147352468E-15, 0.000000000000000000, 20.00000000000000000 ) ) ;
#61530 = PRESENTATION_LAYER_ASSIGNMENT (  '', '', ( #58158 ) ) ;
#61531 = ORIENTED_EDGE ( 'NONE', *, *, #6542, .F. ) ;
#61532 = CARTESIAN_POINT ( 'NONE',  ( 31.95163392065795804, 8.568192436298479819, -17.26688347263179679 ) ) ;
#61533 = LINE ( 'NONE', #39380, #15874 ) ;
#61534 = CARTESIAN_POINT ( 'NONE',  ( 91.11342358617750392, 21.00000175105271083, 58.03984230042496506 ) ) ;
#61535 = DIRECTION ( 'NONE',  ( 1.000000000000000000, 0.000000000000000000, 0.000000000000000000 ) ) ;
#61536 =( NAMED_UNIT ( * ) SI_UNIT ( $, .STERADIAN. ) SOLID_ANGLE_UNIT ( ) );
#61537 = CIRCLE ( 'NONE', #28956, 5.000000000000004441 ) ;
#61538 = EDGE_CURVE ( 'NONE', #51139, #41326, #56655, .T. ) ;
#61539 = CARTESIAN_POINT ( 'NONE',  ( -36.11269837220809364, -10.55634918610397932, 0.000000000000000000 ) ) ;
#61540 = VERTEX_POINT ( 'NONE', #26837 ) ;
#61541 = CARTESIAN_POINT ( 'NONE',  ( 158.3604774538084712, 58.34594647925810307, -9.319281447646249106 ) ) ;
#61542 = DIRECTION ( 'NONE',  ( 0.000000000000000000, -1.000000000000000000, 0.000000000000000000 ) ) ;
#61543 = CARTESIAN_POINT ( 'NONE',  ( 63.98971758354224448, 12.90030016320051232, 71.61000590023084555 ) ) ;
#61544 = CARTESIAN_POINT ( 'NONE',  ( 140.5958192060901695, 46.84598876498518649, 6.864059862099193055 ) ) ;
#61545 = CARTESIAN_POINT ( 'NONE',  ( -12.50000000000002842, -18.06806526123148160, -2.000000000000000000 ) ) ;
#61546 = ORIENTED_EDGE ( 'NONE', *, *, #45250, .T. ) ;
#61547 = EDGE_CURVE ( 'NONE', #56353, #60359, #69297, .T. ) ;
#61548 = CARTESIAN_POINT ( 'NONE',  ( 158.3516718297676107, 59.61984652322050948, -24.24089676901845536 ) ) ;
#61549 = DIRECTION ( 'NONE',  ( 0.000000000000000000, 0.000000000000000000, 1.000000000000000000 ) ) ;
#61550 = ORIENTED_EDGE ( 'NONE', *, *, #46433, .T. ) ;
#61551 = LINE ( 'NONE', #34831, #58100 ) ;
#61552 = CYLINDRICAL_SURFACE ( 'NONE', #4990, 4.999999999999997335 ) ;
#61553 = ADVANCED_FACE ( 'NONE', ( #10995 ), #64120, .T. ) ;
#61554 = ADVANCED_FACE ( 'NONE', ( #52857 ), #53892, .F. ) ;
#61555 = EDGE_LOOP ( 'NONE', ( #38579, #36351, #3419, #24378 ) ) ;
#61556 = CARTESIAN_POINT ( 'NONE',  ( -149.2910611247327779, 63.99625741915658494, -61.65738112195566600 ) ) ;
#61557 = DIRECTION ( 'NONE',  ( 1.000000000000000000, -3.344045254895050726E-17, -0.000000000000000000 ) ) ;
#61558 = DIRECTION ( 'NONE',  ( 0.000000000000000000, 0.000000000000000000, 1.000000000000000000 ) ) ;
#61559 = EDGE_CURVE ( 'NONE', #56069, #14782, #11336, .T. ) ;
#61560 = LINE ( 'NONE', #7756, #7003 ) ;
#61561 = VERTEX_POINT ( 'NONE', #15251 ) ;
#61562 = AXIS2_PLACEMENT_3D ( 'NONE', #15345, #58578, #58244 ) ;
#61563 = CARTESIAN_POINT ( 'NONE',  ( -100.4347360276018861, 32.97716872911836816, 3.890190775139684476 ) ) ;
#61564 = B_SPLINE_CURVE_WITH_KNOTS ( 'NONE', 3,
 ( #9213, #67966, #24013, #19767, #24713, #3937, #61641, #61295, #30326, #29625, #25058, #51779, #2905, #34586, #46147, #2557, #19074, #3585, #46488, #56023, #66939, #50733, #45456, #18730, #24365, #45810, #67289, #13457, #34917, #56356, #20796, #20115, #53482, #68637, #63019, #64050, #15530, #4618, #31362, #58419, #42923, #16206, #58089, #69330, #23 ),
 .UNSPECIFIED., .F., .F.,
 ( 4, 2, 2, 1, 2, 2, 2, 2, 2, 2, 2, 2, 2, 2, 2, 2, 2, 2, 2, 2, 2, 2, 4 ),
 ( 0.02345095402629350512, 0.02491692321306682861, 0.02564990780645348689, 0.02638289239984014517, 0.02711587699322680345, 0.02784886158661346173, 0.02931483077338677828, 0.03004781536677343309, 0.03078079996016008790, 0.03224676914693340446, 0.03297975374032005580, 0.03371273833370671408, 0.03517870752048002370, 0.03664467670725333331, 0.03737766130063998465, 0.03811064589402663599, 0.03957661508079993173, 0.04104258426757322747, 0.04250855345434652321, 0.04324153804773317455, 0.04397452264111981202, 0.04544049182789309388, 0.04690646101466637574 ),
 .UNSPECIFIED. ) ;
#61565 = CARTESIAN_POINT ( 'NONE',  ( 61.73284572609541954, 13.41039274811037352, 83.60527669376516258 ) ) ;
#61566 = CIRCLE ( 'NONE', #36866, 5.000000000000004441 ) ;
#61567 = DIRECTION ( 'NONE',  ( -1.000000000000000000, 0.000000000000000000, 0.000000000000000000 ) ) ;
#61568 = CARTESIAN_POINT ( 'NONE',  ( 81.57915404881515542, 18.81499384983930767, -22.02727323828690231 ) ) ;
#61569 = CARTESIAN_POINT ( 'NONE',  ( -170.2801941679960009, 84.02053682015869640, 31.36767604865260850 ) ) ;
#61570 = CARTESIAN_POINT ( 'NONE',  ( 32.32614265053613423, 8.605592782137726715, -94.18410555706600462 ) ) ;
#61571 = CARTESIAN_POINT ( 'NONE',  ( 24.34685647903079442, -70.88683439560421107, 41.38025477438755928 ) ) ;
#61572 = ORIENTED_EDGE ( 'NONE', *, *, #60585, .T. ) ;
#61573 = LINE ( 'NONE', #40801, #30968 ) ;
#61574 = CIRCLE ( 'NONE', #38003, 65.36598343705435354 ) ;
#61575 = CARTESIAN_POINT ( 'NONE',  ( -12.78319349481552081, 8.274445259016799170, 70.10900556253349691 ) ) ;
#61576 = VERTEX_POINT ( 'NONE', #47580 ) ;
#61577 = CARTESIAN_POINT ( 'NONE',  ( 39.40195752203892710, -170.0000000000000000, 37.41383430596326320 ) ) ;
#61578 = AXIS2_PLACEMENT_3D ( 'NONE', #16897, #11617, #33089 ) ;
#61579 = CARTESIAN_POINT ( 'NONE',  ( 211.1046732743772907, 117.3965485104337461, -13.07269876749372628 ) ) ;
#61580 = DIRECTION ( 'NONE',  ( 0.000000000000000000, 1.000000000000000000, 0.000000000000000000 ) ) ;
#61581 = CARTESIAN_POINT ( 'NONE',  ( -0.3732240621745024356, 7.527003275829099671, 38.59489257713590149 ) ) ;
#61582 = CARTESIAN_POINT ( 'NONE',  ( -12.19213298737871298, 7.214665545688172976, -90.49457743040542823 ) ) ;
#61583 = EDGE_CURVE ( 'NONE', #11134, #67683, #7819, .T. ) ;
#61584 = CARTESIAN_POINT ( 'NONE',  ( -53.13004807512038496, 14.17398740785106526, -62.29520437222935669 ) ) ;
#61585 = CARTESIAN_POINT ( 'NONE',  ( -5.879983509979051171, 7.779504553499513975, -23.33333956214708493 ) ) ;
#61586 = PLANE ( 'NONE',  #31019 ) ;
#61587 = CARTESIAN_POINT ( 'NONE',  ( -60.97011009284709360, 16.34812508431679490, 15.60724065707690755 ) ) ;
#61588 = ORIENTED_EDGE ( 'NONE', *, *, #68411, .T. ) ;
#61589 = VECTOR ( 'NONE', #11650, 1000.000000000000000 ) ;
#61590 = CARTESIAN_POINT ( 'NONE',  ( 0.000000000000000000, 0.000000000000000000, 85.00000000000000000 ) ) ;
#61591 = ORIENTED_EDGE ( 'NONE', *, *, #33835, .T. ) ;
#61592 = LINE ( 'NONE', #32206, #39738 ) ;
#61593 = CARTESIAN_POINT ( 'NONE',  ( 6.375108774214766072E-14, 36.11269837220805812, 0.000000000000000000 ) ) ;
#61594 = CARTESIAN_POINT ( 'NONE',  ( 39.40195752203892710, 8.409560354027384221, 71.75838489642698903 ) ) ;
#61595 = DIRECTION ( 'NONE',  ( -0.000000000000000000, -1.000000000000000000, -0.000000000000000000 ) ) ;
#61596 = CARTESIAN_POINT ( 'NONE',  ( 38.61145306061725080, -15.82625577337686629, 13.79046340968177731 ) ) ;
#61597 = DIRECTION ( 'NONE',  ( 0.000000000000000000, -0.5000000000000008882, 0.8660254037844382635 ) ) ;
#61598 = DIRECTION ( 'NONE',  ( 1.000000000000000000, 2.117582368135750246E-20, -1.697742017499683849E-16 ) ) ;
#61599 = CARTESIAN_POINT ( 'NONE',  ( -165.7689197919845014, 79.30072199592275695, 66.67702330705374436 ) ) ;
#61600 = VERTEX_POINT ( 'NONE', #23995 ) ;
#61601 = ORIENTED_EDGE ( 'NONE', *, *, #51085, .T. ) ;
#61602 = PLANE ( 'NONE',  #62384 ) ;
#61603 = PLANE ( 'NONE',  #11958 ) ;
#61604 = DIRECTION ( 'NONE',  ( -0.000000000000000000, -0.000000000000000000, -1.000000000000000000 ) ) ;
#61605 = CARTESIAN_POINT ( 'NONE',  ( -171.0950923142953854, 86.38958441093224394, 57.93243116198902243 ) ) ;
#61606 = DIRECTION ( 'NONE',  ( 0.000000000000000000, 1.000000000000000000, -0.000000000000000000 ) ) ;
#61607 = CARTESIAN_POINT ( 'NONE',  ( 61.08522853873726177, 13.26388801693370922, -9.112382269691240211 ) ) ;
#61608 = VERTEX_POINT ( 'NONE', #39821 ) ;
#61609 = CARTESIAN_POINT ( 'NONE',  ( 11.05669727962760085, 0.000000000000000000, -27.88815958909220782 ) ) ;
#61610 = DIRECTION ( 'NONE',  ( 1.000000000000000000, 0.000000000000000000, -0.000000000000000000 ) ) ;
#61611 = CARTESIAN_POINT ( 'NONE',  ( -2.699999999999990408, 2.486033002269127373E-15, 20.30000000000000071 ) ) ;
#61612 = CARTESIAN_POINT ( 'NONE',  ( -90.99999999999994316, 0.000000000000000000, -105.0000000000000142 ) ) ;
#61613 = CARTESIAN_POINT ( 'NONE',  ( 8.485361335568063268, 6.376707943524878353, -95.00000000000133582 ) ) ;
#61614 = EDGE_CURVE ( 'NONE', #64271, #67476, #28931, .T. ) ;
#61615 = EDGE_CURVE ( 'NONE', #38817, #57581, #44757, .T. ) ;
#61616 = VECTOR ( 'NONE', #15591, 1000.000000000000000 ) ;
#61617 = ADVANCED_FACE ( 'NONE', ( #60926 ), #60579, .F. ) ;
#61618 = ORIENTED_EDGE ( 'NONE', *, *, #64852, .F. ) ;
#61619 = CONICAL_SURFACE ( 'NONE', #27867, 5.000000000000000888, 0.9599310885968810325 ) ;
#61620 = CARTESIAN_POINT ( 'NONE',  ( 65.02478361689782105, -37.39438481343979959, 170.0000000000000000 ) ) ;
#61621 = CARTESIAN_POINT ( 'NONE',  ( 110.2429982417149574, -170.0000000000000000, 63.95576479620102361 ) ) ;
#61622 = CARTESIAN_POINT ( 'NONE',  ( -65.00000000000000000, 0.000000000000000000, 170.0000000000000000 ) ) ;
#61623 = CARTESIAN_POINT ( 'NONE',  ( -180.5954680880247167, 97.44843622358463620, 10.83696913367529646 ) ) ;
#61624 = CARTESIAN_POINT ( 'NONE',  ( 212.1734186221016216, 119.0499290057855575, 64.24444335267637030 ) ) ;
#61625 = CARTESIAN_POINT ( 'NONE',  ( 80.17205177205137545, 17.31791394718354837, -73.98926831092168754 ) ) ;
#61626 = ORIENTED_EDGE ( 'NONE', *, *, #32938, .F. ) ;
#61627 = DIRECTION ( 'NONE',  ( 0.000000000000000000, 0.000000000000000000, 1.000000000000000000 ) ) ;
#61628 = CARTESIAN_POINT ( 'NONE',  ( -5.355005115540906857, -6.145890662064668497, -9.417753204360275632 ) ) ;
#61629 = ORIENTED_EDGE ( 'NONE', *, *, #13376, .T. ) ;
#61630 = CARTESIAN_POINT ( 'NONE',  ( 18.89356949897907967, -62.19351277735683681, 170.0000000000000000 ) ) ;
#61631 = ORIENTED_EDGE ( 'NONE', *, *, #47710, .F. ) ;
#61632 = CARTESIAN_POINT ( 'NONE',  ( -85.34215807311491631, 24.97769003780924280, -66.03245772043236173 ) ) ;
#61633 = CARTESIAN_POINT ( 'NONE',  ( -21.03405120204953960, -13.73704776265678440, 0.000000000000000000 ) ) ;
#61634 = CARTESIAN_POINT ( 'NONE',  ( 15.78827728214693416, 6.500811158483284835, -77.36349468914950478 ) ) ;
#61635 = EDGE_CURVE ( 'NONE', #31528, #66072, #49314, .T. ) ;
#61636 = ORIENTED_EDGE ( 'NONE', *, *, #62334, .T. ) ;
#61637 = EDGE_CURVE ( 'NONE', #41626, #36843, #50178, .T. ) ;
#61638 = ORIENTED_EDGE ( 'NONE', *, *, #24858, .T. ) ;
#61639 = CARTESIAN_POINT ( 'NONE',  ( 417.3372781065091317, 395.0000000000065938, -116.4497041420121661 ) ) ;
#61640 = CARTESIAN_POINT ( 'NONE',  ( -108.2447486367085929, 37.06113128159649506, -91.63506942693179269 ) ) ;
#61641 = CARTESIAN_POINT ( 'NONE',  ( 18.66025561752211104, 6.609375019058820300, 3.728956910112429579 ) ) ;
#61642 = EDGE_LOOP ( 'NONE', ( #61291, #58314, #19456, #63814 ) ) ;
#61643 = LINE ( 'NONE', #12767, #46912 ) ;
#61644 = CARTESIAN_POINT ( 'NONE',  ( 59.94652978725885362, 13.01168383647462434, -36.37311755078323472 ) ) ;
#61645 = DIRECTION ( 'NONE',  ( -0.000000000000000000, -0.000000000000000000, -1.000000000000000000 ) ) ;
#61646 = CARTESIAN_POINT ( 'NONE',  ( 112.5721302457195350, 29.97407549554797868, -9.433108360236460044 ) ) ;
#61647 = CARTESIAN_POINT ( 'NONE',  ( 81.57915404881515542, 18.81499384983930412, -48.87182382875059261 ) ) ;
#61649 = EDGE_LOOP ( 'NONE', ( #5669, #26315 ) ) ;
#61648 = CARTESIAN_POINT ( 'NONE',  ( -170.4689427914638031, 85.70641121003137641, -88.87457044037061848 ) ) ;
#61650 = ORIENTED_EDGE ( 'NONE', *, *, #18507, .T. ) ;
#61651 = VERTEX_POINT ( 'NONE', #50717 ) ;
#61652 = CARTESIAN_POINT ( 'NONE',  ( 46.13320811200731697, 9.380653113584052960, 7.225283526527610967 ) ) ;
#61653 = LINE ( 'NONE', #34930, #41665 ) ;
#61654 = CARTESIAN_POINT ( 'NONE',  ( -47.80193682758674356, 12.85650137125657544, -17.85234014397047275 ) ) ;
#61655 = CARTESIAN_POINT ( 'NONE',  ( 110.2429982417149290, 28.88204397445231209, -24.07788697519002596 ) ) ;
#61656 = LINE ( 'NONE', #27289, #45664 ) ;
#61657 = CARTESIAN_POINT ( 'NONE',  ( -24.30174763577181096, 8.528231305356500869, -94.16290959115248427 ) ) ;
#61658 = CARTESIAN_POINT ( 'NONE',  ( 212.2010424008437894, 119.0930793856250887, 90.34093224311959602 ) ) ;
#61659 = DIRECTION ( 'NONE',  ( -1.000000000000000000, -0.000000000000000000, -0.000000000000000000 ) ) ;
#61660 = CARTESIAN_POINT ( 'NONE',  ( -85.73740570227381852, 26.23277384689413694, 62.24966593035414064 ) ) ;
#61661 = CARTESIAN_POINT ( 'NONE',  ( -13.47230132170245653, 7.324574289401433624, 42.57560624842334107 ) ) ;
#61662 = ORIENTED_EDGE ( 'NONE', *, *, #40527, .F. ) ;
#61663 = CARTESIAN_POINT ( 'NONE',  ( 8.763528846667103522, 7.383598436776580343, -13.53555138396326996 ) ) ;
#61664 = ORIENTED_EDGE ( 'NONE', *, *, #36079, .T. ) ;
#61665 = ORIENTED_EDGE ( 'NONE', *, *, #24634, .F. ) ;
#61666 = AXIS2_PLACEMENT_3D ( 'NONE', #17405, #48697, #38517 ) ;
#61667 = CARTESIAN_POINT ( 'NONE',  ( -143.8634661037141029, 60.82480701605699380, 6.410842245792165883 ) ) ;
#61668 = CARTESIAN_POINT ( 'NONE',  ( 181.0840389613909736, 80.03940679743418229, -63.06960825634327961 ) ) ;
#61669 = CARTESIAN_POINT ( 'NONE',  ( -32.09642077712169339, 10.71953907670691919, 83.90686141431137912 ) ) ;
#61670 = CARTESIAN_POINT ( 'NONE',  ( 208.9507214515059843, 112.3605999017434698, -76.86410794482465292 ) ) ;
#61671 = MECHANICAL_DESIGN_GEOMETRIC_PRESENTATION_REPRESENTATION (  '', ( #51589 ), #10006 ) ;
#61672 = LINE ( 'NONE', #55083, #18709 ) ;
#61673 = DIRECTION ( 'NONE',  ( 0.000000000000000000, -1.000000000000000000, 0.000000000000000000 ) ) ;
#61674 = CARTESIAN_POINT ( 'NONE',  ( 8.480977594057451441, 7.382886909400596664, -44.72572676602403874 ) ) ;
#61675 = CARTESIAN_POINT ( 'NONE',  ( 126.4083787442699673, 37.10531539900949127, -44.54862598322278444 ) ) ;
#61676 = ORIENTED_EDGE ( 'NONE', *, *, #6986, .F. ) ;
#61677 = ORIENTED_EDGE ( 'NONE', *, *, #47648, .F. ) ;
#61678 = CARTESIAN_POINT ( 'NONE',  ( 60.00000000000000000, 0.000000000000000000, 5.000000000000000000 ) ) ;
#61679 = FACE_OUTER_BOUND ( 'NONE', #55537, .T. ) ;
#61680 = CARTESIAN_POINT ( 'NONE',  ( 112.3013380801408658, 388.0000000000065938, -128.9497041420121093 ) ) ;
#61681 = CARTESIAN_POINT ( 'NONE',  ( -26.87327614295026024, 8.886070347947315540, -63.69140009212348730 ) ) ;
#61682 = CARTESIAN_POINT ( 'NONE',  ( 11.82322073186613132, 6.406156243758798219, 4.299284300909138601 ) ) ;
#61683 = ORIENTED_EDGE ( 'NONE', *, *, #50680, .F. ) ;
#61684 = ADVANCED_FACE ( 'NONE', ( #54946 ), #6767, .F. ) ;
#61685 = CARTESIAN_POINT ( 'NONE',  ( 282.5088088673473976, 21.56899521162237576, -4.337361123092371429 ) ) ;
#61686 = DIRECTION ( 'NONE',  ( -0.000000000000000000, 0.000000000000000000, 1.000000000000000000 ) ) ;
#61687 = CARTESIAN_POINT ( 'NONE',  ( 197.4121679705847896, 98.46451029407251099, -72.45810111998113712 ) ) ;
#61688 = CARTESIAN_POINT ( 'NONE',  ( 275.2579757425518210, -21.94246241598116143, 1.618793836905497940 ) ) ;
#61689 =( NAMED_UNIT ( * ) PLANE_ANGLE_UNIT ( ) SI_UNIT ( $, .RADIAN. ) );
#61690 = CARTESIAN_POINT ( 'NONE',  ( -166.1495968531527581, 79.68938347407072342, -93.12242192314892009 ) ) ;
#61691 = CARTESIAN_POINT ( 'NONE',  ( -1.665334536937750193E-15, 2.999999999999969358, -3.000000000000028422 ) ) ;
#61692 = CARTESIAN_POINT ( 'NONE',  ( -442.6627218934913799, 394.9999999999998295, -132.7581352960343679 ) ) ;
#61693 = EDGE_CURVE ( 'NONE', #68664, #29607, #61276, .T. ) ;
#61694 = EDGE_CURVE ( 'NONE', #15354, #42101, #33160, .T. ) ;
#61695 = CARTESIAN_POINT ( 'NONE',  ( -2.174378755909786687, 6.588636630831476104, 69.41550620898735247 ) ) ;
#61696 = ORIENTED_EDGE ( 'NONE', *, *, #36290, .F. ) ;
#61697 = CARTESIAN_POINT ( 'NONE',  ( 275.2557116016002965, 21.94295192046379128, -1.612329923324941516 ) ) ;
#61698 = EDGE_CURVE ( 'NONE', #26839, #40972, #66766, .T. ) ;
#61699 = CARTESIAN_POINT ( 'NONE',  ( 154.0515132159917471, 56.29926936869307497, 57.06238980954113771 ) ) ;
#61700 = LINE ( 'NONE', #13525, #14129 ) ;
#61701 = FACE_OUTER_BOUND ( 'NONE', #11732, .T. ) ;
#61702 = DIRECTION ( 'NONE',  ( 0.000000000000000000, -1.000000000000000000, 0.000000000000000000 ) ) ;
#61703 = ORIENTED_EDGE ( 'NONE', *, *, #59796, .F. ) ;
#61704 = CARTESIAN_POINT ( 'NONE',  ( -12.71191147681863143, 50.07707417820910933, 26.66469066592269499 ) ) ;
#61705 = DIRECTION ( 'NONE',  ( -0.3930250316539278255, 0.9195277725514487965, 0.000000000000000000 ) ) ;
#61706 = ORIENTED_EDGE ( 'NONE', *, *, #42586, .T. ) ;
#61707 = VERTEX_POINT ( 'NONE', #49660 ) ;
#61708 = CARTESIAN_POINT ( 'NONE',  ( 179.0096185093688064, 76.53352131383245194, -50.94553233058115893 ) ) ;
#61709 = CARTESIAN_POINT ( 'NONE',  ( 156.5890478960376413, 58.24007662587946044, 44.37067197906655736 ) ) ;
#61710 = CARTESIAN_POINT ( 'NONE',  ( 41.49663191311347532, 50.03028622612080767, 170.0000000000000000 ) ) ;
#61711 = EDGE_CURVE ( 'NONE', #21790, #45082, #31485, .T. ) ;
#61712 = ORIENTED_EDGE ( 'NONE', *, *, #11245, .F. ) ;
#61713 = DIRECTION ( 'NONE',  ( 0.000000000000000000, -1.000000000000000000, 0.000000000000000000 ) ) ;
#61714 = AXIS2_PLACEMENT_3D ( 'NONE', #42673, #9287, #68712 ) ;
#61715 = CARTESIAN_POINT ( 'NONE',  ( -177.5271152834791621, 92.16916858125016176, 17.56416516644142334 ) ) ;
#61716 = CARTESIAN_POINT ( 'NONE',  ( -2.866724795119729219, 6.618578306599218308, 16.41915603436029514 ) ) ;
#61717 = FACE_OUTER_BOUND ( 'NONE', #22674, .T. ) ;
#61718 = CARTESIAN_POINT ( 'NONE',  ( -86.16504208171677703, 26.41251233979373936, 37.38851751404891388 ) ) ;
#61719 = CARTESIAN_POINT ( 'NONE',  ( -23.99957301099517437, 9.503061049698496632, -16.95513486474544251 ) ) ;
#61720 = CARTESIAN_POINT ( 'NONE',  ( 139.6203063421347679, 45.01495791936839908, 5.340914006301072270 ) ) ;
#61721 = ORIENTED_EDGE ( 'NONE', *, *, #463, .F. ) ;
#61722 = DIRECTION ( 'NONE',  ( -0.000000000000000000, -0.000000000000000000, -1.000000000000000000 ) ) ;
#61723 = CARTESIAN_POINT ( 'NONE',  ( 427.4999999999999432, -17.50000000000000000, 20.00000000000000000 ) ) ;
#61724 = FACE_BOUND ( 'NONE', #19271, .T. ) ;
#61725 = DIRECTION ( 'NONE',  ( 0.000000000000000000, 1.224646799147353207E-16, 1.000000000000000000 ) ) ;
#61727 = EDGE_LOOP ( 'NONE', ( #44799, #60265, #9093, #20010, #52704, #30175, #32807 ) ) ;
#61726 = LINE ( 'NONE', #13552, #65811 ) ;
#61728 = CARTESIAN_POINT ( 'NONE',  ( 82.74007713545066167, 18.13042311233564163, -49.73892840124477743 ) ) ;
#61729 = VECTOR ( 'NONE', #61814, 1000.000000000000114 ) ;
#61730 = EDGE_LOOP ( 'NONE', ( #30660, #63824, #26454, #27755 ) ) ;
#61731 = CARTESIAN_POINT ( 'NONE',  ( -148.6409722988649662, 63.44808865916662199, 72.51830521237032201 ) ) ;
#61732 = DIRECTION ( 'NONE',  ( -0.3930250316539148359, -0.9195277725514544587, 0.000000000000000000 ) ) ;
#61733 = LINE ( 'NONE', #56458, #7398 ) ;
#61734 = CARTESIAN_POINT ( 'NONE',  ( 185.5572090022886016, 83.24697331286184010, -10.84236386202956304 ) ) ;
#61735 = DIRECTION ( 'NONE',  ( 0.000000000000000000, 0.000000000000000000, 1.000000000000000000 ) ) ;
#61736 = CARTESIAN_POINT ( 'NONE',  ( -79.62207341875655686, 23.76621716825509978, -8.316621442820189003 ) ) ;
#61737 = CARTESIAN_POINT ( 'NONE',  ( 0.000000000000000000, 0.000000000000000000, 41.38025477438755928 ) ) ;
#61738 = CARTESIAN_POINT ( 'NONE',  ( -48.58011387679029269, 14.07568064779664674, 34.02037858821316973 ) ) ;
#61739 = VERTEX_POINT ( 'NONE', #39140 ) ;
#61740 = VERTEX_POINT ( 'NONE', #56008 ) ;
#61741 = CARTESIAN_POINT ( 'NONE',  ( -65.00200000000002376, 1.250000000000011102, 43.58025477438756923 ) ) ;
#61742 = CARTESIAN_POINT ( 'NONE',  ( 41.66904755831208007, -15.55634918610412853, 0.000000000000000000 ) ) ;
#61743 = VECTOR ( 'NONE', #13315, 1000.000000000000000 ) ;
#61744 = DIRECTION ( 'NONE',  ( 1.000000000000000000, 0.000000000000000000, 0.000000000000000000 ) ) ;
#61745 = EDGE_CURVE ( 'NONE', #49052, #33190, #59871, .T. ) ;
#61746 = CARTESIAN_POINT ( 'NONE',  ( 181.0840389613909736, 78.60582251573005408, -51.22505766587963905 ) ) ;
#61747 = CARTESIAN_POINT ( 'NONE',  ( 31.11269837220800127, -26.11269837220812562, 2.000000000000001776 ) ) ;
#61748 = DIRECTION ( 'NONE',  ( -1.000000000000000000, 0.000000000000000000, 0.000000000000000000 ) ) ;
#61749 = CARTESIAN_POINT ( 'NONE',  ( 164.9559213734325169, 63.71338633026441300, -69.92522862138935125 ) ) ;
#61750 = ORIENTED_EDGE ( 'NONE', *, *, #57972, .T. ) ;
#61751 = VERTEX_POINT ( 'NONE', #18365 ) ;
#61752 = ORIENTED_EDGE ( 'NONE', *, *, #53429, .T. ) ;
#61753 = DIRECTION ( 'NONE',  ( 1.000000000000000000, -0.000000000000000000, -0.000000000000000000 ) ) ;
#61754 = CARTESIAN_POINT ( 'NONE',  ( -71.97767679134960872, 19.88555875055813971, 94.99999999999866418 ) ) ;
#61755 = CARTESIAN_POINT ( 'NONE',  ( 37.70910994512001224, 9.209110272746713122, -50.43038720028041411 ) ) ;
#61756 = CARTESIAN_POINT ( 'NONE',  ( 63.01563776193091826, 12.67277567978498531, -50.72069083216976537 ) ) ;
#61757 = CARTESIAN_POINT ( 'NONE',  ( -15.55634918610405748, -15.55634918610400774, 0.000000000000000000 ) ) ;
#61758 = CARTESIAN_POINT ( 'NONE',  ( -29.70166638324964126, 57.83280658984259048, 41.38025477438755928 ) ) ;
#61759 = CARTESIAN_POINT ( 'NONE',  ( 433.3728120124415568, 388.0000000000066507, -132.4852380479447902 ) ) ;
#61760 = CONICAL_SURFACE ( 'NONE', #14619, 8.000000000000001776, 1.047197551196595855 ) ;
#61761 = CARTESIAN_POINT ( 'NONE',  ( 60.63380853769238854, 13.16344960520421736, 30.19706154477051285 ) ) ;
#61762 = FACE_OUTER_BOUND ( 'NONE', #27353, .T. ) ;
#61763 = ORIENTED_EDGE ( 'NONE', *, *, #6819, .F. ) ;
#61764 = FACE_OUTER_BOUND ( 'NONE', #44517, .T. ) ;
#61765 = CARTESIAN_POINT ( 'NONE',  ( 0.000000000000000000, 0.000000000000000000, 0.000000000000000000 ) ) ;
#61766 = CARTESIAN_POINT ( 'NONE',  ( -189.9638655956219964, 108.0957249433520673, -45.34231387932501178 ) ) ;
#61767 = CARTESIAN_POINT ( 'NONE',  ( -144.2029146819478740, 59.80706661873671948, 16.70020471700040332 ) ) ;
#61768 = CARTESIAN_POINT ( 'NONE',  ( 19.54452863209719382, 7.657034792877148277, -9.664348475683180340 ) ) ;
#61769 = CARTESIAN_POINT ( 'NONE',  ( -109.7816385129979153, 36.75776661907243437, -69.85981554950058126 ) ) ;
#61770 = EDGE_CURVE ( 'NONE', #52584, #63745, #32363, .T. ) ;
#61771 = CARTESIAN_POINT ( 'NONE',  ( 126.6464677212869816, 38.39096133771045061, -18.81003903715838987 ) ) ;
#61772 = EDGE_LOOP ( 'NONE', ( #10045, #28781, #18108, #38562 ) ) ;
#61773 = CARTESIAN_POINT ( 'NONE',  ( 703.8385388596457233, 904.8872677060420529, 735.5068267248702796 ) ) ;
#61774 = EDGE_CURVE ( 'NONE', #51387, #64093, #5230, .T. ) ;
#61775 = AXIS2_PLACEMENT_3D ( 'NONE', #10595, #64415, #11285 ) ;
#61776 = LINE ( 'NONE', #4089, #50944 ) ;
#61777 = CARTESIAN_POINT ( 'NONE',  ( -34.06637338149495520, 11.05895377318623574, -49.84616098674828777 ) ) ;
#61778 = CARTESIAN_POINT ( 'NONE',  ( -63.00000000000000000, 0.000000000000000000, 170.0000000000000000 ) ) ;
#61779 = CONTEXT_DEPENDENT_SHAPE_REPRESENTATION ( #9902, #53969 ) ;
#61780 = CARTESIAN_POINT ( 'NONE',  ( -169.7991992212453738, 83.50566726453351407, 85.28103951956639150 ) ) ;
#61781 = VERTEX_POINT ( 'NONE', #8513 ) ;
#61782 = CARTESIAN_POINT ( 'NONE',  ( 126.4757069339777473, 38.29528077539267628, 8.808907411169407453 ) ) ;
#61783 = VECTOR ( 'NONE', #61836, 1000.000000000000114 ) ;
#61784 = ADVANCED_BREP_SHAPE_REPRESENTATION ( '', ( #16293, #66832 ), #51149 ) ;
#61785 = CARTESIAN_POINT ( 'NONE',  ( -143.2464978228199186, 59.04559547356112148, -11.33080930835344624 ) ) ;
#61786 = CARTESIAN_POINT ( 'NONE',  ( 0.000000000000000000, 0.000000000000000000, 85.00000000000000000 ) ) ;
#61787 = ORIENTED_EDGE ( 'NONE', *, *, #6348, .F. ) ;
#61788 = CARTESIAN_POINT ( 'NONE',  ( 152.1975304496806700, 54.91466247927352384, 85.25451727479598674 ) ) ;
#61789 = EDGE_CURVE ( 'NONE', #36104, #25372, #47901, .T. ) ;
#61790 = ORIENTED_EDGE ( 'NONE', *, *, #47627, .T. ) ;
#61791 = CARTESIAN_POINT ( 'NONE',  ( -59.96408504033279740, 17.10126854471816316, 16.66205370559185539 ) ) ;
#61792 = CARTESIAN_POINT ( 'NONE',  ( 127.2202105166096402, 37.55913282978156786, 33.50704232745487587 ) ) ;
#61793 = CARTESIAN_POINT ( 'NONE',  ( -156.7435307435794130, 71.93726016406968427, 36.22848380757431386 ) ) ;
#61794 = VECTOR ( 'NONE', #18853, 1000.000000000000114 ) ;
#61795 = EDGE_CURVE ( 'NONE', #5941, #21329, #7195, .T. ) ;
#61796 = EDGE_CURVE ( 'NONE', #27866, #18637, #68293, .T. ) ;
#61797 = CARTESIAN_POINT ( 'NONE',  ( 26.12852347772543737, 100.0000000000000000, 129.5802547743875550 ) ) ;
#61798 = LINE ( 'NONE', #68137, #40636 ) ;
#61800 = EDGE_LOOP ( 'NONE', ( #64124, #10545 ) ) ;
#61799 = DIRECTION ( 'NONE',  ( -0.000000000000000000, -0.000000000000000000, -1.000000000000000000 ) ) ;
#61801 = CARTESIAN_POINT ( 'NONE',  ( -3.791772492091277424, 7.668372357990064891, -90.22677180356119209 ) ) ;
#61802 = ORIENTED_EDGE ( 'NONE', *, *, #7656, .F. ) ;
#61803 = ORIENTED_EDGE ( 'NONE', *, *, #31365, .F. ) ;
#61804 = CARTESIAN_POINT ( 'NONE',  ( 173.6737675136087660, 72.80308721038095143, 35.61421337580090807 ) ) ;
#61805 = CARTESIAN_POINT ( 'NONE',  ( 15.78827728214693416, 6.500811158483329244, -62.36349468914946925 ) ) ;
#61807 = ORIENTED_EDGE ( 'NONE', *, *, #10134, .F. ) ;
#61806 = CARTESIAN_POINT ( 'NONE',  ( -132.6092625803567273, 52.31125232006263559, 68.31422680659306934 ) ) ;
#61808 = CARTESIAN_POINT ( 'NONE',  ( -96.26864862082260288, 30.94441745358434304, 87.21210164009336552 ) ) ;
#61809 = VECTOR ( 'NONE', #50044, 1000.000000000000000 ) ;
#61810 = CARTESIAN_POINT ( 'NONE',  ( -71.42007367207959589, 20.75704712149296682, -44.61501727073203938 ) ) ;
#61811 = ORIENTED_EDGE ( 'NONE', *, *, #40051, .T. ) ;
#61812 = LINE ( 'NONE', #13981, #51351 ) ;
#61813 = DIRECTION ( 'NONE',  ( 0.000000000000000000, 0.000000000000000000, 1.000000000000000000 ) ) ;
#61814 = DIRECTION ( 'NONE',  ( 0.8584487936018655452, 0.5128992774059070170, 0.000000000000000000 ) ) ;
#61815 = CARTESIAN_POINT ( 'NONE',  ( -133.3944793432480367, 52.87251459353622352, 11.53032100427611795 ) ) ;
#61816 = CARTESIAN_POINT ( 'NONE',  ( 70.51583798635766698, 15.57951509147423330, -70.30715017899500197 ) ) ;
#61817 = VERTEX_POINT ( 'NONE', #52106 ) ;
#61818 = ORIENTED_EDGE ( 'NONE', *, *, #32018, .T. ) ;
#61819 = CARTESIAN_POINT ( 'NONE',  ( -142.5042386072304055, 59.74110826975218203, -18.20533799458240409 ) ) ;
#61820 = DIRECTION ( 'NONE',  ( 0.000000000000000000, 0.000000000000000000, 1.000000000000000000 ) ) ;
#61821 = CARTESIAN_POINT ( 'NONE',  ( -31.11269837220806878, 5.000000000000056843, 0.000000000000000000 ) ) ;
#61822 = EDGE_CURVE ( 'NONE', #40305, #69105, #37819, .T. ) ;
#61823 = CARTESIAN_POINT ( 'NONE',  ( 0.000000000000000000, 0.000000000000000000, 0.000000000000000000 ) ) ;
#61824 = DIRECTION ( 'NONE',  ( 0.000000000000000000, 0.000000000000000000, 1.000000000000000000 ) ) ;
#61825 = DIRECTION ( 'NONE',  ( 0.000000000000000000, -1.000000000000000000, 0.000000000000000000 ) ) ;
#61826 = CARTESIAN_POINT ( 'NONE',  ( -167.1540252468942356, 80.72321878831101571, -73.60722793262152663 ) ) ;
#61827 = ORIENTED_EDGE ( 'NONE', *, *, #48720, .T. ) ;
#61828 = DIRECTION ( 'NONE',  ( -0.9639628606958512425, -0.2660368455666826670, 0.000000000000000000 ) ) ;
#61829 = ORIENTED_EDGE ( 'NONE', *, *, #5405, .F. ) ;
#61830 = EDGE_CURVE ( 'NONE', #62112, #27226, #19776, .T. ) ;
#61831 = CARTESIAN_POINT ( 'NONE',  ( 33.03722315490661998, 7.666819786578626506, 41.38888860195424968 ) ) ;
#61832 = VERTEX_POINT ( 'NONE', #26414 ) ;
#61833 = CARTESIAN_POINT ( 'NONE',  ( -442.6627218934914367, 399.9999999999998863, -141.4497041420118251 ) ) ;
#61834 = DIRECTION ( 'NONE',  ( -0.1785568947986370669, 0.9839295885986296675, 2.500042656554809847E-16 ) ) ;
#61835 = CYLINDRICAL_SURFACE ( 'NONE', #47846, 7.500000000000013323 ) ;
#61836 = DIRECTION ( 'NONE',  ( 0.3090169943749582759, -0.9510565162951499785, 0.000000000000000000 ) ) ;
#61837 = CARTESIAN_POINT ( 'NONE',  ( 32.14349651933086705, 7.576119504381665593, 8.618131405027169123 ) ) ;
#61838 = CARTESIAN_POINT ( 'NONE',  ( -24.98026281234600887, 0.9932118737287082277, 0.000000000000000000 ) ) ;
#61839 = AXIS2_PLACEMENT_3D ( 'NONE', #39708, #67157, #28453 ) ;
#61840 = CARTESIAN_POINT ( 'NONE',  ( 150.4544126017350720, 52.39556706174411005, -46.28865209072233000 ) ) ;
#61841 = B_SPLINE_CURVE_WITH_KNOTS ( 'NONE', 3,
 ( #39257, #50843, #2661, #35016, #24121, #45216, #56461, #55417, #8288, #28702, #51198, #24474, #38909, #12173, #50150, #1975, #62083, #51877, #68076, #25853, #14931, #63474, #4046, #51546, #41335, #14257, #9671, #52565, #30779, #46246, #3689, #35715, #19878, #67383, #41671, #46594, #40980, #13900, #25165, #67725, #58190, #68413, #3351, #62788, #36746, #36398 ),
 .UNSPECIFIED., .F., .F.,
 ( 4, 2, 2, 2, 2, 2, 2, 2, 2, 2, 2, 2, 2, 2, 2, 2, 2, 2, 2, 2, 2, 2, 4 ),
 ( 0.02584318557310391617, 0.02743529570732761852, 0.02823135077443945928, 0.02902740584155130005, 0.03061951597577497464, 0.03221162610999864923, 0.03380373624422232381, 0.03459979131133418540, 0.03539584637844603310, 0.03619190144555788774, 0.03698795651266974238, 0.03858006664689345167, 0.03937612171400529937, 0.04017217678111716095, 0.04096823184822900865, 0.04176428691534087023, 0.04335639704956461421, 0.04494850718378835819, 0.04654061731801210910, 0.04813272745223585308, 0.04892878251934774936, 0.04972483758645964563, 0.05131694772068339655 ),
 .UNSPECIFIED. ) ;
#61842 = EDGE_LOOP ( 'NONE', ( #64061, #8437, #59786, #41739 ) ) ;
#61843 = CARTESIAN_POINT ( 'NONE',  ( -103.1191803759318191, 33.20880928687111577, -88.73880487180355203 ) ) ;
#61844 = VERTEX_POINT ( 'NONE', #4952 ) ;
#61845 = DIRECTION ( 'NONE',  ( -1.000000000000000000, 0.000000000000000000, 0.000000000000000000 ) ) ;
#61846 = CARTESIAN_POINT ( 'NONE',  ( -58.76099769480629931, 16.75353773354893860, 71.18551801496039388 ) ) ;
#61847 = CARTESIAN_POINT ( 'NONE',  ( 311.9975424824652350, 172.0000000000000284, 536.6193948016162949 ) ) ;
#61848 = ORIENTED_EDGE ( 'NONE', *, *, #44800, .F. ) ;
#61849 = EDGE_CURVE ( 'NONE', #36237, #1174, #33983, .T. ) ;
#61850 = DIRECTION ( 'NONE',  ( -0.000000000000000000, -1.000000000000000000, -0.000000000000000000 ) ) ;
#61851 = CARTESIAN_POINT ( 'NONE',  ( -9.763294602873862971, 7.024900256480052896, -62.51313501726206567 ) ) ;
#61852 = DIRECTION ( 'NONE',  ( 0.000000000000000000, 0.000000000000000000, -1.000000000000000000 ) ) ;
#61853 = ADVANCED_FACE ( 'NONE', ( #63235 ), #35465, .T. ) ;
#61854 = CARTESIAN_POINT ( 'NONE',  ( 134.7770330630253284, 41.98246829846537054, -36.06570861580060949 ) ) ;
#61855 = EDGE_CURVE ( 'NONE', #42670, #4994, #9083, .T. ) ;
#61856 = VERTEX_POINT ( 'NONE', #19986 ) ;
#61857 = EDGE_CURVE ( 'NONE', #7708, #19981, #193, .T. ) ;
#61858 = CARTESIAN_POINT ( 'NONE',  ( -156.4966862384869160, 71.70877417666515896, 67.83814759271207606 ) ) ;
#61859 = CARTESIAN_POINT ( 'NONE',  ( -118.6288898061518893, 41.89286798341292695, 36.23774008308858186 ) ) ;
#61860 = CARTESIAN_POINT ( 'NONE',  ( -57.42615654242919732, 15.33060010148603780, -35.59764363562960199 ) ) ;
#61861 = ORIENTED_EDGE ( 'NONE', *, *, #5937, .F. ) ;
#61862 = DIRECTION ( 'NONE',  ( -3.081487911019579554E-32, -1.000000000000000000, -3.469446951953612956E-17 ) ) ;
#61863 = CARTESIAN_POINT ( 'NONE',  ( 126.4143409752912817, 38.26092613416376764, 91.69694997615445686 ) ) ;
#61864 = CARTESIAN_POINT ( 'NONE',  ( 113.8748103246145575, 30.59837980920001854, 43.69098323372512738 ) ) ;
#61865 = CARTESIAN_POINT ( 'NONE',  ( 93.27435913120712030, 21.79585130525710568, -93.43499286684529181 ) ) ;
#61866 = B_SPLINE_CURVE_WITH_KNOTS ( 'NONE', 3,
 ( #47817, #68591, #69277, #20065, #21104, #64002, #8829, #46438, #67919, #41518, #11215, #11555, #28093, #26720, #48831, #17184, #64695, #58708, #32682, #43217, #54823, #33394, #6295, #54107, #15813, #5933, #53430, #11921, #10525, #22827, #48149, #65396, #16502, #31998, #37256, #59059, #38657, #6644, #27745, #21430, #27393, #29953, #5259, #37960 ),
 .UNSPECIFIED., .F., .F.,
 ( 4, 2, 2, 2, 2, 2, 2, 2, 2, 2, 2, 2, 2, 2, 2, 2, 2, 2, 2, 2, 2, 4 ),
 ( 0.02432640572110344318, 0.02583721026359364972, 0.02659261253483873391, 0.02734801480608381810, 0.02885881934857401770, 0.02961422161981914006, 0.03036962389106425894, 0.03188042843355446548, 0.03339123297604467550, 0.03414663524728978050, 0.03490203751853487857, 0.03641284206102507470, 0.03716824433227017277, 0.03792364660351526390, 0.03943445114600544615, 0.04094525568849563535, 0.04245606023098581067, 0.04396686477347599292, 0.04472226704472108405, 0.04547766931596616824, 0.04698847385845635050, 0.04849927840094651887 ),
 .UNSPECIFIED. ) ;
#61867 = DIRECTION ( 'NONE',  ( -0.000000000000000000, -1.000000000000000000, -0.000000000000000000 ) ) ;
#61868 = ORIENTED_EDGE ( 'NONE', *, *, #16598, .F. ) ;
#61869 = CARTESIAN_POINT ( 'NONE',  ( 159.6725804802005939, 59.38339663535512614, -9.596184105213222182 ) ) ;
#61870 = CARTESIAN_POINT ( 'NONE',  ( 115.2288739107204947, 31.25773204386717197, -75.87499467958308230 ) ) ;
#61871 = CARTESIAN_POINT ( 'NONE',  ( 67.56108154898467433, 13.77276756375644950, 70.14326033379539638 ) ) ;
#61872 = CARTESIAN_POINT ( 'NONE',  ( 140.0820590176526252, 46.51134312115247127, 5.975627082199469697 ) ) ;
#61873 = LINE ( 'NONE', #67870, #43140 ) ;
#61874 = CIRCLE ( 'NONE', #51789, 24.17157287525367693 ) ;
#61875 = EDGE_CURVE ( 'NONE', #28828, #28769, #57271, .T. ) ;
#61876 = EDGE_CURVE ( 'NONE', #24043, #12796, #15537, .T. ) ;
#61877 = ADVANCED_FACE ( 'NONE', ( #46014 ), #67481, .T. ) ;
#61878 = STYLED_ITEM ( 'NONE', ( #29874 ), #18268 ) ;
#61879 = ORIENTED_EDGE ( 'NONE', *, *, #53495, .F. ) ;
#61880 = ADVANCED_FACE ( 'NONE', ( #40732 ), #62191, .T. ) ;
#61881 = LINE ( 'NONE', #2461, #2458 ) ;
#61882 = AXIS2_PLACEMENT_3D ( 'NONE', #39324, #11882, #1336 ) ;
#61883 = VERTEX_POINT ( 'NONE', #14008 ) ;
#61884 = CARTESIAN_POINT ( 'NONE',  ( -29.70166638324964126, 57.83280658984259048, 43.58025477438756923 ) ) ;
#61885 = CARTESIAN_POINT ( 'NONE',  ( 127.7862882585783808, 37.87790449424836936, 86.28152948240347087 ) ) ;
#61886 = ORIENTED_EDGE ( 'NONE', *, *, #38417, .T. ) ;
#61887 = CARTESIAN_POINT ( 'NONE',  ( 164.6561571795774626, 64.77723933022092240, -41.40462224256973656 ) ) ;
#61888 = DIRECTION ( 'NONE',  ( -0.9988488985473030768, 0.000000000000000000, 0.04796746679614544151 ) ) ;
#61889 = AXIS2_PLACEMENT_3D ( 'NONE', #18747, #55683, #34600 ) ;
#61890 = CARTESIAN_POINT ( 'NONE',  ( 60.58000000000000540, -36.09918303830819752, 10.41169613715280740 ) ) ;
#61891 = CARTESIAN_POINT ( 'NONE',  ( 164.7167608259061353, 63.51199216609071385, -45.57758983525081220 ) ) ;
#61892 = ORIENTED_EDGE ( 'NONE', *, *, #18012, .T. ) ;
#61893 = PLANE ( 'NONE',  #52444 ) ;
#61894 = CARTESIAN_POINT ( 'NONE',  ( 61.40555507485842668, 13.33627009881806558, 83.66953863785889212 ) ) ;
#61895 = CARTESIAN_POINT ( 'NONE',  ( 154.9766071814075588, 57.00087550806519232, -90.23040783010065979 ) ) ;
#61896 = CARTESIAN_POINT ( 'NONE',  ( -190.6985136298601731, 109.1272424661242582, 94.99999999999866418 ) ) ;
#61897 = DIRECTION ( 'NONE',  ( 0.1342332658176667304, -0.9909497617679331460, 0.000000000000000000 ) ) ;
#61898 = CARTESIAN_POINT ( 'NONE',  ( 36.17848201055296897, 9.023908545482070664, -89.98582735140863065 ) ) ;
#61899 = CARTESIAN_POINT ( 'NONE',  ( 132.7179291807800325, 40.74118679001687582, -77.78442630836887872 ) ) ;
#61900 = EDGE_LOOP ( 'NONE', ( #44287, #50723, #30783, #51965 ) ) ;
#61901 = LINE ( 'NONE', #40117, #27578 ) ;
#61902 = CARTESIAN_POINT ( 'NONE',  ( -8.314488422519710653, 7.931352979988687935, 56.96013162991090439 ) ) ;
#61903 = VERTEX_POINT ( 'NONE', #62892 ) ;
#61904 = CARTESIAN_POINT ( 'NONE',  ( -156.6644740249450649, 71.86407434531901117, -44.57184474382414408 ) ) ;
#61905 = CARTESIAN_POINT ( 'NONE',  ( 210.5008983495072243, 116.4753531594351159, -12.22384055568752892 ) ) ;
#61906 = DIRECTION ( 'NONE',  ( 0.000000000000000000, 1.000000000000000000, -0.000000000000000000 ) ) ;
#61907 = CARTESIAN_POINT ( 'NONE',  ( -3.862560291631543574, 7.672660553664872651, 31.24333188717660192 ) ) ;
#61908 = CARTESIAN_POINT ( 'NONE',  ( 57.45325234994688657, 11.45088831722005906, 85.96000542775017550 ) ) ;
#61909 = CARTESIAN_POINT ( 'NONE',  ( -49.43915770973592316, 13.24768844696975378, -64.56308494239007700 ) ) ;
#61910 = CARTESIAN_POINT ( 'NONE',  ( 206.6955592216990851, 109.1214665502618146, -51.06646129112117904 ) ) ;
#61911 = CARTESIAN_POINT ( 'NONE',  ( 178.1903523079566298, 75.72906488635186406, 3.031147140003530804 ) ) ;
#61912 = CARTESIAN_POINT ( 'NONE',  ( -58.96922974609610435, 15.76655591015166102, 4.571986130225868195 ) ) ;
#61913 = ORIENTED_EDGE ( 'NONE', *, *, #37079, .F. ) ;
#61914 = EDGE_CURVE ( 'NONE', #43775, #54100, #40390, .T. ) ;
#61915 = DIRECTION ( 'NONE',  ( -0.000000000000000000, -0.000000000000000000, -1.000000000000000000 ) ) ;
#61916 = EDGE_LOOP ( 'NONE', ( #51975, #41978 ) ) ;
#61917 = CARTESIAN_POINT ( 'NONE',  ( -130.2647544212423725, 131.3624518482485541, 0.000000000000000000 ) ) ;
#61918 = PLANE ( 'NONE',  #33209 ) ;
#61919 = CARTESIAN_POINT ( 'NONE',  ( 45.49006904354232717, 9.279592366778889101, 59.87143817380967192 ) ) ;
#61920 = DIRECTION ( 'NONE',  ( 0.7530714660036099684, 0.6579387259397136978, 0.000000000000000000 ) ) ;
#61921 = CARTESIAN_POINT ( 'NONE',  ( -4.675860265596308629, 6.706201026861161374, 84.49030423809293211 ) ) ;
#61922 = AXIS2_PLACEMENT_3D ( 'NONE', #43767, #525, #10724 ) ;
#61923 = CARTESIAN_POINT ( 'NONE',  ( -5.767955557622883589E-14, -31.11269837220806878, 0.000000000000000000 ) ) ;
#61924 = CIRCLE ( 'NONE', #43938, 65.00000000000000000 ) ;
#61925 = FACE_OUTER_BOUND ( 'NONE', #54160, .T. ) ;
#61926 = CARTESIAN_POINT ( 'NONE',  ( -165.7138623879809529, 79.24467249981145756, 66.38117368143906560 ) ) ;
#61927 = ORIENTED_EDGE ( 'NONE', *, *, #47825, .T. ) ;
#61928 = ORIENTED_EDGE ( 'NONE', *, *, #17667, .F. ) ;
#61929 = ADVANCED_FACE ( 'NONE', ( #41089 ), #40091, .T. ) ;
#61930 = FACE_OUTER_BOUND ( 'NONE', #32656, .T. ) ;
#61931 = LINE ( 'NONE', #13755, #52379 ) ;
#61932 = B_SPLINE_CURVE_WITH_KNOTS ( 'NONE', 3,
 ( #27725, #45297, #23159, #12962, #66439, #65375, #28071, #2059, #17161, #6268, #50579, #55868, #66783, #2400, #49875, #1701, #40028, #49163, #33718, #1002, #22454, #6974, #43893, #38635, #18227, #54802, #44608, #1350, #60077, #12255, #55504, #11895, #33375, #22803, #6623, #44248, #17878, #65729, #39336, #60779, #12603, #34062, #7331 ),
 .UNSPECIFIED., .F., .F.,
 ( 4, 2, 2, 2, 2, 2, 2, 2, 1, 2, 2, 2, 2, 2, 2, 2, 2, 2, 2, 2, 2, 4 ),
 ( 3.469446951953614189E-18, 0.001466285743483492117, 0.002199428615225232538, 0.002932571486966972958, 0.004398857230450428646, 0.005865142973933883466, 0.007331428717417340021, 0.008064571589159083911, 0.008797714460900827801, 0.009530857332642571692, 0.01026400020438431732, 0.01173028594786780857, 0.01319657169135129808, 0.01466285743483479106, 0.01539600030657653496, 0.01612914317831827885, 0.01759542892180177009, 0.01906171466528526134, 0.01979485753702700870, 0.02052800040876874912, 0.02199428615225223343, 0.02346057189573571775 ),
 .UNSPECIFIED. ) ;
#61934 = CARTESIAN_POINT ( 'NONE',  ( -35.06172987636333005, -15.49744386972411903, 13.32819397642333570 ) ) ;
#61933 = VECTOR ( 'NONE', #57755, 1000.000000000000000 ) ;
#61935 = AXIS2_PLACEMENT_3D ( 'NONE', #32861, #12809, #59926 ) ;
#61936 = B_SPLINE_CURVE_WITH_KNOTS ( 'NONE', 3,
 ( #44057, #33538, #12419, #12067, #6443, #39494, #65538, #32476 ),
 .UNSPECIFIED., .F., .F.,
 ( 4, 2, 2, 4 ),
 ( 0.004673709593152176531, 0.005837709341827659881, 0.007001709090503144099, 0.009329708587854108198 ),
 .UNSPECIFIED. ) ;
#61937 = DIRECTION ( 'NONE',  ( -1.000000000000000000, -1.001918046209079887E-14, 9.729495617646301779E-15 ) ) ;
#61938 = LINE ( 'NONE', #51055, #59955 ) ;
#61939 = EDGE_CURVE ( 'NONE', #37998, #28498, #19629, .T. ) ;
#61940 = ADVANCED_FACE ( 'NONE', ( #14361 ), #68509, .T. ) ;
#61941 = AXIS2_PLACEMENT_3D ( 'NONE', #57353, #62971, #51727 ) ;
#61942 = CARTESIAN_POINT ( 'NONE',  ( 56.52205390515081262, 12.28646189164059344, -12.59121248216328581 ) ) ;
#61943 = EDGE_LOOP ( 'NONE', ( #56137, #50435, #6820, #26864 ) ) ;
#61944 = CARTESIAN_POINT ( 'NONE',  ( 204.6977192012829789, 106.3443248447423457, -63.17048162308526571 ) ) ;
#61945 = CARTESIAN_POINT ( 'NONE',  ( 21.44191228441539465, 7.755009954762289937, -47.97187036235548163 ) ) ;
#61946 = CARTESIAN_POINT ( 'NONE',  ( 9.280894575734579988, 7.385644305345136829, 60.59831840680561044 ) ) ;
#61947 = DIRECTION ( 'NONE',  ( 1.000000000000000000, 0.000000000000000000, 0.000000000000000000 ) ) ;
#61948 = FACE_BOUND ( 'NONE', #18286, .T. ) ;
#61949 = EDGE_LOOP ( 'NONE', ( #31481, #22260 ) ) ;
#61950 = EDGE_LOOP ( 'NONE', ( #59398, #15557 ) ) ;
#61951 = LINE ( 'NONE', #24346, #69332 ) ;
#61952 = CARTESIAN_POINT ( 'NONE',  ( 89.87840278991589571, 21.62393877508910478, -50.08560210100184662 ) ) ;
#61953 = DIRECTION ( 'NONE',  ( -0.000000000000000000, -0.000000000000000000, -1.000000000000000000 ) ) ;
#61954 = CARTESIAN_POINT ( 'NONE',  ( -177.5288247523079121, 93.72924674643515175, 17.56298962112507667 ) ) ;
#61955 = CARTESIAN_POINT ( 'NONE',  ( 12.60449501160847774, 6.419572319999807597, 84.40508385186305418 ) ) ;
#61956 = EDGE_CURVE ( 'NONE', #18072, #60434, #3832, .T. ) ;
#61957 = CARTESIAN_POINT ( 'NONE',  ( 79.38020582286198135, 17.07365509555548400, -72.15476770513920712 ) ) ;
#61958 = EDGE_LOOP ( 'NONE', ( #23148, #32691 ) ) ;
#61959 = EDGE_CURVE ( 'NONE', #37939, #19637, #27104, .T. ) ;
#61960 = CYLINDRICAL_SURFACE ( 'NONE', #34824, 7.500000000000020428 ) ;
#61961 = CARTESIAN_POINT ( 'NONE',  ( 198.4059165548111991, 99.71594270191987164, -39.73513461452476037 ) ) ;
#61962 = ORIENTED_EDGE ( 'NONE', *, *, #6798, .F. ) ;
#61963 = DIRECTION ( 'NONE',  ( -5.055952397801347160E-18, -6.848752866792398399E-19, -1.000000000000000000 ) ) ;
#61964 = EDGE_LOOP ( 'NONE', ( #66467, #1200, #27887, #42161 ) ) ;
#61965 = CARTESIAN_POINT ( 'NONE',  ( 450.2085304802404266, 0.000000000000000000, -250.0000000000000000 ) ) ;
#61966 = CARTESIAN_POINT ( 'NONE',  ( 69.68177367721199289, -20.52767805628082698, 170.0000000000000000 ) ) ;
#61967 = CARTESIAN_POINT ( 'NONE',  ( 89.65730223173022750, 21.54473673261222189, -77.03190999791871718 ) ) ;
#61968 =( REPRESENTATION_RELATIONSHIP ('NONE','NONE', #40274, #57739 ) REPRESENTATION_RELATIONSHIP_WITH_TRANSFORMATION ( #21289 )SHAPE_REPRESENTATION_RELATIONSHIP( ) );
#61969 = VERTEX_POINT ( 'NONE', #27968 ) ;
#61970 = VECTOR ( 'NONE', #33849, 1000.000000000000000 ) ;
#61971 = ORIENTED_EDGE ( 'NONE', *, *, #17309, .F. ) ;
#61972 = CARTESIAN_POINT ( 'NONE',  ( 46.84154678921880333, 10.51341196666389344, 63.27653607351307841 ) ) ;
#61973 = PLANE ( 'NONE',  #19138 ) ;
#61974 = CARTESIAN_POINT ( 'NONE',  ( 102.7983318509014765, 26.68040613344513190, 9.220450153127773163 ) ) ;
#61975 = AXIS2_PLACEMENT_3D ( 'NONE', #40863, #39824, #56696 ) ;
#61976 = ORIENTED_EDGE ( 'NONE', *, *, #41608, .T. ) ;
#61977 = PRODUCT_DEFINITION_SHAPE ( 'NONE', 'NONE',  #69575 ) ;
#61978 = CIRCLE ( 'NONE', #67621, 25.12245591505646303 ) ;
#61979 = PRESENTATION_LAYER_ASSIGNMENT (  '', '', ( #67622 ) ) ;
#61980 = CARTESIAN_POINT ( 'NONE',  ( 174.1422537179815038, 73.24254491731257133, -73.42316486936464059 ) ) ;
#61981 = CARTESIAN_POINT ( 'NONE',  ( -442.9415673952017301, 394.9999999999997726, -125.3784793789377261 ) ) ;
#61982 = CARTESIAN_POINT ( 'NONE',  ( 117.4696399285658686, 32.37118663718647582, -18.65062314217833617 ) ) ;
#61983 = CONICAL_SURFACE ( 'NONE', #41815, 65.00000000000000000, 0.7853981633974497223 ) ;
#61984 = CARTESIAN_POINT ( 'NONE',  ( 83.37782009939536465, 19.39546426214657870, -36.55869151441629583 ) ) ;
#61985 = FACE_OUTER_BOUND ( 'NONE', #53872, .T. ) ;
#61986 = VERTEX_POINT ( 'NONE', #49412 ) ;
#61987 = CLOSED_SHELL ( 'NONE', ( #10205, #31397, #59297, #22226, #30590, #14367, #41460, #2181, #14034, #15329, #46337, #54873, #66885, #18583, #49533, #55536, #19230, #37699, #24870, #62246, #9745, #57492, #65441, #49115, #15959, #11836, #65794, #68679 ) ) ;
#61988 = EDGE_LOOP ( 'NONE', ( #59268, #11977 ) ) ;
#61989 = CARTESIAN_POINT ( 'NONE',  ( 0.08224679563971203089, -6.145890662064649845, 5.355005115540899752 ) ) ;
#61990 = CARTESIAN_POINT ( 'NONE',  ( 179.4227152810058215, 78.36166152262364903, 2.638148450095675557 ) ) ;
#61991 = CARTESIAN_POINT ( 'NONE',  ( 7.762887554996211747E-14, 46.66904755831208718, 85.00100000000000477 ) ) ;
#61992 = CARTESIAN_POINT ( 'NONE',  ( 259.4165763529819060, -27.00000000000000355, 128.9999999999999716 ) ) ;
#61993 = CARTESIAN_POINT ( 'NONE',  ( 126.4083787442700242, 37.10531539900949127, 9.140475197704560628 ) ) ;
#61994 = DIRECTION ( 'NONE',  ( 0.000000000000000000, 0.000000000000000000, 1.000000000000000000 ) ) ;
#61995 = CARTESIAN_POINT ( 'NONE',  ( 202.8553521992888307, 105.5342351882353142, 83.10660119179087246 ) ) ;
#61996 = EDGE_CURVE ( 'NONE', #65404, #2078, #58927, .T. ) ;
#61997 = CARTESIAN_POINT ( 'NONE',  ( 210.5008983495071675, 116.4753531594350875, 41.46526062523980727 ) ) ;
#61998 = CARTESIAN_POINT ( 'NONE',  ( -79.14094329813313777, 23.58034730000056811, 57.26275173013680586 ) ) ;
#61999 = CARTESIAN_POINT ( 'NONE',  ( -14.32120159453989672, 7.401444311907543927, 33.85853709894156793 ) ) ;
#62000 = EDGE_LOOP ( 'NONE', ( #1616, #34574, #52434, #28256 ) ) ;
#62001 = EDGE_CURVE ( 'NONE', #61270, #8605, #22693, .T. ) ;
#62002 = FACE_OUTER_BOUND ( 'NONE', #53124, .T. ) ;
#62003 = ORIENTED_EDGE ( 'NONE', *, *, #32573, .T. ) ;
#62004 = FACE_OUTER_BOUND ( 'NONE', #60996, .T. ) ;
#62005 = B_SPLINE_CURVE_WITH_KNOTS ( 'NONE', 3,
 ( #64067, #59472, #15879, #48552, #27823, #746, #49260, #22200, #43638, #33470, #65467, #17259, #6715, #14345, #62170, #22896, #40713, #60532, #19970, #17620, #30868, #57250, #3436, #62531, #51288, #52311, #61819, #40376, #9065, #12346, #19612, #13992, #55243, #33802, #3102, #35098, #24900, #7066, #18925, #36140, #41072, #24563, #13642, #45996, #41421, #62875 ),
 .UNSPECIFIED., .F., .F.,
 ( 4, 2, 2, 2, 2, 2, 2, 2, 2, 2, 2, 2, 2, 2, 2, 2, 2, 2, 2, 2, 2, 2, 4 ),
 ( 0.000000000000000000, 0.003373244802897266970, 0.004216556003621581977, 0.005059867204345896985, 0.006746489605794529602, 0.007589800806518840273, 0.008433112007243148342, 0.009276423207967458145, 0.01011973440869176621, 0.01180635681014038582, 0.01349297921158900196, 0.01433629041231331176, 0.01517960161303762504, 0.01686622401448622730, 0.01770953521521050761, 0.01855284641593478792, 0.02023946881738338324, 0.02108278001810766356, 0.02192609121883194040, 0.02361271362028050450, 0.02445602482100478481, 0.02529933602172906165, 0.02698595842317762575 ),
 .UNSPECIFIED. ) ;
#62006 = ORIENTED_EDGE ( 'NONE', *, *, #43254, .T. ) ;
#62007 = CARTESIAN_POINT ( 'NONE',  ( -31.43908319763710679, -170.0000000000000000, -15.97264677473816974 ) ) ;
#62008 = CARTESIAN_POINT ( 'NONE',  ( 181.9295958320008424, 80.90438706151871884, -78.03393500570973629 ) ) ;
#62009 = CARTESIAN_POINT ( 'NONE',  ( -38.85841857822266121, 11.95291994873726971, 92.55007051657004524 ) ) ;
#62010 = CARTESIAN_POINT ( 'NONE',  ( -78.66644367742111399, 22.32174330031318732, -88.80455181264524356 ) ) ;
#62011 = CARTESIAN_POINT ( 'NONE',  ( 35.65775178405255730, 7.951994368745585184, -49.62299231391522625 ) ) ;
#62012 = CARTESIAN_POINT ( 'NONE',  ( -109.3553681454883844, 36.52260784104395697, 8.634393988911380546 ) ) ;
#62013 = CARTESIAN_POINT ( 'NONE',  ( 10.83521140779424030, 7.398743030771589346, -48.67192843401519298 ) ) ;
#62014 = CARTESIAN_POINT ( 'NONE',  ( 133.3990214534116774, 41.14886683286417934, -51.01281999844796644 ) ) ;
#62015 = ORIENTED_EDGE ( 'NONE', *, *, #18540, .F. ) ;
#62016 = VERTEX_POINT ( 'NONE', #38885 ) ;
#62017 = EDGE_CURVE ( 'NONE', #25506, #19578, #1587, .T. ) ;
#62018 = CARTESIAN_POINT ( 'NONE',  ( 186.2922852436126959, 85.51514452367332808, 85.09180308946348248 ) ) ;
#62019 = CARTESIAN_POINT ( 'NONE',  ( -50.00000000000001421, -20.00000000000000355, 1.999999999999984457 ) ) ;
#62020 = LINE ( 'NONE', #35301, #59194 ) ;
#62021 = CARTESIAN_POINT ( 'NONE',  ( -27.70005010046228122, 9.007417901453017350, -63.15562276199040781 ) ) ;
#62022 = EDGE_CURVE ( 'NONE', #11917, #11797, #29876, .T. ) ;
#62023 = EDGE_CURVE ( 'NONE', #34941, #36964, #23412, .T. ) ;
#62024 = UNCERTAINTY_MEASURE_WITH_UNIT (LENGTH_MEASURE( 1.000000000000000082E-05 ), #51907, 'distance_accuracy_value', 'NONE');
#62025 = TOROIDAL_SURFACE ( 'NONE', #12629, 20.30000000000000071, 0.3000000000000062061 ) ;
#62026 = CARTESIAN_POINT ( 'NONE',  ( 8.540853903193186270, 6.376814430361481101, 12.61568352143839533 ) ) ;
#62027 = VERTEX_POINT ( 'NONE', #18123 ) ;
#62028 = FACE_OUTER_BOUND ( 'NONE', #51978, .T. ) ;
#62029 = CARTESIAN_POINT ( 'NONE',  ( -61.52761555060400411, 17.56359742150277725, -73.37817215718246189 ) ) ;
#62030 = CARTESIAN_POINT ( 'NONE',  ( 198.7129816317746247, 100.1061386900356069, -66.14231288720782231 ) ) ;
#62031 = VECTOR ( 'NONE', #31969, 1000.000000000000000 ) ;
#62032 = CARTESIAN_POINT ( 'NONE',  ( -180.5231752320737257, 95.76423526868921954, -40.96427428279935157 ) ) ;
#62033 = CARTESIAN_POINT ( 'NONE',  ( -29.68020330876228030, 70.00000000000000000, 4.368699068434031219 ) ) ;
#62034 = CARTESIAN_POINT ( 'NONE',  ( -23.99957301099517437, 9.503061049698491303, 63.57851690664559641 ) ) ;
#62035 = CARTESIAN_POINT ( 'NONE',  ( 106.2339232178672290, 21.75159641080504969, 3.304888597515779125 ) ) ;
#62036 = CARTESIAN_POINT ( 'NONE',  ( -51.13073217147959326, 13.66490163179658879, 71.05935392568744646 ) ) ;
#62037 = AXIS2_PLACEMENT_3D ( 'NONE', #33303, #66707, #44539 ) ;
#62038 = CARTESIAN_POINT ( 'NONE',  ( -1.314022807222069877, 6.554273999800678929, 68.21404729449294280 ) ) ;
#62039 = ORIENTED_EDGE ( 'NONE', *, *, #49593, .F. ) ;
#62040 = CARTESIAN_POINT ( 'NONE',  ( 1.667562369266826661, 64.99262834925669097, 43.58025477438756923 ) ) ;
#62041 = CARTESIAN_POINT ( 'NONE',  ( -2.645453300864630819E-14, -10.55634918610403439, 0.000000000000000000 ) ) ;
#62042 = CARTESIAN_POINT ( 'NONE',  ( -108.9444157621017979, 37.44493815491209432, -65.88002215714232079 ) ) ;
#62043 = CARTESIAN_POINT ( 'NONE',  ( -419.7337897053573670, 395.0000000000063665, -113.5207719538776558 ) ) ;
#62044 = DIRECTION ( 'NONE',  ( -0.9909497617679351444, 0.1342332658176522420, 0.000000000000000000 ) ) ;
#62045 = DIRECTION ( 'NONE',  ( -0.000000000000000000, 1.000000000000000000, -0.000000000000000000 ) ) ;
#62046 = ORIENTED_EDGE ( 'NONE', *, *, #30585, .T. ) ;
#62047 = EDGE_CURVE ( 'NONE', #62713, #69327, #61026, .T. ) ;
#62048 = CARTESIAN_POINT ( 'NONE',  ( 432.4999999999999432, 207.5000000000000284, 0.000000000000000000 ) ) ;
#62049 = CARTESIAN_POINT ( 'NONE',  ( -173.1211646369891355, 88.63826465341151106, 3.977144016177345254 ) ) ;
#62050 = ORIENTED_EDGE ( 'NONE', *, *, #17565, .F. ) ;
#62051 = EDGE_LOOP ( 'NONE', ( #51735, #59947, #54281, #9255 ) ) ;
#62052 = DIRECTION ( 'NONE',  ( -1.000000000000000000, 0.000000000000000000, 0.000000000000000000 ) ) ;
#62053 = CARTESIAN_POINT ( 'NONE',  ( 155.2870855780215038, 57.23765125306422163, 44.09879959064866028 ) ) ;
#62054 = LINE ( 'NONE', #18809, #59434 ) ;
#62055 = ORIENTED_EDGE ( 'NONE', *, *, #62367, .T. ) ;
#62056 = DIRECTION ( 'NONE',  ( -0.000000000000000000, 1.000000000000000000, -0.000000000000000000 ) ) ;
#62057 = CARTESIAN_POINT ( 'NONE',  ( -173.5394735271662228, 87.59446374803708579, 3.977144016177343477 ) ) ;
#62058 = CARTESIAN_POINT ( 'NONE',  ( 0.000000000000000000, 0.000000000000000000, 4.000000000000000000 ) ) ;
#62059 = DIRECTION ( 'NONE',  ( 0.000000000000000000, 0.000000000000000000, -1.000000000000000000 ) ) ;
#62060 = CARTESIAN_POINT ( 'NONE',  ( -85.12122836439577611, 25.97531040437158367, 41.76940575333474470 ) ) ;
#62061 = CARTESIAN_POINT ( 'NONE',  ( -24.18158274621862702, 9.527343002918316373, -17.92767438152212023 ) ) ;
#62062 = CARTESIAN_POINT ( 'NONE',  ( 141.2894128405439176, 46.09731134920846074, 11.20330446142119207 ) ) ;
#62063 = ORIENTED_EDGE ( 'NONE', *, *, #33995, .F. ) ;
#62064 = B_SPLINE_CURVE_WITH_KNOTS ( 'NONE', 3,
 ( #9867, #30630, #4246, #41526, #36940, #52076, #58380, #62978, #31325, #3893, #10189, #31654, #25364, #4576, #53090, #68268, #20073, #14785 ),
 .UNSPECIFIED., .F., .F.,
 ( 4, 2, 2, 2, 2, 2, 2, 2, 4 ),
 ( 0.01384554320395945531, 0.01548911742118727966, 0.01713269163841510401, 0.02041984007287080127, 0.02206341429009864297, 0.02370698850732648119, 0.02452877561594040551, 0.02535056272455432289, 0.02699413694178218540 ),
 .UNSPECIFIED. ) ;
#62065 = CARTESIAN_POINT ( 'NONE',  ( 116.8937673311172603, 32.08228998570057655, -46.89815673556866216 ) ) ;
#62066 = DIRECTION ( 'NONE',  ( 0.000000000000000000, 1.000000000000000000, 0.000000000000000000 ) ) ;
#62067 = CARTESIAN_POINT ( 'NONE',  ( 42.49453823366106064, 8.831814337191470798, -36.28277223276639063 ) ) ;
#62068 = CARTESIAN_POINT ( 'NONE',  ( -73.37451557318128437, 21.44378618812643467, 86.28309517344128210 ) ) ;
#62070 = ORIENTED_EDGE ( 'NONE', *, *, #47261, .T. ) ;
#62069 = CARTESIAN_POINT ( 'NONE',  ( 47.74291447196797833, 190.0000000000000000, -75.60236247897087480 ) ) ;
#62071 = CARTESIAN_POINT ( 'NONE',  ( 79.11678624235125312, 16.99307331934756604, -43.31297501014353202 ) ) ;
#62072 = ORIENTED_EDGE ( 'NONE', *, *, #30171, .F. ) ;
#62073 = VECTOR ( 'NONE', #5841, 1000.000000000000000 ) ;
#62074 = EDGE_CURVE ( 'NONE', #35107, #46320, #67125, .T. ) ;
#62075 = VERTEX_POINT ( 'NONE', #2635 ) ;
#62076 = VECTOR ( 'NONE', #40033, 1000.000000000000000 ) ;
#62077 = CARTESIAN_POINT ( 'NONE',  ( 55.46196446482078812, 34.59309596431376121, 3.125053320693586388E-16 ) ) ;
#62078 = CARTESIAN_POINT ( 'NONE',  ( 80.16761386260780853, 18.37011649821943848, 33.37197744852545611 ) ) ;
#62079 = DIRECTION ( 'NONE',  ( 0.000000000000000000, 1.000000000000000000, 0.000000000000000000 ) ) ;
#62080 = EDGE_CURVE ( 'NONE', #12369, #19058, #55753, .T. ) ;
#62081 = CARTESIAN_POINT ( 'NONE',  ( 437.3372781065086201, 0.000000000000000000, -136.4497041420118251 ) ) ;
#62082 = EDGE_CURVE ( 'NONE', #30638, #56615, #66669, .T. ) ;
#62083 = CARTESIAN_POINT ( 'NONE',  ( -119.1795380580999648, 42.22910606512927956, 61.61258993744711177 ) ) ;
#62084 = CARTESIAN_POINT ( 'NONE',  ( -83.15209219203882185, 25.16621997697718882, -9.740531383382071695 ) ) ;
#62085 = CARTESIAN_POINT ( 'NONE',  ( -179.5186635612084274, 96.12511541314945873, -11.41482807252975462 ) ) ;
#62086 = EDGE_CURVE ( 'NONE', #17852, #11222, #18812, .T. ) ;
#62087 = AXIS2_PLACEMENT_3D ( 'NONE', #43752, #33924, #54660 ) ;
#62088 = CARTESIAN_POINT ( 'NONE',  ( -54.08488990389049889, 15.46443908526321209, 30.36440728263135469 ) ) ;
#62089 = ORIENTED_EDGE ( 'NONE', *, *, #64291, .F. ) ;
#62090 = ORIENTED_EDGE ( 'NONE', *, *, #30117, .T. ) ;
#62091 = CARTESIAN_POINT ( 'NONE',  ( -44.99999999999998579, -22.99999999999998579, 0.000000000000000000 ) ) ;
#62092 = ADVANCED_FACE ( 'NONE', ( #63799 ), #31779, .F. ) ;
#62093 = CARTESIAN_POINT ( 'NONE',  ( -15.55634918610405748, -10.55634918610400597, 2.000000000000001776 ) ) ;
#62094 = CIRCLE ( 'NONE', #23990, 65.00000000000000000 ) ;
#62095 = LINE ( 'NONE', #61058, #61433 ) ;
#62096 = FACE_OUTER_BOUND ( 'NONE', #34509, .T. ) ;
#62097 = CARTESIAN_POINT ( 'NONE',  ( 188.5843222076478582, 86.53342480589839170, -43.42845138699213692 ) ) ;
#62098 = CARTESIAN_POINT ( 'NONE',  ( 18.19980344696536889, 6.589834367837007711, 30.40873729102910517 ) ) ;
#62099 = CARTESIAN_POINT ( 'NONE',  ( 157.4703587214989113, 57.65129005721576050, -62.96873488960130771 ) ) ;
#62100 = ORIENTED_EDGE ( 'NONE', *, *, #30420, .F. ) ;
#62101 = EDGE_LOOP ( 'NONE', ( #40092, #4532, #50345, #21310 ) ) ;
#62102 = VERTEX_POINT ( 'NONE', #20523 ) ;
#62103 = DIRECTION ( 'NONE',  ( 0.000000000000000000, 0.000000000000000000, 1.000000000000000000 ) ) ;
#62104 = CARTESIAN_POINT ( 'NONE',  ( 180.4006926312003714, 77.91522284673895626, -89.91415884680702675 ) ) ;
#62105 = EDGE_CURVE ( 'NONE', #55128, #61056, #9290, .T. ) ;
#62106 = CARTESIAN_POINT ( 'NONE',  ( 70.25990036603481315, 14.47042233282420476, -41.26302775415978630 ) ) ;
#62107 = LINE ( 'NONE', #13246, #14231 ) ;
#62108 = CARTESIAN_POINT ( 'NONE',  ( -57.42826130032240428, 16.37596353166460261, 30.69935087320815015 ) ) ;
#62109 = CARTESIAN_POINT ( 'NONE',  ( -38.45778834351241215, 11.87434869453508135, -67.00674613719260719 ) ) ;
#62110 = CARTESIAN_POINT ( 'NONE',  ( 59.30258796551117939, 12.87111270082601067, 30.77794280086910206 ) ) ;
#62111 = CARTESIAN_POINT ( 'NONE',  ( 0.000000000000000000, 0.000000000000000000, 0.000000000000000000 ) ) ;
#62112 = VERTEX_POINT ( 'NONE', #36724 ) ;
#62113 = CARTESIAN_POINT ( 'NONE',  ( -4.955782654901476292, 6.720825733572403315, -49.86023888739470067 ) ) ;
#62114 = CARTESIAN_POINT ( 'NONE',  ( 39.40195752203892710, -170.0000000000000000, -35.61981746542776506 ) ) ;
#62115 = CARTESIAN_POINT ( 'NONE',  ( 8.000000000000000000, 4.618802153517024500, -0.7145311798163346273 ) ) ;
#62116 = CARTESIAN_POINT ( 'NONE',  ( 16.78635691501517613, 0.000000000000000000, -41.68900338898716740 ) ) ;
#62117 = CARTESIAN_POINT ( 'NONE',  ( 126.6395826915640015, 37.23416510613628105, -18.73613604440101454 ) ) ;
#62118 = CARTESIAN_POINT ( 'NONE',  ( -65.36598343705435354, 0.000000000000000000, 41.38025477438755928 ) ) ;
#62119 = FACE_OUTER_BOUND ( 'NONE', #23584, .T. ) ;
#62120 = VECTOR ( 'NONE', #60810, 1000.000000000000227 ) ;
#62121 = B_SPLINE_CURVE_WITH_KNOTS ( 'NONE', 3,
 ( #29866, #51329, #2788, #46035, #46727, #9104 ),
 .UNSPECIFIED., .F., .F.,
 ( 4, 2, 4 ),
 ( 1.095770181109612726E-06, 0.03239442681617711595, 0.06478775786217311206 ),
 .UNSPECIFIED. ) ;
#62122 = ORIENTED_EDGE ( 'NONE', *, *, #27150, .T. ) ;
#62123 = AXIS2_PLACEMENT_3D ( 'NONE', #64425, #59136, #41592 ) ;
#62124 = PRODUCT_CONTEXT ( 'NONE', #8476, 'mechanical' ) ;
#62125 = CARTESIAN_POINT ( 'NONE',  ( 133.8566784816069344, 42.60093787723652525, -51.02331093239568816 ) ) ;
#62126 = CARTESIAN_POINT ( 'NONE',  ( -33.36965723649377225, 10.93726715887724055, -50.06857660072027727 ) ) ;
#62127 = CARTESIAN_POINT ( 'NONE',  ( -31.90315521289065970, -56.64813493366050068, 43.58025477438756923 ) ) ;
#62128 = ITEM_DEFINED_TRANSFORMATION ( 'NONE', 'NONE', #35524,  #66832 ) ;
#62129 = CARTESIAN_POINT ( 'NONE',  ( 181.0840389613909451, 80.03940679743416808, -36.22505766587961062 ) ) ;
#62130 = ORIENTED_EDGE ( 'NONE', *, *, #17667, .T. ) ;
#62131 = AXIS2_PLACEMENT_3D ( 'NONE', #12526, #50508, #1622 ) ;
#62132 = ORIENTED_EDGE ( 'NONE', *, *, #30440, .F. ) ;
#62133 = CARTESIAN_POINT ( 'NONE',  ( -30.47069031368415182, 9.433993659086596040, -23.42594627002974050 ) ) ;
#62134 = CIRCLE ( 'NONE', #26184, 4.999999999999997335 ) ;
#62135 = DIRECTION ( 'NONE',  ( 1.000000000000000000, 0.000000000000000000, 0.000000000000000000 ) ) ;
#62136 = VERTEX_POINT ( 'NONE', #52202 ) ;
#62137 = AXIS2_PLACEMENT_3D ( 'NONE', #62391, #57119, #36006 ) ;
#62138 = CARTESIAN_POINT ( 'NONE',  ( 150.1388893866326555, 53.40890567970688352, 88.97308815910281510 ) ) ;
#62139 = EDGE_LOOP ( 'NONE', ( #17493, #61481, #5120, #58084 ) ) ;
#62140 = CARTESIAN_POINT ( 'NONE',  ( 127.2358066117906787, 38.72257733469223950, -73.92861135475047263 ) ) ;
#62141 = CARTESIAN_POINT ( 'NONE',  ( 437.3372781065085633, 400.0000000000000568, -141.4497041420118251 ) ) ;
#62142 = CARTESIAN_POINT ( 'NONE',  ( -152.5101325120252795, 68.10842280990928543, 45.10774975830220512 ) ) ;
#62143 = AXIS2_PLACEMENT_3D ( 'NONE', #18855, #50857, #52239 ) ;
#62144 = CARTESIAN_POINT ( 'NONE',  ( 0.000000000000000000, -6.928203230275503444, 4.000000000000010658 ) ) ;
#62145 = DIRECTION ( 'NONE',  ( -1.000000000000000000, 0.000000000000000000, 0.000000000000000000 ) ) ;
#62147 = EDGE_LOOP ( 'NONE', ( #10053, #55661 ) ) ;
#62146 = CARTESIAN_POINT ( 'NONE',  ( 64.52696037203355672, 10.43950074664854633, 6.377659838150160580E-18 ) ) ;
#62148 = EDGE_CURVE ( 'NONE', #30444, #64346, #52542, .T. ) ;
#62149 = CARTESIAN_POINT ( 'NONE',  ( -7.825402957745085430, 7.899365992529253866, -89.10717191287116634 ) ) ;
#62150 = ORIENTED_EDGE ( 'NONE', *, *, #6413, .F. ) ;
#62151 = ORIENTED_EDGE ( 'NONE', *, *, #48372, .F. ) ;
#62152 = CARTESIAN_POINT ( 'NONE',  ( -168.7314919967217861, 83.83749564070828342, 17.57661599061045976 ) ) ;
#62153 = CARTESIAN_POINT ( 'NONE',  ( 16.77391662606471101, 6.533867394142991891, -62.41210858207633549 ) ) ;
#62155 = VERTEX_POINT ( 'NONE', #41646 ) ;
#62154 = CARTESIAN_POINT ( 'NONE',  ( -132.2161740628506550, 52.03204870034955576, 60.92179302142604769 ) ) ;
#62156 = DIRECTION ( 'NONE',  ( -0.000000000000000000, 1.000000000000000000, -0.000000000000000000 ) ) ;
#62157 = FACE_BOUND ( 'NONE', #33563, .T. ) ;
#62158 = VERTEX_POINT ( 'NONE', #37056 ) ;
#62159 = CARTESIAN_POINT ( 'NONE',  ( 178.3500803230180907, 77.29460076174662220, -90.39474168206896820 ) ) ;
#62160 = ADVANCED_FACE ( 'NONE', ( #68388 ), #47591, .F. ) ;
#62161 = CARTESIAN_POINT ( 'NONE',  ( 138.2136629441929472, 45.30947856186676859, 30.88737808275690355 ) ) ;
#62163 = CARTESIAN_POINT ( 'NONE',  ( 115.7731501832035832, 32.64791439093733061, 32.02106840025158618 ) ) ;
#62162 = COLOUR_RGB ( '',0.7921568627450980005, 0.8196078431372548767, 0.9333333333333333481 ) ;
#62164 = CARTESIAN_POINT ( 'NONE',  ( 0.000000000000000000, 0.000000000000000000, 0.000000000000000000 ) ) ;
#62165 = CARTESIAN_POINT ( 'NONE',  ( 63.98689050258322908, 13.93365232918667651, -62.61274692488039051 ) ) ;
#62166 = VERTEX_POINT ( 'NONE', #35692 ) ;
#62167 = ORIENTED_EDGE ( 'NONE', *, *, #1499, .F. ) ;
#62168 = AXIS2_PLACEMENT_3D ( 'NONE', #6291, #675, #59738 ) ;
#62169 = EDGE_CURVE ( 'NONE', #49790, #29458, #20189, .T. ) ;
#62170 = CARTESIAN_POINT ( 'NONE',  ( -143.2587158300142107, 60.34092810886538416, -11.31239974830817374 ) ) ;
#62171 = CARTESIAN_POINT ( 'NONE',  ( -124.1007047332777802, 46.52282960291164216, -49.71035901984455307 ) ) ;
#62172 = CARTESIAN_POINT ( 'NONE',  ( 63.01563776193091826, -170.0000000000000000, -62.56524142263340593 ) ) ;
#62173 = CIRCLE ( 'NONE', #30708, 2.999999999999981792 ) ;
#62174 = B_SPLINE_CURVE_WITH_KNOTS ( 'NONE', 3,
 ( #52158, #11218, #27396, #3975, #64344, #32349, #58712, #46884, #10528, #53775, #37260, #43576, #21775, #69280, #16844, #48152, #21107, #42549, #27672, #64698, #10879, #62721, #64006, #32002, #59407, #53433, #14526, #32685, #48834, #5262, #681, #35985, #54747, #49463, #58983, #16767, #60388, #596, #33667, #28019, #48760, #43840, #12202, #55095, #64269, #27317, #60023, #59667, #37888, #43148, #22750, #28371, #59332, #38226, #1642, #49818, #11480, #32952, #10802, #38943, #32272, #21699, #65674, #53702, #54391, #37532 ),
 .UNSPECIFIED., .F., .F.,
 ( 4, 2, 2, 2, 2, 2, 2, 2, 2, 2, 2, 2, 2, 2, 2, 2, 2, 2, 2, 2, 2, 2, 2, 2, 2, 2, 2, 2, 2, 2, 2, 2, 4 ),
 ( 0.000000000000000000, 0.001357572341309158485, 0.002036358511963770688, 0.002715144682618383324, 0.004072717023927597754, 0.005430289365236812618, 0.006109075535891419183, 0.006787861706546025747, 0.008145434047855280510, 0.009503006389164535272, 0.01018179255981917393, 0.01086057873047381259, 0.01221815107178313153, 0.01357572341309244701, 0.01629086809571106409, 0.01900601277832967770, 0.02172115746094829478, 0.02443630214356691185, 0.02715144682618552546, 0.02986659150880414254, 0.03122416385011346496, 0.03258173619142278737, 0.03393930853273210979, 0.03529688087404143221, 0.03665445321535075462, 0.03733323938600540542, 0.03801202555666004929, 0.03869081172731469315, 0.03936959789796934395, 0.04004838406862398781, 0.04072717023927863861, 0.04208474258058787082, 0.04344231492189710303 ),
 .UNSPECIFIED. ) ;
#62175 = CARTESIAN_POINT ( 'NONE',  ( -51.00284195030131684, 13.63270405836958155, -90.07839450250217794 ) ) ;
#62176 = CARTESIAN_POINT ( 'NONE',  ( -48.20191234209509901, 13.98522789163153135, -93.32217931443403813 ) ) ;
#62177 = CYLINDRICAL_SURFACE ( 'NONE', #2298, 10.00000000000000000 ) ;
#62178 = CARTESIAN_POINT ( 'NONE',  ( -144.2029146819477887, 59.80706661873674079, 43.54475530746405809 ) ) ;
#62179 = CARTESIAN_POINT ( 'NONE',  ( 6.400000000000000355, 0.000000000000000000, 0.000000000000000000 ) ) ;
#62180 = CARTESIAN_POINT ( 'NONE',  ( -170.2801941679960294, 84.02053682015868219, -76.01052631320209230 ) ) ;
#62181 = ORIENTED_EDGE ( 'NONE', *, *, #68391, .F. ) ;
#62183 = CARTESIAN_POINT ( 'NONE',  ( -105.8683518445188412, 35.77995342500074827, 31.41595196880235008 ) ) ;
#62182 = AXIS2_PLACEMENT_3D ( 'NONE', #5379, #21543, #42990 ) ;
#62184 = ORIENTED_EDGE ( 'NONE', *, *, #13273, .F. ) ;
#62185 = CARTESIAN_POINT ( 'NONE',  ( -174.6805680479237424, 88.88026187971797754, -88.55446335397090252 ) ) ;
#62186 = CIRCLE ( 'NONE', #47559, 5.000000000000004441 ) ;
#62187 = CARTESIAN_POINT ( 'NONE',  ( 81.05403189674304087, 18.64820877954959499, 59.01636669307008276 ) ) ;
#62188 = ORIENTED_EDGE ( 'NONE', *, *, #35435, .T. ) ;
#62189 = DIRECTION ( 'NONE',  ( 0.000000000000000000, 0.000000000000000000, 1.000000000000000000 ) ) ;
#62190 = ADVANCED_FACE ( 'NONE', ( #51854, #36370, #4018, #31105, #14570, #58170 ), #57829, .T. ) ;
#62191 = PLANE ( 'NONE',  #46811 ) ;
#62192 = CARTESIAN_POINT ( 'NONE',  ( 16.00641379534997455, -64.51123194475178479, 73.58025477438755502 ) ) ;
#62193 = CARTESIAN_POINT ( 'NONE',  ( -29.70166638324878150, -57.83280658984300970, 0.000000000000000000 ) ) ;
#62194 = CARTESIAN_POINT ( 'NONE',  ( 32.90878072717891456, 7.653588083204819092, 14.33083675908082988 ) ) ;
#62195 = DIRECTION ( 'NONE',  ( -1.000000000000000000, -1.387778780781446908E-16, 0.000000000000000000 ) ) ;
#62196 = VECTOR ( 'NONE', #1463, 1000.000000000000000 ) ;
#62197 = CYLINDRICAL_SURFACE ( 'NONE', #3460, 5.000000000000004441 ) ;
#62198 = VERTEX_POINT ( 'NONE', #9644 ) ;
#62199 = DIRECTION ( 'NONE',  ( 1.000000000000000000, -0.000000000000000000, 0.000000000000000000 ) ) ;
#62200 = ORIENTED_EDGE ( 'NONE', *, *, #5234, .T. ) ;
#62201 = DIRECTION ( 'NONE',  ( -0.3930250316539278255, 0.9195277725514487965, 0.000000000000000000 ) ) ;
#62202 = CARTESIAN_POINT ( 'NONE',  ( 65.02478361689730946, 37.39438481344068776, 43.58025477438756212 ) ) ;
#62203 = DIRECTION ( 'NONE',  ( 0.000000000000000000, 0.000000000000000000, 1.000000000000000000 ) ) ;
#62204 = VERTEX_POINT ( 'NONE', #4365 ) ;
#62205 = DIRECTION ( 'NONE',  ( 0.000000000000000000, 0.000000000000000000, 1.000000000000000000 ) ) ;
#62206 = CARTESIAN_POINT ( 'NONE',  ( -14.19493007850032740, 7.389842975086044596, -73.72984886113263769 ) ) ;
#62207 = CARTESIAN_POINT ( 'NONE',  ( -34.51918258780366244, 10.11719938103012595, 30.87373719683911588 ) ) ;
#62208 = CARTESIAN_POINT ( 'NONE',  ( -24.93568128341083678, 8.613819379861709535, 68.32887008604041057 ) ) ;
#62209 = ORIENTED_EDGE ( 'NONE', *, *, #59613, .T. ) ;
#62210 = CARTESIAN_POINT ( 'NONE',  ( 0.000000000000000000, 0.000000000000000000, 0.000000000000000000 ) ) ;
#62211 = CARTESIAN_POINT ( 'NONE',  ( -152.4930836497867119, 68.09400557494207362, 58.18155450450962007 ) ) ;
#62212 = CARTESIAN_POINT ( 'NONE',  ( 99.99999999999997158, 0.000000000000000000, -46.99999999999997158 ) ) ;
#62213 = DIRECTION ( 'NONE',  ( -0.9174381082928754205, 0.3978785209734126416, 0.000000000000000000 ) ) ;
#62214 = ORIENTED_EDGE ( 'NONE', *, *, #48862, .T. ) ;
#62215 = CARTESIAN_POINT ( 'NONE',  ( -179.5186635612084558, 96.12511541314940189, -65.10392925345711035 ) ) ;
#62216 = CARTESIAN_POINT ( 'NONE',  ( 130.0051068477732485, 40.31041537049797086, 84.25595455720329596 ) ) ;
#62217 = CARTESIAN_POINT ( 'NONE',  ( 114.6890011751076202, 30.99337387307411262, 43.17062650260461254 ) ) ;
#62218 = CARTESIAN_POINT ( 'NONE',  ( 90.45368079632972069, 20.76052788962625328, -90.50765348280665989 ) ) ;
#62219 = DIRECTION ( 'NONE',  ( 1.000000000000000000, 0.000000000000000000, 0.000000000000000000 ) ) ;
#62220 = VERTEX_POINT ( 'NONE', #41310 ) ;
#62221 = CARTESIAN_POINT ( 'NONE',  ( 68.07999999999999829, -36.09918303830819752, 0.000000000000000000 ) ) ;
#62222 = LINE ( 'NONE', #41124, #19348 ) ;
#62223 = VECTOR ( 'NONE', #41272, 1000.000000000000000 ) ;
#62224 = CARTESIAN_POINT ( 'NONE',  ( 66.29961816943399810, 13.45804302849873224, 57.39740238740354528 ) ) ;
#62225 = CARTESIAN_POINT ( 'NONE',  ( -9.964117946888961797, -64.24592483216726180, 41.38025477438755928 ) ) ;
#62226 = DIRECTION ( 'NONE',  ( -0.000000000000000000, 1.000000000000000000, -0.000000000000000000 ) ) ;
#62227 = VECTOR ( 'NONE', #3549, 1000.000000000000000 ) ;
#62228 = ORIENTED_EDGE ( 'NONE', *, *, #30475, .T. ) ;
#62229 = EDGE_CURVE ( 'NONE', #19637, #2392, #46225, .T. ) ;
#62230 = VECTOR ( 'NONE', #21097, 1000.000000000000000 ) ;
#62231 = CARTESIAN_POINT ( 'NONE',  ( 164.9540180502650628, 65.02981548735056094, -16.21117244928680989 ) ) ;
#62232 = VECTOR ( 'NONE', #11342, 1000.000000000000114 ) ;
#62233 = VERTEX_POINT ( 'NONE', #67702 ) ;
#62234 = EDGE_CURVE ( 'NONE', #31627, #44487, #3089, .T. ) ;
#62235 = CARTESIAN_POINT ( 'NONE',  ( 66.73431804020509617, 14.60294556126671672, 57.63975947924529208 ) ) ;
#62236 = DIRECTION ( 'NONE',  ( 0.000000000000000000, 0.000000000000000000, -1.000000000000000000 ) ) ;
#62237 = AXIS2_PLACEMENT_3D ( 'NONE', #29108, #40346, #25568 ) ;
#62238 = VECTOR ( 'NONE', #21527, 1000.000000000000000 ) ;
#62240 = VERTEX_POINT ( 'NONE', #3666 ) ;
#62239 = LINE ( 'NONE', #14054, #10651 ) ;
#62241 = CARTESIAN_POINT ( 'NONE',  ( 164.6598737201887559, 64.78038692612517480, -45.83041859628480097 ) ) ;
#62242 = CARTESIAN_POINT ( 'NONE',  ( -4.000000000000000000, 200.0000000000000000, 0.000000000000000000 ) ) ;
#62243 = CARTESIAN_POINT ( 'NONE',  ( 164.9697211531229755, 63.72502658717166213, -43.92099099202817314 ) ) ;
#62244 = EDGE_LOOP ( 'NONE', ( #63081, #60499, #5821, #39446 ) ) ;
#62245 = DIRECTION ( 'NONE',  ( 0.000000000000000000, 0.000000000000000000, -1.000000000000000000 ) ) ;
#62246 = ADVANCED_FACE ( 'NONE', ( #9986 ), #37865, .T. ) ;
#62247 = ADVANCED_FACE ( 'NONE', ( #58494 ), #25486, .F. ) ;
#62248 = CARTESIAN_POINT ( 'NONE',  ( 437.3372781065091885, 395.0000000000066507, -136.4497041420121661 ) ) ;
#62249 = CARTESIAN_POINT ( 'NONE',  ( 157.4703587214989113, 58.92748579479259519, -89.81328548006499091 ) ) ;
#62250 = CARTESIAN_POINT ( 'NONE',  ( 81.05403189674299824, 18.64820877954959499, -21.51728507832098103 ) ) ;
#62251 = CARTESIAN_POINT ( 'NONE',  ( -173.9107726370295381, 89.52858981106767544, -88.43244303168964393 ) ) ;
#62252 = CARTESIAN_POINT ( 'NONE',  ( 150.4550062612853480, 52.39582885725847916, 66.45880062188886939 ) ) ;
#62253 = CARTESIAN_POINT ( 'NONE',  ( 93.72059824125564376, 23.03897520779757713, 39.70469307016926308 ) ) ;
#62255 = ORIENTED_EDGE ( 'NONE', *, *, #48121, .F. ) ;
#62254 = ADVANCED_FACE ( 'NONE', ( #52872 ), #10316, .T. ) ;
#62256 = CARTESIAN_POINT ( 'NONE',  ( -96.76336539645312484, 31.18045094643429493, 59.75870862236858017 ) ) ;
#62257 = CARTESIAN_POINT ( 'NONE',  ( -11.79249160485394299, 8.191429102467033374, 70.82980661725612492 ) ) ;
#62258 = VERTEX_POINT ( 'NONE', #25139 ) ;
#62259 = EDGE_CURVE ( 'NONE', #37698, #34548, #31357, .T. ) ;
#62260 = CARTESIAN_POINT ( 'NONE',  ( 150.9128604434957595, 53.97103482421773180, -20.45779706337464887 ) ) ;
#62261 = CARTESIAN_POINT ( 'NONE',  ( 21.27121078971695312, -61.42097029141944375, 40.00000000000003553 ) ) ;
#62262 = CARTESIAN_POINT ( 'NONE',  ( 109.3154830994003390, 29.56170298203815605, 29.65404401712086013 ) ) ;
#62263 = CARTESIAN_POINT ( 'NONE',  ( -1.096061481932295356, 7.553048580900439291, 34.29492952217174206 ) ) ;
#62264 = CARTESIAN_POINT ( 'NONE',  ( 6.000000000000000000, 23.07878402833891229, 9.999999999999998224 ) ) ;
#62265 = CYLINDRICAL_SURFACE ( 'NONE', #25812, 2.999999999999999112 ) ;
#62266 = CARTESIAN_POINT ( 'NONE',  ( 210.1954643503416094, 114.1986276268024056, -38.71856909762487930 ) ) ;
#62267 = CARTESIAN_POINT ( 'NONE',  ( 177.7889574972181777, 75.33777460203559428, 3.211639890609760517 ) ) ;
#62268 = CARTESIAN_POINT ( 'NONE',  ( -55.54058841405665703, 14.81234591756537355, 18.47277718246749956 ) ) ;
#62269 = VERTEX_POINT ( 'NONE', #32818 ) ;
#62270 = VECTOR ( 'NONE', #24200, 1000.000000000000000 ) ;
#62271 = DIRECTION ( 'NONE',  ( -1.020422603260505347E-14, 1.000000000000000000, 5.551115123125782702E-17 ) ) ;
#62272 = ORIENTED_EDGE ( 'NONE', *, *, #10483, .T. ) ;
#62273 = CARTESIAN_POINT ( 'NONE',  ( 104.3931729003987101, 26.26823401847089201, -65.54728805928756685 ) ) ;
#62274 = ADVANCED_FACE ( 'NONE', ( #54247 ), #32127, .F. ) ;
#62275 = CARTESIAN_POINT ( 'NONE',  ( 46.89016064832838993, 10.52130577388959054, -16.76345691462488929 ) ) ;
#62276 = CARTESIAN_POINT ( 'NONE',  ( 44.86216938219161676, 9.182565662897493652, 59.11098717133123870 ) ) ;
#62277 = CARTESIAN_POINT ( 'NONE',  ( 0.000000000000000000, 70.00000000000000000, 0.000000000000000000 ) ) ;
#62278 = CARTESIAN_POINT ( 'NONE',  ( -10.07658142808628199, 7.047931155041471385, 84.14318101103907566 ) ) ;
#62279 = EDGE_CURVE ( 'NONE', #56653, #15171, #8665, .T. ) ;
#62280 = EDGE_CURVE ( 'NONE', #12765, #14559, #49020, .T. ) ;
#62281 = EDGE_CURVE ( 'NONE', #38976, #50879, #19327, .T. ) ;
#62282 = CARTESIAN_POINT ( 'NONE',  ( -109.7811201291769834, 37.90784085457606523, -15.43969849781013259 ) ) ;
#62283 = AXIS2_PLACEMENT_3D ( 'NONE', #24844, #36783, #9349 ) ;
#62284 = ORIENTED_EDGE ( 'NONE', *, *, #40527, .T. ) ;
#62285 = CARTESIAN_POINT ( 'NONE',  ( 55.97663400285460256, 12.17578876026178669, -94.18817934799618286 ) ) ;
#62286 = DIRECTION ( 'NONE',  ( 0.000000000000000000, 1.000000000000000000, 0.000000000000000000 ) ) ;
#62287 = ORIENTED_EDGE ( 'NONE', *, *, #62829, .F. ) ;
#62288 = CIRCLE ( 'NONE', #57767, 97.99999999999994316 ) ;
#62289 = ORIENTED_EDGE ( 'NONE', *, *, #11725, .F. ) ;
#62290 = VECTOR ( 'NONE', #56179, 1000.000000000000000 ) ;
#62291 = CARTESIAN_POINT ( 'NONE',  ( -156.0300823189602681, 69.91528270335483342, 34.48016162486435832 ) ) ;
#62292 = LINE ( 'NONE', #8489, #8613 ) ;
#62293 = CARTESIAN_POINT ( 'NONE',  ( 173.6020601204682237, 71.36108012062133810, -16.28340663019495338 ) ) ;
#62294 = CARTESIAN_POINT ( 'NONE',  ( -172.7173255566596879, 88.18461381371093921, 57.66624519710471475 ) ) ;
#62295 = VECTOR ( 'NONE', #19152, 1000.000000000000000 ) ;
#62296 = CARTESIAN_POINT ( 'NONE',  ( -447.6627218934913230, 1.665334536937734811E-13, 103.5502958579881749 ) ) ;
#62297 = CARTESIAN_POINT ( 'NONE',  ( 56.94505604581134861, 12.37336791557970805, -20.78740111288298564 ) ) ;
#62298 = ORIENTED_EDGE ( 'NONE', *, *, #10248, .T. ) ;
#62299 = CARTESIAN_POINT ( 'NONE',  ( 45.78444578632068840, -59.41672343742509810, 170.0000000000000000 ) ) ;
#62300 = ORIENTED_EDGE ( 'NONE', *, *, #15982, .F. ) ;
#62301 = CARTESIAN_POINT ( 'NONE',  ( 208.9507214515059559, 112.3605999017435124, 3.669543826566413980 ) ) ;
#62302 = CARTESIAN_POINT ( 'NONE',  ( -142.5087559769085033, 59.74468185400777998, 40.96956311530343697 ) ) ;
#62303 = DIRECTION ( 'NONE',  ( 1.000000000000000000, 0.000000000000000000, -5.551115123125593376E-15 ) ) ;
#62304 = FACE_BOUND ( 'NONE', #59912, .T. ) ;
#62305 = ORIENTED_EDGE ( 'NONE', *, *, #1652, .T. ) ;
#62306 = ORIENTED_EDGE ( 'NONE', *, *, #11245, .T. ) ;
#62307 = DIRECTION ( 'NONE',  ( 0.000000000000000000, 4.930380657631322689E-32, 1.000000000000000000 ) ) ;
#62308 = CARTESIAN_POINT ( 'NONE',  ( -118.4647292297932495, 42.97137042695754161, 90.72527677266357671 ) ) ;
#62309 = CARTESIAN_POINT ( 'NONE',  ( 33.77444274891860942, 8.756048688386677270, -74.92843515396829446 ) ) ;
#62310 = CARTESIAN_POINT ( 'NONE',  ( -179.2210908201800237, 95.76260491022608790, 15.86921790254495335 ) ) ;
#62311 = CARTESIAN_POINT ( 'NONE',  ( 205.5049354810107047, 109.1776577097391652, 56.05227132923312894 ) ) ;
#62312 = CARTESIAN_POINT ( 'NONE',  ( 79.52861599156693728, 17.11914630560287875, -72.63190030141871034 ) ) ;
#62313 = VERTEX_POINT ( 'NONE', #40778 ) ;
#62314 = CARTESIAN_POINT ( 'NONE',  ( 8.828807734115066808, -74.48902371486708773, 43.58025477438756212 ) ) ;
#62315 = CARTESIAN_POINT ( 'NONE',  ( 198.2588776805010298, 99.52972231602373654, -47.68225496974167754 ) ) ;
#62316 = ORIENTED_EDGE ( 'NONE', *, *, #64138, .F. ) ;
#62317 = CARTESIAN_POINT ( 'NONE',  ( -86.09999398724995956, 25.29376521564874380, 12.10207219235686793 ) ) ;
#62318 = VERTEX_POINT ( 'NONE', #45369 ) ;
#62319 = EDGE_CURVE ( 'NONE', #52558, #57335, #61480, .T. ) ;
#62320 = VECTOR ( 'NONE', #1346, 1000.000000000000000 ) ;
#62321 = CARTESIAN_POINT ( 'NONE',  ( -86.09999398724994535, 25.29376521564874025, -68.43157957903414967 ) ) ;
#62322 = FACE_OUTER_BOUND ( 'NONE', #60717, .T. ) ;
#62323 = ORIENTED_EDGE ( 'NONE', *, *, #10386, .T. ) ;
#62324 = VECTOR ( 'NONE', #65891, 1000.000000000000000 ) ;
#62325 = ORIENTED_EDGE ( 'NONE', *, *, #50276, .T. ) ;
#62326 = CARTESIAN_POINT ( 'NONE',  ( 15.78827728214693416, 6.500811158483327468, -35.51894409868578606 ) ) ;
#62327 = CARTESIAN_POINT ( 'NONE',  ( 46.39999999999999858, 0.000000000000000000, 0.000000000000000000 ) ) ;
#62328 = CARTESIAN_POINT ( 'NONE',  ( 103.1534365798308812, 26.83148826706847601, 12.76670356914313942 ) ) ;
#62329 = VECTOR ( 'NONE', #60965, 1000.000000000000000 ) ;
#62330 = VECTOR ( 'NONE', #42729, 1000.000000000000227 ) ;
#62331 = VERTEX_POINT ( 'NONE', #51352 ) ;
#62332 = VECTOR ( 'NONE', #40397, 1000.000000000000000 ) ;
#62333 = EDGE_CURVE ( 'NONE', #3736, #25681, #2465, .T. ) ;
#62334 = EDGE_CURVE ( 'NONE', #46955, #20867, #61551, .T. ) ;
#62335 = CIRCLE ( 'NONE', #58951, 5.000000000000004441 ) ;
#62336 = EDGE_CURVE ( 'NONE', #26503, #9081, #35159, .T. ) ;
#62337 = CARTESIAN_POINT ( 'NONE',  ( -26.19968929187003326, 8.789572452951027515, 86.01030072649960800 ) ) ;
#62338 = CARTESIAN_POINT ( 'NONE',  ( -52.00092620775819796, 14.92276858858357258, 4.117465040003481569 ) ) ;
#62339 = CIRCLE ( 'NONE', #49984, 89.99999999999998579 ) ;
#62340 = DIRECTION ( 'NONE',  ( 0.000000000000000000, 0.000000000000000000, 1.000000000000000000 ) ) ;
#62341 = CYLINDRICAL_SURFACE ( 'NONE', #28233, 245.3095347406802205 ) ;
#62342 = ADVANCED_FACE ( 'NONE', ( #8438 ), #35512, .F. ) ;
#62343 = CARTESIAN_POINT ( 'NONE',  ( 86.62931800182293784, 20.48449268398423584, -35.82156419891171595 ) ) ;
#62344 = CARTESIAN_POINT ( 'NONE',  ( -172.3565569771572257, 87.77934603007950898, -88.40105834567737020 ) ) ;
#62345 = VERTEX_POINT ( 'NONE', #55931 ) ;
#62346 = EDGE_CURVE ( 'NONE', #58885, #19257, #45766, .T. ) ;
#62347 = EDGE_LOOP ( 'NONE', ( #48919, #32996, #27712, #44845 ) ) ;
#62348 = CARTESIAN_POINT ( 'NONE',  ( 46.50704915687943242, 9.440294391580041022, 12.98352632930303407 ) ) ;
#62349 = LINE ( 'NONE', #26445, #50648 ) ;
#62350 = CARTESIAN_POINT ( 'NONE',  ( 3.000000000000030198, 6.000000000000000000, -1.665334536937751377E-15 ) ) ;
#62351 = PLANE ( 'NONE',  #36665 ) ;
#62352 = CARTESIAN_POINT ( 'NONE',  ( 129.1381264900934696, 38.64720302602603397, 16.01571092030106414 ) ) ;
#62353 = CARTESIAN_POINT ( 'NONE',  ( 38.57272366894952853, 8.302820907903958769, -89.34357163266685120 ) ) ;
#62354 = CARTESIAN_POINT ( 'NONE',  ( 201.5359545986093508, 103.7719700437703949, 83.58986283284697549 ) ) ;
#62355 = LINE ( 'NONE', #37332, #44460 ) ;
#62356 = CARTESIAN_POINT ( 'NONE',  ( 31.11269837220812562, 36.11269837220800838, 85.00100000000000477 ) ) ;
#62357 = CARTESIAN_POINT ( 'NONE',  ( -106.6940984894958149, 35.07986071359380986, 31.93677410839523034 ) ) ;
#62358 = EDGE_LOOP ( 'NONE', ( #46067, #12647, #59618, #46232 ) ) ;
#62359 = CARTESIAN_POINT ( 'NONE',  ( 12.47451846520756646, 7.423604437114562415, -22.90708336615600160 ) ) ;
#62360 = ORIENTED_EDGE ( 'NONE', *, *, #11347, .T. ) ;
#62361 = CARTESIAN_POINT ( 'NONE',  ( 203.9181091394787018, 105.2759068139671115, -9.481380442157897548 ) ) ;
#62362 = ORIENTED_EDGE ( 'NONE', *, *, #43724, .T. ) ;
#62363 = DIRECTION ( 'NONE',  ( -0.7071067811865474617, 0.000000000000000000, -0.7071067811865474617 ) ) ;
#62364 = CARTESIAN_POINT ( 'NONE',  ( 187.6511924654682559, 87.00187850361888309, -74.20232582961776302 ) ) ;
#62365 = CARTESIAN_POINT ( 'NONE',  ( -144.2155061717025717, 61.10843690942978412, 70.38575101539866807 ) ) ;
#62366 = DIRECTION ( 'NONE',  ( -0.000000000000000000, 1.000000000000000000, -0.000000000000000000 ) ) ;
#62367 = EDGE_CURVE ( 'NONE', #59387, #17233, #46856, .T. ) ;
#62368 = EDGE_CURVE ( 'NONE', #31528, #43301, #33097, .T. ) ;
#62369 = CARTESIAN_POINT ( 'NONE',  ( 36.09137906183516264, 8.001963043161762101, -49.85409025298285712 ) ) ;
#62370 = B_SPLINE_CURVE_WITH_KNOTS ( 'NONE', 3,
 ( #45916, #13224, #8290, #13563, #18839, #39945, #7244, #24123, #40294, #45218, #23436, #18490, #29058, #29736, #1978, #50500, #51200, #61399, #28704, #56463, #45565, #34686, #40982, #3013, #44875, #24477, #67385, #19174, #40627, #66358, #12878, #62085, #3353, #56121, #18146, #13902, #39601, #24813, #35365, #23771, #50152, #56827, #7938, #61051 ),
 .UNSPECIFIED., .F., .F.,
 ( 4, 2, 2, 2, 2, 2, 2, 2, 2, 2, 2, 2, 2, 2, 2, 2, 2, 2, 2, 2, 2, 4 ),
 ( 0.02908143158676660192, 0.03095422299093867138, 0.03282701439511073738, 0.03469980579928280684, 0.03657259720345487630, 0.03844538860762694577, 0.04031818001179900829, 0.04125457571388502914, 0.04219097141597105693, 0.04312736711805707779, 0.04359556496910008128, 0.04406376282014309864, 0.04500015852222911256, 0.04593655422431514035, 0.04687294992640116120, 0.04780934562848718206, 0.04968213703265925846, 0.05155492843683133486, 0.05342771984100341126, 0.05530051124517548766, 0.05717330264934757100, 0.05904609405351964740 ),
 .UNSPECIFIED. ) ;
#62371 = CYLINDRICAL_SURFACE ( 'NONE', #16929, 299.9999999999999432 ) ;
#62372 = CARTESIAN_POINT ( 'NONE',  ( 15.78827728214693416, 7.507518794609576496, -35.51894409868578606 ) ) ;
#62373 = EDGE_CURVE ( 'NONE', #43813, #54143, #53048, .T. ) ;
#62374 = CARTESIAN_POINT ( 'NONE',  ( 132.0440382699655117, 40.34028297386451811, -50.81529750769279730 ) ) ;
#62375 = ORIENTED_EDGE ( 'NONE', *, *, #64818, .F. ) ;
#62376 = EDGE_LOOP ( 'NONE', ( #40899, #26632, #4433, #34017 ) ) ;
#62377 = AXIS2_PLACEMENT_3D ( 'NONE', #22186, #47871, #5646 ) ;
#62378 = CARTESIAN_POINT ( 'NONE',  ( 10.55634918610397577, -26.11269837220809364, 2.000000000000001776 ) ) ;
#62379 = DIRECTION ( 'NONE',  ( 1.000000000000000000, 0.000000000000000000, 0.000000000000000000 ) ) ;
#62380 = CARTESIAN_POINT ( 'NONE',  ( -24.41864932425148282, 8.543938959778817122, -67.01132967089127135 ) ) ;
#62381 = AXIS2_PLACEMENT_3D ( 'NONE', #49966, #16567, #64410 ) ;
#62382 = CARTESIAN_POINT ( 'NONE',  ( 8.336882341125875229, 6.376438415325264231, 9.686664293182547070 ) ) ;
#62383 = CARTESIAN_POINT ( 'NONE',  ( 40.38495044702530379, 9.554194848483440694, -77.41568337247169040 ) ) ;
#62384 = AXIS2_PLACEMENT_3D ( 'NONE', #13754, #13076, #67575 ) ;
#62385 = AXIS2_PLACEMENT_3D ( 'NONE', #19569, #10049, #3732 ) ;
#62386 = CARTESIAN_POINT ( 'NONE',  ( 111.9975424824652634, 0.000000000000000000, 256.6193948016162381 ) ) ;
#62387 = PLANE ( 'NONE',  #31548 ) ;
#62388 = CARTESIAN_POINT ( 'NONE',  ( -180.6009936245623066, 95.85948119829087943, -41.58058426359100679 ) ) ;
#62389 = DIRECTION ( 'NONE',  ( -0.8660254037844378194, 0.5000000000000013323, 0.000000000000000000 ) ) ;
#62390 = CARTESIAN_POINT ( 'NONE',  ( -169.1005390226458758, 82.76152663947081578, 17.82399784940768228 ) ) ;
#62391 = CARTESIAN_POINT ( 'NONE',  ( -55.05276343752910151, -170.0000000000000000, -96.40542517938723677 ) ) ;
#62392 = CARTESIAN_POINT ( 'NONE',  ( -47.56463531432803649, 12.80077789972090052, 65.15204238671329051 ) ) ;
#62393 = AXIS2_PLACEMENT_3D ( 'NONE', #58771, #37669, #32057 ) ;
#62394 = APPLICATION_CONTEXT ( 'automotive_design' ) ;
#62395 = CARTESIAN_POINT ( 'NONE',  ( -6.851003965218991354, 6.829052369041588300, 57.00742815665407903 ) ) ;
#62396 = ORIENTED_EDGE ( 'NONE', *, *, #16335, .F. ) ;
#62397 = CARTESIAN_POINT ( 'NONE',  ( 141.9165763529819344, -2.000000000000001776, 129.0000000000000000 ) ) ;
#62398 = CARTESIAN_POINT ( 'NONE',  ( 150.9128604434957595, 53.97103482421773180, 60.07585470801640781 ) ) ;
#62399 = CARTESIAN_POINT ( 'NONE',  ( -105.8879245385188597, 35.79035667534149923, -62.76632112264718444 ) ) ;
#62400 = CARTESIAN_POINT ( 'NONE',  ( -51.35181696773307181, 13.72007042346227657, -49.25810110310893464 ) ) ;
#62401 = CARTESIAN_POINT ( 'NONE',  ( 311.9975424824652350, 172.0000000000000000, 529.9060149868649887 ) ) ;
#62402 = DIRECTION ( 'NONE',  ( 0.000000000000000000, 0.000000000000000000, 1.000000000000000000 ) ) ;
#62403 = EDGE_LOOP ( 'NONE', ( #21299, #39338, #61665, #22797 ) ) ;
#62404 = DIRECTION ( 'NONE',  ( -1.850371928290090422E-16, 1.000000000000000000, 1.110223024625156171E-16 ) ) ;
#62405 = FACE_OUTER_BOUND ( 'NONE', #48129, .T. ) ;
#62406 = ORIENTED_EDGE ( 'NONE', *, *, #68835, .F. ) ;
#62407 = ORIENTED_EDGE ( 'NONE', *, *, #22852, .T. ) ;
#62408 = EDGE_CURVE ( 'NONE', #7321, #62016, #25999, .T. ) ;
#62409 = FACE_BOUND ( 'NONE', #14726, .T. ) ;
#62410 = DIRECTION ( 'NONE',  ( -0.000000000000000000, 1.000000000000000000, -0.000000000000000000 ) ) ;
#62411 = CARTESIAN_POINT ( 'NONE',  ( 427.4999999999999432, -17.50000000000000000, 0.000000000000000000 ) ) ;
#62412 = B_SPLINE_CURVE_WITH_KNOTS ( 'NONE', 3,
 ( #48482, #65044, #317, #43218, #58371, #10184, #64003, #31646, #4913, #69278, #10526, #31999, #53431, #26721, #48150, #28852, #6997, #11922, #28094, #44269, #61161, #39357, #38658, #2421, #33395, #65397, #54824, #12982, #44974, #55525, #1370, #13328, #39017, #7705, #12626, #44632, #29151, #49539, #7356, #34785, #60462, #50601, #28811, #1725, #23876, #22828 ),
 .UNSPECIFIED., .F., .F.,
 ( 4, 2, 2, 2, 2, 2, 2, 2, 2, 2, 2, 2, 2, 2, 2, 2, 2, 2, 2, 2, 2, 2, 4 ),
 ( 6.938893903907228378E-18, 0.003192770216278338277, 0.003990962770347912004, 0.004789155324417485732, 0.006385540432556642727, 0.007183732986626235537, 0.007981925540695827478, 0.009578310648835042587, 0.01037650320290463973, 0.01117469575697423514, 0.01197288831104383056, 0.01277108086511342597, 0.01436746597325257689, 0.01596385108139172782, 0.01676204363546130241, 0.01756023618953087700, 0.01835842874360045160, 0.01915662129767002619, 0.02075300640580919273, 0.02234939151394836274, 0.02394577662208753274, 0.02474396917615711428, 0.02554216173022670275 ),
 .UNSPECIFIED. ) ;
#62413 = PRESENTATION_LAYER_ASSIGNMENT (  '', '', ( #13521 ) ) ;
#62414 = ORIENTED_EDGE ( 'NONE', *, *, #31005, .F. ) ;
#62415 = CARTESIAN_POINT ( 'NONE',  ( -125.8938041572051389, -170.0000000000000000, 18.77539728269342945 ) ) ;
#62416 = CARTESIAN_POINT ( 'NONE',  ( 0.000000000000000000, 0.000000000000000000, 0.000000000000000000 ) ) ;
#62417 = DIRECTION ( 'NONE',  ( -0.000000000000000000, 0.000000000000000000, 1.000000000000000000 ) ) ;
#62418 = DIRECTION ( 'NONE',  ( -0.000000000000000000, -0.000000000000000000, -1.000000000000000000 ) ) ;
#62419 = CARTESIAN_POINT ( 'NONE',  ( -82.33596576276352152, 24.83688096733769513, 44.47724042997496952 ) ) ;
#62420 = CARTESIAN_POINT ( 'NONE',  ( 150.6448088972535402, 52.53284510403385354, 93.79555634108432116 ) ) ;
#62421 = LINE ( 'NONE', #67366, #25302 ) ;
#62422 = EDGE_CURVE ( 'NONE', #32318, #5211, #41458, .T. ) ;
#62423 = ORIENTED_EDGE ( 'NONE', *, *, #43014, .F. ) ;
#62424 = CARTESIAN_POINT ( 'NONE',  ( 117.0065308422768453, 32.13872219870569324, -46.67330633784816740 ) ) ;
#62425 = AXIS2_PLACEMENT_3D ( 'NONE', #45559, #13559, #13898 ) ;
#62426 = DIRECTION ( 'NONE',  ( -0.000000000000000000, -0.000000000000000000, 1.000000000000000000 ) ) ;
#62427 = EDGE_CURVE ( 'NONE', #66426, #47377, #4189, .T. ) ;
#62428 = CARTESIAN_POINT ( 'NONE',  ( 44.86216938219162387, 9.182565662897474112, -48.26721519052350828 ) ) ;
#62429 = EDGE_CURVE ( 'NONE', #62781, #43813, #6254, .T. ) ;
#62430 = CARTESIAN_POINT ( 'NONE',  ( 57.25833571151868284, 48.36523237396223607, 41.38025477438755928 ) ) ;
#62432 = EDGE_LOOP ( 'NONE', ( #40905, #27758, #68750, #14273 ) ) ;
#62431 = FACE_OUTER_BOUND ( 'NONE', #5243, .T. ) ;
#62433 = CARTESIAN_POINT ( 'NONE',  ( 68.94309019697860208, 15.16533147648755175, 41.93448570448100554 ) ) ;
#62434 = ORIENTED_EDGE ( 'NONE', *, *, #10466, .T. ) ;
#62435 = AXIS2_PLACEMENT_3D ( 'NONE', #40323, #11847, #12555 ) ;
#62436 = VERTEX_POINT ( 'NONE', #49151 ) ;
#62437 = CARTESIAN_POINT ( 'NONE',  ( 15.55634918610406103, 20.55634918610400064, 85.00100000000000477 ) ) ;
#62438 = DIRECTION ( 'NONE',  ( 1.000000000000000000, 0.000000000000000000, 0.000000000000000000 ) ) ;
#62439 = CARTESIAN_POINT ( 'NONE',  ( 15.55634918610396511, -46.66904755831214402, 2.000000000000001776 ) ) ;
#62440 = AXIS2_PLACEMENT_3D ( 'NONE', #63603, #57289, #15065 ) ;
#62441 = CARTESIAN_POINT ( 'NONE',  ( -46.66904755831210139, 5.000000000000066613, 85.00100000000000477 ) ) ;
#62442 = LINE ( 'NONE', #19172, #44405 ) ;
#62443 = FACE_BOUND ( 'NONE', #55186, .T. ) ;
#62444 = DIRECTION ( 'NONE',  ( 0.9639628606958550172, -0.2660368455666687892, 0.000000000000000000 ) ) ;
#62445 = AXIS2_PLACEMENT_3D ( 'NONE', #20740, #37820, #21421 ) ;
#62446 = CARTESIAN_POINT ( 'NONE',  ( -55.05276343752909440, 15.72344139423348430, 30.31732777293113301 ) ) ;
#62447 = ORIENTED_EDGE ( 'NONE', *, *, #7463, .T. ) ;
#62448 = EDGE_LOOP ( 'NONE', ( #29281, #33231 ) ) ;
#62449 = CARTESIAN_POINT ( 'NONE',  ( -109.7790042512817621, 37.90666514836943435, 10.88333844894347457 ) ) ;
#62450 = CARTESIAN_POINT ( 'NONE',  ( 106.4107271020440209, 27.14892220304138704, 57.50428525336668173 ) ) ;
#62451 = CARTESIAN_POINT ( 'NONE',  ( 164.4728833318992542, 63.30716077995683833, 66.45373925860369013 ) ) ;
#62452 = FACE_OUTER_BOUND ( 'NONE', #41033, .T. ) ;
#62453 = DIRECTION ( 'NONE',  ( 0.7071067811865477948, -9.875400524329059797E-15, 0.7071067811865473507 ) ) ;
#62454 = CARTESIAN_POINT ( 'NONE',  ( 16.76400266940279593, 6.533513613209220416, 30.06214509688793157 ) ) ;
#62455 = EDGE_CURVE ( 'NONE', #28945, #37023, #35599, .T. ) ;
#62456 = CARTESIAN_POINT ( 'NONE',  ( 11.30618213853492904, -74.15344055032291237, 43.58025477438756923 ) ) ;
#62457 = ORIENTED_EDGE ( 'NONE', *, *, #66565, .T. ) ;
#62458 = ORIENTED_EDGE ( 'NONE', *, *, #6969, .T. ) ;
#62459 = ORIENTED_EDGE ( 'NONE', *, *, #54510, .F. ) ;
#62460 = CARTESIAN_POINT ( 'NONE',  ( 0.000000000000000000, 0.000000000000000000, 41.38025477438755928 ) ) ;
#62461 = CARTESIAN_POINT ( 'NONE',  ( 175.8197560646975717, 73.44385669436823605, -92.05716592950678034 ) ) ;
#62462 = DIRECTION ( 'NONE',  ( 0.000000000000000000, 0.000000000000000000, 1.000000000000000000 ) ) ;
#62463 = CARTESIAN_POINT ( 'NONE',  ( -4.999999999999922728, 46.66904755831208718, 85.00100000000000477 ) ) ;
#62464 = LINE ( 'NONE', #56143, #62630 ) ;
#62465 = CARTESIAN_POINT ( 'NONE',  ( -37.39246151129641049, 11.66872370876246201, -65.07389322207556859 ) ) ;
#62466 = CARTESIAN_POINT ( 'NONE',  ( 187.2384682876462421, 86.54721710842893856, 67.96900511035511272 ) ) ;
#62467 = CARTESIAN_POINT ( 'NONE',  ( 12.03317402819681803, 6.409531826169462931, -22.67129521315044727 ) ) ;
#62468 =( NAMED_UNIT ( * ) SI_UNIT ( $, .STERADIAN. ) SOLID_ANGLE_UNIT ( ) );
#62469 = EDGE_LOOP ( 'NONE', ( #60883, #5899, #50119, #7040 ) ) ;
#62470 = CARTESIAN_POINT ( 'NONE',  ( -1.083610669212422550, 6.545642299653468221, -39.59529283513472819 ) ) ;
#62471 = CARTESIAN_POINT ( 'NONE',  ( 65.02478361689784947, -37.39438481343977116, 43.58025477438756923 ) ) ;
#62472 = CARTESIAN_POINT ( 'NONE',  ( 4.339467034331195627, 6.732211846623388674, 5.929018872543287221E-15 ) ) ;
#62473 = FACE_OUTER_BOUND ( 'NONE', #53477, .T. ) ;
#62474 = CARTESIAN_POINT ( 'NONE',  ( 127.2202105166096686, 37.55913282978156786, -20.18205885347246920 ) ) ;
#62475 = DIRECTION ( 'NONE',  ( -0.000000000000000000, 0.000000000000000000, -1.000000000000000000 ) ) ;
#62476 = CARTESIAN_POINT ( 'NONE',  ( 10.15118267943872254, 7.391905976536035539, 5.716968369951990425 ) ) ;
#62477 = AXIS2_PLACEMENT_3D ( 'NONE', #61992, #3604, #25072 ) ;
#62478 = EDGE_LOOP ( 'NONE', ( #12294, #64356, #62209 ) ) ;
#62479 = VECTOR ( 'NONE', #58979, 1000.000000000000000 ) ;
#62480 = APPLICATION_PROTOCOL_DEFINITION ( 'draft international standard', 'automotive_design', 1998, #8476 ) ;
#62481 = CARTESIAN_POINT ( 'NONE',  ( 126.6266894765173703, 38.37986986668738609, -41.46026502974351047 ) ) ;
#62482 = DIRECTION ( 'NONE',  ( -3.330669073875466466E-14, 0.000000000000000000, -1.000000000000000000 ) ) ;
#62483 = LINE ( 'NONE', #50544, #66063 ) ;
#62484 = ITEM_DEFINED_TRANSFORMATION ( 'NONE', 'NONE', #54586,  #66832 ) ;
#62485 = DIRECTION ( 'NONE',  ( -0.000000000000000000, -0.000000000000000000, -1.000000000000000000 ) ) ;
#62486 = ORIENTED_EDGE ( 'NONE', *, *, #57328, .F. ) ;
#62487 = VECTOR ( 'NONE', #65604, 1000.000000000000000 ) ;
#62488 = AXIS2_PLACEMENT_3D ( 'NONE', #20520, #46220, #67698 ) ;
#62489 = EDGE_CURVE ( 'NONE', #47113, #51654, #313, .T. ) ;
#62490 = PRODUCT_DEFINITION_FORMATION_WITH_SPECIFIED_SOURCE ( 'ANY', '', #28232, .NOT_KNOWN. ) ;
#62491 = ORIENTED_EDGE ( 'NONE', *, *, #54298, .F. ) ;
#62492 = ADVANCED_FACE ( 'NONE', ( #66421 ), #24195, .F. ) ;
#62493 = CARTESIAN_POINT ( 'NONE',  ( -146.7345109736526467, 61.86270848728295846, -8.496187606269963055 ) ) ;
#62494 = CONICAL_SURFACE ( 'NONE', #23128, 185.0000000000000000, 1.279339532317029793 ) ;
#62495 = EDGE_CURVE ( 'NONE', #51047, #18819, #22123, .T. ) ;
#62496 = FACE_OUTER_BOUND ( 'NONE', #43135, .T. ) ;
#62497 = ORIENTED_EDGE ( 'NONE', *, *, #814, .T. ) ;
#62498 = AXIS2_PLACEMENT_3D ( 'NONE', #2854, #25494, #43579 ) ;
#62499 = EDGE_CURVE ( 'NONE', #25496, #12560, #68144, .T. ) ;
#62500 = CARTESIAN_POINT ( 'NONE',  ( 159.6439063569485199, 60.64869340040664980, 83.41414359430092418 ) ) ;
#62501 = EDGE_LOOP ( 'NONE', ( #51443, #2245, #53447, #11716 ) ) ;
#62502 = CARTESIAN_POINT ( 'NONE',  ( 132.2818448028689033, 41.65267246304673421, -77.70421314065404772 ) ) ;
#62503 = CARTESIAN_POINT ( 'NONE',  ( 390.9212159716611836, 2.000000000000001776, 0.000000000000000000 ) ) ;
#62504 = ADVANCED_FACE ( 'NONE', ( #41405 ), #36463, .F. ) ;
#62505 = FACE_BOUND ( 'NONE', #9586, .T. ) ;
#62506 = CARTESIAN_POINT ( 'NONE',  ( 0.000000000000000000, 0.000000000000000000, 0.000000000000000000 ) ) ;
#62507 = CARTESIAN_POINT ( 'NONE',  ( 0.000000000000000000, 0.000000000000000000, 5.000000000000000000 ) ) ;
#62509 = EDGE_LOOP ( 'NONE', ( #22626, #59642, #41637, #7038 ) ) ;
#62508 = CARTESIAN_POINT ( 'NONE',  ( 0.000000000000000000, 0.000000000000000000, 0.000000000000000000 ) ) ;
#62510 = CARTESIAN_POINT ( 'NONE',  ( -2.368959188627906887, 24.88750755625416744, 0.000000000000000000 ) ) ;
#62511 = ORIENTED_EDGE ( 'NONE', *, *, #2568, .T. ) ;
#62512 = ORIENTED_EDGE ( 'NONE', *, *, #133, .F. ) ;
#62513 = CARTESIAN_POINT ( 'NONE',  ( 173.6007744016332310, 72.73482010729016167, 37.39045840423305833 ) ) ;
#62514 = EDGE_CURVE ( 'NONE', #8866, #3372, #26377, .T. ) ;
#62515 = CARTESIAN_POINT ( 'NONE',  ( 16.76400266940279238, 6.533513613209218640, -77.31605726496678699 ) ) ;
#62516 = ADVANCED_FACE ( 'NONE', ( #1248 ), #34534, .F. ) ;
#62518 = ORIENTED_EDGE ( 'NONE', *, *, #49397, .F. ) ;
#62517 = CARTESIAN_POINT ( 'NONE',  ( -128.1267916618074594, 49.19573276651586724, 72.13916297000683642 ) ) ;
#62519 = CARTESIAN_POINT ( 'NONE',  ( 59.73312635112155533, 12.96464920523511211, 3.707537953021396326 ) ) ;
#62520 = DIRECTION ( 'NONE',  ( 0.000000000000000000, 0.000000000000000000, 1.000000000000000000 ) ) ;
#62521 = ORIENTED_EDGE ( 'NONE', *, *, #14075, .T. ) ;
#62522 = CARTESIAN_POINT ( 'NONE',  ( -61.38706483483510823, 16.47181058798476272, -11.84841205307662371 ) ) ;
#62523 = AXIS2_PLACEMENT_3D ( 'NONE', #64954, #16750, #17088 ) ;
#62524 = CARTESIAN_POINT ( 'NONE',  ( 141.3556389957210513, 47.34429831367557284, 37.30624493767670913 ) ) ;
#62525 = CARTESIAN_POINT ( 'NONE',  ( 110.2429982417149574, 29.99119854320846201, 29.61121420573730489 ) ) ;
#62526 = CARTESIAN_POINT ( 'NONE',  ( 200.0000000000000000, 0.000000000000000000, 7.000000000000000000 ) ) ;
#62527 = CARTESIAN_POINT ( 'NONE',  ( -100.4466073551323149, 31.85873123265079698, -76.64638814016929302 ) ) ;
#62528 = VERTEX_POINT ( 'NONE', #27626 ) ;
#62529 = EDGE_LOOP ( 'NONE', ( #464, #52616, #38159, #6518 ) ) ;
#62530 = VECTOR ( 'NONE', #29759, 1000.000000000000000 ) ;
#62531 = CARTESIAN_POINT ( 'NONE',  ( -142.0860844253783171, 59.41107357617634932, -16.58767256066205675 ) ) ;
#62532 = DIRECTION ( 'NONE',  ( -0.000000000000000000, 1.000000000000000000, -0.000000000000000000 ) ) ;
#62533 = DIRECTION ( 'NONE',  ( -0.000000000000000000, 0.000000000000000000, 1.000000000000000000 ) ) ;
#62534 = VECTOR ( 'NONE', #48957, 1000.000000000000000 ) ;
#62535 = DIRECTION ( 'NONE',  ( 1.000000000000000000, 1.387778780781445922E-16, 0.000000000000000000 ) ) ;
#62536 = PLANE ( 'NONE',  #68010 ) ;
#62537 = PLANE ( 'NONE',  #5632 ) ;
#62538 = EDGE_LOOP ( 'NONE', ( #215, #13324, #41487, #16726 ) ) ;
#62539 = CARTESIAN_POINT ( 'NONE',  ( 70.41705859591010608, 15.55317472777718102, -44.45805487547348633 ) ) ;
#62540 = CARTESIAN_POINT ( 'NONE',  ( -118.4470345550925572, 42.96051736048242731, 37.07762135854807894 ) ) ;
#62541 = CARTESIAN_POINT ( 'NONE',  ( -173.1211646369891355, 87.12891641440857882, -61.55650775521367279 ) ) ;
#62542 = ADVANCED_BREP_SHAPE_REPRESENTATION ( '', ( #64301, #66832 ), #19703 ) ;
#62543 = ORIENTED_EDGE ( 'NONE', *, *, #16669, .T. ) ;
#62544 = CARTESIAN_POINT ( 'NONE',  ( -104.5916564445180228, 35.10571011602408475, 45.16936569891448983 ) ) ;
#62545 = ORIENTED_EDGE ( 'NONE', *, *, #17391, .F. ) ;
#62547 = AXIS2_PLACEMENT_3D ( 'NONE', #17553, #11560, #17907 ) ;
#62546 = CARTESIAN_POINT ( 'NONE',  ( -37.92542950990691253, 10.74638084523341952, 7.098505947254272641 ) ) ;
#62548 = CARTESIAN_POINT ( 'NONE',  ( 79.54836217416615796, 18.17815803851261691, 61.57198874188753024 ) ) ;
#62549 = VERTEX_POINT ( 'NONE', #32563 ) ;
#62550 = CARTESIAN_POINT ( 'NONE',  ( 1.005827167100601827, 0.000000000000000000, -9.949286995052577964 ) ) ;
#62551 = CARTESIAN_POINT ( 'NONE',  ( 0.000000000000000000, 0.000000000000000000, 41.38025477438755928 ) ) ;
#62552 = DIRECTION ( 'NONE',  ( 1.387778780781445429E-16, -1.000000000000000000, -3.081487911019577365E-33 ) ) ;
#62553 = PRESENTATION_STYLE_ASSIGNMENT (( #41092 ) ) ;
#62554 = CARTESIAN_POINT ( 'NONE',  ( 33.44527180510248598, 7.709232309484696621, 5.985868913544964087 ) ) ;
#62555 = CARTESIAN_POINT ( 'NONE',  ( -12.77550690612891948, 8.273784096785062658, -48.57362545616927463 ) ) ;
#62556 = CARTESIAN_POINT ( 'NONE',  ( -31.43908319763710679, 10.61114334766716283, -8.472646774738153752 ) ) ;
#62557 = ORIENTED_EDGE ( 'NONE', *, *, #7211, .F. ) ;
#62558 = CARTESIAN_POINT ( 'NONE',  ( -120.5470175916968714, 44.25832081621095426, -90.82375973165250116 ) ) ;
#62559 = ORIENTED_EDGE ( 'NONE', *, *, #41977, .F. ) ;
#62560 = CARTESIAN_POINT ( 'NONE',  ( -42.52062450115279546, -29.34795704556003670, 26.66469104408689361 ) ) ;
#62561 = CARTESIAN_POINT ( 'NONE',  ( -61.77164219855451677, 17.63686644795249592, 68.03177444750755853 ) ) ;
#62562 = CARTESIAN_POINT ( 'NONE',  ( -24.32937228292060894, 8.531905774118433428, 8.433788283749800385 ) ) ;
#62563 = VERTEX_POINT ( 'NONE', #23058 ) ;
#62564 = DIRECTION ( 'NONE',  ( 0.000000000000000000, 0.000000000000000000, 1.000000000000000000 ) ) ;
#62565 = CARTESIAN_POINT ( 'NONE',  ( -59.45032975077103998, 15.90473825383027418, -90.32613011058693075 ) ) ;
#62566 = CARTESIAN_POINT ( 'NONE',  ( -101.8191498210054817, 32.54686850610963234, -23.17002667451226117 ) ) ;
#62567 = B_SPLINE_CURVE_WITH_KNOTS ( 'NONE', 3,
 ( #8860, #29605, #19396, #35589, #63005, #52105, #2883, #40507, #24350, #30654, #30310, #45792, #67269, #14126, #46129, #14476, #19055, #8512, #25731, #3919, #67951, #29962, #61955, #40859, #13776, #47161, #4268, #35236, #51424, #3568, #68624, #57046, #41551, #46472, #51759, #20429, #9544, #19747, #56691, #68292, #41209, #67600, #3235, #25039, #57733, #46825, #62669, #41894, #34899, #35931, #57383, #25392, #20098, #14807, #36272, #31004 ),
 .UNSPECIFIED., .F., .F.,
 ( 4, 2, 2, 2, 2, 2, 2, 2, 2, 2, 2, 2, 2, 2, 2, 2, 2, 2, 2, 2, 2, 2, 2, 2, 2, 2, 2, 4 ),
 ( 0.000000000000000000, 0.001960808883428094649, 0.002941213325142143058, 0.003921617766856191033, 0.004902022208570239008, 0.005882426650284287850, 0.006862831091998335825, 0.007843235533712383800, 0.009804044417140516179, 0.01078444885885456589, 0.01176485330056861733, 0.01274525774228266704, 0.01372566218399671849, 0.01470606662571076993, 0.01568647106742481964, 0.01764727995085291212, 0.01960808883428100113, 0.02058849327599503176, 0.02156889771770906239, 0.02254930215942309302, 0.02352970660113712364, 0.02451011104285115080, 0.02549051548456518143, 0.02745132436799324616, 0.02843172880970725944, 0.02941213325142126925, 0.03039253769313528253, 0.03137294213484929234 ),
 .UNSPECIFIED. ) ;
#62568 = CARTESIAN_POINT ( 'NONE',  ( 157.4703587214989113, 58.92748579479260229, -36.12418429913763163 ) ) ;
#62569 = ORIENTED_EDGE ( 'NONE', *, *, #65655, .F. ) ;
#62570 = DIRECTION ( 'NONE',  ( 9.981598880770548021E-15, -1.000000000000000000, -4.052314039881821373E-15 ) ) ;
#62571 = CARTESIAN_POINT ( 'NONE',  ( -157.0079874970172966, 72.18249880494042259, 65.33901375635429076 ) ) ;
#62572 = CARTESIAN_POINT ( 'NONE',  ( 0.000000000000000000, 0.000000000000000000, 10.00000000000000000 ) ) ;
#62573 = CARTESIAN_POINT ( 'NONE',  ( -123.4531143159639299, 44.90777521523904880, 31.02450779894023469 ) ) ;
#62574 = LINE ( 'NONE', #30219, #31059 ) ;
#62575 = ORIENTED_EDGE ( 'NONE', *, *, #45250, .F. ) ;
#62576 = CARTESIAN_POINT ( 'NONE',  ( 32.99392442438140449, -170.0000000000000000, 94.99999999999866418 ) ) ;
#62577 = CARTESIAN_POINT ( 'NONE',  ( 136.3620490432820418, 44.14280731999023288, 83.62320897871926206 ) ) ;
#62578 = PRODUCT_DEFINITION_SHAPE ( 'NONE', 'NONE',  #69595 ) ;
#62579 = CARTESIAN_POINT ( 'NONE',  ( 112.1164716692773169, 29.75790342121399590, 44.38885595698212683 ) ) ;
#62580 = EDGE_CURVE ( 'NONE', #43828, #5944, #65967, .T. ) ;
#62581 = CARTESIAN_POINT ( 'NONE',  ( -7.916219337932451694, 0.000000000000000000, 6.110112224316693208 ) ) ;
#62582 = AXIS2_PLACEMENT_3D ( 'NONE', #21774, #43219, #64697 ) ;
#62583 = EDGE_CURVE ( 'NONE', #31341, #14491, #42386, .T. ) ;
#62584 = CARTESIAN_POINT ( 'NONE',  ( 444.9999999999999432, -35.00000000000000000, 380.0000000000000000 ) ) ;
#62585 = ORIENTED_EDGE ( 'NONE', *, *, #64314, .F. ) ;
#62586 = DIRECTION ( 'NONE',  ( -0.000000000000000000, 1.000000000000000000, -0.000000000000000000 ) ) ;
#62587 = DIRECTION ( 'NONE',  ( 1.000000000000000000, 0.000000000000000000, 0.000000000000000000 ) ) ;
#62588 = AXIS2_PLACEMENT_3D ( 'NONE', #13340, #35481, #12999 ) ;
#62589 = CYLINDRICAL_SURFACE ( 'NONE', #39799, 7.500000000000013323 ) ;
#62590 = CARTESIAN_POINT ( 'NONE',  ( 140.4769819293526893, 46.76840769395177944, 6.632038057673795173 ) ) ;
#62591 = EDGE_CURVE ( 'NONE', #47824, #18390, #39241, .T. ) ;
#62592 = DIRECTION ( 'NONE',  ( 0.000000000000000000, 0.000000000000000000, 1.000000000000000000 ) ) ;
#62593 = AXIS2_PLACEMENT_3D ( 'NONE', #455, #42675, #5395 ) ;
#62594 = VERTEX_POINT ( 'NONE', #53991 ) ;
#62595 = B_SPLINE_CURVE_WITH_KNOTS ( 'NONE', 3,
 ( #51851, #45535, #13536, #34304 ),
 .UNSPECIFIED., .F., .F.,
 ( 4, 4 ),
 ( 0.1259919275528358917, 0.1829744153748749103 ),
 .UNSPECIFIED. ) ;
#62596 = VECTOR ( 'NONE', #6825, 1000.000000000000000 ) ;
#62597 = CARTESIAN_POINT ( 'NONE',  ( 159.2258951716709134, 60.31399909112330704, -24.08478607002721006 ) ) ;
#62598 = ORIENTED_EDGE ( 'NONE', *, *, #41782, .F. ) ;
#62599 = VECTOR ( 'NONE', #47616, 1000.000000000000000 ) ;
#62600 = DIRECTION ( 'NONE',  ( -0.8118923937861950435, -0.5838071093367415143, 0.000000000000000000 ) ) ;
#62601 = CARTESIAN_POINT ( 'NONE',  ( 141.2703093103738468, 46.08481602256642873, 89.55010852364083007 ) ) ;
#62602 = ADVANCED_FACE ( 'NONE', ( #22008 ), #16720, .F. ) ;
#62604 = ORIENTED_EDGE ( 'NONE', *, *, #3498, .F. ) ;
#62603 = CARTESIAN_POINT ( 'NONE',  ( -12.50012419267789632, 70.00000000000000000, -27.27172336262651697 ) ) ;
#62605 = CARTESIAN_POINT ( 'NONE',  ( 160.2883311361769643, 61.16711613734478448, -36.67006685438227720 ) ) ;
#62606 = CARTESIAN_POINT ( 'NONE',  ( -25.00000000000028066, -65.13282190615278466, -5.000000000000000000 ) ) ;
#62607 = CARTESIAN_POINT ( 'NONE',  ( 160.9241720448058857, 60.38677655937336652, -36.95059568240409931 ) ) ;
#62608 = ORIENTED_EDGE ( 'NONE', *, *, #57745, .T. ) ;
#62609 = CARTESIAN_POINT ( 'NONE',  ( -61.68940124183720286, 16.56194981783060172, 94.99999999999866418 ) ) ;
#62610 = CARTESIAN_POINT ( 'NONE',  ( -131.6133495896317527, 50.37677745548732844, 42.97774246646625329 ) ) ;
#62611 = CARTESIAN_POINT ( 'NONE',  ( -3.000000000000002665, 3.043247295881173007E-15, 24.69999999999999929 ) ) ;
#62612 = DIRECTION ( 'NONE',  ( -1.000000000000000000, 0.000000000000000000, 0.000000000000000000 ) ) ;
#62613 = CARTESIAN_POINT ( 'NONE',  ( -166.9982296371934467, 80.56207291422407479, 33.98233018829063923 ) ) ;
#62614 = CARTESIAN_POINT ( 'NONE',  ( 150.2809931605061990, 52.27058242113235309, 61.60090139188071845 ) ) ;
#62615 = CARTESIAN_POINT ( 'NONE',  ( 149.0250918491436494, 6.000000000000000000, -41.68900338898718871 ) ) ;
#62616 = ORIENTED_EDGE ( 'NONE', *, *, #67667, .F. ) ;
#62617 = CARTESIAN_POINT ( 'NONE',  ( -99.98584758882475398, 32.75338129098884110, 57.70757149447982215 ) ) ;
#62618 = CARTESIAN_POINT ( 'NONE',  ( -9.524904342798462764, 8.016391612076533946, 57.15107637743524549 ) ) ;
#62619 = ORIENTED_EDGE ( 'NONE', *, *, #50188, .F. ) ;
#62620 = CARTESIAN_POINT ( 'NONE',  ( 0.000000000000000000, 6.928203230275506108, 4.000000000000007105 ) ) ;
#62621 = CARTESIAN_POINT ( 'NONE',  ( -55.70465171559254003, 14.85707552169330015, 84.02815862627096521 ) ) ;
#62622 = CARTESIAN_POINT ( 'NONE',  ( -22.17966048971185344, 25.00691465344610265, 6.893343212288939981 ) ) ;
#62623 = DIRECTION ( 'NONE',  ( 1.000000000000000000, -0.000000000000000000, 0.000000000000000000 ) ) ;
#62624 = AXIS2_PLACEMENT_3D ( 'NONE', #16539, #27429, #48866 ) ;
#62625 = LINE ( 'NONE', #4224, #60681 ) ;
#62626 = CARTESIAN_POINT ( 'NONE',  ( 185.5412249395996582, 84.70425786166001103, 3.927857500730326912 ) ) ;
#62627 = CARTESIAN_POINT ( 'NONE',  ( 210.0292194063021896, 113.9511645670926470, -38.54573400340662914 ) ) ;
#62628 = CYLINDRICAL_SURFACE ( 'NONE', #17489, 7.500000000000013323 ) ;
#62629 = VERTEX_POINT ( 'NONE', #17785 ) ;
#62630 = VECTOR ( 'NONE', #57191, 1000.000000000000000 ) ;
#62631 = CARTESIAN_POINT ( 'NONE',  ( 309.8720357909272707, 172.0000000000000284, 256.6193948016162381 ) ) ;
#62632 = ORIENTED_EDGE ( 'NONE', *, *, #17130, .F. ) ;
#62633 = CARTESIAN_POINT ( 'NONE',  ( 311.9732115134679020, 188.0000000000000000, -151.4173343409194672 ) ) ;
#62634 = CARTESIAN_POINT ( 'NONE',  ( 46.90170507415071910, 10.52318308703817884, -15.77993614618464591 ) ) ;
#62635 = VECTOR ( 'NONE', #54489, 1000.000000000000000 ) ;
#62636 = FACE_OUTER_BOUND ( 'NONE', #52585, .T. ) ;
#62637 = DIRECTION ( 'NONE',  ( -0.000000000000000000, -0.000000000000000000, 1.000000000000000000 ) ) ;
#62638 = DIRECTION ( 'NONE',  ( -0.000000000000000000, 1.000000000000000000, -0.000000000000000000 ) ) ;
#62639 = CARTESIAN_POINT ( 'NONE',  ( -103.8932886509196720, 34.74144483217663293, -22.99819252106857803 ) ) ;
#62640 = ORIENTED_EDGE ( 'NONE', *, *, #38012, .T. ) ;
#62641 = EDGE_CURVE ( 'NONE', #57574, #59496, #67500, .T. ) ;
#62643 = CIRCLE ( 'NONE', #10946, 8.000000000000000000 ) ;
#62642 = LINE ( 'NONE', #63327, #46507 ) ;
#62644 = DIRECTION ( 'NONE',  ( -0.000000000000000000, -0.000000000000000000, 1.000000000000000000 ) ) ;
#62645 = ORIENTED_EDGE ( 'NONE', *, *, #53883, .F. ) ;
#62646 = ORIENTED_EDGE ( 'NONE', *, *, #7939, .T. ) ;
#62647 = CARTESIAN_POINT ( 'NONE',  ( -152.9121563765244503, 67.12206067149024591, 44.90729742860457208 ) ) ;
#62648 = CARTESIAN_POINT ( 'NONE',  ( -23.73638277007043840, 7.847555861075215411, 0.000000000000000000 ) ) ;
#62649 = CARTESIAN_POINT ( 'NONE',  ( 173.6718135456487460, 71.42581476597410983, -15.69921511153743765 ) ) ;
#62650 = FILL_AREA_STYLE ('',( #20762 ) ) ;
#62651 = VECTOR ( 'NONE', #10252, 1000.000000000000000 ) ;
#62652 = CARTESIAN_POINT ( 'NONE',  ( 0.000000000000000000, 5.000000000000000000, 0.000000000000000000 ) ) ;
#62653 = ORIENTED_EDGE ( 'NONE', *, *, #59862, .F. ) ;
#62654 = CARTESIAN_POINT ( 'NONE',  ( 16.78635691501517613, 6.000000000000000000, -46.68900338898716029 ) ) ;
#62655 = ORIENTED_EDGE ( 'NONE', *, *, #63973, .F. ) ;
#62656 = CARTESIAN_POINT ( 'NONE',  ( 208.5889601154908917, 111.8333159387241551, 3.437899764226651111 ) ) ;
#62657 = CARTESIAN_POINT ( 'NONE',  ( 12.68603346975296198, 7.427591953486040843, 71.19195324979203576 ) ) ;
#62658 = CARTESIAN_POINT ( 'NONE',  ( 211.3917124729449881, 115.9987099435923170, 40.10166218625693801 ) ) ;
#62659 = CARTESIAN_POINT ( 'NONE',  ( 10.49251118870545874, 6.388821808438093441, -91.38086936670454463 ) ) ;
#62660 = EDGE_CURVE ( 'NONE', #57612, #44678, #13185, .T. ) ;
#62661 = ADVANCED_FACE ( 'NONE', ( #16386 ), #904, .F. ) ;
#62662 = EDGE_LOOP ( 'NONE', ( #63445, #63111, #4806, #32621 ) ) ;
#62663 = VERTEX_POINT ( 'NONE', #5816 ) ;
#62664 = CARTESIAN_POINT ( 'NONE',  ( 112.5114001799272074, -21.56931564127029688, 4.335727404899796689 ) ) ;
#62665 = CARTESIAN_POINT ( 'NONE',  ( -130.9554073334018938, 51.14437639132944469, 86.26655013740494837 ) ) ;
#62666 = CARTESIAN_POINT ( 'NONE',  ( -171.0814041607220020, 84.88598211196838861, -22.59712748936987481 ) ) ;
#62667 = CARTESIAN_POINT ( 'NONE',  ( -175.1968289912784087, 90.99944698359487916, 18.69656961583812915 ) ) ;
#62668 = EDGE_CURVE ( 'NONE', #5375, #38218, #43912, .T. ) ;
#62669 = CARTESIAN_POINT ( 'NONE',  ( 23.29087563001241179, 6.856811323692250326, 90.57454065962596701 ) ) ;
#62670 = CARTESIAN_POINT ( 'NONE',  ( 81.74909803672913711, 17.81295302817863302, -75.88269741394819334 ) ) ;
#62671 = AXIS2_PLACEMENT_3D ( 'NONE', #59359, #32638, #54063 ) ;
#62672 = ORIENTED_EDGE ( 'NONE', *, *, #53812, .T. ) ;
#62673 = DIRECTION ( 'NONE',  ( 1.000000000000000000, 0.000000000000000000, -0.000000000000000000 ) ) ;
#62674 = CARTESIAN_POINT ( 'NONE',  ( 204.3091227790962705, 107.5190503136782638, -36.32593103262159673 ) ) ;
#62675 = ORIENTED_EDGE ( 'NONE', *, *, #31931, .T. ) ;
#62676 =( BOUNDED_CURVE ( )  B_SPLINE_CURVE ( 3, ( #44145, #66346, #23760, #38898 ),
 .UNSPECIFIED., .F., .F. ) 
 B_SPLINE_CURVE_WITH_KNOTS ( ( 4, 4 ),
 ( 1.570796326794884568, 3.141592653589783346 ),
 .UNSPECIFIED. ) 
 CURVE ( )  GEOMETRIC_REPRESENTATION_ITEM ( )  RATIONAL_B_SPLINE_CURVE ( ( 1.000000000000000000, 0.8047378541243644934, 0.8047378541243644934, 1.000000000000000000 ) ) 
 REPRESENTATION_ITEM ( '' )  );
#62678 = CARTESIAN_POINT ( 'NONE',  ( -31.43908319763710679, -170.0000000000000000, -96.50629854612921577 ) ) ;
#62677 = VECTOR ( 'NONE', #57451, 1000.000000000000000 ) ;
#62679 = VERTEX_POINT ( 'NONE', #29374 ) ;
#62680 = CARTESIAN_POINT ( 'NONE',  ( -58.76099769480629220, 16.75353773354893860, -9.348133756430646812 ) ) ;
#62682 = ORIENTED_EDGE ( 'NONE', *, *, #49949, .F. ) ;
#62681 = EDGE_CURVE ( 'NONE', #40853, #43873, #19159, .T. ) ;
#62683 = VECTOR ( 'NONE', #41380, 1000.000000000000000 ) ;
#62684 = ORIENTED_EDGE ( 'NONE', *, *, #11025, .F. ) ;
#62685 = CARTESIAN_POINT ( 'NONE',  ( 50.97490815085634352, 6.000000000000000000, -41.68900338898716740 ) ) ;
#62686 = EDGE_CURVE ( 'NONE', #39748, #49666, #18131, .T. ) ;
#62688 = EDGE_CURVE ( 'NONE', #35709, #695, #27231, .T. ) ;
#62687 = CARTESIAN_POINT ( 'NONE',  ( -16.35146342289110422, 18.91109843266242052, 0.000000000000000000 ) ) ;
#62689 = CARTESIAN_POINT ( 'NONE',  ( 103.4725384926516654, 26.96797537091728003, 7.030248456595348472 ) ) ;
#62690 = ORIENTED_EDGE ( 'NONE', *, *, #21820, .F. ) ;
#62691 = CARTESIAN_POINT ( 'NONE',  ( 266.9165763529819628, -2.000000000000001776, 128.9999999999999716 ) ) ;
#62692 = VECTOR ( 'NONE', #45408, 999.9999999999998863 ) ;
#62693 = CARTESIAN_POINT ( 'NONE',  ( 174.2468109002382732, 73.34092405459593067, -67.47484041734936966 ) ) ;
#62694 = CARTESIAN_POINT ( 'NONE',  ( -65.20298343242130557, -4.613322252418190494, 6.377659838150142091E-18 ) ) ;
#62695 = CARTESIAN_POINT ( 'NONE',  ( 102.7571040248401459, 25.57023079238896557, -42.89496695998435172 ) ) ;
#62696 = CARTESIAN_POINT ( 'NONE',  ( 0.000000000000000000, 0.000000000000000000, 0.000000000000000000 ) ) ;
#62697 = CARTESIAN_POINT ( 'NONE',  ( -5.000000000000000000, 0.000000000000000000, 0.000000000000000000 ) ) ;
#62698 = VERTEX_POINT ( 'NONE', #67030 ) ;
#62699 = ORIENTED_EDGE ( 'NONE', *, *, #5607, .F. ) ;
#62700 = LINE ( 'NONE', #53142, #16271 ) ;
#62701 = CARTESIAN_POINT ( 'NONE',  ( -86.06525741550316866, 26.37048289224656372, -68.20633391999385253 ) ) ;
#62702 = CARTESIAN_POINT ( 'NONE',  ( 173.6700117628887483, 72.79957362875124716, 11.13452001345382314 ) ) ;
#62703 = DIRECTION ( 'NONE',  ( 0.000000000000000000, 0.000000000000000000, 1.000000000000000000 ) ) ;
#62704 = CARTESIAN_POINT ( 'NONE',  ( 16.54503815046451010, -18.74197728628616844, 0.000000000000000000 ) ) ;
#62705 = CARTESIAN_POINT ( 'NONE',  ( 136.4532421912245468, 43.01422451910222833, -90.16584641462647198 ) ) ;
#62706 = CARTESIAN_POINT ( 'NONE',  ( 33.59857101126895174, 7.725381174399810646, -92.04009980661062684 ) ) ;
#62707 = DIRECTION ( 'NONE',  ( 0.000000000000000000, 0.000000000000000000, 1.000000000000000000 ) ) ;
#62708 = CARTESIAN_POINT ( 'NONE',  ( 210.6592759200687510, 116.7161312026394029, 41.26595981562259396 ) ) ;
#62709 = CARTESIAN_POINT ( 'NONE',  ( -86.11230725916333029, 26.39026888680172434, 63.72904867199921597 ) ) ;
#62710 = CARTESIAN_POINT ( 'NONE',  ( -102.7502407665687798, 33.01985383847078026, 45.51907450641513719 ) ) ;
#62711 = VERTEX_POINT ( 'NONE', #18476 ) ;
#62712 = DIRECTION ( 'NONE',  ( 7.703719777548943412E-34, -1.479221584281240009E-31, 1.000000000000000000 ) ) ;
#62713 = VERTEX_POINT ( 'NONE', #44857 ) ;
#62714 = CARTESIAN_POINT ( 'NONE',  ( 203.1420903260745661, 104.2307086582026869, -9.599904899726423579 ) ) ;
#62715 = ORIENTED_EDGE ( 'NONE', *, *, #20387, .T. ) ;
#62716 = CARTESIAN_POINT ( 'NONE',  ( 64.99999999999997158, 0.000000000000000000, -105.0000000000000000 ) ) ;
#62717 = LINE ( 'NONE', #47543, #36141 ) ;
#62718 = DIRECTION ( 'NONE',  ( -1.000000000000000000, 0.000000000000000000, 0.000000000000000000 ) ) ;
#62719 = CARTESIAN_POINT ( 'NONE',  ( 21.57182537987927162, 17.67134260003770052, -14.82801705809902515 ) ) ;
#62720 = CARTESIAN_POINT ( 'NONE',  ( 32.90878072717890745, 7.653588083204843073, -39.35826442184654894 ) ) ;
#62721 = CARTESIAN_POINT ( 'NONE',  ( 198.5761553035918894, 98.31031792041292761, 86.05966332576983291 ) ) ;
#62722 = EDGE_CURVE ( 'NONE', #476, #15914, #40613, .T. ) ;
#62723 = CARTESIAN_POINT ( 'NONE',  ( 10.13563904803030979, 7.391572367417537315, -38.06542051270953664 ) ) ;
#62724 = CARTESIAN_POINT ( 'NONE',  ( 133.3996297101684263, 41.14871796345732236, -36.02331093239567394 ) ) ;
#62725 = ORIENTED_EDGE ( 'NONE', *, *, #27211, .T. ) ;
#62726 = VERTEX_POINT ( 'NONE', #30075 ) ;
#62727 = VECTOR ( 'NONE', #39816, 1000.000000000000000 ) ;
#62728 = EDGE_CURVE ( 'NONE', #62792, #16895, #19505, .T. ) ;
#62729 = CARTESIAN_POINT ( 'NONE',  ( -125.8938041572051389, 47.69968343338780414, -8.069153307770243089 ) ) ;
#62730 = CARTESIAN_POINT ( 'NONE',  ( -149.5074843970971017, 65.50121172469319220, 18.87627064943540134 ) ) ;
#62731 = CARTESIAN_POINT ( 'NONE',  ( -28.13266652174641180, 9.071935854491414375, -62.92545503574774557 ) ) ;
#62732 = VECTOR ( 'NONE', #7733, 1000.000000000000114 ) ;
#62733 = UNCERTAINTY_MEASURE_WITH_UNIT (LENGTH_MEASURE( 1.000000000000000082E-05 ), #68183, 'distance_accuracy_value', 'NONE');
#62734 = CARTESIAN_POINT ( 'NONE',  ( 8.951900209438536038, 6.378066731449593796, 7.575917132388738651 ) ) ;
#62735 = FACE_OUTER_BOUND ( 'NONE', #21926, .T. ) ;
#62736 = VERTEX_POINT ( 'NONE', #45545 ) ;
#62737 = LINE ( 'NONE', #62386, #52566 ) ;
#62738 = CARTESIAN_POINT ( 'NONE',  ( 173.5843421840238250, 71.34465141434344559, -70.26636659897270931 ) ) ;
#62739 = CARTESIAN_POINT ( 'NONE',  ( -173.1211646369891355, 87.12891641440857882, -49.71195716475001092 ) ) ;
#62740 = CARTESIAN_POINT ( 'NONE',  ( 93.92280655489128094, 22.03989931749466180, -18.24301154267179825 ) ) ;
#62741 = CARTESIAN_POINT ( 'NONE',  ( -28.13527276074848160, 10.08983026464524357, 57.82341847530290835 ) ) ;
#62742 = CARTESIAN_POINT ( 'NONE',  ( 105.6617573822854155, 21.85836566642198520, 2.507523880400407190 ) ) ;
#62743 = EDGE_CURVE ( 'NONE', #14641, #62240, #13884, .T. ) ;
#62744 = DIRECTION ( 'NONE',  ( -0.000000000000000000, -0.000000000000000000, -1.000000000000000000 ) ) ;
#62745 = EDGE_CURVE ( 'NONE', #14749, #31022, #34315, .T. ) ;
#62746 = EDGE_CURVE ( 'NONE', #44262, #1254, #40966, .T. ) ;
#62747 = ORIENTED_EDGE ( 'NONE', *, *, #58511, .T. ) ;
#62748 = LINE ( 'NONE', #57809, #4678 ) ;
#62749 = CARTESIAN_POINT ( 'NONE',  ( 7.762887554996211747E-14, 51.66904755831208718, 0.000000000000000000 ) ) ;
#62750 = CARTESIAN_POINT ( 'NONE',  ( -109.7811201291770118, 37.90784085457603680, -69.12879967873752207 ) ) ;
#62751 = CARTESIAN_POINT ( 'NONE',  ( -47.80896875121164413, 12.85816703949531181, -40.75691379661022751 ) ) ;
#62752 = DIRECTION ( 'NONE',  ( 0.3930250316539148359, 0.9195277725514544587, 0.000000000000000000 ) ) ;
#62753 = PLANE ( 'NONE',  #38986 ) ;
#62754 = ORIENTED_EDGE ( 'NONE', *, *, #33555, .F. ) ;
#62755 = PLANE ( 'NONE',  #6852 ) ;
#62756 = VERTEX_POINT ( 'NONE', #61383 ) ;
#62757 = VERTEX_POINT ( 'NONE', #28682 ) ;
#62758 = CARTESIAN_POINT ( 'NONE',  ( 0.7145311798163248573, -4.618802153517011178, 8.000000000000000000 ) ) ;
#62759 = DIRECTION ( 'NONE',  ( -1.000000000000000000, 0.000000000000000000, 0.000000000000000000 ) ) ;
#62760 = CARTESIAN_POINT ( 'NONE',  ( 0.000000000000000000, 6.000000000000000000, -20.00000000000000000 ) ) ;
#62761 = ORIENTED_EDGE ( 'NONE', *, *, #30733, .F. ) ;
#62762 = CARTESIAN_POINT ( 'NONE',  ( 200.0000000000000000, 3.000000000000030198, -3.000000000000030198 ) ) ;
#62763 = DIRECTION ( 'NONE',  ( -0.000000000000000000, 1.000000000000000000, -0.000000000000000000 ) ) ;
#62764 = CARTESIAN_POINT ( 'NONE',  ( 0.000000000000000000, 0.000000000000000000, -9.500000000000000000 ) ) ;
#62765 = CARTESIAN_POINT ( 'NONE',  ( -15.47041015649658391, 73.39774458108210808, 73.58025477438756923 ) ) ;
#62766 = EDGE_CURVE ( 'NONE', #40228, #58737, #55400, .T. ) ;
#62768 = ADVANCED_FACE ( 'NONE', ( #56106 ), #2645, .F. ) ;
#62767 = CARTESIAN_POINT ( 'NONE',  ( -81.90760111942958588, 24.66532273091448246, 44.69847146411395755 ) ) ;
#62769 = CARTESIAN_POINT ( 'NONE',  ( -4.000000000000009770, -6.928203230275505220, 0.000000000000000000 ) ) ;
#62770 = CARTESIAN_POINT ( 'NONE',  ( 204.6977192012829789, -170.0000000000000000, -63.17048162308526571 ) ) ;
#62771 = EDGE_CURVE ( 'NONE', #36722, #15646, #21108, .T. ) ;
#62772 = ORIENTED_EDGE ( 'NONE', *, *, #26494, .F. ) ;
#62773 = CARTESIAN_POINT ( 'NONE',  ( 0.000000000000000000, 0.000000000000000000, 8.000000000000000000 ) ) ;
#62774 = CARTESIAN_POINT ( 'NONE',  ( 11.82322073186613487, 6.406156243758798219, 57.98838548183650232 ) ) ;
#62775 = DIRECTION ( 'NONE',  ( 0.008343357611898890094, 0.000000000000000000, 0.9999651935861366692 ) ) ;
#62776 = CARTESIAN_POINT ( 'NONE',  ( 199.7286177451875915, 101.4075663537892069, 31.07105176568274629 ) ) ;
#62777 = CARTESIAN_POINT ( 'NONE',  ( -81.12211859130741232, 24.35291027093249383, 84.49380358467659846 ) ) ;
#62779 = ORIENTED_EDGE ( 'NONE', *, *, #69541, .T. ) ;
#62778 = CARTESIAN_POINT ( 'NONE',  ( -34.75846525698938194, -54.92585086258257121, 170.0000000000000000 ) ) ;
#62780 = CARTESIAN_POINT ( 'NONE',  ( -447.6627218934913230, 1.665334536937734811E-13, 83.55029585798817493 ) ) ;
#62781 = VERTEX_POINT ( 'NONE', #52550 ) ;
#62782 = VECTOR ( 'NONE', #18624, 1000.000000000000000 ) ;
#62783 = ORIENTED_EDGE ( 'NONE', *, *, #46678, .F. ) ;
#62784 = CARTESIAN_POINT ( 'NONE',  ( 115.7731501832036400, 32.64791439093733061, -75.35713396160309685 ) ) ;
#62785 = CARTESIAN_POINT ( 'NONE',  ( 3.245026627011502907, -33.26789626822845491, 6.893343212288929323 ) ) ;
#62786 = CARTESIAN_POINT ( 'NONE',  ( 198.2545923567585646, 97.90679023593577313, -74.51984543740591960 ) ) ;
#62787 = CARTESIAN_POINT ( 'NONE',  ( -38.54712373114178092, 11.89174538567466932, 62.11797067184914312 ) ) ;
#62788 = CARTESIAN_POINT ( 'NONE',  ( -124.9927180788553756, 45.90286323198617424, 72.42390737291080427 ) ) ;
#62789 = CARTESIAN_POINT ( 'NONE',  ( -85.89078989036967471, 26.29712602777651398, -17.80139899211184940 ) ) ;
#62790 = PLANE ( 'NONE',  #65698 ) ;
#62791 = CARTESIAN_POINT ( 'NONE',  ( -48.58279704072702998, 14.07632445131079635, 41.61883750805020554 ) ) ;
#62792 = VERTEX_POINT ( 'NONE', #10324 ) ;
#62793 = EDGE_LOOP ( 'NONE', ( #33389, #30304, #57983, #32644, #18410, #21063, #60928, #34202, #40264 ) ) ;
#62794 = DIRECTION ( 'NONE',  ( -1.110223024625156540E-16, -1.358505038629840220E-33, -1.000000000000000000 ) ) ;
#62795 = B_SPLINE_CURVE_WITH_KNOTS ( 'NONE', 3,
 ( #4349, #20173, #41627, #18885 ),
 .UNSPECIFIED., .F., .F.,
 ( 4, 4 ),
 ( 0.1259919275528361415, 0.1829744153748754654 ),
 .UNSPECIFIED. ) ;
#62796 = CARTESIAN_POINT ( 'NONE',  ( 103.1653143050726271, 25.74301230421576747, 66.48834995395209546 ) ) ;
#62797 = CARTESIAN_POINT ( 'NONE',  ( 113.6936194768560853, 30.51122948389054201, 84.13335573343988472 ) ) ;
#62798 = FACE_OUTER_BOUND ( 'NONE', #14344, .T. ) ;
#62799 = AXIS2_PLACEMENT_3D ( 'NONE', #50600, #2420, #8395 ) ;
#62800 = LINE ( 'NONE', #67737, #19153 ) ;
#62801 = CARTESIAN_POINT ( 'NONE',  ( 0.06809871960542744629, 7.710219529346611367, -2.645508037661881584 ) ) ;
#62802 = DIRECTION ( 'NONE',  ( -0.000000000000000000, -1.000000000000000000, -0.000000000000000000 ) ) ;
#62803 = ORIENTED_EDGE ( 'NONE', *, *, #6103, .F. ) ;
#62804 = ORIENTED_EDGE ( 'NONE', *, *, #8082, .T. ) ;
#62805 = VERTEX_POINT ( 'NONE', #14913 ) ;
#62806 = EDGE_CURVE ( 'NONE', #43392, #20959, #28873, .T. ) ;
#62807 = SURFACE_SIDE_STYLE ('',( #36072 ) ) ;
#62808 = CARTESIAN_POINT ( 'NONE',  ( -83.14462298835724141, 24.07775853418029754, 58.72718026324421459 ) ) ;
#62809 = DIRECTION ( 'NONE',  ( 0.000000000000000000, -1.000000000000000000, 0.000000000000000000 ) ) ;
#62810 = CARTESIAN_POINT ( 'NONE',  ( 107.5866342775021849, 27.67195717782396969, -90.08692006097672333 ) ) ;
#62811 = CARTESIAN_POINT ( 'NONE',  ( -55.54036735998995766, 15.85474597822063991, 45.31732777293116499 ) ) ;
#62812 = MANIFOLD_SOLID_BREP ( 'Cut-Extrude7', #29416 ) ;
#62813 = CARTESIAN_POINT ( 'NONE',  ( -31.93169728792084783, 10.69234447276977562, -62.16174795566553257 ) ) ;
#62814 = CIRCLE ( 'NONE', #59423, 5.000000000000000888 ) ;
#62815 = CARTESIAN_POINT ( 'NONE',  ( -156.6692143066620702, 70.50016761530885390, -17.71246865387325897 ) ) ;
#62816 = CARTESIAN_POINT ( 'NONE',  ( 186.5979919519638202, 85.84756789133376742, 68.74285688226639479 ) ) ;
#62817 = CARTESIAN_POINT ( 'NONE',  ( 14.80582440982707482, 6.470883766728821485, -8.722983937927098808 ) ) ;
#62818 = ORIENTED_EDGE ( 'NONE', *, *, #2053, .T. ) ;
#62819 = CARTESIAN_POINT ( 'NONE',  ( -1.314022807222076761, 6.554273999800675377, -39.16415506736178287 ) ) ;
#62820 = CARTESIAN_POINT ( 'NONE',  ( 188.4937788906148910, 86.43336847120860966, 64.85195978288442120 ) ) ;
#62821 = DIRECTION ( 'NONE',  ( -0.000000000000000000, -1.000000000000000000, -0.000000000000000000 ) ) ;
#62822 = CARTESIAN_POINT ( 'NONE',  ( 66.30567821786755189, 13.45988234822863205, -63.32099564467209518 ) ) ;
#62823 = CARTESIAN_POINT ( 'NONE',  ( 126.8015497489690659, 37.32461426945043570, -19.23696772009197176 ) ) ;
#62824 = EDGE_CURVE ( 'NONE', #37937, #29599, #57493, .T. ) ;
#62825 = CARTESIAN_POINT ( 'NONE',  ( 22.28556289340099639, 7.803548444155008035, -19.92885657512854536 ) ) ;
#62826 = CARTESIAN_POINT ( 'NONE',  ( 8.679939806240508204, 7.383357464882123189, 13.07472991024607190 ) ) ;
#62827 = EDGE_CURVE ( 'NONE', #54796, #56777, #25837, .T. ) ;
#62828 = VECTOR ( 'NONE', #41986, 1000.000000000000000 ) ;
#62829 = EDGE_CURVE ( 'NONE', #10603, #67718, #47269, .T. ) ;
#62830 = ORIENTED_EDGE ( 'NONE', *, *, #57352, .T. ) ;
#62831 = CARTESIAN_POINT ( 'NONE',  ( 185.1647878987785987, 82.82967084668429436, 3.655828051775791288 ) ) ;
#62832 = PRODUCT_CONTEXT ( 'NONE', #45758, 'mechanical' ) ;
#62833 = CARTESIAN_POINT ( 'NONE',  ( 127.4669243510812890, 38.85312661085429653, -39.56414112603825117 ) ) ;
#62834 = CARTESIAN_POINT ( 'NONE',  ( -128.9786047358386725, 48.55852351614670681, -35.57352493381657865 ) ) ;
#62835 = CARTESIAN_POINT ( 'NONE',  ( -107.2385267828037314, 36.51474259889400287, -48.14687793975550534 ) ) ;
#62836 = EDGE_CURVE ( 'NONE', #29447, #51672, #68721, .T. ) ;
#62837 = MECHANICAL_DESIGN_GEOMETRIC_PRESENTATION_REPRESENTATION (  '', ( #53859 ), #2183 ) ;
#62838 = CARTESIAN_POINT ( 'NONE',  ( 186.6075385349484463, 85.85749512876283518, -48.82324223727037804 ) ) ;
#62839 = ORIENTED_EDGE ( 'NONE', *, *, #14314, .F. ) ;
#62840 = ORIENTED_EDGE ( 'NONE', *, *, #32632, .T. ) ;
#62841 = CARTESIAN_POINT ( 'NONE',  ( -142.3178993725748569, 58.31327888234796575, -13.25976637110863443 ) ) ;
#62842 = CARTESIAN_POINT ( 'NONE',  ( -1.224646799147352468E-15, 16.00000000000000000, -5.803681084894614095 ) ) ;
#62843 = ORIENTED_EDGE ( 'NONE', *, *, #57121, .T. ) ;
#62844 = CARTESIAN_POINT ( 'NONE',  ( 151.9622908680735520, 54.74094082471709299, 85.49672239616074876 ) ) ;
#62845 = ORIENTED_EDGE ( 'NONE', *, *, #57723, .F. ) ;
#62846 = CARTESIAN_POINT ( 'NONE',  ( 133.4058733589413634, 42.32720528873925758, -77.86786152285935714 ) ) ;
#62847 = CARTESIAN_POINT ( 'NONE',  ( 126.4083787442699958, 37.10531539900949127, 35.98502578816821540 ) ) ;
#62848 = CARTESIAN_POINT ( 'NONE',  ( -29.72794987547381140, 29.28418937382772569, 13.79046412439885927 ) ) ;
#62849 = CIRCLE ( 'NONE', #32506, 5.000000000000115463 ) ;
#62850 = CARTESIAN_POINT ( 'NONE',  ( 29.86848256228606502, -58.14280299503694494, 6.377659838150125914E-18 ) ) ;
#62851 = DIRECTION ( 'NONE',  ( 0.000000000000000000, 0.000000000000000000, 1.000000000000000000 ) ) ;
#62852 = B_SPLINE_CURVE_WITH_KNOTS ( 'NONE', 3,
 ( #34707, #19903, #30118, #50866, #13582, #62108, #67071, #13247, #41359, #8312, #3712, #18865, #7961, #14280, #13924, #40313, #56846, #3039, #39967, #46624, #29415, #51569, #8663, #68099, #3377, #51222, #40653, #61426, #2682, #24500, #67402, #24148, #45590, #9006, #19193, #25189, #35044, #24831, #56486, #35740, #46273, #67749, #62811, #29760 ),
 .UNSPECIFIED., .F., .F.,
 ( 4, 2, 2, 2, 2, 2, 2, 2, 2, 2, 2, 2, 1, 2, 2, 2, 2, 2, 2, 1, 2, 2, 4 ),
 ( 0.02381751147647563974, 0.02531129726520769258, 0.02605819015957371726, 0.02680508305393974541, 0.02829886884267179131, 0.02979265463140384068, 0.03053954752576986884, 0.03128644042013589699, 0.03278022620886796024, 0.03427401199760002348, 0.03576779778633208673, 0.03651469068069810447, 0.03726158357506412222, 0.03800847646943014690, 0.03875536936379617159, 0.04024915515252819320, 0.04174294094126021482, 0.04323672672999225031, 0.04398361962435826111, 0.04473051251872428580, 0.04547740541309029660, 0.04622429830745632129, 0.04771808409618833596 ),
 .UNSPECIFIED. ) ;
#62854 = VERTEX_POINT ( 'NONE', #36036 ) ;
#62853 = LINE ( 'NONE', #62146, #42093 ) ;
#62855 = EDGE_CURVE ( 'NONE', #564, #27576, #30621, .T. ) ;
#62856 = DIRECTION ( 'NONE',  ( 0.000000000000000000, 0.000000000000000000, -1.000000000000000000 ) ) ;
#62857 = ORIENTED_EDGE ( 'NONE', *, *, #11125, .T. ) ;
#62858 = ORIENTED_EDGE ( 'NONE', *, *, #66176, .F. ) ;
#62859 = CARTESIAN_POINT ( 'NONE',  ( -169.8885678771097787, 85.07765565657315676, 4.695052042634683787 ) ) ;
#62860 = CARTESIAN_POINT ( 'NONE',  ( -177.1539090641757639, 91.73101548694630480, -9.028362732657411627 ) ) ;
#62862 = ORIENTED_EDGE ( 'NONE', *, *, #30989, .F. ) ;
#62861 = LINE ( 'NONE', #57585, #61282 ) ;
#62863 = CARTESIAN_POINT ( 'NONE',  ( -108.8469686167213837, 37.39105600699775778, 88.02876656477920392 ) ) ;
#62864 = CIRCLE ( 'NONE', #35902, 10.00000000000000000 ) ;
#62865 = LINE ( 'NONE', #51956, #23881 ) ;
#62866 = ORIENTED_EDGE ( 'NONE', *, *, #1181, .F. ) ;
#62867 = DIRECTION ( 'NONE',  ( 0.000000000000000000, 0.000000000000000000, 1.000000000000000000 ) ) ;
#62868 = CARTESIAN_POINT ( 'NONE',  ( -132.4776673493543058, 52.21763813822162348, -72.85944512281113816 ) ) ;
#62869 = CARTESIAN_POINT ( 'NONE',  ( -56.44201257846588504, -32.26641783793643015, 3.061616997868437868E-16 ) ) ;
#62870 = CARTESIAN_POINT ( 'NONE',  ( 290.0000000000000568, 2.449293598294704935E-15, -19.99999999999997868 ) ) ;
#62871 = CARTESIAN_POINT ( 'NONE',  ( 69.83260694998129736, 15.39825517924929343, -66.92839821032720238 ) ) ;
#62872 = ORIENTED_EDGE ( 'NONE', *, *, #47877, .T. ) ;
#62873 = VECTOR ( 'NONE', #39844, 1000.000000000000000 ) ;
#62874 = ORIENTED_EDGE ( 'NONE', *, *, #44740, .T. ) ;
#62875 = CARTESIAN_POINT ( 'NONE',  ( -149.5074843970971017, 65.50121172469319220, -22.96827994102830317 ) ) ;
#62876 = DIRECTION ( 'NONE',  ( 0.000000000000000000, 1.000000000000000000, 0.000000000000000000 ) ) ;
#62877 = FACE_BOUND ( 'NONE', #19110, .T. ) ;
#62878 = CARTESIAN_POINT ( 'NONE',  ( -47.68562151781910785, 12.82916850665305475, -95.00000000000133582 ) ) ;
#62879 = CARTESIAN_POINT ( 'NONE',  ( -53.57849794046929759, 15.33131313570892829, -89.04869412804561080 ) ) ;
#62880 = LINE ( 'NONE', #14681, #51743 ) ;
#62881 = CARTESIAN_POINT ( 'NONE',  ( -147.7845268487069177, 62.73119438705055018, 45.53313422460936266 ) ) ;
#62882 = DIRECTION ( 'NONE',  ( 4.640644490319818793E-15, 1.000000000000000000, -7.216449660063517513E-16 ) ) ;
#62883 = CARTESIAN_POINT ( 'NONE',  ( 205.5004956747122549, 107.4493581495447927, 56.08442209846073467 ) ) ;
#62885 = ORIENTED_EDGE ( 'NONE', *, *, #36906, .F. ) ;
#62884 = EDGE_CURVE ( 'NONE', #44487, #33757, #23327, .T. ) ;
#62886 = CARTESIAN_POINT ( 'NONE',  ( -108.6944271866238978, 37.30738480893074183, 41.93777729395904430 ) ) ;
#62887 = ORIENTED_EDGE ( 'NONE', *, *, #52690, .T. ) ;
#62888 = CARTESIAN_POINT ( 'NONE',  ( -33.13098007862451055, 9.875138601866705557, 18.18261215273323472 ) ) ;
#62889 = EDGE_CURVE ( 'NONE', #57138, #26335, #33181, .T. ) ;
#62890 = CARTESIAN_POINT ( 'NONE',  ( 79.14113188808478583, 18.05280674635441684, 64.54754759442464263 ) ) ;
#62891 = DIRECTION ( 'NONE',  ( 1.000000000000000000, 0.000000000000000000, 0.000000000000000000 ) ) ;
#62892 = CARTESIAN_POINT ( 'NONE',  ( -59.42430146430426419, 27.22983999535709287, 43.58025477438756212 ) ) ;
#62893 = SPHERICAL_SURFACE ( 'NONE', #17522, 3.000000000000000000 ) ;
#62894 = CYLINDRICAL_SURFACE ( 'NONE', #45622, 5.000000000000000888 ) ;
#62895 = CARTESIAN_POINT ( 'NONE',  ( 31.96227686234411181, 7.558148489540048587, 9.588200182408197492 ) ) ;
#62896 = DIRECTION ( 'NONE',  ( -1.110223024625155594E-14, 0.000000000000000000, -1.000000000000000000 ) ) ;
#62897 = CIRCLE ( 'NONE', #13488, 4.999999999999997335 ) ;
#62898 = LINE ( 'NONE', #30539, #57384 ) ;
#62899 = EDGE_LOOP ( 'NONE', ( #62938, #65835, #7791, #15780 ) ) ;
#62900 = CARTESIAN_POINT ( 'NONE',  ( 29.99999999999999645, 26.99999999999999645, 12.00000000000000000 ) ) ;
#62901 = ORIENTED_EDGE ( 'NONE', *, *, #4527, .F. ) ;
#62902 = CARTESIAN_POINT ( 'NONE',  ( -58.10608953386395825, 15.52134062643866486, 30.96269639377317517 ) ) ;
#62903 = CARTESIAN_POINT ( 'NONE',  ( -31.43908319763710679, 9.591432048623756756, -8.472646774738153752 ) ) ;
#62904 = CARTESIAN_POINT ( 'NONE',  ( -189.7987719395348734, 107.8653664616570609, 14.45894391646097077 ) ) ;
#62905 = DIRECTION ( 'NONE',  ( 0.000000000000000000, 0.000000000000000000, 1.000000000000000000 ) ) ;
#62906 = CARTESIAN_POINT ( 'NONE',  ( -55.48029021084977330, 14.79618042659997634, -88.90542517938726519 ) ) ;
#62907 = CARTESIAN_POINT ( 'NONE',  ( -101.8145602049405625, 32.54453702486149780, -8.170026674512225640 ) ) ;
#62908 = CARTESIAN_POINT ( 'NONE',  ( 149.9883446984744921, 53.30011109831376359, -44.21193250460613910 ) ) ;
#62910 = EDGE_CURVE ( 'NONE', #21098, #52425, #43172, .T. ) ;
#62909 =( REPRESENTATION_RELATIONSHIP ('NONE','NONE', #40274, #60409 ) REPRESENTATION_RELATIONSHIP_WITH_TRANSFORMATION ( #47536 )SHAPE_REPRESENTATION_RELATIONSHIP( ) );
#62911 = EDGE_CURVE ( 'NONE', #36977, #2227, #39841, .T. ) ;
#62912 = ORIENTED_EDGE ( 'NONE', *, *, #9627, .F. ) ;
#62913 = DIRECTION ( 'NONE',  ( -0.4127148655274864297, 0.9108602745606095841, 7.704279872735864927E-15 ) ) ;
#62914 = AXIS2_PLACEMENT_3D ( 'NONE', #6476, #50433, #1911 ) ;
#62915 = DIRECTION ( 'NONE',  ( -0.000000000000000000, -1.000000000000000000, -0.000000000000000000 ) ) ;
#62916 = CARTESIAN_POINT ( 'NONE',  ( 173.5844030397475706, 72.71952271766126330, -17.18546232013203934 ) ) ;
#62917 = EDGE_CURVE ( 'NONE', #60171, #66426, #34585, .T. ) ;
#62918 = CARTESIAN_POINT ( 'NONE',  ( -108.9444157621018405, 37.44493815491210853, 68.34273079517608096 ) ) ;
#62919 = CARTESIAN_POINT ( 'NONE',  ( -2.954450920023000372E-15, 7.124194613927624431, 3.660532965668821248 ) ) ;
#62920 = ORIENTED_EDGE ( 'NONE', *, *, #25645, .F. ) ;
#62921 = CARTESIAN_POINT ( 'NONE',  ( -173.1211646369891071, 88.63826465341152527, -61.55650775521367279 ) ) ;
#62922 = CARTESIAN_POINT ( 'NONE',  ( -0.5183605925911975998, 6.525266619725953454, -17.78142633563535213 ) ) ;
#62923 = CARTESIAN_POINT ( 'NONE',  ( 110.7114632166112358, 29.09878355652111992, 29.61121420573730134 ) ) ;
#62924 =( NAMED_UNIT ( * ) SI_UNIT ( $, .STERADIAN. ) SOLID_ANGLE_UNIT ( ) );
#62925 = CARTESIAN_POINT ( 'NONE',  ( 400.0000000000000000, 0.000000000000000000, 20.00000000000000000 ) ) ;
#62926 = VERTEX_POINT ( 'NONE', #8182 ) ;
#62927 = CARTESIAN_POINT ( 'NONE',  ( 201.9869293910475392, 102.6997661182767274, 43.71240911156287012 ) ) ;
#62928 = CARTESIAN_POINT ( 'NONE',  ( 113.8568724296587789, 30.58972477291341363, -76.85635754368730943 ) ) ;
#62929 = CARTESIAN_POINT ( 'NONE',  ( -51.84164840787130402, -39.21024726209533640, 170.0000000000000000 ) ) ;
#62930 = CARTESIAN_POINT ( 'NONE',  ( 141.1220430186942281, 47.19066702031171445, 12.04571220398737452 ) ) ;
#62931 = DIRECTION ( 'NONE',  ( 0.000000000000000000, 0.000000000000000000, 1.000000000000000000 ) ) ;
#62932 = VERTEX_POINT ( 'NONE', #24715 ) ;
#62933 = CARTESIAN_POINT ( 'NONE',  ( 0.000000000000000000, 0.000000000000000000, 7.000000000000000000 ) ) ;
#62934 = ORIENTED_EDGE ( 'NONE', *, *, #16192, .F. ) ;
#62935 = CARTESIAN_POINT ( 'NONE',  ( 70.51583798635768119, 15.57951509147424041, 63.91560277332340689 ) ) ;
#62936 = CARTESIAN_POINT ( 'NONE',  ( 129.1909336867078935, 38.67767333518755635, 84.81811994820998279 ) ) ;
#62938 = ORIENTED_EDGE ( 'NONE', *, *, #5300, .F. ) ;
#62937 = CARTESIAN_POINT ( 'NONE',  ( 152.1381498073140790, 54.87048121475570639, 4.768634089295844980 ) ) ;
#62939 = CARTESIAN_POINT ( 'NONE',  ( 159.6614743841974473, 60.66237087206235401, -50.81097292345923222 ) ) ;
#62940 = VECTOR ( 'NONE', #51889, 1000.000000000000000 ) ;
#62941 = PLANE ( 'NONE',  #31665 ) ;
#62942 = CARTESIAN_POINT ( 'NONE',  ( 112.5537757279407316, 31.07998172410697180, -36.27139529453720712 ) ) ;
#62943 = EDGE_LOOP ( 'NONE', ( #53292, #13964, #55349, #44306 ) ) ;
#62944 = CARTESIAN_POINT ( 'NONE',  ( 26.99999999999999645, 26.99999999999999289, 15.00000000000000000 ) ) ;
#62945 = CARTESIAN_POINT ( 'NONE',  ( -17.50000000000002842, -18.06806526123148160, 0.000000000000000000 ) ) ;
#62946 = ORIENTED_EDGE ( 'NONE', *, *, #30021, .F. ) ;
#62947 = CARTESIAN_POINT ( 'NONE',  ( 136.3292018078239494, 42.93753790426542594, 56.77035877741786862 ) ) ;
#62948 = CARTESIAN_POINT ( 'NONE',  ( -165.7143741370936709, 79.24519349471955820, 37.10392210004761893 ) ) ;
#62949 = CARTESIAN_POINT ( 'NONE',  ( 26.99999999999999289, 26.99999999999999645, 15.00000000000000000 ) ) ;
#62950 = DIRECTION ( 'NONE',  ( -0.000000000000000000, 1.000000000000000000, -0.000000000000000000 ) ) ;
#62951 = VERTEX_POINT ( 'NONE', #50740 ) ;
#62952 = DIRECTION ( 'NONE',  ( 1.000000000000000000, 0.000000000000000000, 0.000000000000000000 ) ) ;
#62953 = ORIENTED_EDGE ( 'NONE', *, *, #10851, .T. ) ;
#62954 = VECTOR ( 'NONE', #27748, 1000.000000000000000 ) ;
#62955 = CARTESIAN_POINT ( 'NONE',  ( 151.3136733342016953, 54.26417151662140981, -12.48898785249184407 ) ) ;
#62956 = ADVANCED_FACE ( 'NONE', ( #28599 ), #44776, .T. ) ;
#62957 = CARTESIAN_POINT ( 'NONE',  ( -49.88515215727291263, 13.35630923481828169, 86.04290591518972064 ) ) ;
#62958 = CARTESIAN_POINT ( 'NONE',  ( 107.2614272668149340, 28.62909081796205513, 43.99715716284213585 ) ) ;
#62959 = CARTESIAN_POINT ( 'NONE',  ( -151.2497169612549328, 65.66843968092751993, -61.80823754933450687 ) ) ;
#62960 = DIRECTION ( 'NONE',  ( -0.000000000000000000, -0.000000000000000000, 1.000000000000000000 ) ) ;
#62961 = CARTESIAN_POINT ( 'NONE',  ( 188.4374648754671284, 87.87346242052440459, 8.459214379405038287 ) ) ;
#62962 = CARTESIAN_POINT ( 'NONE',  ( 208.9781236209186090, 112.4006213943319636, -37.65073565875546535 ) ) ;
#62963 = EDGE_CURVE ( 'NONE', #30890, #37055, #13460, .T. ) ;
#62964 = CARTESIAN_POINT ( 'NONE',  ( 176.0745160362857860, 73.68684431790050837, 15.55076182205331570 ) ) ;
#62965 = VERTEX_POINT ( 'NONE', #19076 ) ;
#62966 = LINE ( 'NONE', #19710, #45308 ) ;
#62968 = VERTEX_POINT ( 'NONE', #39160 ) ;
#62967 = EDGE_CURVE ( 'NONE', #18071, #63625, #55670, .T. ) ;
#62969 = CARTESIAN_POINT ( 'NONE',  ( -77.71801202538871678, 23.03755222122951452, 72.21756683605353544 ) ) ;
#62970 = DIRECTION ( 'NONE',  ( -1.387778780781445429E-16, 1.000000000000000000, 3.081487911019577365E-33 ) ) ;
#62971 = DIRECTION ( 'NONE',  ( -1.000000000000000000, 0.000000000000000000, 0.000000000000000000 ) ) ;
#62972 = DIRECTION ( 'NONE',  ( 0.000000000000000000, 0.000000000000000000, -1.000000000000000000 ) ) ;
#62973 = EDGE_CURVE ( 'NONE', #14060, #48814, #4242, .T. ) ;
#62974 = CARTESIAN_POINT ( 'NONE',  ( -118.4753258120605324, -170.0000000000000000, -95.00000000000133582 ) ) ;
#62975 = CARTESIAN_POINT ( 'NONE',  ( -105.8879245385188455, 35.79035667534149212, -9.077219941719809171 ) ) ;
#62976 = ORIENTED_EDGE ( 'NONE', *, *, #32018, .F. ) ;
#62977 = CARTESIAN_POINT ( 'NONE',  ( -1.148430018225554461, 500.0000000000000000, -91.64566090791306863 ) ) ;
#62978 = CARTESIAN_POINT ( 'NONE',  ( 200.5226609475754458, 100.7898801217142051, -91.27370320419781535 ) ) ;
#62979 = EDGE_LOOP ( 'NONE', ( #3100, #32460, #43351, #64700, #12320, #52851, #50815 ) ) ;
#62980 = ORIENTED_EDGE ( 'NONE', *, *, #1755, .F. ) ;
#62981 = CARTESIAN_POINT ( 'NONE',  ( -153.5002794404625774, 67.64160439471096709, 31.86792471940524152 ) ) ;
#62982 = CARTESIAN_POINT ( 'NONE',  ( 59.29615173875419742, 11.84060224810188622, -49.73800052251814208 ) ) ;
#62983 = CARTESIAN_POINT ( 'NONE',  ( 175.8855729601531550, 73.50624012737692681, -22.30791473185340834 ) ) ;
#62984 = LINE ( 'NONE', #47830, #9178 ) ;
#62985 = FACE_OUTER_BOUND ( 'NONE', #67217, .T. ) ;
#62986 = EDGE_CURVE ( 'NONE', #27414, #30796, #43527, .T. ) ;
#62987 = CIRCLE ( 'NONE', #9119, 21.00000000000000355 ) ;
#62988 = ORIENTED_EDGE ( 'NONE', *, *, #33758, .F. ) ;
#62989 = CARTESIAN_POINT ( 'NONE',  ( -31.43908319763709969, 9.591432048623767415, -50.31719736520186359 ) ) ;
#62990 = ORIENTED_EDGE ( 'NONE', *, *, #62824, .T. ) ;
#62991 = CARTESIAN_POINT ( 'NONE',  ( 20.74185656603722450, 7.717159106492252896, -48.67200694907381120 ) ) ;
#62992 = CARTESIAN_POINT ( 'NONE',  ( -147.7895256390024485, 64.04409735547017135, 45.57579272523850022 ) ) ;
#62993 = VECTOR ( 'NONE', #2449, 1000.000000000000000 ) ;
#62994 = CARTESIAN_POINT ( 'NONE',  ( 212.0739503583954217, 117.0412199804969759, 35.30913288153361407 ) ) ;
#62995 = CARTESIAN_POINT ( 'NONE',  ( 11.46041170590452296, 6.400589304860417883, -90.56819552826038944 ) ) ;
#62996 = PRODUCT ( 'hex bolt gradeb_iso_ISO 4015 - M10 x 40 x 26-N', 'hex bolt gradeb_iso_ISO 4015 - M10 x 40 x 26-N', '', ( #24850 ) ) ;
#62997 = VECTOR ( 'NONE', #25582, 1000.000000000000000 ) ;
#62998 = EDGE_LOOP ( 'NONE', ( #56831, #39973, #43375, #57528, #57180, #12677, #52752, #66965, #23548 ) ) ;
#62999 = B_SPLINE_CURVE_WITH_KNOTS ( 'NONE', 3,
 ( #13026, #39745, #34828, #45011, #46054, #24619, #19325, #55928, #7745, #18982, #8436, #2121, #19670, #51349, #24270, #14406, #61201, #35509, #45718, #40776, #29885, #62231, #34488, #14049, #56971, #18287, #28853, #30236, #35857, #56612, #8789, #51687, #29194, #8079, #18635, #3494, #50304, #46395, #67874, #41129, #62597, #61548, #57311, #23573 ),
 .UNSPECIFIED., .F., .F.,
 ( 4, 2, 2, 2, 2, 2, 2, 2, 2, 2, 2, 2, 2, 2, 2, 2, 2, 2, 2, 2, 2, 4 ),
 ( 0.000000000000000000, 0.003360573201437662503, 0.004200716501797043326, 0.005040859802156424582, 0.006721146402875118574, 0.007561289703234486820, 0.008401433003593854199, 0.009241576303953223312, 0.01008171960431258896, 0.01176200620503132545, 0.01260214950539068415, 0.01344229280575004286, 0.01428243610610940330, 0.01512257940646876200, 0.01680286600718750023, 0.01764300930754687455, 0.01848315260790624887, 0.02016343920862501138, 0.02184372580934377736, 0.02352401241006254334, 0.02520429901078130933, 0.02688458561150007531 ),
 .UNSPECIFIED. ) ;
#63000 = ORIENTED_EDGE ( 'NONE', *, *, #8511, .F. ) ;
#63001 = CARTESIAN_POINT ( 'NONE',  ( 114.8387163486435298, -21.96381563589838493, -1.302408292197374307 ) ) ;
#63002 = CARTESIAN_POINT ( 'NONE',  ( -131.5919238272131508, 51.59099727820048997, 86.92280933128381548 ) ) ;
#63003 = CARTESIAN_POINT ( 'NONE',  ( 35.65622260226240314, 8.964590916200311455, -63.46208756248341842 ) ) ;
#63004 = CARTESIAN_POINT ( 'NONE',  ( -178.5848962563133568, 94.99295350784004199, 16.63922201400802692 ) ) ;
#63005 = CARTESIAN_POINT ( 'NONE',  ( 8.402653425627045536, 6.376553021891479212, 92.54943276849337508 ) ) ;
#63006 = VECTOR ( 'NONE', #38373, 1000.000000000000000 ) ;
#63007 = CARTESIAN_POINT ( 'NONE',  ( 84.73231936899554739, 18.78199960571075877, -77.43798840702864084 ) ) ;
#63008 = ORIENTED_EDGE ( 'NONE', *, *, #14702, .F. ) ;
#63009 = LINE ( 'NONE', #20102, #29192 ) ;
#63010 = CARTESIAN_POINT ( 'NONE',  ( -102.2801239173131052, 32.78103895658058065, 72.36362509687883460 ) ) ;
#63011 = ORIENTED_EDGE ( 'NONE', *, *, #63696, .F. ) ;
#63012 = CARTESIAN_POINT ( 'NONE',  ( -83.51052366780672287, 24.22613130369188639, 16.80462344529878749 ) ) ;
#63013 = EDGE_LOOP ( 'NONE', ( #11077, #10954, #23999, #37304 ) ) ;
#63014 = CARTESIAN_POINT ( 'NONE',  ( -55.54036735998997898, 15.85474597822064702, -8.371773407996174754 ) ) ;
#63015 = ORIENTED_EDGE ( 'NONE', *, *, #31131, .T. ) ;
#63016 = ORIENTED_EDGE ( 'NONE', *, *, #21815, .T. ) ;
#63017 = CARTESIAN_POINT ( 'NONE',  ( 12.46704290855393182, 6.417105965824391411, -49.74798076428597682 ) ) ;
#63018 = CARTESIAN_POINT ( 'NONE',  ( -178.5835577246388084, 93.42126246260829703, 60.02133511208158012 ) ) ;
#63019 = CARTESIAN_POINT ( 'NONE',  ( 20.74852474914887779, 6.709938988646747760, 16.31688092656622757 ) ) ;
#63020 = ORIENTED_EDGE ( 'NONE', *, *, #22308, .F. ) ;
#63021 = EDGE_CURVE ( 'NONE', #21253, #64530, #61643, .T. ) ;
#63022 = LINE ( 'NONE', #41913, #64885 ) ;
#63023 = CARTESIAN_POINT ( 'NONE',  ( 178.1888264190354789, 77.13727704498029425, -63.63756854808438845 ) ) ;
#63024 = LINE ( 'NONE', #14831, #41534 ) ;
#63025 = CARTESIAN_POINT ( 'NONE',  ( 102.8111940033034415, 25.59308899183601582, -42.38074508319384393 ) ) ;
#63026 = DIRECTION ( 'NONE',  ( -0.1342332658176522420, -0.9909497617679352555, 0.000000000000000000 ) ) ;
#63027 = DIRECTION ( 'NONE',  ( 1.000000000000000000, 0.000000000000000000, 0.000000000000000000 ) ) ;
#63028 = ORIENTED_EDGE ( 'NONE', *, *, #3920, .T. ) ;
#63029 = MANIFOLD_SOLID_BREP ( 'Cut-Extrude4', #24962 ) ;
#63030 = AXIS2_PLACEMENT_3D ( 'NONE', #69300, #21127, #42571 ) ;
#63031 = DIRECTION ( 'NONE',  ( 0.3978782902816504485, 0.9174375763581196219, -0.001076851285082543489 ) ) ;
#63032 = CARTESIAN_POINT ( 'NONE',  ( 39.40195752203892710, 8.409560354027389550, 18.06928371549960133 ) ) ;
#63034 = CARTESIAN_POINT ( 'NONE',  ( 173.6007744016332595, 72.73482010729023273, 10.54590781376938580 ) ) ;
#63033 = AXIS2_PLACEMENT_3D ( 'NONE', #30059, #13863, #51513 ) ;
#63035 = PLANE ( 'NONE',  #21119 ) ;
#63036 = PLANE ( 'NONE',  #2928 ) ;
#63037 = CARTESIAN_POINT ( 'NONE',  ( 137.8342272233871881, 43.87828770902297748, -90.84184450531311938 ) ) ;
#63038 = CARTESIAN_POINT ( 'NONE',  ( -157.0077369422018023, 70.81157624963285002, 11.09516931919394978 ) ) ;
#63039 = PLANE ( 'NONE',  #60878 ) ;
#63040 = ADVANCED_FACE ( 'NONE', ( #56716 ), #27820, .T. ) ;
#63042 = CARTESIAN_POINT ( 'NONE',  ( 207.8407634284390895, 112.5209879629464211, 43.53050796622361673 ) ) ;
#63041 = AXIS2_PLACEMENT_3D ( 'NONE', #13538, #57482, #34993 ) ;
#63043 = VECTOR ( 'NONE', #8577, 1000.000000000000114 ) ;
#63044 = CARTESIAN_POINT ( 'NONE',  ( -82.32006615997346444, 24.83050031643766431, 58.19495574293904383 ) ) ;
#63045 = CARTESIAN_POINT ( 'NONE',  ( -109.7647482398635361, 36.74843029291201191, 38.56660667589553526 ) ) ;
#63046 = ORIENTED_EDGE ( 'NONE', *, *, #64477, .T. ) ;
#63047 = CONTEXT_DEPENDENT_SHAPE_REPRESENTATION ( #8055, #24945 ) ;
#63048 = CARTESIAN_POINT ( 'NONE',  ( -47.55539076061677406, 13.83217677045059268, 91.88810249661966623 ) ) ;
#63049 = ORIENTED_EDGE ( 'NONE', *, *, #66746, .F. ) ;
#63050 = FACE_OUTER_BOUND ( 'NONE', #35079, .T. ) ;
#63051 = VERTEX_POINT ( 'NONE', #56026 ) ;
#63052 = CARTESIAN_POINT ( 'NONE',  ( 21.75198946226450758, 7.772524967554916842, -74.43766794452670865 ) ) ;
#63053 = FILL_AREA_STYLE_COLOUR ( '', #64195 ) ;
#63054 = FACE_OUTER_BOUND ( 'NONE', #33520, .T. ) ;
#63055 = ADVANCED_FACE ( 'NONE', ( #7838 ), #67291, .F. ) ;
#63056 = CARTESIAN_POINT ( 'NONE',  ( -737.6000277536880958, -694.2189502691660437, 0.000000000000000000 ) ) ;
#63057 = VECTOR ( 'NONE', #42546, 1000.000000000000000 ) ;
#63058 = CARTESIAN_POINT ( 'NONE',  ( 140.0820590176526252, 46.51134312115247837, -47.71347409872789314 ) ) ;
#63059 = CARTESIAN_POINT ( 'NONE',  ( 207.0312524359575832, 111.3509507522488917, -90.37915150709905276 ) ) ;
#63060 = CARTESIAN_POINT ( 'NONE',  ( 12.03162622199373111, 7.415834979634797541, -36.52294849145773270 ) ) ;
#63061 = DIRECTION ( 'NONE',  ( 0.000000000000000000, 0.000000000000000000, -1.000000000000000000 ) ) ;
#63062 = CARTESIAN_POINT ( 'NONE',  ( -122.1940143064357187, 45.29738883755585732, -9.041013927513500192 ) ) ;
#63063 = ORIENTED_EDGE ( 'NONE', *, *, #66253, .T. ) ;
#63064 = EDGE_LOOP ( 'NONE', ( #29071, #19733, #30132 ) ) ;
#63065 = CARTESIAN_POINT ( 'NONE',  ( 173.9599793006471486, 73.07129831195001657, 92.85047428432565653 ) ) ;
#63066 = CARTESIAN_POINT ( 'NONE',  ( -59.09450113343241640, 27.07101652673493319, 40.00000000000003553 ) ) ;
#63067 = CARTESIAN_POINT ( 'NONE',  ( -25.50312845906833559, 8.692070753302667541, -74.25253205409154589 ) ) ;
#63068 = EDGE_CURVE ( 'NONE', #56795, #21961, #57400, .T. ) ;
#63069 = EDGE_CURVE ( 'NONE', #65127, #16895, #51781, .T. ) ;
#63070 = CARTESIAN_POINT ( 'NONE',  ( 13.37366753069833258, 6.435102282077985514, 3.552458417556365156 ) ) ;
#63071 = PLANE ( 'NONE',  #51390 ) ;
#63072 = FACE_OUTER_BOUND ( 'NONE', #41473, .T. ) ;
#63073 = CARTESIAN_POINT ( 'NONE',  ( 208.5884523568772693, 113.6152425727545250, 16.28900457481658393 ) ) ;
#63074 =( LENGTH_UNIT ( ) NAMED_UNIT ( * ) SI_UNIT ( .MILLI., .METRE. ) );
#63075 = CARTESIAN_POINT ( 'NONE',  ( -175.9970298498767534, 90.38640259140139221, -49.15178234214096875 ) ) ;
#63076 = CARTESIAN_POINT ( 'NONE',  ( -430.1627218934917209, 400.0000000000021600, 91.05029585799256608 ) ) ;
#63077 = CARTESIAN_POINT ( 'NONE',  ( -24.18270484670773612, 9.527492911955590671, 66.52113223989842083 ) ) ;
#63078 = LINE ( 'NONE', #41623, #18355 ) ;
#63079 = LINE ( 'NONE', #3304, #1838 ) ;
#63080 = SHAPE_REPRESENTATION ( 'shaft', ( #66832 ), #32049 ) ;
#63081 = ORIENTED_EDGE ( 'NONE', *, *, #12539, .T. ) ;
#63082 = CARTESIAN_POINT ( 'NONE',  ( 141.9165763529819344, -2.000000000000001776, 108.9999999999999858 ) ) ;
#63083 = DIRECTION ( 'NONE',  ( 0.000000000000000000, 1.000000000000000000, -0.000000000000000000 ) ) ;
#63084 = VECTOR ( 'NONE', #23726, 1000.000000000000000 ) ;
#63085 = CARTESIAN_POINT ( 'NONE',  ( 41.66904755831210849, -9.150666335777657423E-14, 0.000000000000000000 ) ) ;
#63086 = CARTESIAN_POINT ( 'NONE',  ( -106.4728934171454284, 36.10295170132727804, -75.58225694355543567 ) ) ;
#63087 = DIRECTION ( 'NONE',  ( 1.000000000000000000, 0.000000000000000000, 0.000000000000000000 ) ) ;
#63088 = DIRECTION ( 'NONE',  ( -0.000000000000000000, 1.000000000000000000, -0.000000000000000000 ) ) ;
#63089 = CARTESIAN_POINT ( 'NONE',  ( -102.2801239173131194, -170.0000000000000000, -69.35912785543959558 ) ) ;
#63090 = VECTOR ( 'NONE', #51077, 1000.000000000000000 ) ;
#63091 = ORIENTED_EDGE ( 'NONE', *, *, #59984, .F. ) ;
#63092 = CARTESIAN_POINT ( 'NONE',  ( 59.29597493004737174, 11.84030339376940688, 16.99923005275914534 ) ) ;
#63093 = CARTESIAN_POINT ( 'NONE',  ( -61.75629144857965258, 16.58190704077737720, 68.03453561796777649 ) ) ;
#63094 = VERTEX_POINT ( 'NONE', #62691 ) ;
#63095 = AXIS2_PLACEMENT_3D ( 'NONE', #29290, #50743, #24020 ) ;
#63096 = CIRCLE ( 'NONE', #2450, 24.99999999999985434 ) ;
#63097 = ORIENTED_EDGE ( 'NONE', *, *, #33944, .F. ) ;
#63098 = CARTESIAN_POINT ( 'NONE',  ( 46.48565096083556369, 10.45589966334459575, 88.61677544424188113 ) ) ;
#63099 = CARTESIAN_POINT ( 'NONE',  ( -177.1540936177023013, 91.73126115633630207, -75.39503670027723103 ) ) ;
#63100 = PLANE ( 'NONE',  #49336 ) ;
#63101 = EDGE_LOOP ( 'NONE', ( #3600, #3826, #5879, #64424 ) ) ;
#63102 = CARTESIAN_POINT ( 'NONE',  ( -20.63749999999999574, 2.936090700955778569E-15, 23.97499999999999787 ) ) ;
#63103 = CARTESIAN_POINT ( 'NONE',  ( 63.72039997003725631, -12.83396383267754537, 40.00000000000003553 ) ) ;
#63104 = CIRCLE ( 'NONE', #32772, 65.00000000000000000 ) ;
#63105 = CARTESIAN_POINT ( 'NONE',  ( 55.51637278631174155, 12.08345311280959855, -43.73033833359424705 ) ) ;
#63106 = CARTESIAN_POINT ( 'NONE',  ( -86.11230725916333029, 26.39026888680170657, 36.88449808153552567 ) ) ;
#63107 = CARTESIAN_POINT ( 'NONE',  ( -24.71604178686819253, 9.599501655372943532, -19.30609868970467957 ) ) ;
#63108 = CARTESIAN_POINT ( 'NONE',  ( 92.19920907511536257, 21.39700525884453342, 32.16603705074736297 ) ) ;
#63109 = B_SPLINE_CURVE_WITH_KNOTS ( 'NONE', 3,
 ( #11805, #58014, #54714, #22716 ),
 .UNSPECIFIED., .F., .F.,
 ( 4, 4 ),
 ( 9.900409498990251444E-07, 0.05658314289920113316 ),
 .UNSPECIFIED. ) ;
#63110 = EDGE_CURVE ( 'NONE', #18323, #564, #63022, .T. ) ;
#63111 = ORIENTED_EDGE ( 'NONE', *, *, #59527, .F. ) ;
#63113 = EDGE_CURVE ( 'NONE', #44678, #5653, #8693, .T. ) ;
#63112 = SURFACE_STYLE_USAGE ( .BOTH. , #4026 ) ;
#63114 = CARTESIAN_POINT ( 'NONE',  ( 8.288104306525687193, 6.376394648992965486, 63.87267987369663302 ) ) ;
#63115 = B_SPLINE_CURVE_WITH_KNOTS ( 'NONE', 3,
 ( #13691, #62923, #56598, #40766, #14724, #4517, #51675, #20344, #52015, #30225, #15073, #25647, #57299, #30564, #25301, #3829, #24946, #36187, #41120, #46382, #57646, #14037, #35495, #52692, #3152, #67861, #47077, #67183, #41810, #9455, #56957, #30916, #62217, #61864, #8421, #35145, #62579, #19657, #14395, #36533 ),
 .UNSPECIFIED., .F., .F.,
 ( 4, 2, 2, 2, 2, 2, 2, 2, 2, 2, 2, 2, 2, 2, 2, 2, 2, 2, 2, 4 ),
 ( 0.02454308262169000582, 0.02608670964102885112, 0.02685852315069829285, 0.02763033666036773459, 0.02917396367970661458, 0.02994577718937605978, 0.03071759069904549458, 0.03226121771838433294, 0.03303303122805375386, 0.03380484473772318171, 0.03534847175706200967, 0.03689209877640083068, 0.03843572579573965864, 0.03997935281507848659, 0.04152297983441731455, 0.04306660685375614250, 0.04461023387309497046, 0.04615386089243379841, 0.04769748791177262637, 0.04924111493111145432 ),
 .UNSPECIFIED. ) ;
#63116 = CARTESIAN_POINT ( 'NONE',  ( -27.49195330402089255, 9.993776132065303131, 31.33447323685886587 ) ) ;
#63117 = CARTESIAN_POINT ( 'NONE',  ( 203.1423857108907782, 105.9238244286949850, 29.36013609250961309 ) ) ;
#63118 = CARTESIAN_POINT ( 'NONE',  ( -72.54813618488350357, 21.15114325868153244, 87.25760088006373394 ) ) ;
#63120 = ORIENTED_EDGE ( 'NONE', *, *, #49564, .T. ) ;
#63119 = DIRECTION ( 'NONE',  ( -0.000000000000000000, -0.000000000000000000, -1.000000000000000000 ) ) ;
#63121 = DIRECTION ( 'NONE',  ( 0.000000000000000000, 0.000000000000000000, 1.000000000000000000 ) ) ;
#63122 = ORIENTED_EDGE ( 'NONE', *, *, #49375, .F. ) ;
#63123 = ORIENTED_EDGE ( 'NONE', *, *, #53399, .T. ) ;
#63124 = CARTESIAN_POINT ( 'NONE',  ( 117.6924004117966689, 33.61107268965020722, -71.28084340972505117 ) ) ;
#63125 = DIRECTION ( 'NONE',  ( -0.8118923937861950435, -0.5838071093367415143, 0.000000000000000000 ) ) ;
#63126 = CARTESIAN_POINT ( 'NONE',  ( 197.5334904971816172, 97.00846725096926093, -68.42925186292004014 ) ) ;
#63127 = EDGE_CURVE ( 'NONE', #31978, #24127, #64396, .T. ) ;
#63128 = CARTESIAN_POINT ( 'NONE',  ( -38.93847286785603501, 11.96870349976817494, 64.05428266636177170 ) ) ;
#63129 = EDGE_CURVE ( 'NONE', #45635, #67175, #67178, .T. ) ;
#63130 = CARTESIAN_POINT ( 'NONE',  ( -38.78626392836186909, -170.0000000000000000, -95.00000000000133582 ) ) ;
#63131 = CARTESIAN_POINT ( 'NONE',  ( -85.35172689181706573, 26.07142112926218047, -19.20697335453129284 ) ) ;
#63132 = DIRECTION ( 'NONE',  ( 1.000000000000000000, 0.000000000000000000, 0.000000000000000000 ) ) ;
#63133 = DIRECTION ( 'NONE',  ( -0.000000000000000000, -1.000000000000000000, -0.000000000000000000 ) ) ;
#63134 = ORIENTED_EDGE ( 'NONE', *, *, #34722, .F. ) ;
#63135 = VERTEX_POINT ( 'NONE', #32400 ) ;
#63136 = EDGE_CURVE ( 'NONE', #22403, #56265, #59458, .T. ) ;
#63137 = CARTESIAN_POINT ( 'NONE',  ( -108.1180879163843116, 36.99199941971030370, 15.90925667645064578 ) ) ;
#63138 = AXIS2_PLACEMENT_3D ( 'NONE', #13361, #34818, #24265 ) ;
#63139 = CARTESIAN_POINT ( 'NONE',  ( -85.96384504792885650, 26.32782846176032621, -40.86557644392104294 ) ) ;
#63140 = CARTESIAN_POINT ( 'NONE',  ( 164.6499013411308283, 63.45576988183551492, 65.93988476214543937 ) ) ;
#63141 = EDGE_CURVE ( 'NONE', #26680, #27057, #12120, .T. ) ;
#63142 = DIRECTION ( 'NONE',  ( 0.000000000000000000, 0.000000000000000000, 1.000000000000000000 ) ) ;
#63143 = CIRCLE ( 'NONE', #64232, 65.36598343705435354 ) ;
#63144 = CARTESIAN_POINT ( 'NONE',  ( -60.57719060482967421, 27.78504214373295511, 34.48241823988800547 ) ) ;
#63145 = LINE ( 'NONE', #35729, #9039 ) ;
#63146 = CARTESIAN_POINT ( 'NONE',  ( 159.2389084450350367, 59.03884018680375334, -63.16658458358803330 ) ) ;
#63147 = ORIENTED_EDGE ( 'NONE', *, *, #373, .F. ) ;
#63148 = ORIENTED_EDGE ( 'NONE', *, *, #2462, .T. ) ;
#63149 = ORIENTED_EDGE ( 'NONE', *, *, #37558, .T. ) ;
#63150 = AXIS2_PLACEMENT_3D ( 'NONE', #32336, #48821, #16492 ) ;
#63151 = STYLED_ITEM ( 'NONE', ( #29183 ), #18150 ) ;
#63152 = CARTESIAN_POINT ( 'NONE',  ( -34.39004539972345498, 0.000000000000000000, 5.000000000000000000 ) ) ;
#63153 = CARTESIAN_POINT ( 'NONE',  ( 38.43102714813442589, 9.298961820315049920, -50.57286685989200947 ) ) ;
#63154 = CARTESIAN_POINT ( 'NONE',  ( 106.2372751229154773, -21.75101418369301598, 3.308700176549400851 ) ) ;
#63155 = EDGE_CURVE ( 'NONE', #53816, #46344, #43970, .T. ) ;
#63156 = CIRCLE ( 'NONE', #32817, 21.02500000000000213 ) ;
#63157 = MANIFOLD_SOLID_BREP ( 'Boss-Extrude1', #19320 ) ;
#63158 = CLOSED_SHELL ( 'NONE', ( #57169, #37380, #55155, #57810, #31158, #6662, #768, #45961, #26923 ) ) ;
#63159 = CARTESIAN_POINT ( 'NONE',  ( -31.92572261726340344, 10.69135962481465540, -77.16174795566556099 ) ) ;
#63160 = EDGE_CURVE ( 'NONE', #4775, #13320, #23757, .T. ) ;
#63161 = LINE ( 'NONE', #2426, #24046 ) ;
#63162 = EDGE_CURVE ( 'NONE', #41559, #8207, #42600, .T. ) ;
#63163 = EDGE_CURVE ( 'NONE', #14371, #41081, #26774, .T. ) ;
#63164 = CARTESIAN_POINT ( 'NONE',  ( 36.31593203568480988, 8.028139509847024513, 57.41831045774998188 ) ) ;
#63165 = CARTESIAN_POINT ( 'NONE',  ( 8.670103207226935282, 6.377073801252348240, -18.58750088859477856 ) ) ;
#63166 = CARTESIAN_POINT ( 'NONE',  ( 22.15926701483429895, 7.796117250416237709, 14.63516493621701642 ) ) ;
#63167 = DIRECTION ( 'NONE',  ( 0.000000000000000000, 1.000000000000000000, -0.000000000000000000 ) ) ;
#63168 = CARTESIAN_POINT ( 'NONE',  ( -122.3963566076408114, 44.23346594671846788, 4.624121492655477894 ) ) ;
#63169 = CARTESIAN_POINT ( 'NONE',  ( 39.40195752203892710, 8.409560354027385998, -8.775266874964067654 ) ) ;
#63170 = CARTESIAN_POINT ( 'NONE',  ( 126.3580543567275072, 37.07735301062816546, -16.37485516677961073 ) ) ;
#63171 = CARTESIAN_POINT ( 'NONE',  ( 18.43272992546528855, 7.606837839440253823, -9.151768092893727058 ) ) ;
#63172 = CARTESIAN_POINT ( 'NONE',  ( 11.81843724556921060, 7.412394300769732602, 17.03812180473721938 ) ) ;
#63173 = VERTEX_POINT ( 'NONE', #21157 ) ;
#63174 = DIRECTION ( 'NONE',  ( 0.000000000000000000, 0.000000000000000000, 1.000000000000000000 ) ) ;
#63175 = APPLICATION_PROTOCOL_DEFINITION ( 'draft international standard', 'automotive_design', 1998, #26937 ) ;
#63176 = DIRECTION ( 'NONE',  ( -0.000000000000000000, 1.000000000000000000, -0.000000000000000000 ) ) ;
#63177 = LINE ( 'NONE', #68451, #59005 ) ;
#63178 = CARTESIAN_POINT ( 'NONE',  ( -109.6752351740181695, 37.84903014964773860, -41.23783467770100941 ) ) ;
#63179 = CARTESIAN_POINT ( 'NONE',  ( 188.2962140587030149, 87.71627202537843004, -45.80397896477450814 ) ) ;
#63180 = ORIENTED_EDGE ( 'NONE', *, *, #15034, .T. ) ;
#63181 = VERTEX_POINT ( 'NONE', #53825 ) ;
#63182 = B_SPLINE_CURVE_WITH_KNOTS ( 'NONE', 3,
 ( #28521, #55595, #29558, #49965, #1801, #23942, #29219, #66870, #67223, #51022, #23256, #2832, #18313, #13728, #2146, #65823, #7769, #39419, #8107, #13391, #12693, #61904, #35187, #34513, #18669, #44336, #40460, #34159, #17974, #49607, #45039, #24300, #7426, #28878, #50329, #17617, #56640, #66182, #23601, #22893, #56289, #66521, #39769, #12343, #19008, #60868, #61228, #13055 ),
 .UNSPECIFIED., .F., .F.,
 ( 4, 2, 2, 2, 2, 2, 2, 2, 2, 2, 2, 2, 2, 2, 2, 2, 2, 2, 2, 2, 2, 2, 2, 4 ),
 ( 0.02698595842317763269, 0.02784423243973405820, 0.02870250645629048025, 0.03041905448940323414, 0.03127732850595960762, 0.03213560252251598803, 0.03385215055562873498, 0.03471042457218508070, 0.03556869858874141949, 0.03728524662185411093, 0.03814352063841044971, 0.03900179465496678849, 0.03986006867152312727, 0.04071834268807946605, 0.04157661670463580483, 0.04243489072119214361, 0.04415143875430481424, 0.04500971277086115996, 0.04586798678741749180, 0.04758453482053018324, 0.04930108285364286774, 0.05101763088675554531, 0.05273417891986822981, 0.05445072695298091431 ),
 .UNSPECIFIED. ) ;
#63183 = CARTESIAN_POINT ( 'NONE',  ( -142.0685766576042397, 58.11789490499572963, -14.35908353972402551 ) ) ;
#63184 = CARTESIAN_POINT ( 'NONE',  ( 199.3764470687682433, 100.9548044849099142, 15.15399381071274831 ) ) ;
#63185 = ORIENTED_EDGE ( 'NONE', *, *, #53796, .F. ) ;
#63186 = CARTESIAN_POINT ( 'NONE',  ( 113.8568724296587789, 30.58972477291343850, 57.36639540863109232 ) ) ;
#63187 = ORIENTED_EDGE ( 'NONE', *, *, #57827, .T. ) ;
#63188 = CARTESIAN_POINT ( 'NONE',  ( -61.77164219855450966, 17.63686644795249592, 14.34267326658022235 ) ) ;
#63189 = CARTESIAN_POINT ( 'NONE',  ( 126.9201538765324386, 37.39093565120715112, 39.87409765458102129 ) ) ;
#63190 = CARTESIAN_POINT ( 'NONE',  ( -78.66644367742109978, 22.32174330031318732, -50.11545063171791270 ) ) ;
#63191 = VECTOR ( 'NONE', #69511, 1000.000000000000000 ) ;
#63192 = CARTESIAN_POINT ( 'NONE',  ( -95.88718821240196633, 29.65015105908826953, 34.08905749573029453 ) ) ;
#63193 = LINE ( 'NONE', #30842, #10300 ) ;
#63194 = AXIS2_PLACEMENT_3D ( 'NONE', #41749, #63209, #472 ) ;
#63196 = ORIENTED_EDGE ( 'NONE', *, *, #50688, .T. ) ;
#63195 = DIRECTION ( 'NONE',  ( -0.000000000000000000, 1.000000000000000000, -0.000000000000000000 ) ) ;
#63197 = CARTESIAN_POINT ( 'NONE',  ( 2.999999999999995559, 0.000000000000000000, 0.000000000000000000 ) ) ;
#63198 = EDGE_LOOP ( 'NONE', ( #18741, #15984, #59076, #40007 ) ) ;
#63199 = VECTOR ( 'NONE', #68171, 1000.000000000000000 ) ;
#63200 = ORIENTED_EDGE ( 'NONE', *, *, #16907, .F. ) ;
#63202 = EDGE_CURVE ( 'NONE', #14330, #9201, #54169, .T. ) ;
#63201 = CARTESIAN_POINT ( 'NONE',  ( -167.4844853368928739, 82.52074065752738363, 6.523106101700750337 ) ) ;
#63203 = CARTESIAN_POINT ( 'NONE',  ( 133.8566784816069344, -170.0000000000000000, -97.21241211332302612 ) ) ;
#63204 = CARTESIAN_POINT ( 'NONE',  ( -175.9970298498766965, 90.38640259140137800, -22.30723175167727490 ) ) ;
#63206 = ORIENTED_EDGE ( 'NONE', *, *, #13653, .T. ) ;
#63205 = CARTESIAN_POINT ( 'NONE',  ( -131.3096895243910751, 51.39228038925231346, 70.17557077602670290 ) ) ;
#63207 = CARTESIAN_POINT ( 'NONE',  ( -109.5800870510459646, 37.79624625667730697, 93.46020534934932300 ) ) ;
#63208 = VECTOR ( 'NONE', #4111, 1000.000000000000000 ) ;
#63209 = DIRECTION ( 'NONE',  ( -0.000000000000000000, -0.000000000000000000, -1.000000000000000000 ) ) ;
#63210 = ORIENTED_EDGE ( 'NONE', *, *, #69545, .F. ) ;
#63211 = CARTESIAN_POINT ( 'NONE',  ( -60.97011009284708649, 16.34812508431679490, -11.23730993338677031 ) ) ;
#63212 = EDGE_CURVE ( 'NONE', #34656, #62854, #64751, .T. ) ;
#63213 = LINE ( 'NONE', #57592, #26371 ) ;
#63214 = CARTESIAN_POINT ( 'NONE',  ( 56.00903540737504471, 11.15594382527104500, -94.20234774883739703 ) ) ;
#63215 = DIRECTION ( 'NONE',  ( -1.000000000000000000, -0.000000000000000000, -0.000000000000000000 ) ) ;
#63216 = CARTESIAN_POINT ( 'NONE',  ( 69.83617901654359628, 15.39919709983075613, -73.19441325359579764 ) ) ;
#63217 = ORIENTED_EDGE ( 'NONE', *, *, #17127, .F. ) ;
#63218 = ADVANCED_FACE ( 'NONE', ( #38013 ), #22254, .T. ) ;
#63219 = ORIENTED_EDGE ( 'NONE', *, *, #59931, .T. ) ;
#63220 = DIRECTION ( 'NONE',  ( -0.000000000000000000, -0.000000000000000000, -1.000000000000000000 ) ) ;
#63221 = DIRECTION ( 'NONE',  ( -1.000000000000000000, 0.000000000000000000, 0.000000000000000000 ) ) ;
#63222 = DIRECTION ( 'NONE',  ( 0.01527021686369653929, 0.000000000000000000, 0.9998834034410890581 ) ) ;
#63223 = CARTESIAN_POINT ( 'NONE',  ( 36.85262215550149278, -53.56030941157680303, 170.0000000000000000 ) ) ;
#63224 = CARTESIAN_POINT ( 'NONE',  ( -71.22896441287284119, 20.69091426169410042, 36.91910425864390533 ) ) ;
#63225 = DIRECTION ( 'NONE',  ( -1.000000000000000000, 0.000000000000000000, 0.000000000000000000 ) ) ;
#63226 = CARTESIAN_POINT ( 'NONE',  ( -200.0000000000000000, 2.449293598294706434E-14, 10.00000000000000000 ) ) ;
#63227 = CARTESIAN_POINT ( 'NONE',  ( -4.250000000000000000, 5.204748896376250699E-16, -8.949444346342716017 ) ) ;
#63228 = CARTESIAN_POINT ( 'NONE',  ( -166.2028193222418793, 79.74385139484276408, -71.96685162649892220 ) ) ;
#63229 = EDGE_LOOP ( 'NONE', ( #65148, #3579, #22027, #58635 ) ) ;
#63230 = CARTESIAN_POINT ( 'NONE',  ( -109.0297561673456102, 36.34391931706016976, -12.38998052533776040 ) ) ;
#63231 = ORIENTED_EDGE ( 'NONE', *, *, #69567, .F. ) ;
#63232 = CARTESIAN_POINT ( 'NONE',  ( -37.79823708645146496, 10.72197716414928692, 6.888035153445309255 ) ) ;
#63233 = FACE_OUTER_BOUND ( 'NONE', #30761, .T. ) ;
#63234 = DIRECTION ( 'NONE',  ( 1.000000000000000000, 0.000000000000000000, 0.000000000000000000 ) ) ;
#63235 = FACE_OUTER_BOUND ( 'NONE', #13130, .T. ) ;
#63236 = CARTESIAN_POINT ( 'NONE',  ( 110.2429982417149574, -170.0000000000000000, 90.80031538666469260 ) ) ;
#63237 = DIRECTION ( 'NONE',  ( -0.000000000000000000, -0.000000000000000000, -1.000000000000000000 ) ) ;
#63238 = DIRECTION ( 'NONE',  ( 0.000000000000000000, 0.000000000000000000, -1.000000000000000000 ) ) ;
#63239 = CARTESIAN_POINT ( 'NONE',  ( -13.45956523846224506, 8.333781915634244086, -47.87459002919935358 ) ) ;
#63240 = VECTOR ( 'NONE', #52150, 1000.000000000000000 ) ;
#63241 = LINE ( 'NONE', #41095, #14651 ) ;
#63242 = EDGE_CURVE ( 'NONE', #6906, #32464, #60515, .T. ) ;
#63243 = ORIENTED_EDGE ( 'NONE', *, *, #12144, .F. ) ;
#63244 = CIRCLE ( 'NONE', #23978, 21.50000000000000000 ) ;
#63245 = CARTESIAN_POINT ( 'NONE',  ( -121.5684475810873266, 44.90063534192884731, -89.97182396522346437 ) ) ;
#63246 = VERTEX_POINT ( 'NONE', #23588 ) ;
#63247 = CARTESIAN_POINT ( 'NONE',  ( 58.09877917144279280, 12.61383386832655340, 58.47304198809774078 ) ) ;
#63248 = CARTESIAN_POINT ( 'NONE',  ( -36.84489839129339828, 53.54860840895182150, 170.0000000000000000 ) ) ;
#63250 = EDGE_CURVE ( 'NONE', #58728, #14130, #55228, .T. ) ;
#63249 = CARTESIAN_POINT ( 'NONE',  ( -25.81763596640060499, 8.735969132042864516, 5.900969464607853432 ) ) ;
#63251 = CARTESIAN_POINT ( 'NONE',  ( 39.40195752203892710, -170.0000000000000000, 3.069283715499574239 ) ) ;
#63252 = CARTESIAN_POINT ( 'NONE',  ( -14.94265033805046095, 7.459411036484912216, -72.17853611393870494 ) ) ;
#63253 = CARTESIAN_POINT ( 'NONE',  ( -102.2801239173131194, 32.78103895658057354, -8.170026674512225640 ) ) ;
#63254 = CIRCLE ( 'NONE', #38484, 10.00000000000000178 ) ;
#63255 = CARTESIAN_POINT ( 'NONE',  ( 154.6530827109542940, 56.75509330623209792, -36.66977919429117350 ) ) ;
#63256 = CIRCLE ( 'NONE', #52050, 65.36598343705435354 ) ;
#63257 = ORIENTED_EDGE ( 'NONE', *, *, #60582, .F. ) ;
#63259 = AXIS2_PLACEMENT_3D ( 'NONE', #60624, #49004, #54641 ) ;
#63258 = DIRECTION ( 'NONE',  ( -0.4127148655274877065, 0.9108602745606090290, 7.591648651863730094E-15 ) ) ;
#63260 = CARTESIAN_POINT ( 'NONE',  ( -153.6946616617038615, 69.16142959008686830, 58.82626357113776550 ) ) ;
#63261 = CARTESIAN_POINT ( 'NONE',  ( 177.0110682437507705, 75.98481089748382544, -23.19430282288263356 ) ) ;
#63262 = CARTESIAN_POINT ( 'NONE',  ( -109.7079446832838698, 37.86719386855315150, 63.79328878868093256 ) ) ;
#63263 = CARTESIAN_POINT ( 'NONE',  ( 15.68296563925591514, -63.09411298019745828, 170.0000000000000000 ) ) ;
#63264 = ORIENTED_EDGE ( 'NONE', *, *, #35186, .T. ) ;
#63265 = LINE ( 'NONE', #24259, #2075 ) ;
#63266 = CARTESIAN_POINT ( 'NONE',  ( 87.11228333101210808, 19.58587579906928156, 71.55663816294303103 ) ) ;
#63267 = CARTESIAN_POINT ( 'NONE',  ( 201.9822477997853980, 104.3642793804900037, -23.98431144848092345 ) ) ;
#63268 = CARTESIAN_POINT ( 'NONE',  ( 133.8566784816069628, 41.42467568809806977, 44.51034083899536142 ) ) ;
#63269 = DIRECTION ( 'NONE',  ( -0.000000000000000000, 0.000000000000000000, 1.000000000000000000 ) ) ;
#63270 = EDGE_LOOP ( 'NONE', ( #52674, #50773, #14898, #7586 ) ) ;
#63271 = DIRECTION ( 'NONE',  ( 0.000000000000000000, 0.000000000000000000, 1.000000000000000000 ) ) ;
#63272 = CARTESIAN_POINT ( 'NONE',  ( 113.4493678088378346, 30.39339414805072437, -63.47052499151446625 ) ) ;
#63273 = CARTESIAN_POINT ( 'NONE',  ( 39.77028211725815510, -51.87520073220884598, 41.38025477438755928 ) ) ;
#63274 = CARTESIAN_POINT ( 'NONE',  ( 163.2911130186310800, 63.63047778106597718, 14.80112738755994428 ) ) ;
#63275 = PLANE ( 'NONE',  #6082 ) ;
#63276 = PRODUCT_DEFINITION ( 'UNKNOWN', '', #52341, #73 ) ;
#63277 = ORIENTED_EDGE ( 'NONE', *, *, #32653, .F. ) ;
#63278 = EDGE_CURVE ( 'NONE', #39615, #31797, #2038, .T. ) ;
#63279 = FACE_OUTER_BOUND ( 'NONE', #26855, .T. ) ;
#63280 = VERTEX_POINT ( 'NONE', #17606 ) ;
#63282 = EDGE_CURVE ( 'NONE', #56227, #52276, #29207, .T. ) ;
#63281 = CARTESIAN_POINT ( 'NONE',  ( -103.2169245450825343, 33.25885825286820108, -49.97046926489813501 ) ) ;
#63283 = CARTESIAN_POINT ( 'NONE',  ( 126.3770099964006732, 37.08789675649202167, 91.36094124151978235 ) ) ;
#63284 = CARTESIAN_POINT ( 'NONE',  ( -62.54085973597666026, 16.81797209566547124, 37.32607792003522462 ) ) ;
#63285 = VECTOR ( 'NONE', #47206, 1000.000000000000000 ) ;
#63287 = EDGE_LOOP ( 'NONE', ( #62070, #27113, #12963, #67602 ) ) ;
#63286 = CARTESIAN_POINT ( 'NONE',  ( 150.5744176759382640, 53.72473166688032364, 7.104188182867663848 ) ) ;
#63288 = CARTESIAN_POINT ( 'NONE',  ( -180.6009936245623066, 95.85948119829087943, 38.95306750779999305 ) ) ;
#63289 = CARTESIAN_POINT ( 'NONE',  ( 6.526941389886052214, 24.13294503563511029, 0.000000000000000000 ) ) ;
#63290 = CARTESIAN_POINT ( 'NONE',  ( 112.1100957124161397, 30.86846953551571104, -50.70151326046267570 ) ) ;
#63291 = CIRCLE ( 'NONE', #39686, 21.02499999999999858 ) ;
#63292 = VERTEX_POINT ( 'NONE', #61215 ) ;
#63293 = CARTESIAN_POINT ( 'NONE',  ( 20.86596623802176609, -36.13760097092460910, 13.79046412339527805 ) ) ;
#63294 = ADVANCED_FACE ( 'NONE', ( #2820 ), #44702, .T. ) ;
#63295 = AXIS2_PLACEMENT_3D ( 'NONE', #7645, #49125, #966 ) ;
#63296 = DIRECTION ( 'NONE',  ( 0.9989930665413144784, 0.04486483035051863633, 5.102127870520020458E-18 ) ) ;
#63297 = ORIENTED_EDGE ( 'NONE', *, *, #36948, .T. ) ;
#63298 = CARTESIAN_POINT ( 'NONE',  ( 141.2894128405440028, 46.09731134920848916, 64.89240564234853537 ) ) ;
#63299 = CARTESIAN_POINT ( 'NONE',  ( -169.1005390226459326, 82.76152663947085841, 44.66854843987135837 ) ) ;
#63300 = CIRCLE ( 'NONE', #58811, 243.4957430088094839 ) ;
#63301 = DIRECTION ( 'NONE',  ( 0.000000000000000000, 0.000000000000000000, -1.000000000000000000 ) ) ;
#63302 = EDGE_CURVE ( 'NONE', #29554, #57393, #69078, .T. ) ;
#63303 = CARTESIAN_POINT ( 'NONE',  ( 89.20981392318257974, 21.38519354635263170, 44.25831453610486221 ) ) ;
#63304 = ORIENTED_EDGE ( 'NONE', *, *, #23457, .F. ) ;
#63306 = ADVANCED_FACE ( 'NONE', ( #48045 ), #8800, .T. ) ;
#63305 = DIRECTION ( 'NONE',  ( 0.000000000000000000, 0.000000000000000000, 1.000000000000000000 ) ) ;
#63307 = ORIENTED_EDGE ( 'NONE', *, *, #52083, .T. ) ;
#63308 = CARTESIAN_POINT ( 'NONE',  ( 15.55634918610403261, -3.079134169858832593E-14, 0.000000000000000000 ) ) ;
#63309 = CARTESIAN_POINT ( 'NONE',  ( -54.44503425861569923, 14.51857899460407708, 84.00475665173640039 ) ) ;
#63310 = CARTESIAN_POINT ( 'NONE',  ( 108.3753929817421664, 29.13179266688724312, 44.39034800661560354 ) ) ;
#63311 = CARTESIAN_POINT ( 'NONE',  ( -12.50000000000002842, -18.06806526123148160, 0.000000000000000000 ) ) ;
#63312 = CARTESIAN_POINT ( 'NONE',  ( 55.66333002014489750, 11.08673571569896943, 92.52088922431616425 ) ) ;
#63313 = CARTESIAN_POINT ( 'NONE',  ( 188.4365915667138438, 87.87248959723055464, 11.47310305952803056 ) ) ;
#63314 = CARTESIAN_POINT ( 'NONE',  ( 210.9506883977751954, 115.3310071214937267, -47.97542656608541733 ) ) ;
#63315 = B_SPLINE_CURVE_WITH_KNOTS ( 'NONE', 3,
 ( #57833, #21232, #20527, #53217, #10662, #26508 ),
 .UNSPECIFIED., .F., .F.,
 ( 4, 2, 4 ),
 ( 2.380731629708308052E-07, 0.002336973833157560305, 0.004673709593152149643 ),
 .UNSPECIFIED. ) ;
#63316 = CARTESIAN_POINT ( 'NONE',  ( 444.9999999999999432, 225.0000000000000000, -2.000000000000000000 ) ) ;
#63317 = ORIENTED_EDGE ( 'NONE', *, *, #22852, .F. ) ;
#63318 = DIRECTION ( 'NONE',  ( 0.000000000000000000, 0.000000000000000000, 1.000000000000000000 ) ) ;
#63319 = ORIENTED_EDGE ( 'NONE', *, *, #48649, .T. ) ;
#63320 =( REPRESENTATION_RELATIONSHIP ('NONE','NONE', #40274, #63080 ) REPRESENTATION_RELATIONSHIP_WITH_TRANSFORMATION ( #48335 )SHAPE_REPRESENTATION_RELATIONSHIP( ) );
#63321 = FACE_OUTER_BOUND ( 'NONE', #40070, .T. ) ;
#63322 = DIRECTION ( 'NONE',  ( -0.000000000000000000, -0.000000000000000000, -1.000000000000000000 ) ) ;
#63323 = CARTESIAN_POINT ( 'NONE',  ( 46.66904755831212981, 15.55634918610394379, 0.000000000000000000 ) ) ;
#63324 = LINE ( 'NONE', #58040, #42330 ) ;
#63325 = CARTESIAN_POINT ( 'NONE',  ( -105.4642082819536313, 35.56541171990216554, -8.863305472588931977 ) ) ;
#63326 = VERTEX_POINT ( 'NONE', #69501 ) ;
#63327 = CARTESIAN_POINT ( 'NONE',  ( -452.6627218934913230, 399.9999999999997726, 113.5502958579881891 ) ) ;
#63328 = FACE_OUTER_BOUND ( 'NONE', #7332, .T. ) ;
#63329 = ORIENTED_EDGE ( 'NONE', *, *, #46004, .T. ) ;
#63330 = EDGE_CURVE ( 'NONE', #45231, #20757, #43114, .T. ) ;
#63331 = ORIENTED_EDGE ( 'NONE', *, *, #28757, .F. ) ;
#63332 = LINE ( 'NONE', #15142, #3990 ) ;
#63333 = CARTESIAN_POINT ( 'NONE',  ( 56.30011474572734187, 11.21470186335419505, -46.56933648099417411 ) ) ;
#63334 = CARTESIAN_POINT ( 'NONE',  ( 174.1251613516844543, 71.84747073139210727, -14.02940449773612208 ) ) ;
#63335 = COLOUR_RGB ( '',0.7921568627450980005, 0.8196078431372548767, 0.9333333333333333481 ) ;
#63336 = DIRECTION ( 'NONE',  ( 1.000000000000000000, 0.000000000000000000, 0.000000000000000000 ) ) ;
#63337 = ORIENTED_EDGE ( 'NONE', *, *, #40820, .F. ) ;
#63338 = CARTESIAN_POINT ( 'NONE',  ( -133.3799602664182089, 52.86209125874979975, 38.65010449165978201 ) ) ;
#63339 = ORIENTED_EDGE ( 'NONE', *, *, #38504, .F. ) ;
#63340 = CARTESIAN_POINT ( 'NONE',  ( 19.54326199789021956, 7.657220834818549093, -49.51591199172310809 ) ) ;
#63341 = CARTESIAN_POINT ( 'NONE',  ( -142.0084862216822330, 59.34995487985344909, 38.79924527383067101 ) ) ;
#63342 = VECTOR ( 'NONE', #56674, 1000.000000000000000 ) ;
#63343 = DIRECTION ( 'NONE',  ( 0.000000000000000000, 1.000000000000000000, 0.000000000000000000 ) ) ;
#63344 = VECTOR ( 'NONE', #13577, 1000.000000000000000 ) ;
#63345 = VECTOR ( 'NONE', #51069, 1000.000000000000000 ) ;
#63346 = VECTOR ( 'NONE', #62592, 1000.000000000000000 ) ;
#63347 = ORIENTED_EDGE ( 'NONE', *, *, #47237, .T. ) ;
#63348 = ORIENTED_EDGE ( 'NONE', *, *, #12621, .F. ) ;
#63349 = CARTESIAN_POINT ( 'NONE',  ( 112.2220340837702395, -21.53708152545855370, -4.491189304432825047 ) ) ;
#63350 = CARTESIAN_POINT ( 'NONE',  ( -118.8238520964533507, 43.19104454097361412, 94.39884469698169767 ) ) ;
#63351 = AXIS2_PLACEMENT_3D ( 'NONE', #9516, #52424, #1034 ) ;
#63352 = FACE_OUTER_BOUND ( 'NONE', #38256, .T. ) ;
#63353 = CARTESIAN_POINT ( 'NONE',  ( -62.41990535723909517, -170.0000000000000000, -95.00000000000133582 ) ) ;
#63354 = CARTESIAN_POINT ( 'NONE',  ( 67.93926590385568431, 13.86859831467922710, 42.99160110879589780 ) ) ;
#63355 = CARTESIAN_POINT ( 'NONE',  ( 8.976513922597330719, 7.384348797512408247, 88.04828221664904220 ) ) ;
#63356 = EDGE_CURVE ( 'NONE', #57513, #43949, #5492, .T. ) ;
#63357 = EDGE_CURVE ( 'NONE', #51688, #48281, #14417, .T. ) ;
#63358 = ORIENTED_EDGE ( 'NONE', *, *, #56442, .T. ) ;
#63359 = DIRECTION ( 'NONE',  ( 8.893845946170152056E-21, -1.110223024625156294E-16, 1.000000000000000000 ) ) ;
#63360 = FACE_OUTER_BOUND ( 'NONE', #45690, .T. ) ;
#63361 = EDGE_CURVE ( 'NONE', #52273, #62726, #204, .T. ) ;
#63362 = ORIENTED_EDGE ( 'NONE', *, *, #43981, .T. ) ;
#63363 = CARTESIAN_POINT ( 'NONE',  ( -82.32750425780476178, 23.74963782027935721, 17.63696427471160888 ) ) ;
#63364 = ORIENTED_EDGE ( 'NONE', *, *, #30579, .T. ) ;
#63365 = DIRECTION ( 'NONE',  ( 7.703719777548945123E-34, 1.479221584281240009E-31, -1.000000000000000000 ) ) ;
#63366 = EDGE_CURVE ( 'NONE', #51103, #44250, #24978, .T. ) ;
#63367 = ORIENTED_EDGE ( 'NONE', *, *, #12225, .T. ) ;
#63368 = EDGE_CURVE ( 'NONE', #46924, #50931, #12331, .T. ) ;
#63369 = EDGE_LOOP ( 'NONE', ( #21266, #65176, #39034, #29142 ) ) ;
#63370 = LINE ( 'NONE', #20111, #3831 ) ;
#63371 = CARTESIAN_POINT ( 'NONE',  ( -180.2244609727085276, 95.39945930389644957, 62.74216164717486066 ) ) ;
#63372 = CARTESIAN_POINT ( 'NONE',  ( 130.7531879853686405, 39.58149302537893988, 70.69835057338305262 ) ) ;
#63373 = ORIENTED_EDGE ( 'NONE', *, *, #5396, .T. ) ;
#63374 = CARTESIAN_POINT ( 'NONE',  ( -38.02163356681019479, 10.76490728754187032, 94.99999999999866418 ) ) ;
#63375 = CARTESIAN_POINT ( 'NONE',  ( 400.0000000000000000, 0.000000000000000000, 0.000000000000000000 ) ) ;
#63376 = AXIS2_PLACEMENT_3D ( 'NONE', #8714, #62156, #29459 ) ;
#63377 = CARTESIAN_POINT ( 'NONE',  ( -444.3843108123961088, 394.6949978562683441, -128.2300613526361701 ) ) ;
#63378 = EDGE_CURVE ( 'NONE', #27549, #33732, #68239, .T. ) ;
#63379 = CARTESIAN_POINT ( 'NONE',  ( 103.8093541423579325, 26.01745837747062851, -47.30919203401695228 ) ) ;
#63380 = CARTESIAN_POINT ( 'NONE',  ( -25.80058235236790054, 8.733375263008323230, 42.68610631600346039 ) ) ;
#63382 = EDGE_CURVE ( 'NONE', #19486, #22868, #565, .T. ) ;
#63381 = CARTESIAN_POINT ( 'NONE',  ( -144.9412191745148277, 61.69548892475970803, -63.18798172190984275 ) ) ;
#63383 = ORIENTED_EDGE ( 'NONE', *, *, #16636, .F. ) ;
#63384 = STYLED_ITEM ( 'NONE', ( #31154 ), #40361 ) ;
#63385 = FACE_OUTER_BOUND ( 'NONE', #46278, .T. ) ;
#63386 = AXIS2_PLACEMENT_3D ( 'NONE', #49207, #67085, #16519 ) ;
#63387 = CARTESIAN_POINT ( 'NONE',  ( -84.23336401058612921, 25.60798568215576054, -64.41046605635534661 ) ) ;
#63388 = CARTESIAN_POINT ( 'NONE',  ( -6.140867422161948141, 6.785844475553973965, -89.24911309443601226 ) ) ;
#63389 = CARTESIAN_POINT ( 'NONE',  ( 0.000000000000000000, 0.000000000000000000, 0.000000000000000000 ) ) ;
#63390 = CARTESIAN_POINT ( 'NONE',  ( 447.3372781065086201, 400.0000000000044338, 113.5502958579838122 ) ) ;
#63391 = CARTESIAN_POINT ( 'NONE',  ( 126.8015497489690375, 37.32461426945043570, 7.607582870371705219 ) ) ;
#63392 = VECTOR ( 'NONE', #2169, 1000.000000000000114 ) ;
#63393 = CARTESIAN_POINT ( 'NONE',  ( -153.1121305730337099, 67.29834700374524914, 17.95717372012110502 ) ) ;
#63394 = LINE ( 'NONE', #63741, #19308 ) ;
#63395 = AXIS2_PLACEMENT_3D ( 'NONE', #17404, #27611, #38881 ) ;
#63396 = CARTESIAN_POINT ( 'NONE',  ( 211.1046732743772338, 117.3965485104337176, 40.61640241343361168 ) ) ;
#63397 = CARTESIAN_POINT ( 'NONE',  ( -81.90760111942955746, 24.66532273091451088, 71.54302205457766206 ) ) ;
#63398 = CARTESIAN_POINT ( 'NONE',  ( -103.2169245450825343, 33.25885825286820108, 30.56318250649291457 ) ) ;
#63399 = ORIENTED_EDGE ( 'NONE', *, *, #18623, .F. ) ;
#63401 = AXIS2_PLACEMENT_3D ( 'NONE', #44317, #49942, #27797 ) ;
#63400 = ITEM_DEFINED_TRANSFORMATION ( 'NONE', 'NONE', #33217,  #66832 ) ;
#63402 = PLANE ( 'NONE',  #30720 ) ;
#63403 = ORIENTED_EDGE ( 'NONE', *, *, #67221, .F. ) ;
#63404 = CARTESIAN_POINT ( 'NONE',  ( -17.50000000000002842, 207.5000000000000284, 0.000000000000000000 ) ) ;
#63405 = ORIENTED_EDGE ( 'NONE', *, *, #37873, .T. ) ;
#63406 = DIRECTION ( 'NONE',  ( -0.000000000000000000, 1.000000000000000000, -0.000000000000000000 ) ) ;
#63407 = CYLINDRICAL_SURFACE ( 'NONE', #15900, 65.36598343705435354 ) ;
#63408 = CARTESIAN_POINT ( 'NONE',  ( -169.8885678771098640, 85.07765565657317097, 31.53960263309836520 ) ) ;
#63409 = FACE_OUTER_BOUND ( 'NONE', #12341, .T. ) ;
#63410 = CARTESIAN_POINT ( 'NONE',  ( 136.7690435008551049, 44.39743995805024213, -50.43862942802062577 ) ) ;
#63411 = CARTESIAN_POINT ( 'NONE',  ( 32.29989959354727347, 7.591763852038295290, -40.69674924162746521 ) ) ;
#63412 = CARTESIAN_POINT ( 'NONE',  ( 149.9552318559266837, 52.03645904563050095, -43.60103139574965780 ) ) ;
#63413 = DIRECTION ( 'NONE',  ( 1.000000000000000000, -0.000000000000000000, -0.000000000000000000 ) ) ;
#63414 = CARTESIAN_POINT ( 'NONE',  ( -123.0348077379026819, 45.83489305753317211, -8.631653705166407065 ) ) ;
#63415 = EDGE_LOOP ( 'NONE', ( #38318, #5156, #37521, #63307 ) ) ;
#63417 = EDGE_LOOP ( 'NONE', ( #49129, #69391 ) ) ;
#63416 = ADVANCED_BREP_SHAPE_REPRESENTATION ( '', ( #18150, #66832 ), #5131 ) ;
#63418 = CARTESIAN_POINT ( 'NONE',  ( 182.3755817553430063, 81.36527810436713537, 83.10424013160293555 ) ) ;
#63419 = CARTESIAN_POINT ( 'NONE',  ( -165.6754884515988522, 80.64428675972324356, -95.00000000000133582 ) ) ;
#63420 = DIRECTION ( 'NONE',  ( -0.000000000000000000, -1.000000000000000000, -0.000000000000000000 ) ) ;
#63421 = UNCERTAINTY_MEASURE_WITH_UNIT (LENGTH_MEASURE( 1.000000000000000082E-05 ), #46277, 'distance_accuracy_value', 'NONE');
#63422 = CARTESIAN_POINT ( 'NONE',  ( 64.63121951458684578, 14.08762381031449351, -89.57469566860601162 ) ) ;
#63423 = CARTESIAN_POINT ( 'NONE',  ( 90.30732934992393268, 21.77797012484618122, 16.92149306509885776 ) ) ;
#63424 = DIRECTION ( 'NONE',  ( -0.000000000000000000, -0.000000000000000000, -1.000000000000000000 ) ) ;
#63425 = CARTESIAN_POINT ( 'NONE',  ( 173.6012773665504199, 71.36035397668607061, -71.15789844731480684 ) ) ;
#63426 = CARTESIAN_POINT ( 'NONE',  ( 0.01688885742777323368, -7.321065037175435997, -3.319543390096042046 ) ) ;
#63427 = CARTESIAN_POINT ( 'NONE',  ( 93.86680996363766383, 22.01878169039503774, -14.49409919722980256 ) ) ;
#63428 = CARTESIAN_POINT ( 'NONE',  ( -27.70115495247213033, 10.02455692117576191, 71.08150156007859266 ) ) ;
#63429 = DIRECTION ( 'NONE',  ( 0.000000000000000000, 0.000000000000000000, 1.000000000000000000 ) ) ;
#63430 = CARTESIAN_POINT ( 'NONE',  ( -417.6627218934915504, 399.9999999999957367, 78.55029585799222502 ) ) ;
#63431 = VECTOR ( 'NONE', #54439, 1000.000000000000000 ) ;
#63432 = ORIENTED_EDGE ( 'NONE', *, *, #59142, .F. ) ;
#63433 = LINE ( 'NONE', #47923, #52614 ) ;
#63434 = FACE_OUTER_BOUND ( 'NONE', #41515, .T. ) ;
#63435 = CARTESIAN_POINT ( 'NONE',  ( 154.6530827109543509, 56.75509330623210502, 70.70842316756356638 ) ) ;
#63436 = CARTESIAN_POINT ( 'NONE',  ( -104.5916564445180512, 35.10571011602409186, -62.20883666294024295 ) ) ;
#63437 = DIRECTION ( 'NONE',  ( 0.000000000000000000, 0.000000000000000000, 1.000000000000000000 ) ) ;
#63438 = CARTESIAN_POINT ( 'NONE',  ( -0.3276879771421796761, 7.525453440574858988, 90.93095886057497523 ) ) ;
#63439 = VECTOR ( 'NONE', #62821, 1000.000000000000000 ) ;
#63440 = ORIENTED_EDGE ( 'NONE', *, *, #56195, .T. ) ;
#63441 = CARTESIAN_POINT ( 'NONE',  ( 0.3194001229790394136, 3.115132258388581210, 7.999999999999998224 ) ) ;
#63442 = VECTOR ( 'NONE', #68470, 1000.000000000000000 ) ;
#63443 = DIRECTION ( 'NONE',  ( -1.000000000000000000, -0.000000000000000000, 0.000000000000000000 ) ) ;
#63444 = ADVANCED_FACE ( 'NONE', ( #5825 ), #49428, .F. ) ;
#63445 = ORIENTED_EDGE ( 'NONE', *, *, #12015, .T. ) ;
#63446 = ORIENTED_EDGE ( 'NONE', *, *, #17607, .T. ) ;
#63447 = VECTOR ( 'NONE', #8629, 1000.000000000000114 ) ;
#63448 = CARTESIAN_POINT ( 'NONE',  ( 46.42183744180581328, 10.44561024203780875, 93.82526922102383082 ) ) ;
#63449 = CARTESIAN_POINT ( 'NONE',  ( -179.6470915626257465, 94.69856161161352759, -72.76301568367956918 ) ) ;
#63450 = CARTESIAN_POINT ( 'NONE',  ( 140.8933556880726030, 47.04060091794853804, -94.58027771532738370 ) ) ;
#63451 = ORIENTED_EDGE ( 'NONE', *, *, #7147, .F. ) ;
#63452 = DIRECTION ( 'NONE',  ( 0.000000000000000000, 0.000000000000000000, 1.000000000000000000 ) ) ;
#63453 = DIRECTION ( 'NONE',  ( 1.000000000000000000, 0.000000000000000000, 0.000000000000000000 ) ) ;
#63454 = EDGE_CURVE ( 'NONE', #3025, #28173, #12169, .T. ) ;
#63455 = CARTESIAN_POINT ( 'NONE',  ( -0.9897066053608921665, 7.549089325901768177, 7.675277931132895581 ) ) ;
#63456 = CARTESIAN_POINT ( 'NONE',  ( 174.9099402067543565, 73.96774984027639732, -39.45882913571559669 ) ) ;
#63457 = CARTESIAN_POINT ( 'NONE',  ( -153.6946616617039183, 69.16142959008689672, -75.39648938118064336 ) ) ;
#63458 = DIRECTION ( 'NONE',  ( -1.850169831522831466E-16, 1.000000000000000000, 1.110223024625156294E-16 ) ) ;
#63459 = EDGE_LOOP ( 'NONE', ( #10028, #13785, #6394, #21471 ) ) ;
#63460 = DIRECTION ( 'NONE',  ( -0.000000000000000000, -0.000000000000000000, -1.000000000000000000 ) ) ;
#63461 = CARTESIAN_POINT ( 'NONE',  ( 8.336031647119270360, 6.376437040857335425, 65.33787955784195844 ) ) ;
#63463 = ADVANCED_FACE ( 'NONE', ( #43457 ), #55411, .F. ) ;
#63462 = CARTESIAN_POINT ( 'NONE',  ( -63.73419499958997392, 12.83646726144839079, 3.061616997868437868E-16 ) ) ;
#63464 = CARTESIAN_POINT ( 'NONE',  ( 202.7506655727289342, 105.3943386412348815, 43.96215325962744913 ) ) ;
#63465 = CARTESIAN_POINT ( 'NONE',  ( 79.20784687562183990, 17.02089708476972874, 89.76511234889541413 ) ) ;
#63467 = ORIENTED_EDGE ( 'NONE', *, *, #728, .T. ) ;
#63466 = DIRECTION ( 'NONE',  ( -0.6246950475544236214, 7.650307904307285654E-17, 0.7808688094430308313 ) ) ;
#63468 = ORIENTED_EDGE ( 'NONE', *, *, #36224, .F. ) ;
#63469 = ORIENTED_EDGE ( 'NONE', *, *, #39057, .T. ) ;
#63470 = CARTESIAN_POINT ( 'NONE',  ( 117.4711568421289911, 33.49899443629669804, -68.20117326592374241 ) ) ;
#63471 = DIRECTION ( 'NONE',  ( -0.8160245890732938934, -0.5780171883497599028, 0.000000000000000000 ) ) ;
#63472 = CARTESIAN_POINT ( 'NONE',  ( 199.3743599161303450, 99.31857334527873604, -65.36260388931131615 ) ) ;
#63473 = DIRECTION ( 'NONE',  ( -1.000000000000000000, 0.000000000000000000, -0.000000000000000000 ) ) ;
#63474 = CARTESIAN_POINT ( 'NONE',  ( -118.4553071845214873, 41.78724769484929880, 63.86654146996676218 ) ) ;
#63475 = CARTESIAN_POINT ( 'NONE',  ( 151.6351261592329251, 53.25263237790402115, -65.75027802898746643 ) ) ;
#63476 = CARTESIAN_POINT ( 'NONE',  ( 22.54170116539453161, 7.818774103032803069, -93.41931582978958204 ) ) ;
#63477 = VECTOR ( 'NONE', #25079, 1000.000000000000000 ) ;
#63478 = DIRECTION ( 'NONE',  ( 0.000000000000000000, 0.000000000000000000, 1.000000000000000000 ) ) ;
#63479 = EDGE_LOOP ( 'NONE', ( #54600, #45520, #831, #41116 ) ) ;
#63480 = ORIENTED_EDGE ( 'NONE', *, *, #45020, .F. ) ;
#63481 = CARTESIAN_POINT ( 'NONE',  ( 68.94309019697858787, 15.16533147648755175, -11.75461547644634841 ) ) ;
#63482 = VECTOR ( 'NONE', #46139, 1000.000000000000000 ) ;
#63483 = CARTESIAN_POINT ( 'NONE',  ( -85.90077524418995836, 26.30132018890135726, -40.62086469904666330 ) ) ;
#63484 = CARTESIAN_POINT ( 'NONE',  ( 117.3330559693645938, 32.30248182301458115, 88.32983765503517759 ) ) ;
#63485 = CARTESIAN_POINT ( 'NONE',  ( 114.6659427952414632, 32.10199811723105512, -10.50219939888065745 ) ) ;
#63486 = AXIS2_PLACEMENT_3D ( 'NONE', #33559, #28618, #22991 ) ;
#63487 = VECTOR ( 'NONE', #24519, 1000.000000000000000 ) ;
#63488 = FACE_BOUND ( 'NONE', #29028, .T. ) ;
#63489 = LINE ( 'NONE', #15303, #49426 ) ;
#63490 = CARTESIAN_POINT ( 'NONE',  ( -149.8802420082118374, 65.81997532648824745, 84.41443440944620136 ) ) ;
#63491 = ORIENTED_EDGE ( 'NONE', *, *, #67416, .F. ) ;
#63492 = ORIENTED_EDGE ( 'NONE', *, *, #48902, .F. ) ;
#63493 = VECTOR ( 'NONE', #53909, 1000.000000000000000 ) ;
#63494 = ORIENTED_EDGE ( 'NONE', *, *, #15624, .F. ) ;
#63495 = AXIS2_PLACEMENT_3D ( 'NONE', #4030, #51867, #13551 ) ;
#63496 = CARTESIAN_POINT ( 'NONE',  ( 32.37980458033285203, 8.611076697115699119, -40.47400308918246736 ) ) ;
#63497 = DIRECTION ( 'NONE',  ( 0.000000000000000000, 0.000000000000000000, 1.000000000000000000 ) ) ;
#63498 = CARTESIAN_POINT ( 'NONE',  ( 447.3372781065085633, 399.9999999999998863, 113.5502958579882034 ) ) ;
#63499 = CARTESIAN_POINT ( 'NONE',  ( 199.3764173596862292, 100.9540560740992419, 58.24261284197358890 ) ) ;
#63500 = FACE_BOUND ( 'NONE', #12148, .T. ) ;
#63501 = CARTESIAN_POINT ( 'NONE',  ( 46.91100451385224801, 9.505349959559994844, 90.54425985225793738 ) ) ;
#63502 = ADVANCED_FACE ( 'NONE', ( #49780 ), #53999, .F. ) ;
#63503 = CARTESIAN_POINT ( 'NONE',  ( 31.11269837220800127, -26.11269837220812562, 2.000000000000001776 ) ) ;
#63504 = DIRECTION ( 'NONE',  ( -0.000000000000000000, -0.000000000000000000, -1.000000000000000000 ) ) ;
#63505 = PLANE ( 'NONE',  #1677 ) ;
#63506 = LINE ( 'NONE', #15319, #32016 ) ;
#63507 = CARTESIAN_POINT ( 'NONE',  ( 126.5710838895482198, 37.19597237024179037, -18.47868295772153502 ) ) ;
#63508 = PLANE ( 'NONE',  #44448 ) ;
#63509 = CARTESIAN_POINT ( 'NONE',  ( 0.000000000000000000, 0.000000000000000000, 30.00000000000000000 ) ) ;
#63510 = EDGE_CURVE ( 'NONE', #15369, #66651, #19508, .T. ) ;
#63511 = ORIENTED_EDGE ( 'NONE', *, *, #9597, .T. ) ;
#63512 = CARTESIAN_POINT ( 'NONE',  ( -4.364688291132793552, 24.74039788130344419, 0.000000000000000000 ) ) ;
#63513 = APPLICATION_PROTOCOL_DEFINITION ( 'draft international standard', 'automotive_design', 1998, #37723 ) ;
#63514 = FACE_OUTER_BOUND ( 'NONE', #23161, .T. ) ;
#63515 = DIRECTION ( 'NONE',  ( 0.000000000000000000, 0.000000000000000000, -1.000000000000000000 ) ) ;
#63516 = CARTESIAN_POINT ( 'NONE',  ( -108.9145525555662459, 37.42858360505776005, -46.02153963151565108 ) ) ;
#63517 = CARTESIAN_POINT ( 'NONE',  ( 183.1873354889583254, 82.20882912211250471, -50.93700232963676200 ) ) ;
#63518 = ORIENTED_EDGE ( 'NONE', *, *, #12907, .F. ) ;
#63519 = ORIENTED_EDGE ( 'NONE', *, *, #17946, .T. ) ;
#63520 = ADVANCED_FACE ( 'NONE', ( #23765 ), #67040, .F. ) ;
#63521 = DIRECTION ( 'NONE',  ( -0.9989930665413151445, 0.04486483035050446017, 0.000000000000000000 ) ) ;
#63522 = CARTESIAN_POINT ( 'NONE',  ( 173.6502905022586560, 71.40583870588187665, 91.51296465151303039 ) ) ;
#63523 = EDGE_CURVE ( 'NONE', #39998, #23524, #45859, .T. ) ;
#63524 = EDGE_LOOP ( 'NONE', ( #51596, #19038, #20514, #23764 ) ) ;
#63525 = CIRCLE ( 'NONE', #37703, 20.00000000000000000 ) ;
#63526 = CARTESIAN_POINT ( 'NONE',  ( 117.0065308422768595, 32.13872219870570035, 60.70489602400656537 ) ) ;
#63527 = ORIENTED_EDGE ( 'NONE', *, *, #27801, .F. ) ;
#63528 = DIRECTION ( 'NONE',  ( 1.387778780781445429E-16, -1.000000000000000000, -3.081487911019577365E-33 ) ) ;
#63529 = CARTESIAN_POINT ( 'NONE',  ( 129.4987365823221808, 38.85470922756777412, 30.90157705602048921 ) ) ;
#63530 = AXIS2_PLACEMENT_3D ( 'NONE', #47896, #53515, #31392 ) ;
#63531 = CARTESIAN_POINT ( 'NONE',  ( -31.11269837220812207, -26.11269837220801193, 2.000000000000001776 ) ) ;
#63532 = ADVANCED_FACE ( 'NONE', ( #61045 ), #35710, .F. ) ;
#63533 = CARTESIAN_POINT ( 'NONE',  ( -95.19652294162978023, 29.32558722310179178, 40.53639674485660294 ) ) ;
#63534 = CIRCLE ( 'NONE', #11800, 4.999999999999990230 ) ;
#63536 = CARTESIAN_POINT ( 'NONE',  ( 91.49345572560145001, 21.13836538408682131, -49.03551200642353081 ) ) ;
#63535 = AXIS2_PLACEMENT_3D ( 'NONE', #12836, #13182, #67005 ) ;
#63538 = ORIENTED_EDGE ( 'NONE', *, *, #26354, .T. ) ;
#63537 = DIRECTION ( 'NONE',  ( 0.9839295885986295565, 0.1785568947986370392, 0.000000000000000000 ) ) ;
#63539 =( GEOMETRIC_REPRESENTATION_CONTEXT ( 3 ) GLOBAL_UNCERTAINTY_ASSIGNED_CONTEXT ( ( #31075 ) ) GLOBAL_UNIT_ASSIGNED_CONTEXT ( ( #69381, #32102, #32790 ) ) REPRESENTATION_CONTEXT ( 'NONE', 'WORKASPACE' ) );
#63540 = DIRECTION ( 'NONE',  ( 1.000000000000000000, 0.000000000000000000, 0.000000000000000000 ) ) ;
#63541 = VECTOR ( 'NONE', #52214, 1000.000000000000000 ) ;
#63542 = ORIENTED_EDGE ( 'NONE', *, *, #46510, .F. ) ;
#63543 = VERTEX_POINT ( 'NONE', #57162 ) ;
#63544 = CARTESIAN_POINT ( 'NONE',  ( 429.8372781065087338, 388.0000000000065938, 96.05029585798857283 ) ) ;
#63545 = CARTESIAN_POINT ( 'NONE',  ( 0.000000000000000000, 0.000000000000000000, 40.00000000000003553 ) ) ;
#63546 = EDGE_CURVE ( 'NONE', #42469, #24394, #13896, .T. ) ;
#63547 = DIRECTION ( 'NONE',  ( 0.000000000000000000, 1.000000000000000000, -0.000000000000000000 ) ) ;
#63549 = EDGE_LOOP ( 'NONE', ( #60397, #32980, #39445, #10574 ) ) ;
#63548 = CARTESIAN_POINT ( 'NONE',  ( 10.55634918610411432, 46.66904755831205875, 2.000000000000000000 ) ) ;
#63550 = CARTESIAN_POINT ( 'NONE',  ( 61.09977118998600076, 13.26754120022606109, 3.213164665537364684 ) ) ;
#63551 = ADVANCED_FACE ( 'NONE', ( #19168 ), #34328, .F. ) ;
#63552 = EDGE_CURVE ( 'NONE', #7998, #59358, #55776, .T. ) ;
#63553 = CARTESIAN_POINT ( 'NONE',  ( -452.6627218934913230, 177.8591479523843475, -111.4497041420117966 ) ) ;
#63554 = ORIENTED_EDGE ( 'NONE', *, *, #11015, .T. ) ;
#63555 = DIRECTION ( 'NONE',  ( -0.000000000000000000, -0.000000000000000000, -1.000000000000000000 ) ) ;
#63556 = CARTESIAN_POINT ( 'NONE',  ( -132.5976199670998597, 52.30296609017644016, -72.63115324000138173 ) ) ;
#63557 = CARTESIAN_POINT ( 'NONE',  ( 433.3728120124415568, 395.0000000000001137, -132.4852380479447902 ) ) ;
#63558 = CARTESIAN_POINT ( 'NONE',  ( -94.78109144324893975, 29.13179392050638583, 10.88929637896141855 ) ) ;
#63559 = CARTESIAN_POINT ( 'NONE',  ( -94.84390436305042726, 29.16104988397311715, -68.34880207487753978 ) ) ;
#63560 = VERTEX_POINT ( 'NONE', #66691 ) ;
#63561 = ORIENTED_EDGE ( 'NONE', *, *, #54208, .F. ) ;
#63562 = CARTESIAN_POINT ( 'NONE',  ( 187.2354698746857480, 85.05376776489251256, -74.88949992417202850 ) ) ;
#63563 = CARTESIAN_POINT ( 'NONE',  ( -165.6212796729685692, 79.15047440262054579, -42.51887467077794014 ) ) ;
#63564 = CARTESIAN_POINT ( 'NONE',  ( -24.39004539972345498, 0.000000000000000000, 5.000000000000000000 ) ) ;
#63565 = CARTESIAN_POINT ( 'NONE',  ( 107.9213359589208494, 28.92595015506873324, -63.11969581620832770 ) ) ;
#63566 = CARTESIAN_POINT ( 'NONE',  ( -73.09214866197369531, 21.34321757515763451, 32.87608688857182671 ) ) ;
#63567 = CARTESIAN_POINT ( 'NONE',  ( 80.17205177205137545, 17.31791394718354482, 33.38893405093305944 ) ) ;
#63568 = CARTESIAN_POINT ( 'NONE',  ( 64.93224207568367490, 14.16036304753835040, -35.96564466294290696 ) ) ;
#63569 = LINE ( 'NONE', #30184, #51946 ) ;
#63570 = PLANE ( 'NONE',  #41960 ) ;
#63571 = EDGE_LOOP ( 'NONE', ( #16801, #39351, #51790, #32222 ) ) ;
#63572 = CARTESIAN_POINT ( 'NONE',  ( -104.5827168854524700, 33.96561401163045701, -22.82331764786334816 ) ) ;
#63573 = ORIENTED_EDGE ( 'NONE', *, *, #61307, .T. ) ;
#63574 = VECTOR ( 'NONE', #17348, 1000.000000000000000 ) ;
#63575 = CARTESIAN_POINT ( 'NONE',  ( -38.69408084385329971, 10.89529537250243152, 12.83750613738102153 ) ) ;
#63576 = CARTESIAN_POINT ( 'NONE',  ( 82.94816950786170651, 19.25538918181906922, 70.59558542695980066 ) ) ;
#63577 = CARTESIAN_POINT ( 'NONE',  ( -78.66644367742111399, 22.32174330031318732, -88.80455181264524356 ) ) ;
#63578 = CARTESIAN_POINT ( 'NONE',  ( 151.1873096904021452, 52.92629247302094342, -12.67588465243391127 ) ) ;
#63579 = CARTESIAN_POINT ( 'NONE',  ( 0.000000000000000000, 0.000000000000000000, 0.000000000000000000 ) ) ;
#63581 = PLANE ( 'NONE',  #13634 ) ;
#63580 = AXIS2_PLACEMENT_3D ( 'NONE', #41090, #57272, #31236 ) ;
#63582 = CARTESIAN_POINT ( 'NONE',  ( 37.47081272996199885, 8.166145978397521432, -62.71310258412169958 ) ) ;
#63583 = CARTESIAN_POINT ( 'NONE',  ( -95.05323930133205579, 30.36974142673410526, -67.28845679951155034 ) ) ;
#63584 = CARTESIAN_POINT ( 'NONE',  ( -36.89224332184166855, 11.57404295377975956, -21.12750825744156913 ) ) ;
#63585 = VECTOR ( 'NONE', #36431, 1000.000000000000000 ) ;
#63586 = CIRCLE ( 'NONE', #15281, 4.999999999999997335 ) ;
#63587 = ORIENTED_EDGE ( 'NONE', *, *, #54919, .F. ) ;
#63588 = DIRECTION ( 'NONE',  ( -1.000000000000000000, 0.000000000000000000, 0.000000000000000000 ) ) ;
#63590 = ORIENTED_EDGE ( 'NONE', *, *, #44651, .T. ) ;
#63589 = EDGE_CURVE ( 'NONE', #60452, #22374, #39936, .T. ) ;
#63591 = AXIS2_PLACEMENT_3D ( 'NONE', #11491, #53365, #59346 ) ;
#63592 = DIRECTION ( 'NONE',  ( -1.000000000000000000, -1.387778780781445676E-16, 0.000000000000000000 ) ) ;
#63593 = DIRECTION ( 'NONE',  ( -1.000000000000000000, 0.000000000000000000, 0.000000000000000000 ) ) ;
#63594 = CARTESIAN_POINT ( 'NONE',  ( -24.33435124463266419, 8.532637995283112176, 13.28721146798333841 ) ) ;
#63595 = DIRECTION ( 'NONE',  ( 1.000000000000000000, 0.000000000000000000, 0.000000000000000000 ) ) ;
#63596 = CIRCLE ( 'NONE', #59048, 242.4895526022646379 ) ;
#63597 = CARTESIAN_POINT ( 'NONE',  ( -7.825402957745083654, 6.891034867348166948, -77.26262132240753999 ) ) ;
#63598 = DIRECTION ( 'NONE',  ( 1.000000000000000000, 0.000000000000000000, 0.000000000000000000 ) ) ;
#63599 = CARTESIAN_POINT ( 'NONE',  ( 155.7265855639938650, 57.57443315515123317, -50.93204425173435368 ) ) ;
#63600 = EDGE_CURVE ( 'NONE', #30587, #48842, #9908, .T. ) ;
#63601 = AXIS2_PLACEMENT_3D ( 'NONE', #21764, #68914, #16494 ) ;
#63602 = EDGE_LOOP ( 'NONE', ( #9173, #26361, #6668, #18843 ) ) ;
#63603 = CARTESIAN_POINT ( 'NONE',  ( 519.1032903415814417, 910.0916049287825444, 745.5068267248719849 ) ) ;
#63604 = CARTESIAN_POINT ( 'NONE',  ( -152.9143627383494959, 68.46626892668655273, 71.76242021779931690 ) ) ;
#63605 = DIRECTION ( 'NONE',  ( 1.000000000000000000, 0.000000000000000000, 0.000000000000000000 ) ) ;
#63606 = CARTESIAN_POINT ( 'NONE',  ( -102.7494334820057276, 34.14986869751101040, 72.36362509687886302 ) ) ;
#63607 = CARTESIAN_POINT ( 'NONE',  ( -44.29440389294402536, -17.09499999999999886, 4.000000000000000000 ) ) ;
#63608 = ORIENTED_EDGE ( 'NONE', *, *, #52632, .T. ) ;
#63609 = CARTESIAN_POINT ( 'NONE',  ( 2.129405171194437063, -25.03204795498853841, 0.000000000000000000 ) ) ;
#63610 = CARTESIAN_POINT ( 'NONE',  ( -2.874437057892792247, 6.618922960888032669, -21.72834514570417497 ) ) ;
#63611 = ADVANCED_FACE ( 'NONE', ( #35011, #8635, #56456 ), #8284, .F. ) ;
#63612 = CARTESIAN_POINT ( 'NONE',  ( -26.69131247781221106, -59.26697088777007849, 40.00000000000003553 ) ) ;
#63613 = CARTESIAN_POINT ( 'NONE',  ( -142.9185165087913845, 58.78605825417614739, 88.31239537911277182 ) ) ;
#63614 = EDGE_CURVE ( 'NONE', #29355, #5954, #13659, .T. ) ;
#63615 = DIRECTION ( 'NONE',  ( -1.000000000000000000, -0.000000000000000000, 2.312964634635743450E-16 ) ) ;
#63616 = EDGE_CURVE ( 'NONE', #23082, #40754, #25848, .T. ) ;
#63617 = VERTEX_POINT ( 'NONE', #58519 ) ;
#63618 = LINE ( 'NONE', #47417, #18783 ) ;
#63619 = LINE ( 'NONE', #68872, #252 ) ;
#63620 = CARTESIAN_POINT ( 'NONE',  ( 188.0103583326377930, 87.39896620268125105, 39.69940583340289919 ) ) ;
#63622 = CARTESIAN_POINT ( 'NONE',  ( 157.0357419681844533, 58.58786672900118475, 29.41886851933077196 ) ) ;
#63621 = B_SPLINE_CURVE_WITH_KNOTS ( 'NONE', 3,
 ( #30699, #33645, #6893, #40552, #41259, #28350 ),
 .UNSPECIFIED., .F., .F.,
 ( 4, 2, 4 ),
 ( 2.380731629582122378E-07, 0.002336973833157553367, 0.004673709593152147908 ),
 .UNSPECIFIED. ) ;
#63623 = MANIFOLD_SOLID_BREP ( 'HeadChamfer', #6963 ) ;
#63624 = CARTESIAN_POINT ( 'NONE',  ( -53.31111153860302210, 37.18770477615724701, 40.00000000000003553 ) ) ;
#63625 = VERTEX_POINT ( 'NONE', #26526 ) ;
#63626 = CARTESIAN_POINT ( 'NONE',  ( 173.6737675136086523, 72.80308721038092301, 62.45876396626458416 ) ) ;
#63627 = ORIENTED_EDGE ( 'NONE', *, *, #8704, .T. ) ;
#63628 = AXIS2_PLACEMENT_3D ( 'NONE', #69365, #15899, #10612 ) ;
#63629 = CARTESIAN_POINT ( 'NONE',  ( -71.59086462055191191, 19.75139532313339075, -18.27088716436448479 ) ) ;
#63630 = CARTESIAN_POINT ( 'NONE',  ( 63.69186821587121017, 39.51023455020778385, 41.38025477438755928 ) ) ;
#63631 = CARTESIAN_POINT ( 'NONE',  ( 209.9518228411288874, 20.00000000000003197, 31.43423095485942298 ) ) ;
#63632 = VECTOR ( 'NONE', #9788, 1000.000000000000000 ) ;
#63634 = VERTEX_POINT ( 'NONE', #69428 ) ;
#63633 = CARTESIAN_POINT ( 'NONE',  ( 150.0278556977734752, 53.32860603304212788, 11.14328715965509176 ) ) ;
#63635 = CARTESIAN_POINT ( 'NONE',  ( -177.1539090641757923, 91.73101548694627638, 44.66073844826994588 ) ) ;
#63636 = CARTESIAN_POINT ( 'NONE',  ( 10.65073749997984898, 36.82468443433825911, 13.32819299319723960 ) ) ;
#63637 = EDGE_CURVE ( 'NONE', #59026, #69403, #40238, .T. ) ;
#63638 = ADVANCED_FACE ( 'NONE', ( #65551 ), #36877, .T. ) ;
#63639 = CARTESIAN_POINT ( 'NONE',  ( 116.5100763992442836, 33.01539745157280237, -39.29511836571368377 ) ) ;
#63640 = CONICAL_SURFACE ( 'NONE', #54628, 4.171999999999999709, 0.7853981633974437271 ) ;
#63641 = ORIENTED_EDGE ( 'NONE', *, *, #10769, .F. ) ;
#63642 = CARTESIAN_POINT ( 'NONE',  ( 16.54503815046424009, 18.74197728628641002, 0.000000000000000000 ) ) ;
#63643 = EDGE_CURVE ( 'NONE', #41303, #14641, #30155, .T. ) ;
#63644 = PLANE ( 'NONE',  #10852 ) ;
#63645 = CARTESIAN_POINT ( 'NONE',  ( 0.000000000000000000, 0.000000000000000000, 41.38025477438755928 ) ) ;
#63646 = AXIS2_PLACEMENT_3D ( 'NONE', #67922, #57356, #4243 ) ;
#63647 = CARTESIAN_POINT ( 'NONE',  ( 135.6651581599209919, 42.52720121194705172, 56.57256158429925819 ) ) ;
#63648 = CARTESIAN_POINT ( 'NONE',  ( 204.6977192012829789, -170.0000000000000000, -43.82593103262159673 ) ) ;
#63649 = LINE ( 'NONE', #57330, #14335 ) ;
#63650 = DIRECTION ( 'NONE',  ( 1.000000000000000000, 3.700743415417210977E-14, 0.000000000000000000 ) ) ;
#63651 = ORIENTED_EDGE ( 'NONE', *, *, #65922, .T. ) ;
#63652 = CARTESIAN_POINT ( 'NONE',  ( 46.51679720856117228, 10.46086439153923742, 8.146061147039359795 ) ) ;
#63653 = EDGE_LOOP ( 'NONE', ( #60443, #32539, #18392, #41987 ) ) ;
#63654 = CARTESIAN_POINT ( 'NONE',  ( 150.4722669492348643, 53.65054032737658929, -19.49086022515975358 ) ) ;
#63655 = CARTESIAN_POINT ( 'NONE',  ( -61.68940124183720286, 16.56194981783060172, 94.99999999999866418 ) ) ;
#63656 = DIRECTION ( 'NONE',  ( -0.000000000000000000, -1.000000000000000000, -0.000000000000000000 ) ) ;
#63657 = CARTESIAN_POINT ( 'NONE',  ( -151.6716822472524484, 66.03661194063732864, -76.35210402040455335 ) ) ;
#63658 = CARTESIAN_POINT ( 'NONE',  ( -109.5542371224815810, 36.63223321375210162, 89.85165753065791705 ) ) ;
#63659 = B_SPLINE_CURVE_WITH_KNOTS ( 'NONE', 3,
 ( #15587, #21206, #36700, #15921, #58821, #27159, #53540, #26825, #48252, #32450, #27506, #64807, #16607, #32793, #54224, #6047, #50709, #39129, #33148, #44745, #6754, #60567, #13090, #49302, #29260, #2526, #1843, #60912, #11677, #7809, #49650, #54933, #16948, #12384, #61267, #22939, #1478, #44381, #54584, #23980, #33505, #50008, #6409, #1135, #65870, #17665, #22586, #34555, #12037, #44026 ),
 .UNSPECIFIED., .F., .F.,
 ( 4, 2, 2, 2, 2, 2, 2, 2, 2, 2, 2, 2, 2, 2, 2, 2, 2, 2, 2, 2, 2, 2, 2, 2, 4 ),
 ( 0.03126542424884329319, 0.03330676804260272739, 0.03534811183636216853, 0.03738945563012160966, 0.03943079942388104386, 0.04045147132076077484, 0.04147214321764051276, 0.04249281511452024374, 0.04351348701139998165, 0.04555483080515944361, 0.04657550270203918152, 0.04759617459891891944, 0.04810651054735878146, 0.04861684649579864348, 0.04963751839267835364, 0.05065819028955807768, 0.05167886218643778784, 0.05269953408331751188, 0.05372020598019722204, 0.05474087787707693220, 0.05576154977395665624, 0.05780289356771613207, 0.05984423736147560791, 0.06188558115523508374, 0.06392692494899455957 ),
 .UNSPECIFIED. ) ;
#63660 = PLANE ( 'NONE',  #2212 ) ;
#63661 = CARTESIAN_POINT ( 'NONE',  ( 205.1049299651095907, 106.9023875785546238, -36.32593103262159673 ) ) ;
#63662 = LINE ( 'NONE', #48471, #57974 ) ;
#63663 = ORIENTED_EDGE ( 'NONE', *, *, #16289, .T. ) ;
#63664 = DIRECTION ( 'NONE',  ( -0.04486483035050447404, -0.9989930665413151445, 0.000000000000000000 ) ) ;
#63665 = ORIENTED_EDGE ( 'NONE', *, *, #27390, .F. ) ;
#63666 = CARTESIAN_POINT ( 'NONE',  ( -72.21947956767111521, 21.03570528348188873, 60.92218443414460438 ) ) ;
#63667 = CARTESIAN_POINT ( 'NONE',  ( -102.2801239173131194, 32.78103895658057354, -35.01457726497591239 ) ) ;
#63668 = CARTESIAN_POINT ( 'NONE',  ( 55.51547041749727640, 11.05727559334827070, -70.30740390392726624 ) ) ;
#63669 = CARTESIAN_POINT ( 'NONE',  ( 0.000000000000000000, 0.000000000000000000, 40.00000000000003553 ) ) ;
#63670 = CARTESIAN_POINT ( 'NONE',  ( 21.74799039132244260, 7.772294950329607488, 42.09455586677241001 ) ) ;
#63671 = CARTESIAN_POINT ( 'NONE',  ( 160.2883311361769643, 61.16711613734476316, -63.51461744484596039 ) ) ;
#63672 = VERTEX_POINT ( 'NONE', #64501 ) ;
#63673 = CARTESIAN_POINT ( 'NONE',  ( -89.99999999999998579, 1.102182119232617596E-14, -7.000000000000000000 ) ) ;
#63674 = DIRECTION ( 'NONE',  ( -1.000000000000000000, -0.000000000000000000, -0.000000000000000000 ) ) ;
#63675 = EDGE_LOOP ( 'NONE', ( #33767, #38306, #49252, #14818 ) ) ;
#63676 = ORIENTED_EDGE ( 'NONE', *, *, #44691, .F. ) ;
#63677 = CARTESIAN_POINT ( 'NONE',  ( -149.5074843970971017, 64.17983161892347255, 45.72082123989907387 ) ) ;
#63678 = CARTESIAN_POINT ( 'NONE',  ( 61.33627421985469397, 12.28939706835343237, -35.90714437952212990 ) ) ;
#63679 = DIRECTION ( 'NONE',  ( -1.000000000000000000, 0.000000000000000000, 0.000000000000000000 ) ) ;
#63680 = CIRCLE ( 'NONE', #63628, 243.4957430088094839 ) ;
#63681 = FACE_OUTER_BOUND ( 'NONE', #62662, .T. ) ;
#63682 = EDGE_CURVE ( 'NONE', #61969, #67011, #26243, .T. ) ;
#63683 = CARTESIAN_POINT ( 'NONE',  ( -145.5261806899006842, 60.87473129144527917, 5.016016613215474429 ) ) ;
#63684 = VERTEX_POINT ( 'NONE', #22280 ) ;
#63685 = CARTESIAN_POINT ( 'NONE',  ( -130.5811943660945076, 50.88295841537572528, 32.24531123205569827 ) ) ;
#63686 = VECTOR ( 'NONE', #50804, 1000.000000000000000 ) ;
#63687 = EDGE_LOOP ( 'NONE', ( #16290, #24344 ) ) ;
#63688 = CARTESIAN_POINT ( 'NONE',  ( 34.45972925205163762, 8.830088223935252500, -21.93772383615038635 ) ) ;
#63689 = CARTESIAN_POINT ( 'NONE',  ( 31.11269837220806522, 0.000000000000000000, 0.000000000000000000 ) ) ;
#63690 = CARTESIAN_POINT ( 'NONE',  ( 205.5004956747123117, 107.4493581495447927, 29.23987150799703727 ) ) ;
#63691 = CARTESIAN_POINT ( 'NONE',  ( -2.869721780807583666, 7.625909776230887616, 70.11086547301624705 ) ) ;
#63692 = CIRCLE ( 'NONE', #33369, 65.00000000000000000 ) ;
#63693 = EDGE_CURVE ( 'NONE', #30206, #69370, #57111, .T. ) ;
#63694 = B_SPLINE_CURVE_WITH_KNOTS ( 'NONE', 3,
 ( #3332, #40272, #8266, #30073, #3671, #13203, #29718, #18817, #67707, #51180, #29370, #40611, #61720, #35000, #19157, #24793, #40962, #56104, #19501, #35344, #46231, #56441, #2995, #36031, #62062, #2301, #30759, #45543, #8622, #51526, #61378, #7920, #50823, #14238, #8960, #24454, #25146, #45895, #2642, #30407, #56803, #51861, #46577 ),
 .UNSPECIFIED., .F., .F.,
 ( 4, 2, 2, 2, 2, 2, 2, 2, 2, 2, 2, 1, 2, 2, 2, 2, 2, 2, 2, 2, 2, 4 ),
 ( 0.02515559250233026511, 0.02674001423437957076, 0.02753222510040422011, 0.02832443596642887293, 0.02990885769847824449, 0.03149327943052761258, 0.03307770116257698761, 0.03386991202860167860, 0.03466212289462636265, 0.03624654462667570298, 0.03703875549270038009, 0.03783096635872505720, 0.03862317722474973430, 0.03941538809077441141, 0.04099980982282376563, 0.04258423155487311290, 0.04337644242089779001, 0.04416865328692246712, 0.04575307501897181439, 0.04733749675102115473, 0.04892191848307049507, 0.05050634021511984234 ),
 .UNSPECIFIED. ) ;
#63695 = CIRCLE ( 'NONE', #3053, 25.00000000000145306 ) ;
#63696 = EDGE_CURVE ( 'NONE', #61334, #52913, #6795, .T. ) ;
#63697 = VERTEX_POINT ( 'NONE', #17712 ) ;
#63698 = EDGE_CURVE ( 'NONE', #62198, #43392, #16133, .T. ) ;
#63699 = ORIENTED_EDGE ( 'NONE', *, *, #62346, .F. ) ;
#63700 = LINE ( 'NONE', #15510, #22182 ) ;
#63701 = CARTESIAN_POINT ( 'NONE',  ( -125.4034380163612212, 47.37464824346550074, 84.30384953410292326 ) ) ;
#63702 = CARTESIAN_POINT ( 'NONE',  ( -125.8938041572051389, -170.0000000000000000, -49.91370389823397602 ) ) ;
#63703 = CARTESIAN_POINT ( 'NONE',  ( 46.76173513940489812, 58.63736118510233553, 43.58025477438756212 ) ) ;
#63704 = CARTESIAN_POINT ( 'NONE',  ( 70.25990036603481315, 14.47042233282420298, 39.27062401723128460 ) ) ;
#63705 = CARTESIAN_POINT ( 'NONE',  ( 8.285723989432073111, 7.382582932371003714, 90.57384125127391883 ) ) ;
#63706 = EDGE_CURVE ( 'NONE', #45015, #25409, #26770, .T. ) ;
#63707 = VERTEX_POINT ( 'NONE', #40537 ) ;
#63708 = CARTESIAN_POINT ( 'NONE',  ( 112.3013380801408800, 395.0000000000065938, -128.9497041420121093 ) ) ;
#63709 = CARTESIAN_POINT ( 'NONE',  ( -94.88380767928867954, 29.17964217339916644, 66.13299744995647700 ) ) ;
#63710 = EDGE_LOOP ( 'NONE', ( #63049, #38788, #2987, #63930 ) ) ;
#63711 = CARTESIAN_POINT ( 'NONE',  ( -84.23431294393863311, 24.52078568147204507, 6.024674515077490078 ) ) ;
#63712 = ORIENTED_EDGE ( 'NONE', *, *, #30224, .T. ) ;
#63713 = ORIENTED_EDGE ( 'NONE', *, *, #43876, .F. ) ;
#63714 = ORIENTED_EDGE ( 'NONE', *, *, #42167, .T. ) ;
#63715 = CARTESIAN_POINT ( 'NONE',  ( -120.0051930351106506, 43.92079660368832350, 15.92705009691551865 ) ) ;
#63716 = CARTESIAN_POINT ( 'NONE',  ( -176.3791001330698975, 90.82833141237288999, 71.93620537013939042 ) ) ;
#63717 = CARTESIAN_POINT ( 'NONE',  ( 130.3245512970360664, 39.33195360491890824, 70.48796868334781607 ) ) ;
#63718 = EDGE_LOOP ( 'NONE', ( #25931, #31943, #19285, #8221 ) ) ;
#63719 = VECTOR ( 'NONE', #10830, 1000.000000000000000 ) ;
#63720 = B_SPLINE_CURVE_WITH_KNOTS ( 'NONE', 3,
 ( #60736, #18183, #50187, #55819, #35055, #39980, #23470, #56497, #29772, #8678, #51235, #51582, #39634, #61090, #3052, #24846, #46285, #50537, #23809, #56155, #45251, #61439, #34717, #7972, #35753, #14966, #47313, #30816, #57203, #52262, #68772, #36092, #53277, #42050, #25203, #48002, #41709, #46637 ),
 .UNSPECIFIED., .F., .F.,
 ( 4, 2, 2, 2, 2, 2, 2, 2, 2, 2, 2, 2, 2, 2, 2, 2, 2, 2, 4 ),
 ( 1.387778780781445676E-17, 0.003908178031105413383, 0.005862267046658129616, 0.007816356062210845848, 0.009770445077763562081, 0.01172453409331627831, 0.01270157860109262862, 0.01367862310886898240, 0.01465566761664533271, 0.01563271212442168476, 0.01660975663219804027, 0.01758680113997438538, 0.01954089015552708253, 0.02051793466330342416, 0.02149497917107976580, 0.02344906818663246642, 0.02540315720218516357, 0.02735724621773786766, 0.03126542424884323768 ),
 .UNSPECIFIED. ) ;
#63721 = ADVANCED_FACE ( 'NONE', ( #19427 ), #8544, .F. ) ;
#63722 = CARTESIAN_POINT ( 'NONE',  ( -38.94401347518159895, 10.94428672445531348, 91.58116192842672376 ) ) ;
#63723 = VECTOR ( 'NONE', #37885, 1000.000000000000000 ) ;
#63724 = CARTESIAN_POINT ( 'NONE',  ( 149.9872551245000807, 52.05943539582076340, 37.48403949321973982 ) ) ;
#63725 = CARTESIAN_POINT ( 'NONE',  ( 0.000000000000000000, 0.000000000000000000, -5.000000000000000000 ) ) ;
#63726 = APPLICATION_CONTEXT ( 'automotive_design' ) ;
#63727 = CARTESIAN_POINT ( 'NONE',  ( 103.1653143050726271, 25.74301230421576747, -40.88985240790263020 ) ) ;
#63728 = CARTESIAN_POINT ( 'NONE',  ( -30.94753041835915752, 9.510749728915508072, 45.21645440618920020 ) ) ;
#63729 = VECTOR ( 'NONE', #40493, 1000.000000000000000 ) ;
#63730 = CARTESIAN_POINT ( 'NONE',  ( 0.000000000000000000, 0.000000000000000000, 0.000000000000000000 ) ) ;
#63731 = EDGE_LOOP ( 'NONE', ( #68350, #26370, #40603, #57776, #22039, #13470, #42986, #67840, #45556 ) ) ;
#63732 = VECTOR ( 'NONE', #46925, 1000.000000000000000 ) ;
#63733 = LINE ( 'NONE', #46857, #10690 ) ;
#63734 = CARTESIAN_POINT ( 'NONE',  ( -3.660532965668825245, 7.124194613927617326, -9.500000000000007105 ) ) ;
#63735 = FACE_OUTER_BOUND ( 'NONE', #36991, .T. ) ;
#63736 = CARTESIAN_POINT ( 'NONE',  ( -118.8392474096541918, 43.20060570451233417, -45.01293686198101796 ) ) ;
#63737 = CARTESIAN_POINT ( 'NONE',  ( -82.93126516400698733, 25.07709093823495650, 4.899509067904407544 ) ) ;
#63738 = VECTOR ( 'NONE', #26778, 1000.000000000000000 ) ;
#63739 = CARTESIAN_POINT ( 'NONE',  ( 14.99999999999998579, 0.000000000000000000, 0.000000000000000000 ) ) ;
#63740 = CARTESIAN_POINT ( 'NONE',  ( 34.47024887486590217, 7.819232357299694236, -91.15458136497296948 ) ) ;
#63741 = CARTESIAN_POINT ( 'NONE',  ( 34.43940527065477397, -66.63700071734618291, 170.0000000000000000 ) ) ;
#63742 = CARTESIAN_POINT ( 'NONE',  ( 70.50372867914781239, 14.53505678900966380, 10.95890223166102118 ) ) ;
#63743 = CARTESIAN_POINT ( 'NONE',  ( -80.32755469740935439, 24.04130076192508270, 72.08040740567068383 ) ) ;
#63744 = CARTESIAN_POINT ( 'NONE',  ( -109.7078892845591582, 36.71702188566216307, 39.09037949355451502 ) ) ;
#63745 = VERTEX_POINT ( 'NONE', #13805 ) ;
#63746 = VECTOR ( 'NONE', #566, 1000.000000000000000 ) ;
#63747 = CARTESIAN_POINT ( 'NONE',  ( -56.32964631401103617, 16.07016196819930087, 84.08885397732279898 ) ) ;
#63748 = ORIENTED_EDGE ( 'NONE', *, *, #13270, .F. ) ;
#63749 = LINE ( 'NONE', #26799, #37407 ) ;
#63750 = VERTEX_POINT ( 'NONE', #44787 ) ;
#63751 = CARTESIAN_POINT ( 'NONE',  ( 22.90619343622340764, 7.840927939412484449, -72.27737759400322659 ) ) ;
#63752 = PLANE ( 'NONE',  #10270 ) ;
#63753 = CARTESIAN_POINT ( 'NONE',  ( -65.20298343242134820, 4.613322252417262348, 41.38025477438755928 ) ) ;
#63754 = DIRECTION ( 'NONE',  ( 1.000000000000000000, 1.001918829714556097E-14, -9.899279560275163638E-15 ) ) ;
#63755 = CARTESIAN_POINT ( 'NONE',  ( 140.4641697461912884, 46.75994457266055804, -39.93676995691901510 ) ) ;
#63756 = CARTESIAN_POINT ( 'NONE',  ( -51.77431913897919458, 14.86466849149170777, -62.79783711398949464 ) ) ;
#63757 = CARTESIAN_POINT ( 'NONE',  ( 151.6351261592328683, 53.25263237790398563, -38.90572743852373350 ) ) ;
#63758 = CARTESIAN_POINT ( 'NONE',  ( 149.4165763529819344, -26.99999999999998224, 129.0000000000000000 ) ) ;
#63759 = CARTESIAN_POINT ( 'NONE',  ( -8.712114576423529044, -23.56346432108879441, 3.061616997868437868E-16 ) ) ;
#63760 = ORIENTED_EDGE ( 'NONE', *, *, #19931, .T. ) ;
#63761 = EDGE_CURVE ( 'NONE', #22952, #33925, #32093, .T. ) ;
#63762 = ORIENTED_EDGE ( 'NONE', *, *, #3064, .T. ) ;
#63763 = EDGE_CURVE ( 'NONE', #27226, #52905, #66604, .T. ) ;
#63764 = CARTESIAN_POINT ( 'NONE',  ( 24.34427655538949509, 5.688250960946272805, 0.000000000000000000 ) ) ;
#63765 = FILL_AREA_STYLE ('',( #27757 ) ) ;
#63766 = EDGE_CURVE ( 'NONE', #43079, #14540, #3561, .T. ) ;
#63767 = CARTESIAN_POINT ( 'NONE',  ( 131.2739575565289272, 41.05411765250562439, -90.16079167367058744 ) ) ;
#63768 = DIRECTION ( 'NONE',  ( 0.000000000000000000, 0.000000000000000000, 1.000000000000000000 ) ) ;
#63769 = DIRECTION ( 'NONE',  ( -1.000000000000000000, 0.000000000000000000, 0.000000000000000000 ) ) ;
#63770 = DIRECTION ( 'NONE',  ( 0.000000000000000000, 1.000000000000000000, -0.000000000000000000 ) ) ;
#63771 = CARTESIAN_POINT ( 'NONE',  ( 176.4367926094704728, 74.03315361639846515, -76.46119564883423436 ) ) ;
#63772 = AXIS2_PLACEMENT_3D ( 'NONE', #24785, #61713, #2633 ) ;
#63773 = DIRECTION ( 'NONE',  ( 1.000000000000000000, 0.000000000000000000, 0.000000000000000000 ) ) ;
#63774 = CARTESIAN_POINT ( 'NONE',  ( 89.21005684773500377, 20.31770592753387916, -23.52307059860430627 ) ) ;
#63775 = CYLINDRICAL_SURFACE ( 'NONE', #48788, 7.500000000000013323 ) ;
#63776 = DIRECTION ( 'NONE',  ( 0.000000000000000000, 0.000000000000000000, 1.000000000000000000 ) ) ;
#63777 = DIRECTION ( 'NONE',  ( 0.000000000000000000, -0.000000000000000000, -1.000000000000000000 ) ) ;
#63778 = VECTOR ( 'NONE', #35046, 1000.000000000000000 ) ;
#63779 = EDGE_CURVE ( 'NONE', #53742, #28520, #57270, .T. ) ;
#63780 = ORIENTED_EDGE ( 'NONE', *, *, #12961, .F. ) ;
#63781 = VECTOR ( 'NONE', #62044, 1000.000000000000227 ) ;
#63782 = EDGE_CURVE ( 'NONE', #10029, #47318, #56515, .T. ) ;
#63783 = DIRECTION ( 'NONE',  ( -1.000000000000000000, 0.000000000000000000, 0.000000000000000000 ) ) ;
#63784 = LINE ( 'NONE', #31763, #3581 ) ;
#63785 = DIRECTION ( 'NONE',  ( 0.000000000000000000, -1.000000000000000000, 0.000000000000000000 ) ) ;
#63786 = PLANE ( 'NONE',  #41097 ) ;
#63787 = DIRECTION ( 'NONE',  ( 1.387778780781445429E-16, -1.000000000000000000, -3.081487911019577365E-33 ) ) ;
#63788 = CARTESIAN_POINT ( 'NONE',  ( -5.583677117989181760, 7.762972448524147140, 84.14020024624272764 ) ) ;
#63789 = AXIS2_PLACEMENT_3D ( 'NONE', #58765, #17245, #37662 ) ;
#63790 = VERTEX_POINT ( 'NONE', #69345 ) ;
#63791 = DIRECTION ( 'NONE',  ( -1.000000000000000000, 0.000000000000000000, 0.000000000000000000 ) ) ;
#63792 = DIRECTION ( 'NONE',  ( 0.000000000000000000, 0.000000000000000000, 1.000000000000000000 ) ) ;
#63793 = ORIENTED_EDGE ( 'NONE', *, *, #17869, .T. ) ;
#63794 = ORIENTED_EDGE ( 'NONE', *, *, #65532, .T. ) ;
#63795 = CARTESIAN_POINT ( 'NONE',  ( 39.08704187494956983, 9.383114233299528095, 83.60237209767953459 ) ) ;
#63796 = DIRECTION ( 'NONE',  ( 1.000000000000000000, -0.000000000000000000, 0.000000000000000000 ) ) ;
#63797 = CARTESIAN_POINT ( 'NONE',  ( 110.2429982417149574, -170.0000000000000000, 63.95576479620102361 ) ) ;
#63798 = ORIENTED_EDGE ( 'NONE', *, *, #23136, .F. ) ;
#63799 = FACE_OUTER_BOUND ( 'NONE', #11524, .T. ) ;
#63800 = CARTESIAN_POINT ( 'NONE',  ( -6.840981040171510763, 6.828436339979224279, 18.22255534678397026 ) ) ;
#63801 = CARTESIAN_POINT ( 'NONE',  ( 32.90878072717890745, 7.653588083204842185, -12.51371383138284443 ) ) ;
#63802 = CARTESIAN_POINT ( 'NONE',  ( 159.2325040199866635, 60.31699144791972600, 44.25496482726027381 ) ) ;
#63803 = CARTESIAN_POINT ( 'NONE',  ( 164.0443904173016847, 62.94849960635616526, 86.97141621194363381 ) ) ;
#63804 = DIRECTION ( 'NONE',  ( 0.000000000000000000, 0.000000000000000000, 1.000000000000000000 ) ) ;
#63805 = EDGE_LOOP ( 'NONE', ( #37733, #64617, #33946, #66576 ) ) ;
#63806 = CARTESIAN_POINT ( 'NONE',  ( 103.1695711638930959, 26.83837309506523638, -19.12163667725788940 ) ) ;
#63807 = CARTESIAN_POINT ( 'NONE',  ( 0.000000000000000000, 0.000000000000000000, 73.58025477438756923 ) ) ;
#63808 = LINE ( 'NONE', #63462, #35226 ) ;
#63809 = CARTESIAN_POINT ( 'NONE',  ( 204.3129818922372749, 107.5244029525887868, 29.20772073876942443 ) ) ;
#63810 = DIRECTION ( 'NONE',  ( 0.000000000000000000, -0.000000000000000000, -1.000000000000000000 ) ) ;
#63812 = ORIENTED_EDGE ( 'NONE', *, *, #23350, .T. ) ;
#63811 = DIRECTION ( 'NONE',  ( 0.9959742939952397345, -0.08963930890342655666, 0.000000000000000000 ) ) ;
#63813 = ORIENTED_EDGE ( 'NONE', *, *, #69144, .T. ) ;
#63814 = ORIENTED_EDGE ( 'NONE', *, *, #34434, .T. ) ;
#63815 = CARTESIAN_POINT ( 'NONE',  ( 112.1100957124161539, 30.86846953551572525, -77.54606385092635890 ) ) ;
#63816 = DIRECTION ( 'NONE',  ( -0.000000000000000000, 1.000000000000000000, -0.000000000000000000 ) ) ;
#63817 = CARTESIAN_POINT ( 'NONE',  ( 197.8572563162090319, 97.41072138832259952, -67.58039613982114702 ) ) ;
#63818 = CARTESIAN_POINT ( 'NONE',  ( -31.92572261726339633, 10.69135962481465008, 57.06100499665285497 ) ) ;
#63819 = CARTESIAN_POINT ( 'NONE',  ( -14.56151485655250788, 8.434196591921333308, -19.40760647807576333 ) ) ;
#63820 = CIRCLE ( 'NONE', #66057, 5.000000000000004441 ) ;
#63821 = CARTESIAN_POINT ( 'NONE',  ( 155.2910738464913720, 55.97560547655807284, -77.65936666156605384 ) ) ;
#63822 = CARTESIAN_POINT ( 'NONE',  ( 17.48889770758267304, 6.561062909825354339, -23.48319453253814260 ) ) ;
#63823 = CARTESIAN_POINT ( 'NONE',  ( -155.5978531700835958, 69.52241200678682276, -37.92872988257907707 ) ) ;
#63824 = ORIENTED_EDGE ( 'NONE', *, *, #54686, .T. ) ;
#63825 = ORIENTED_EDGE ( 'NONE', *, *, #7578, .F. ) ;
#63826 = VECTOR ( 'NONE', #48175, 1000.000000000000000 ) ;
#63827 = DIRECTION ( 'NONE',  ( 0.000000000000000000, 1.000000000000000000, -0.000000000000000000 ) ) ;
#63828 = CARTESIAN_POINT ( 'NONE',  ( -84.55783695959763691, 25.74181993349145614, -37.94774160841574684 ) ) ;
#63829 = CARTESIAN_POINT ( 'NONE',  ( 106.0226973295788468, 26.97779350220217154, 84.59144110998217059 ) ) ;
#63830 = CARTESIAN_POINT ( 'NONE',  ( -154.8006992380338716, 70.15733562427989511, 16.71094074788830497 ) ) ;
#63831 = EDGE_CURVE ( 'NONE', #55220, #45879, #27922, .T. ) ;
#63832 = STYLED_ITEM ( 'NONE', ( #52560 ), #63623 ) ;
#63833 = CARTESIAN_POINT ( 'NONE',  ( -21.27554331372908081, -61.43430442924895374, 170.0000000000000000 ) ) ;
#63834 = CARTESIAN_POINT ( 'NONE',  ( 23.28785143291466397, 6.856621069835718174, 37.01352062635557161 ) ) ;
#63835 = CARTESIAN_POINT ( 'NONE',  ( -156.9646383917485650, 72.14225053943575006, 91.09065068128420251 ) ) ;
#63836 = EDGE_LOOP ( 'NONE', ( #60580, #68505, #55270, #67981 ) ) ;
#63837 = ORIENTED_EDGE ( 'NONE', *, *, #13025, .F. ) ;
#63838 = EDGE_CURVE ( 'NONE', #59358, #23153, #43622, .T. ) ;
#63839 = ORIENTED_EDGE ( 'NONE', *, *, #1260, .F. ) ;
#63840 = CIRCLE ( 'NONE', #25649, 5.000000000000004441 ) ;
#63841 = CARTESIAN_POINT ( 'NONE',  ( 75.00000000000000000, 1.249999999999979350, 170.0000000000000000 ) ) ;
#63842 = EDGE_CURVE ( 'NONE', #66387, #39196, #20252, .T. ) ;
#63843 = CARTESIAN_POINT ( 'NONE',  ( 91.42704446803595886, 22.18527496519091713, -91.23189972359006106 ) ) ;
#63844 = CARTESIAN_POINT ( 'NONE',  ( 103.1665074762347700, 25.74358939450902639, -94.59055577750497434 ) ) ;
#63846 = MANIFOLD_SOLID_BREP ( 'Cut-Extrude1[4]', #8076 ) ;
#63845 = ADVANCED_FACE ( 'NONE', ( #58776 ), #16911, .F. ) ;
#63847 = CARTESIAN_POINT ( 'NONE',  ( -31.43908319763709969, 9.591432048623765638, 57.06100499665286208 ) ) ;
#63848 = CARTESIAN_POINT ( 'NONE',  ( -154.2585856850054995, 68.31650218414620213, -21.27640989008226313 ) ) ;
#63849 = ORIENTED_EDGE ( 'NONE', *, *, #40424, .T. ) ;
#63850 = CARTESIAN_POINT ( 'NONE',  ( 184.5867277229703802, 83.68414666546580349, 70.28875302066492736 ) ) ;
#63851 = CARTESIAN_POINT ( 'NONE',  ( 10.13405324523498408, 6.385324379632245417, -21.12665790197542037 ) ) ;
#63852 = CARTESIAN_POINT ( 'NONE',  ( 21.74799039132244260, 7.772294950329608376, 15.25000527630873393 ) ) ;
#63853 = CARTESIAN_POINT ( 'NONE',  ( 188.0141161196705752, 85.90515114331884661, 66.53510735707675394 ) ) ;
#63854 = DIRECTION ( 'NONE',  ( -0.7071067811865473507, -1.232595164407830946E-32, 0.7071067811865476838 ) ) ;
#63855 = CARTESIAN_POINT ( 'NONE',  ( -78.66644367742111399, 22.32174330031317311, -35.11545063171788428 ) ) ;
#63856 = CARTESIAN_POINT ( 'NONE',  ( 21.44031696305384571, 6.747195267824411147, 69.31344765735015301 ) ) ;
#63857 = DIRECTION ( 'NONE',  ( -0.000000000000000000, -1.000000000000000000, -0.000000000000000000 ) ) ;
#63858 = CARTESIAN_POINT ( 'NONE',  ( 8.480977594057446112, 7.382886909400592224, 8.963374414903345411 ) ) ;
#63859 = EDGE_CURVE ( 'NONE', #64139, #51909, #29470, .T. ) ;
#63860 = VERTEX_POINT ( 'NONE', #18671 ) ;
#63861 = CARTESIAN_POINT ( 'NONE',  ( 184.3994103300443896, 82.02159554764426730, 16.70644533388108144 ) ) ;
#63862 = CONTEXT_DEPENDENT_SHAPE_REPRESENTATION ( #39482, #13120 ) ;
#63863 = PLANE ( 'NONE',  #24035 ) ;
#63864 = CARTESIAN_POINT ( 'NONE',  ( 48.39383208188379371, 43.94028683479089636, 43.58025477438756212 ) ) ;
#63865 = CARTESIAN_POINT ( 'NONE',  ( -107.0544991134679265, 36.41543129049374983, -48.30370310564277503 ) ) ;
#63866 = CARTESIAN_POINT ( 'NONE',  ( 181.5079096844946491, 80.47139261082473638, -51.22505766587965326 ) ) ;
#63867 = ORIENTED_EDGE ( 'NONE', *, *, #51765, .T. ) ;
#63868 = EDGE_LOOP ( 'NONE', ( #25312, #55846, #27936, #54520 ) ) ;
#63869 = CARTESIAN_POINT ( 'NONE',  ( 200.0000000000000000, 0.000000000000000000, 10.00000000000000000 ) ) ;
#63870 = CARTESIAN_POINT ( 'NONE',  ( -18.15845058245935562, -17.18344181019548955, 0.000000000000000000 ) ) ;
#63871 = VERTEX_POINT ( 'NONE', #23944 ) ;
#63872 = AXIS2_PLACEMENT_3D ( 'NONE', #32800, #793, #37726 ) ;
#63873 = CARTESIAN_POINT ( 'NONE',  ( 110.2429982417149290, 28.88204397445231209, 56.45576479620100940 ) ) ;
#63874 = ORIENTED_EDGE ( 'NONE', *, *, #2460, .T. ) ;
#63875 = DIRECTION ( 'NONE',  ( 1.000000000000000000, 1.387778780781445429E-16, 0.000000000000000000 ) ) ;
#63876 = CARTESIAN_POINT ( 'NONE',  ( 132.9440032680862771, 40.87616997986732059, 29.56257473360772892 ) ) ;
#63877 = FACE_OUTER_BOUND ( 'NONE', #67608, .T. ) ;
#63878 = CARTESIAN_POINT ( 'NONE',  ( -99.97541017369786687, 31.62502926470687470, 45.17167492092433179 ) ) ;
#63879 = AXIS2_PLACEMENT_3D ( 'NONE', #43383, #64328, #33016 ) ;
#63880 = CARTESIAN_POINT ( 'NONE',  ( 93.92280655489132357, 22.03989931749466535, -45.08756213313548500 ) ) ;
#63882 = VERTEX_POINT ( 'NONE', #45392 ) ;
#63881 = DIRECTION ( 'NONE',  ( 0.000000000000000000, -0.1086713087885527451, -0.9940777367219241212 ) ) ;
#63883 = VERTEX_POINT ( 'NONE', #61232 ) ;
#63884 = ORIENTED_EDGE ( 'NONE', *, *, #31692, .T. ) ;
#63885 = DIRECTION ( 'NONE',  ( -1.000000000000000000, 0.000000000000000000, 0.000000000000000000 ) ) ;
#63886 = CARTESIAN_POINT ( 'NONE',  ( -31.43908319763710679, -170.0000000000000000, -23.47264677473818395 ) ) ;
#63887 = CARTESIAN_POINT ( 'NONE',  ( -180.6011569556094969, 95.85968111394262792, -15.99745918700219072 ) ) ;
#63888 = CARTESIAN_POINT ( 'NONE',  ( -172.3038663181179970, 87.72015621195184565, -61.55650775521367990 ) ) ;
#63890 = ORIENTED_EDGE ( 'NONE', *, *, #53254, .F. ) ;
#63889 = CARTESIAN_POINT ( 'NONE',  ( -146.1260528621667731, 61.36307454672302697, -49.02329722400514811 ) ) ;
#63891 = CARTESIAN_POINT ( 'NONE',  ( 312.3372781065084496, 394.9999999999999432, -21.44970414201177888 ) ) ;
#63892 = VERTEX_POINT ( 'NONE', #24303 ) ;
#63894 = ADVANCED_FACE ( 'NONE', ( #34515 ), #2490, .T. ) ;
#63893 = CARTESIAN_POINT ( 'NONE',  ( -133.1527834403230486, 51.46311219732123732, 40.02479403497597588 ) ) ;
#63895 = CARTESIAN_POINT ( 'NONE',  ( -61.86403937395562025, 16.61416349803656800, -12.72252382116044522 ) ) ;
#63896 = CARTESIAN_POINT ( 'NONE',  ( -96.43817545481738307, 31.02509717589733640, 60.13372018734977331 ) ) ;
#63897 = CARTESIAN_POINT ( 'NONE',  ( -132.2161740628506550, 52.03204870034954865, -73.30095993089241801 ) ) ;
#63898 = CARTESIAN_POINT ( 'NONE',  ( -55.05276343752909440, 14.68156374112638929, -77.06087458892358200 ) ) ;
#63899 = DIRECTION ( 'NONE',  ( 0.000000000000000000, -1.000000000000000000, 0.000000000000000000 ) ) ;
#63900 = CARTESIAN_POINT ( 'NONE',  ( -100.4262673593280368, 31.84860241619272969, -62.07669865031897416 ) ) ;
#63901 = ORIENTED_EDGE ( 'NONE', *, *, #35581, .F. ) ;
#63902 = ORIENTED_EDGE ( 'NONE', *, *, #12389, .T. ) ;
#63903 = LINE ( 'NONE', #64597, #12496 ) ;
#63904 = DIRECTION ( 'NONE',  ( 0.000000000000000000, 0.000000000000000000, -1.000000000000000000 ) ) ;
#63905 = DIRECTION ( 'NONE',  ( 0.000000000000000000, -0.000000000000000000, -1.000000000000000000 ) ) ;
#63906 = CARTESIAN_POINT ( 'NONE',  ( 103.5849290181279088, 27.01613348792540847, -73.72874238742858211 ) ) ;
#63907 = CARTESIAN_POINT ( 'NONE',  ( -71.17984086584779391, 20.67393782512344558, 38.43314760115057993 ) ) ;
#63908 = CARTESIAN_POINT ( 'NONE',  ( 81.03898448521319153, 17.58847173596443270, 32.18774333821972533 ) ) ;
#63909 = CARTESIAN_POINT ( 'NONE',  ( 69.36287815987334682, 15.27486453472191208, -47.22355319605652824 ) ) ;
#63910 = CARTESIAN_POINT ( 'NONE',  ( -122.8011284400168108, 45.68452922414294193, 31.27179024729560908 ) ) ;
#63911 = FACE_OUTER_BOUND ( 'NONE', #66503, .T. ) ;
#63912 = ORIENTED_EDGE ( 'NONE', *, *, #16588, .T. ) ;
#63913 = CARTESIAN_POINT ( 'NONE',  ( -104.1244073710070239, 33.72720758483612258, -8.385545890535196278 ) ) ;
#63914 = EDGE_CURVE ( 'NONE', #65364, #7527, #50669, .T. ) ;
#63915 = ORIENTED_EDGE ( 'NONE', *, *, #34936, .T. ) ;
#63916 = CARTESIAN_POINT ( 'NONE',  ( -11.14880195267006968, 7.129907723790826601, -36.17668213044176184 ) ) ;
#63917 = DIRECTION ( 'NONE',  ( 0.6579387259397028176, 0.7530714660036196273, 2.500042656554810340E-16 ) ) ;
#63918 = CARTESIAN_POINT ( 'NONE',  ( 88.98820631332498010, 21.30618275724810573, 56.92102499358249901 ) ) ;
#63919 = CARTESIAN_POINT ( 'NONE',  ( 150.9184679586219033, 52.73111408630722963, -13.12037300805640783 ) ) ;
#63920 = CARTESIAN_POINT ( 'NONE',  ( -46.06722295615723795, -46.37372919877119415, 41.38025477438755928 ) ) ;
#63921 = VECTOR ( 'NONE', #65178, 1000.000000000000000 ) ;
#63922 = VECTOR ( 'NONE', #2900, 1000.000000000000000 ) ;
#63923 = CARTESIAN_POINT ( 'NONE',  ( 31.96227686234409759, 7.558148489540045034, -70.94545158898284853 ) ) ;
#63924 = CARTESIAN_POINT ( 'NONE',  ( -95.60805465865863084, 30.63099276904602419, -72.82232827928781660 ) ) ;
#63925 = EDGE_CURVE ( 'NONE', #22108, #36497, #2086, .T. ) ;
#63926 = CARTESIAN_POINT ( 'NONE',  ( -31.93169728792082651, 10.69234447276976852, -8.472646774738153752 ) ) ;
#63927 = AXIS2_PLACEMENT_3D ( 'NONE', #23561, #7730, #12655 ) ;
#63928 = ORIENTED_EDGE ( 'NONE', *, *, #27948, .F. ) ;
#63929 = FACE_OUTER_BOUND ( 'NONE', #43454, .T. ) ;
#63930 = ORIENTED_EDGE ( 'NONE', *, *, #321, .T. ) ;
#63931 = DIRECTION ( 'NONE',  ( 0.000000000000000000, 0.000000000000000000, 1.000000000000000000 ) ) ;
#63932 = CARTESIAN_POINT ( 'NONE',  ( 10.83521140779422609, 7.398743030771587570, -75.51647902447882643 ) ) ;
#63933 = CARTESIAN_POINT ( 'NONE',  ( -27.70005010046227412, 9.007417901453017350, 17.37802900940060624 ) ) ;
#63934 = FACE_OUTER_BOUND ( 'NONE', #54076, .T. ) ;
#63935 = CARTESIAN_POINT ( 'NONE',  ( -6.840981040171507210, 6.828436339979226055, 45.06710593724763214 ) ) ;
#63936 = LINE ( 'NONE', #15747, #63632 ) ;
#63937 = CARTESIAN_POINT ( 'NONE',  ( 150.0980941434704903, 53.37942190380065455, -45.02911393569248588 ) ) ;
#63938 = EDGE_CURVE ( 'NONE', #55116, #25227, #9497, .T. ) ;
#63939 = ORIENTED_EDGE ( 'NONE', *, *, #43807, .T. ) ;
#63940 = DIRECTION ( 'NONE',  ( 0.1884548733085519845, -2.077167649210491653E-15, 0.9820818503191358628 ) ) ;
#63941 = CARTESIAN_POINT ( 'NONE',  ( -152.5101325120252795, 68.10842280990928543, 71.95230034876590253 ) ) ;
#63943 = EDGE_CURVE ( 'NONE', #61153, #22625, #53869, .T. ) ;
#63942 = CARTESIAN_POINT ( 'NONE',  ( 0.000000000000000000, 0.000000000000000000, 40.00000000000003553 ) ) ;
#63944 = EDGE_CURVE ( 'NONE', #59754, #41324, #25689, .T. ) ;
#63945 = CARTESIAN_POINT ( 'NONE',  ( -109.0291978193666438, 37.49173305805086898, 61.58271146452185718 ) ) ;
#63946 = CARTESIAN_POINT ( 'NONE',  ( -129.4036885357273832, 50.06837984316182144, -35.78160727525695961 ) ) ;
#63947 = EDGE_LOOP ( 'NONE', ( #50899, #36164, #31355, #648 ) ) ;
#63948 = DIRECTION ( 'NONE',  ( -0.000000000000000000, -1.000000000000000000, -0.000000000000000000 ) ) ;
#63949 = CARTESIAN_POINT ( 'NONE',  ( 92.53566308513175898, 21.52138666710688142, 68.70529524960606693 ) ) ;
#63950 = CARTESIAN_POINT ( 'NONE',  ( 197.6329787101074658, 98.74106466892200729, -19.51727163173970681 ) ) ;
#63951 = CARTESIAN_POINT ( 'NONE',  ( -142.0117116388610157, 58.07347023268670227, 91.60223103192235783 ) ) ;
#63952 = CARTESIAN_POINT ( 'NONE',  ( 140.4586216751744701, 45.55624550472996503, 33.44244638526205193 ) ) ;
#63953 = ORIENTED_EDGE ( 'NONE', *, *, #26622, .T. ) ;
#63954 = FACE_OUTER_BOUND ( 'NONE', #13918, .T. ) ;
#63955 = DIRECTION ( 'NONE',  ( 0.000000000000000000, 0.000000000000000000, 1.000000000000000000 ) ) ;
#63956 = CARTESIAN_POINT ( 'NONE',  ( 163.1313205310724186, 63.49733392291055623, 14.99077136729292015 ) ) ;
#63957 = CYLINDRICAL_SURFACE ( 'NONE', #57774, 7.500000000000020428 ) ;
#63958 = AXIS2_PLACEMENT_3D ( 'NONE', #67804, #20293, #19254 ) ;
#63959 = ORIENTED_EDGE ( 'NONE', *, *, #62148, .T. ) ;
#63960 = CARTESIAN_POINT ( 'NONE',  ( 173.9405361758639117, 73.05302209498822208, 65.95550401125700546 ) ) ;
#63961 = ORIENTED_EDGE ( 'NONE', *, *, #13762, .F. ) ;
#63962 = CARTESIAN_POINT ( 'NONE',  ( -106.6781182590523400, 35.07133425426479079, -36.42098577216694366 ) ) ;
#63963 = CARTESIAN_POINT ( 'NONE',  ( 63.01563776193091826, 12.67277567978498176, -77.56524142263344856 ) ) ;
#63964 = CARTESIAN_POINT ( 'NONE',  ( 2.905661822261151883E-14, 15.55634918610403084, 0.000000000000000000 ) ) ;
#63965 = AXIS2_PLACEMENT_3D ( 'NONE', #19774, #62340, #57068 ) ;
#63967 = VERTEX_POINT ( 'NONE', #47804 ) ;
#63966 = CARTESIAN_POINT ( 'NONE',  ( 155.2870855780214754, 57.23765125306422163, 17.25424900018499486 ) ) ;
#63968 = CARTESIAN_POINT ( 'NONE',  ( 160.5018603162735076, 61.33906090758085838, -50.49884186580090528 ) ) ;
#63969 = CARTESIAN_POINT ( 'NONE',  ( -4.364688291132434728, -24.74039788130350459, 3.061616997868437868E-16 ) ) ;
#63970 = COLOUR_RGB ( '',0.7921568627450980005, 0.8196078431372548767, 0.9333333333333333481 ) ;
#63971 = CARTESIAN_POINT ( 'NONE',  ( -15.76129977463437015, -63.43731725181460490, 41.38025477438755928 ) ) ;
#63972 = EDGE_LOOP ( 'NONE', ( #38348, #35619, #55071, #12589 ) ) ;
#63973 = EDGE_CURVE ( 'NONE', #62155, #18800, #56009, .T. ) ;
#63974 = CARTESIAN_POINT ( 'NONE',  ( 0.000000000000000000, -6.928203230275509661, -3.999999999999999112 ) ) ;
#63975 = EDGE_CURVE ( 'NONE', #30581, #39218, #56386, .T. ) ;
#63976 = CARTESIAN_POINT ( 'NONE',  ( 138.6020257460769756, 44.36414356192208430, 69.68300242728969351 ) ) ;
#63977 = DIRECTION ( 'NONE',  ( -0.000000000000000000, 1.000000000000000000, -0.000000000000000000 ) ) ;
#63978 = CARTESIAN_POINT ( 'NONE',  ( -38.69408084385329971, 10.89529537250242974, -67.69614563400999430 ) ) ;
#63979 = ORIENTED_EDGE ( 'NONE', *, *, #59128, .F. ) ;
#63980 = CARTESIAN_POINT ( 'NONE',  ( 42.71680114082826663, 9.880016734137541334, 17.31480560921531975 ) ) ;
#63981 = ORIENTED_EDGE ( 'NONE', *, *, #25925, .F. ) ;
#63982 = ORIENTED_EDGE ( 'NONE', *, *, #18850, .T. ) ;
#63983 = VECTOR ( 'NONE', #15709, 1000.000000000000114 ) ;
#63984 = FACE_OUTER_BOUND ( 'NONE', #27696, .T. ) ;
#63985 = CARTESIAN_POINT ( 'NONE',  ( -62.21707580470530274, 16.72016638215685447, 93.81846384057118371 ) ) ;
#63986 = DIRECTION ( 'NONE',  ( -1.000000000000000000, 0.000000000000000000, 0.000000000000000000 ) ) ;
#63987 = CARTESIAN_POINT ( 'NONE',  ( -152.5067928559255392, 66.76529500553621688, -76.04591788159349619 ) ) ;
#63988 = CARTESIAN_POINT ( 'NONE',  ( -108.8294929810133880, 36.23425003200458860, 88.03925474513930283 ) ) ;
#63989 = CARTESIAN_POINT ( 'NONE',  ( 188.2950976467627413, 87.71503060978560029, 12.04681166319859997 ) ) ;
#63990 = EDGE_CURVE ( 'NONE', #53396, #57040, #15117, .T. ) ;
#63991 = CARTESIAN_POINT ( 'NONE',  ( -131.1078488676298832, 50.02394948559179255, 70.36092292693098216 ) ) ;
#63992 = CARTESIAN_POINT ( 'NONE',  ( -8.062763165560543399, 40.94272254494899244, 13.79046340968178264 ) ) ;
#63993 = EDGE_CURVE ( 'NONE', #18531, #19486, #20735, .T. ) ;
#63994 = ORIENTED_EDGE ( 'NONE', *, *, #8680, .F. ) ;
#63995 = DIRECTION ( 'NONE',  ( 0.000000000000000000, -1.000000000000000000, 0.000000000000000000 ) ) ;
#63996 = ORIENTED_EDGE ( 'NONE', *, *, #68607, .F. ) ;
#63997 = CARTESIAN_POINT ( 'NONE',  ( -75.00452312211128003, 22.03104735285382887, 58.21301458073671142 ) ) ;
#63998 = CARTESIAN_POINT ( 'NONE',  ( 182.5617509987552864, 80.11195108039726165, 29.45250294282221404 ) ) ;
#63999 = ADVANCED_FACE ( 'NONE', ( #10173 ), #10862, .F. ) ;
#64000 = CARTESIAN_POINT ( 'NONE',  ( 57.08336938683661543, 11.37442068895389191, -65.44980484747004823 ) ) ;
#64001 = B_SPLINE_CURVE_WITH_KNOTS ( 'NONE', 3,
 ( #15903, #15213, #41599, #5000, #69009, #9943, #58127, #32083, #42293, #52156, #31399, #35983, #42632, #25786, #63755, #46882, #64089, #52830, #47212, #57782, #42962, #9249, #68344, #20147, #37344, #53519, #20482, #30706, #41946, #58456, #63058, #3973, #14862, #10271, #58797, #48233, #10613, #36327, #5351, #4652, #63410, #9596, #58, #21518, #31058, #26114, #52502, #12016 ),
 .UNSPECIFIED., .F., .F.,
 ( 4, 2, 2, 2, 2, 2, 2, 2, 2, 2, 2, 2, 2, 2, 2, 2, 2, 2, 2, 2, 2, 2, 2, 4 ),
 ( 6.938893903907228378E-18, 0.001591515129442207981, 0.003183030258884409023, 0.003978787823605504231, 0.004774545388326600741, 0.006366060517768843199, 0.007957575647211086525, 0.009549090776653329851, 0.01034484834137445845, 0.01114060590609558532, 0.01193636347081671219, 0.01273212103553784079, 0.01432363616498011881, 0.01591515129442239510, 0.01671090885914353064, 0.01750666642386466271, 0.01830242398858579825, 0.01909818155330693379, 0.02068969668274925344, 0.02148545424747042021, 0.02228121181219158697, 0.02387272694163384071, 0.02466848450635493462, 0.02546424207107603199 ),
 .UNSPECIFIED. ) ;
#64002 = CARTESIAN_POINT ( 'NONE',  ( -76.32962633615586867, 21.44528079176259538, 3.942966790981714098 ) ) ;
#64003 = CARTESIAN_POINT ( 'NONE',  ( -122.1940143064357187, 45.29738883755586443, 71.49263784387757426 ) ) ;
#64004 = CARTESIAN_POINT ( 'NONE',  ( 23.24047374271773592, 7.861801299833796719, 38.49384045076077143 ) ) ;
#64005 = EDGE_CURVE ( 'NONE', #42885, #37440, #13331, .T. ) ;
#64006 = CARTESIAN_POINT ( 'NONE',  ( 198.6830395803476108, 98.44480157511503648, 85.91292533661551545 ) ) ;
#64007 = VECTOR ( 'NONE', #64416, 1000.000000000000000 ) ;
#64008 = CARTESIAN_POINT ( 'NONE',  ( -417.6627218934913230, 219.4906275429376308, -144.4497041420118819 ) ) ;
#64009 = ORIENTED_EDGE ( 'NONE', *, *, #63366, .F. ) ;
#64010 = CARTESIAN_POINT ( 'NONE',  ( 11.70038247058342051, 40.05515948024370232, 13.79046412305353009 ) ) ;
#64011 = CARTESIAN_POINT ( 'NONE',  ( -172.7116702014379825, 86.67317892691258407, 72.66624519710477159 ) ) ;
#64012 = ORIENTED_EDGE ( 'NONE', *, *, #26494, .T. ) ;
#64013 = EDGE_LOOP ( 'NONE', ( #18952, #16279, #61927, #27914 ) ) ;
#64014 = CARTESIAN_POINT ( 'NONE',  ( -25.79929641484369185, 9.749255553662443674, -74.63048772539220010 ) ) ;
#64015 = CARTESIAN_POINT ( 'NONE',  ( 0.000000000000000000, 0.000000000000000000, 170.0000000000000000 ) ) ;
#64016 = LINE ( 'NONE', #38576, #25578 ) ;
#64017 = DIRECTION ( 'NONE',  ( -0.000000000000000000, -1.000000000000000000, -0.000000000000000000 ) ) ;
#64018 = CARTESIAN_POINT ( 'NONE',  ( -149.0782809666403921, 63.81577337591404131, 3.876270649435374693 ) ) ;
#64019 = ADVANCED_FACE ( 'NONE', ( #27731 ), #11201, .T. ) ;
#64020 = ORIENTED_EDGE ( 'NONE', *, *, #39021, .T. ) ;
#64021 = EDGE_LOOP ( 'NONE', ( #5637, #29908, #49364, #35167 ) ) ;
#64022 = EDGE_CURVE ( 'NONE', #14720, #59570, #42859, .T. ) ;
#64023 = ADVANCED_FACE ( 'NONE', ( #300 ), #48817, .F. ) ;
#64024 = AXIS2_PLACEMENT_3D ( 'NONE', #40513, #41212, #62673 ) ;
#64025 = CARTESIAN_POINT ( 'NONE',  ( -133.1640943168118838, 52.70734926280005794, 39.98146393653333064 ) ) ;
#64026 = EDGE_LOOP ( 'NONE', ( #66044, #3934, #55608, #40057, #52904 ) ) ;
#64027 = LINE ( 'NONE', #338, #10987 ) ;
#64028 = PLANE ( 'NONE',  #45057 ) ;
#64029 = CARTESIAN_POINT ( 'NONE',  ( 58.47673920847985585, 11.66523265296355305, 58.16705259761723568 ) ) ;
#64030 = PLANE ( 'NONE',  #65511 ) ;
#64031 = LINE ( 'NONE', #59084, #41444 ) ;
#64032 = FACE_BOUND ( 'NONE', #24825, .T. ) ;
#64033 = ORIENTED_EDGE ( 'NONE', *, *, #54565, .F. ) ;
#64034 = VERTEX_POINT ( 'NONE', #49169 ) ;
#64035 = CARTESIAN_POINT ( 'NONE',  ( 74.39890044415633952, 7.951074708187157114, 0.000000000000000000 ) ) ;
#64036 = LINE ( 'NONE', #31680, #45102 ) ;
#64037 = CARTESIAN_POINT ( 'NONE',  ( -165.7689197919845014, 79.30072199592279958, -13.85662846433732831 ) ) ;
#64038 = CARTESIAN_POINT ( 'NONE',  ( 137.3958226571046737, 43.60243650158410134, -76.99682858792697004 ) ) ;
#64039 = CARTESIAN_POINT ( 'NONE',  ( 44.99999999999999289, 22.99999999999998579, 4.000000000000000000 ) ) ;
#64040 = VECTOR ( 'NONE', #60178, 1000.000000000000000 ) ;
#64041 = CARTESIAN_POINT ( 'NONE',  ( -189.4248691432192402, 107.3461292335514514, -70.68823927268300622 ) ) ;
#64042 = EDGE_LOOP ( 'NONE', ( #25013, #42254, #47960, #4161 ) ) ;
#64043 = CARTESIAN_POINT ( 'NONE',  ( -95.19652294162979445, 29.32558722310179888, 67.38094733532032876 ) ) ;
#64044 = ORIENTED_EDGE ( 'NONE', *, *, #65765, .F. ) ;
#64045 = DIRECTION ( 'NONE',  ( 0.000000000000000000, 1.000000000000000000, -0.000000000000000000 ) ) ;
#64046 = ORIENTED_EDGE ( 'NONE', *, *, #52805, .F. ) ;
#64047 = ORIENTED_EDGE ( 'NONE', *, *, #31698, .T. ) ;
#64048 = CARTESIAN_POINT ( 'NONE',  ( -120.1346137380981958, 44.00127440773565723, 6.464595127001305563 ) ) ;
#64049 = CARTESIAN_POINT ( 'NONE',  ( -179.6470915626256613, 94.69856161161349917, 61.45973726863883968 ) ) ;
#64050 = CARTESIAN_POINT ( 'NONE',  ( 20.37135563017390183, 6.690359945346087578, 16.62731626407598640 ) ) ;
#64051 = VERTEX_POINT ( 'NONE', #32670 ) ;
#64052 = B_SPLINE_CURVE_WITH_KNOTS ( 'NONE', 3,
 ( #21407, #36908, #37234, #58346, #47790, #53059, #4887, #58685, #53402, #27028, #32662, #16131, #5908, #59033, #10855, #21749, #27370, #43196, #64673, #16480, #37935, #59380, #68571, #20373, #60075, #18225, #48810, #23157, #28419, #65021, #16816, #39334, #34060, #66437, #2057, #50235, #44950, #54800, #39676, #12601, #33373, #49872, #61136, #12959 ),
 .UNSPECIFIED., .F., .F.,
 ( 4, 2, 2, 2, 2, 2, 2, 2, 2, 2, 2, 2, 2, 2, 2, 2, 2, 2, 2, 2, 2, 4 ),
 ( 0.02908143158676661927, 0.03095422299093867138, 0.03282701439511072350, 0.03469980579928277908, 0.03657259720345483467, 0.03844538860762689025, 0.04031818001179893890, 0.04125457571388495281, 0.04219097141597095979, 0.04312736711805697370, 0.04359556496909998413, 0.04406376282014300150, 0.04500015852222903623, 0.04593655422431506402, 0.04687294992640109181, 0.04780934562848712654, 0.04968213703265919601, 0.05155492843683127935, 0.05342771984100334881, 0.05530051124517543215, 0.05717330264934750855, 0.05904609405351958495 ),
 .UNSPECIFIED. ) ;
#64053 = CARTESIAN_POINT ( 'NONE',  ( -444.4229916354184411, 394.6798985497180752, 96.40978294693171335 ) ) ;
#64054 = EDGE_CURVE ( 'NONE', #56182, #9547, #68358, .T. ) ;
#64055 = CARTESIAN_POINT ( 'NONE',  ( 150.7926588734435427, 52.63999027731880176, 40.33416883845127643 ) ) ;
#64056 = CARTESIAN_POINT ( 'NONE',  ( 10.01137213834873840, 64.59476928204603041, 43.58025477438756212 ) ) ;
#64057 = CARTESIAN_POINT ( 'NONE',  ( 63.01563776193090405, 13.70579113808098271, 71.65751152968501003 ) ) ;
#64058 = CARTESIAN_POINT ( 'NONE',  ( -20.55634918610403261, 2.818925648462311528E-14, 2.000000000000001776 ) ) ;
#64059 = CARTESIAN_POINT ( 'NONE',  ( -23.93965512371325133, 8.480096402797091315, 37.21140884057258802 ) ) ;
#64060 = CARTESIAN_POINT ( 'NONE',  ( -13.24252603915519444, -63.63674649211960599, 40.00000000000003553 ) ) ;
#64061 = ORIENTED_EDGE ( 'NONE', *, *, #46932, .F. ) ;
#64062 = MANIFOLD_SOLID_BREP ( 'Angle iron 35 X 35 X 5(3)', #63158 ) ;
#64063 = AXIS2_PLACEMENT_3D ( 'NONE', #897, #34665, #54696 ) ;
#64064 = FACE_BOUND ( 'NONE', #29196, .T. ) ;
#64065 = CARTESIAN_POINT ( 'NONE',  ( -24.40147488398704567, -5.437648709335880071, 0.000000000000000000 ) ) ;
#64066 = CARTESIAN_POINT ( 'NONE',  ( -85.66184035008927822, 26.20110535976566979, -66.74364312913436947 ) ) ;
#64067 = CARTESIAN_POINT ( 'NONE',  ( -149.5074843970971017, 65.50121172469319220, -7.968279941028269420 ) ) ;
#64068 = DIRECTION ( 'NONE',  ( 0.000000000000000000, 1.000000000000000000, -0.000000000000000000 ) ) ;
#64069 = CARTESIAN_POINT ( 'NONE',  ( -80.31482177285911916, 24.03632224640839610, 3.753151970507568436 ) ) ;
#64070 = DIRECTION ( 'NONE',  ( -1.000000000000000000, 0.000000000000000000, -0.000000000000000000 ) ) ;
#64071 = CARTESIAN_POINT ( 'NONE',  ( -5.767955557622883589E-14, -31.11269837220806878, 85.00100000000000477 ) ) ;
#64072 = ADVANCED_FACE ( 'NONE', ( #1010 ), #28079, .F. ) ;
#64073 = CARTESIAN_POINT ( 'NONE',  ( -118.4106078162223525, 42.93830006159887347, -68.68850339543098471 ) ) ;
#64074 = CARTESIAN_POINT ( 'NONE',  ( 67.93926590385571274, 13.86859831467923065, 16.14705051833222171 ) ) ;
#64075 = CARTESIAN_POINT ( 'NONE',  ( -85.12122836439576190, 25.97531040437156591, 68.61395634379843500 ) ) ;
#64076 = CARTESIAN_POINT ( 'NONE',  ( 41.44377882552309700, 9.699415982225042754, -89.58024731985329936 ) ) ;
#64077 = EDGE_LOOP ( 'NONE', ( #11178, #45614 ) ) ;
#64078 = CONTEXT_DEPENDENT_SHAPE_REPRESENTATION ( #859, #40641 ) ;
#64079 = ORIENTED_EDGE ( 'NONE', *, *, #65508, .F. ) ;
#64080 = ADVANCED_FACE ( 'NONE', ( #38642 ), #59728, .T. ) ;
#64081 = LINE ( 'NONE', #37338, #350 ) ;
#64082 = ORIENTED_EDGE ( 'NONE', *, *, #12077, .T. ) ;
#64083 = ADVANCED_FACE ( 'NONE', ( #11538 ), #16140, .F. ) ;
#64084 = CARTESIAN_POINT ( 'NONE',  ( 20.35964562795319921, 7.697260051881319676, -63.89753274017193263 ) ) ;
#64085 = FILL_AREA_STYLE ('',( #63053 ) ) ;
#64086 = CARTESIAN_POINT ( 'NONE',  ( -146.1140637052939155, 62.65471088530802035, 58.36122317852547070 ) ) ;
#64087 = CARTESIAN_POINT ( 'NONE',  ( -8.663926357538780820, -23.45072237845004182, 0.000000000000000000 ) ) ;
#64088 = CIRCLE ( 'NONE', #37120, 8.000000000000000000 ) ;
#64089 = CARTESIAN_POINT ( 'NONE',  ( 140.8855094313933023, 47.03549517811089231, -40.89384161477261870 ) ) ;
#64090 = CARTESIAN_POINT ( 'NONE',  ( 209.8197250501989970, 115.4463023161200823, -92.02305923795135811 ) ) ;
#64091 = DIRECTION ( 'NONE',  ( 2.220446049250313081E-16, 0.000000000000000000, 1.000000000000000000 ) ) ;
#64092 = CYLINDRICAL_SURFACE ( 'NONE', #14993, 7.500000000000020428 ) ;
#64093 = VERTEX_POINT ( 'NONE', #27379 ) ;
#64094 = ORIENTED_EDGE ( 'NONE', *, *, #30263, .F. ) ;
#64095 = CARTESIAN_POINT ( 'NONE',  ( 70.51601918574517924, 14.53832276813547431, -42.98226787025442519 ) ) ;
#64096 = SHAPE_REPRESENTATION ( 'cutting blade 2', ( #66832 ), #44451 ) ;
#64097 = CARTESIAN_POINT ( 'NONE',  ( -55.05276343752910151, 14.68156374112637330, -88.90542517938719413 ) ) ;
#64098 = CARTESIAN_POINT ( 'NONE',  ( -17.50000000000002842, -18.06806526123148160, 0.000000000000000000 ) ) ;
#64099 = PRODUCT_DEFINITION_CONTEXT ( 'detailed design', #33228, 'design' ) ;
#64100 = VECTOR ( 'NONE', #27398, 1000.000000000000000 ) ;
#64101 = DIRECTION ( 'NONE',  ( -0.000000000000000000, -0.000000000000000000, -1.000000000000000000 ) ) ;
#64102 = ORIENTED_EDGE ( 'NONE', *, *, #25292, .T. ) ;
#64103 = EDGE_CURVE ( 'NONE', #47168, #21445, #9958, .T. ) ;
#64104 = CARTESIAN_POINT ( 'NONE',  ( 88.52077179907877280, 21.14145351760140557, 17.62907072079950410 ) ) ;
#64105 = CARTESIAN_POINT ( 'NONE',  ( 188.0094179620990928, 87.39792407168452826, -19.77360373632219392 ) ) ;
#64106 = CARTESIAN_POINT ( 'NONE',  ( 212.1913428512246753, 119.0779339498137688, 9.508615975002843612 ) ) ;
#64107 = SHAPE_REPRESENTATION_RELATIONSHIP ( 'NONE' , 'NONE' ,  #32051, #45848 ) ;
#64108 = CARTESIAN_POINT ( 'NONE',  ( -180.3158531669106708, 95.51092859788505507, -44.35178396430072922 ) ) ;
#64109 = CARTESIAN_POINT ( 'NONE',  ( -17.50000000000002842, -18.06806526123148160, 378.0000000000000000 ) ) ;
#64110 = DIRECTION ( 'NONE',  ( -0.000000000000000000, 1.000000000000000000, -0.000000000000000000 ) ) ;
#64111 = CARTESIAN_POINT ( 'NONE',  ( 105.0320943261246356, 21.99263847259266669, 0.6545153999150219448 ) ) ;
#64112 = EDGE_CURVE ( 'NONE', #39615, #51018, #969, .T. ) ;
#64113 = CARTESIAN_POINT ( 'NONE',  ( 164.8908506817023181, 64.97619709085121542, 64.87856429165069017 ) ) ;
#64114 = ORIENTED_EDGE ( 'NONE', *, *, #10872, .T. ) ;
#64115 = FACE_OUTER_BOUND ( 'NONE', #68950, .T. ) ;
#64116 = CARTESIAN_POINT ( 'NONE',  ( -56.28348399776042044, 22.91216519805203333, -19.22558936715843814 ) ) ;
#64117 = CARTESIAN_POINT ( 'NONE',  ( 155.2870855780215891, 57.23765125306421453, 70.94335018111237900 ) ) ;
#64118 = CARTESIAN_POINT ( 'NONE',  ( 0.000000000000000000, 0.000000000000000000, 0.000000000000000000 ) ) ;
#64119 = CARTESIAN_POINT ( 'NONE',  ( 150.8925291903904053, 52.71218673668931842, 6.422435693488909969 ) ) ;
#64120 = CYLINDRICAL_SURFACE ( 'NONE', #10847, 5.000000000000004441 ) ;
#64121 = VERTEX_POINT ( 'NONE', #50242 ) ;
#64122 = FACE_OUTER_BOUND ( 'NONE', #17768, .T. ) ;
#64123 = CARTESIAN_POINT ( 'NONE',  ( 6.400000000000000355, 4.618802153517004960, 7.999999999999998224 ) ) ;
#64124 = ORIENTED_EDGE ( 'NONE', *, *, #40347, .F. ) ;
#64125 = ORIENTED_EDGE ( 'NONE', *, *, #62746, .T. ) ;
#64126 = CARTESIAN_POINT ( 'NONE',  ( 33.04185335729066253, 8.678858904955234266, 87.11446200076579771 ) ) ;
#64127 = CARTESIAN_POINT ( 'NONE',  ( 0.000000000000000000, 35.00000000000000000, 0.000000000000000000 ) ) ;
#64128 = FACE_OUTER_BOUND ( 'NONE', #32939, .T. ) ;
#64129 = VERTEX_POINT ( 'NONE', #17887 ) ;
#64130 = CARTESIAN_POINT ( 'NONE',  ( -62.49130718206700408, 16.80297926264070796, -70.55131870819045048 ) ) ;
#64131 = VECTOR ( 'NONE', #25092, 1000.000000000000000 ) ;
#64132 = CARTESIAN_POINT ( 'NONE',  ( -5.412684891282530053, 7.753215344827987465, 3.652707060347378576 ) ) ;
#64133 = CARTESIAN_POINT ( 'NONE',  ( 174.9161599490640810, 73.97365196673304411, -48.00021783180836366 ) ) ;
#64134 = FACE_OUTER_BOUND ( 'NONE', #41383, .T. ) ;
#64135 = CARTESIAN_POINT ( 'NONE',  ( 68.07999999999999829, 0.000000000000000000, 30.00000000000000000 ) ) ;
#64136 = AXIS2_PLACEMENT_3D ( 'NONE', #29354, #67350, #40257 ) ;
#64137 = PRODUCT_DEFINITION_SHAPE ( 'NONE', 'NONE',  #9991 ) ;
#64138 = EDGE_CURVE ( 'NONE', #19844, #15020, #60446, .T. ) ;
#64139 = VERTEX_POINT ( 'NONE', #28431 ) ;
#64140 = SURFACE_STYLE_FILL_AREA ( #52209 ) ;
#64141 = EDGE_CURVE ( 'NONE', #56268, #50425, #21199, .T. ) ;
#64142 = DIRECTION ( 'NONE',  ( -0.000000000000000000, -1.000000000000000000, -0.000000000000000000 ) ) ;
#64143 = CARTESIAN_POINT ( 'NONE',  ( 10.15118267943872432, 7.391905976536037315, 32.56151896041566118 ) ) ;
#64144 = CARTESIAN_POINT ( 'NONE',  ( 201.9721407532274782, 104.3507814346147597, 43.70693720603514265 ) ) ;
#64145 = CARTESIAN_POINT ( 'NONE',  ( 0.000000000000000000, 0.000000000000000000, -10.00000000000000000 ) ) ;
#64147 = EDGE_LOOP ( 'NONE', ( #63665, #52649, #48380, #15295, #31770, #60145, #8725, #53371, #62512 ) ) ;
#64146 = CARTESIAN_POINT ( 'NONE',  ( -447.6627218934919483, 370.0000000000064233, -141.4497041420121661 ) ) ;
#64148 = ORIENTED_EDGE ( 'NONE', *, *, #38703, .T. ) ;
#64149 = ORIENTED_EDGE ( 'NONE', *, *, #50575, .T. ) ;
#64150 = CARTESIAN_POINT ( 'NONE',  ( 0.000000000000000000, 0.000000000000000000, 30.00000000000000000 ) ) ;
#64151 = CARTESIAN_POINT ( 'NONE',  ( 112.3013380801408658, 388.0000000000065938, -123.9497041420121235 ) ) ;
#64152 = FACE_OUTER_BOUND ( 'NONE', #63479, .T. ) ;
#64153 = EDGE_CURVE ( 'NONE', #6514, #55030, #39189, .T. ) ;
#64154 = CARTESIAN_POINT ( 'NONE',  ( -37.52119286077852678, 11.69341290629619756, 60.16572187417437334 ) ) ;
#64155 = CARTESIAN_POINT ( 'NONE',  ( -15.07533778868020669, 8.482826962130836534, -14.13728325526587781 ) ) ;
#64156 = CARTESIAN_POINT ( 'NONE',  ( 149.9872551245001375, 52.05943539582077051, -69.89416286863497874 ) ) ;
#64157 = CARTESIAN_POINT ( 'NONE',  ( 2.129405171194075130, 25.03204795498856683, 3.061616997868437868E-16 ) ) ;
#64158 = CARTESIAN_POINT ( 'NONE',  ( -46.66904755831212981, -15.55634918610397222, 2.000000000000001776 ) ) ;
#64159 = EDGE_LOOP ( 'NONE', ( #35733, #42375, #15086, #47329 ) ) ;
#64160 = ADVANCED_FACE ( 'NONE', ( #39343 ), #13312, .F. ) ;
#64161 = ORIENTED_EDGE ( 'NONE', *, *, #20549, .F. ) ;
#64162 = EDGE_CURVE ( 'NONE', #35195, #60279, #1708, .T. ) ;
#64163 = CARTESIAN_POINT ( 'NONE',  ( 63.50537371531942199, 13.81987663608982331, -8.876140241706055534 ) ) ;
#64164 = CARTESIAN_POINT ( 'NONE',  ( -80.32755469740935439, 24.04130076192510046, -35.29779495618403473 ) ) ;
#64165 = DIRECTION ( 'NONE',  ( 0.000000000000000000, 1.000000000000000000, -0.000000000000000000 ) ) ;
#64166 = CARTESIAN_POINT ( 'NONE',  ( 116.6436511186860656, 33.08230081168870385, -12.66062602132463866 ) ) ;
#64167 = CARTESIAN_POINT ( 'NONE',  ( 50.98853755884153571, 388.0000000000071054, 101.0502958579881465 ) ) ;
#64168 = CYLINDRICAL_SURFACE ( 'NONE', #41564, 10.00000000000000178 ) ;
#64169 = CARTESIAN_POINT ( 'NONE',  ( -156.6359381387761118, 71.83770944710386175, 89.57239090401904491 ) ) ;
#64170 = ORIENTED_EDGE ( 'NONE', *, *, #1847, .T. ) ;
#64171 = VERTEX_POINT ( 'NONE', #2064 ) ;
#64172 = ORIENTED_EDGE ( 'NONE', *, *, #37320, .T. ) ;
#64173 = CARTESIAN_POINT ( 'NONE',  ( -156.1477286774994298, 71.38742644140637594, -11.97128653975141965 ) ) ;
#64174 = CARTESIAN_POINT ( 'NONE',  ( 37.45439421541016145, 9.177432671831375899, -35.86035370546551349 ) ) ;
#64175 = MANIFOLD_SOLID_BREP ( 'Cut-Extrude1[2]', #22676 ) ;
#64176 = AXIS2_PLACEMENT_3D ( 'NONE', #6317, #1050, #44291 ) ;
#64177 = CARTESIAN_POINT ( 'NONE',  ( -35.17600017528511103, 10.23461991275926586, 58.05366031714377328 ) ) ;
#64178 = CARTESIAN_POINT ( 'NONE',  ( 198.7123879174244223, 100.1053816708572697, 59.02484461029090568 ) ) ;
#64179 = ORIENTED_EDGE ( 'NONE', *, *, #6934, .F. ) ;
#64180 = LINE ( 'NONE', #65587, #8765 ) ;
#64181 = CARTESIAN_POINT ( 'NONE',  ( -156.9910258076866398, 70.79617246506501260, 64.49172258714661154 ) ) ;
#64182 = CIRCLE ( 'NONE', #13688, 21.00000000000000355 ) ;
#64183 = CARTESIAN_POINT ( 'NONE',  ( 18.19858669090299230, 7.596860100017451600, 17.77656158943756992 ) ) ;
#64184 = FILL_AREA_STYLE_COLOUR ( '', #40836 ) ;
#64185 = FACE_OUTER_BOUND ( 'NONE', #4423, .T. ) ;
#64186 = CARTESIAN_POINT ( 'NONE',  ( -85.75947274862032543, 25.15128705015478516, -45.10382441638937934 ) ) ;
#64188 = ADVANCED_FACE ( 'NONE', ( #55873 ), #33724, .T. ) ;
#64187 = CARTESIAN_POINT ( 'NONE',  ( 23.09784929786603058, 6.844738137842329984, 66.05627411941513571 ) ) ;
#64189 = CARTESIAN_POINT ( 'NONE',  ( -64.97888516016280391, 7.103257987405394935, 43.58025477438756212 ) ) ;
#64190 = CARTESIAN_POINT ( 'NONE',  ( 12.03317402819681980, 6.409531826169462043, -76.36039639407782431 ) ) ;
#64191 = VECTOR ( 'NONE', #67662, 1000.000000000000000 ) ;
#64192 = EDGE_LOOP ( 'NONE', ( #66964, #47922 ) ) ;
#64193 = CARTESIAN_POINT ( 'NONE',  ( -102.2801239173131194, -170.0000000000000000, -61.85912785543958847 ) ) ;
#64194 = CONTEXT_DEPENDENT_SHAPE_REPRESENTATION ( #63320, #61977 ) ;
#64195 = COLOUR_RGB ( '',0.7921568627450980005, 0.8196078431372548767, 0.9333333333333333481 ) ;
#64196 = CARTESIAN_POINT ( 'NONE',  ( 173.6718135456486607, 71.42581476597409562, 37.98988606938989676 ) ) ;
#64197 = FACE_OUTER_BOUND ( 'NONE', #26729, .T. ) ;
#64198 = CARTESIAN_POINT ( 'NONE',  ( -109.3585523124447434, 37.67345343047318096, -39.98222387189748162 ) ) ;
#64199 = CARTESIAN_POINT ( 'NONE',  ( 62.53356220515465935, 13.59349015304565000, -77.56524142263343435 ) ) ;
#64200 = ORIENTED_EDGE ( 'NONE', *, *, #59924, .T. ) ;
#64201 = VERTEX_POINT ( 'NONE', #18577 ) ;
#64202 = CARTESIAN_POINT ( 'NONE',  ( -23.95096213915837069, 8.481591526885939203, -15.48390114642075588 ) ) ;
#64203 = CARTESIAN_POINT ( 'NONE',  ( 197.2199163281727863, 98.22431253015351160, 9.199768454146621366 ) ) ;
#64204 = VERTEX_POINT ( 'NONE', #65735 ) ;
#64205 = EDGE_LOOP ( 'NONE', ( #59220, #62228, #46078, #25563 ) ) ;
#64206 = LINE ( 'NONE', #47330, #66160 ) ;
#64207 = EDGE_LOOP ( 'NONE', ( #47, #53570, #35798, #57512 ) ) ;
#64208 = DIRECTION ( 'NONE',  ( 0.000000000000000000, -1.000000000000000000, 0.000000000000000000 ) ) ;
#64209 = DIRECTION ( 'NONE',  ( -0.000000000000000000, 0.000000000000000000, -1.000000000000000000 ) ) ;
#64210 = B_SPLINE_CURVE_WITH_KNOTS ( 'NONE', 3,
 ( #55223, #38353, #28504, #39064, #34139, #22523, #12324, #49239, #44319, #49587, #1419, #38710, #60154, #22877, #65806, #49947, #1778, #17952, #39404, #60852, #48531, #21819, #46403, #61207, #45019, #18991, #13709, #34835, #57317, #56621, #13035, #8443, #29892, #24628, #3168, #34497, #29200, #35162, #19677, #8086, #39754, #51694, #40440, #55934, #51356, #14056, #61556, #30243 ),
 .UNSPECIFIED., .F., .F.,
 ( 4, 2, 2, 2, 2, 2, 2, 2, 2, 2, 2, 2, 2, 2, 2, 2, 2, 2, 2, 2, 2, 2, 2, 4 ),
 ( 0.02746511744866865501, 0.02914922134997097181, 0.03083332525127328513, 0.03251742915257559846, 0.03335948110322677768, 0.03420153305387795689, 0.03504358500452913611, 0.03588563695518031532, 0.03756974085648259742, 0.03841179280713374194, 0.03925384475778488647, 0.04009589670843603099, 0.04093794865908717551, 0.04262205256038942291, 0.04430615646169167032, 0.04514820841234279403, 0.04599026036299390385, 0.04767436426429618596, 0.04935846816559846806, 0.05020052011624961258, 0.05104257206690077098, 0.05272667596820312941, 0.05356872791885428781, 0.05441077986950545314 ),
 .UNSPECIFIED. ) ;
#64211 = CARTESIAN_POINT ( 'NONE',  ( -173.1211646369891071, 87.12891641440859303, 18.97714401617737678 ) ) ;
#64212 = CARTESIAN_POINT ( 'NONE',  ( -7.825402957745081878, 7.899365992529268965, -23.57352014148015584 ) ) ;
#64214 = ADVANCED_FACE ( 'NONE', ( #55156 ), #6980, .T. ) ;
#64213 = CARTESIAN_POINT ( 'NONE',  ( 82.82003103503667774, 18.15602011327363385, -90.53761154839286007 ) ) ;
#64215 = CARTESIAN_POINT ( 'NONE',  ( 87.10668362745099103, 19.58396519288864113, -50.82156419891175858 ) ) ;
#64216 = PLANE ( 'NONE',  #28598 ) ;
#64217 = ADVANCED_FACE ( 'NONE', ( #39002 ), #44255, .T. ) ;
#64218 = ORIENTED_EDGE ( 'NONE', *, *, #17361, .F. ) ;
#64219 = ORIENTED_EDGE ( 'NONE', *, *, #18012, .F. ) ;
#64220 = CARTESIAN_POINT ( 'NONE',  ( -118.6157340058430094, 41.88485941274768010, -13.73874819522372981 ) ) ;
#64221 = EDGE_CURVE ( 'NONE', #1580, #20970, #60562, .T. ) ;
#64222 = FACE_BOUND ( 'NONE', #5264, .T. ) ;
#64223 =( REPRESENTATION_RELATIONSHIP ('NONE','NONE', #40274, #35767 ) REPRESENTATION_RELATIONSHIP_WITH_TRANSFORMATION ( #33336 )SHAPE_REPRESENTATION_RELATIONSHIP( ) );
#64224 = CARTESIAN_POINT ( 'NONE',  ( -179.5178913137217194, 94.54206947403388028, -11.41325856914813208 ) ) ;
#64225 = DIRECTION ( 'NONE',  ( 1.387778780781446169E-16, -1.000000000000000000, -3.469446951953615421E-17 ) ) ;
#64227 = EDGE_LOOP ( 'NONE', ( #1155, #45656 ) ) ;
#64226 = CARTESIAN_POINT ( 'NONE',  ( -142.0902782307735492, 58.13494170556000995, -43.45927447690819179 ) ) ;
#64228 = CARTESIAN_POINT ( 'NONE',  ( 55.57634120535662703, 12.09544293553732608, 11.45258174193541656 ) ) ;
#64229 = EDGE_CURVE ( 'NONE', #35720, #55116, #10902, .T. ) ;
#64230 = VECTOR ( 'NONE', #47240, 1000.000000000000000 ) ;
#64231 = EDGE_LOOP ( 'NONE', ( #67264, #21859, #35810 ) ) ;
#64232 = AXIS2_PLACEMENT_3D ( 'NONE', #30591, #15102, #64316 ) ;
#64233 = CARTESIAN_POINT ( 'NONE',  ( 440.2662102946433151, 395.0000000000066507, -139.3786363301462927 ) ) ;
#64234 = CARTESIAN_POINT ( 'NONE',  ( 15.78827728214693416, -170.0000000000000000, 64.35925826316893961 ) ) ;
#64235 = VECTOR ( 'NONE', #51379, 1000.000000000000227 ) ;
#64236 = VECTOR ( 'NONE', #54839, 1000.000000000000000 ) ;
#64237 = CARTESIAN_POINT ( 'NONE',  ( 83.60262962804351616, 18.41036205028015615, -23.34340396361722725 ) ) ;
#64238 = DIRECTION ( 'NONE',  ( -0.3090169943749447312, -0.9510565162951544194, 7.147453794906795954E-17 ) ) ;
#64239 = CARTESIAN_POINT ( 'NONE',  ( 63.01563776193091826, -170.0000000000000000, -35.72069083216973695 ) ) ;
#64240 = CARTESIAN_POINT ( 'NONE',  ( -94.88380767928866533, 29.17964217339915933, 12.44389626902909640 ) ) ;
#64241 = CARTESIAN_POINT ( 'NONE',  ( -95.61819996182568104, 29.52346081122274768, -65.90474338168506563 ) ) ;
#64242 = EDGE_LOOP ( 'NONE', ( #62055, #67284, #63798, #26043 ) ) ;
#64243 = EDGE_CURVE ( 'NONE', #4465, #6992, #37634, .T. ) ;
#64244 = ORIENTED_EDGE ( 'NONE', *, *, #30518, .F. ) ;
#64245 = CIRCLE ( 'NONE', #27026, 2.999999999999999112 ) ;
#64246 = CARTESIAN_POINT ( 'NONE',  ( 181.9295719569813912, 79.46350097013163349, -78.03405158388139284 ) ) ;
#64247 = CLOSED_SHELL ( 'NONE', ( #16018, #34904, #7311, #67619, #12082, #33439, #62516, #55257, #34559, #33853, #20557, #32270, #1249, #33205, #41718, #12883, #41225, #10303, #52800, #59039, #29955, #22942, #59239, #53685, #2865, #28693, #10394, #25324, #31074, #3093, #60657, #1759, #29687, #52435, #30645, #20447, #32797, #22202, #25983, #66553, #57975, #10624, #68972, #3747, #37414, #19294, #8344, #31289, #48042, #556, #7401, #64713, #10544, #46392, #50422, #39632, #36561, #69387, #21268, #63845, #2540, #32409, #41414, #39243, #57562, #38415, #28730, #60678, #62602, #66958, #13282, #62274, #22786, #66645, #61466, #12019, #54963, #51908, #7079, #2860, #63532, #27171, #30881, #59623, #18569, #16735, #64023, #8218, #17478, #20875, #47599, #27571, #30136, #20756, #19148, #34644, #49034, #40027, #6520, #62661, #32523, #39452, #40964, #8987, #10708, #9863, #57520, #49313, #21076, #20629, #62768, #18248, #69444, #4279, #17472, #45898, #18025, #20630, #3178, #58502, #58995, #20025, #322, #36214, #22451, #26744, #51178, #25118, #55442, #47646, #55249, #28037, #19532, #16420, #44880, #23822, #33691, #52243, #57891, #34863, #58994, #14117, #11900, #16680, #5547, #58343, #23138, #59689, #20578, #44305, #23824, #40815, #8213, #28166, #35700, #48971, #6676, #38158 ) ) ;
#64248 = FACE_OUTER_BOUND ( 'NONE', #39808, .T. ) ;
#64249 = CARTESIAN_POINT ( 'NONE',  ( -168.7150276173047700, 82.35404041280327192, -36.12430427854839365 ) ) ;
#64250 = FACE_OUTER_BOUND ( 'NONE', #40060, .T. ) ;
#64251 = CARTESIAN_POINT ( 'NONE',  ( 106.0228389049370463, 28.07756796303167945, -76.47167350182498069 ) ) ;
#64252 = CARTESIAN_POINT ( 'NONE',  ( -76.79042791651913547, 22.68960395613480685, 45.18370245349827741 ) ) ;
#64253 = CARTESIAN_POINT ( 'NONE',  ( 82.95057496836383848, 18.19812356106674400, 43.76578103429130806 ) ) ;
#64254 = CARTESIAN_POINT ( 'NONE',  ( 64.94098077424388293, 14.16208887966256924, -50.48552314904699756 ) ) ;
#64255 = CARTESIAN_POINT ( 'NONE',  ( 40.38132770291767315, 9.553709436640060559, -35.66812004169860018 ) ) ;
#64256 = CARTESIAN_POINT ( 'NONE',  ( 212.0180052085437694, 116.9552462415715439, 65.21599223484632546 ) ) ;
#64257 = ORIENTED_EDGE ( 'NONE', *, *, #24805, .T. ) ;
#64258 = DIRECTION ( 'NONE',  ( 0.000000000000000000, 0.000000000000000000, -1.000000000000000000 ) ) ;
#64259 = ORIENTED_EDGE ( 'NONE', *, *, #46703, .T. ) ;
#64260 = CARTESIAN_POINT ( 'NONE',  ( -13.47230132170245653, 7.324574289401434513, -37.95804552296768719 ) ) ;
#64261 = CARTESIAN_POINT ( 'NONE',  ( -85.14310402784583687, 24.89513709528457142, 87.81192798829980006 ) ) ;
#64262 = CARTESIAN_POINT ( 'NONE',  ( 88.52077179907880122, 21.14145351760140912, 71.31817190172689891 ) ) ;
#64263 = CARTESIAN_POINT ( 'NONE',  ( 150.0973882686025149, 52.13852366454153042, -15.37827118707424567 ) ) ;
#64264 = CARTESIAN_POINT ( 'NONE',  ( 33.44035656425386804, 8.720466003183661385, 15.14638828237973556 ) ) ;
#64265 = CARTESIAN_POINT ( 'NONE',  ( 33.76124497394583557, 7.742545529019360551, -64.99726042931528980 ) ) ;
#64266 = LINE ( 'NONE', #69532, #27762 ) ;
#64267 = DIRECTION ( 'NONE',  ( 0.000000000000000000, 1.000000000000000000, -0.000000000000000000 ) ) ;
#64268 = ORIENTED_EDGE ( 'NONE', *, *, #44740, .F. ) ;
#64269 = CARTESIAN_POINT ( 'NONE',  ( 211.1750821748527187, 115.6700317698878564, 86.59810276603568013 ) ) ;
#64270 = LINE ( 'NONE', #16079, #46560 ) ;
#64271 = VERTEX_POINT ( 'NONE', #33066 ) ;
#64272 = DIRECTION ( 'NONE',  ( -0.000000000000000000, -0.000000000000000000, -1.000000000000000000 ) ) ;
#64273 = CARTESIAN_POINT ( 'NONE',  ( 9.280894575734579988, 7.385644305345137717, -73.62443454551277000 ) ) ;
#64274 = CARTESIAN_POINT ( 'NONE',  ( 2.905661822261151883E-14, 15.55634918610403084, 2.000000000000001776 ) ) ;
#64275 = ADVANCED_BREP_SHAPE_REPRESENTATION ( '', ( #40140, #64062, #16744, #16860, #40361, #41747, #40938, #16524, #40015, #64175, #17808, #63846, #66832 ), #12890 ) ;
#64276 = FACE_OUTER_BOUND ( 'NONE', #16674, .T. ) ;
#64277 = CARTESIAN_POINT ( 'NONE',  ( -3.252497086158843143, 6.636017118948017490, 31.65047178693046348 ) ) ;
#64278 = CARTESIAN_POINT ( 'NONE',  ( -94.84390436305044148, 29.16104988397310649, -14.65970089395015208 ) ) ;
#64279 = CARTESIAN_POINT ( 'NONE',  ( 79.68347087906724369, 18.21983559625775939, 93.81314209895157319 ) ) ;
#64280 = B_SPLINE_CURVE_WITH_KNOTS ( 'NONE', 3,
 ( #834, #10676, #32150, #38462 ),
 .UNSPECIFIED., .F., .F.,
 ( 4, 4 ),
 ( 0.1259919275528360028, 0.1829744153748751878 ),
 .UNSPECIFIED. ) ;
#64281 = VERTEX_POINT ( 'NONE', #26405 ) ;
#64282 = AXIS2_PLACEMENT_3D ( 'NONE', #39737, #1404, #22858 ) ;
#64283 = DIRECTION ( 'NONE',  ( 0.000000000000000000, -1.000000000000000000, 0.000000000000000000 ) ) ;
#64284 = CARTESIAN_POINT ( 'NONE',  ( -155.1359377029286293, 70.46175948311802983, 70.04776735375013175 ) ) ;
#64285 = CARTESIAN_POINT ( 'NONE',  ( -132.6161619568759704, 51.08240647571221160, 7.939436356385802362 ) ) ;
#64286 = CARTESIAN_POINT ( 'NONE',  ( -109.3585523124447860, 37.67345343047320227, 67.39597848995725826 ) ) ;
#64287 = CARTESIAN_POINT ( 'NONE',  ( -180.4445711980297915, 95.66806589453305776, 93.66785953383893570 ) ) ;
#64288 = ORIENTED_EDGE ( 'NONE', *, *, #30579, .F. ) ;
#64289 = LINE ( 'NONE', #11164, #52466 ) ;
#64290 = CIRCLE ( 'NONE', #33971, 8.000000000000000000 ) ;
#64291 = EDGE_CURVE ( 'NONE', #33219, #69014, #64031, .T. ) ;
#64292 = CARTESIAN_POINT ( 'NONE',  ( 93.92280655489126673, 22.03989931749464404, 62.29064022871924777 ) ) ;
#64293 = CARTESIAN_POINT ( 'NONE',  ( 197.5344630110112689, 98.61758706718745771, -19.22573370218078281 ) ) ;
#64294 = VECTOR ( 'NONE', #3465, 1000.000000000000000 ) ;
#64295 = CARTESIAN_POINT ( 'NONE',  ( 88.21404966472069020, 19.96646357304423347, -89.63590846026569636 ) ) ;
#64296 = CARTESIAN_POINT ( 'NONE',  ( -29.87147652227456263, 100.0000000000000000, 73.58025477438756923 ) ) ;
#64297 = EDGE_LOOP ( 'NONE', ( #26223, #722 ) ) ;
#64298 = CARTESIAN_POINT ( 'NONE',  ( 0.08224679563971869223, -6.145890662064657839, 5.355005115540905081 ) ) ;
#64299 = CARTESIAN_POINT ( 'NONE',  ( 85.68197636629476222, 20.16141071296263831, 2.912210986997132878 ) ) ;
#64300 = DIRECTION ( 'NONE',  ( 0.000000000000000000, 1.000000000000000000, -0.000000000000000000 ) ) ;
#64301 = MANIFOLD_SOLID_BREP ( 'Extrude-Thin1', #11411 ) ;
#64302 = LINE ( 'NONE', #4528, #45371 ) ;
#64303 = AXIS2_PLACEMENT_3D ( 'NONE', #39157, #12418, #40709 ) ;
#64304 = ORIENTED_EDGE ( 'NONE', *, *, #8248, .T. ) ;
#64305 = CARTESIAN_POINT ( 'NONE',  ( 180.2565361171340612, 79.19912802278402353, 56.18695598174853956 ) ) ;
#64306 = EDGE_CURVE ( 'NONE', #37055, #38069, #1053, .T. ) ;
#64307 = EDGE_LOOP ( 'NONE', ( #30592, #31874, #4110, #41269 ) ) ;
#64308 = CARTESIAN_POINT ( 'NONE',  ( -76.10397364431024414, 21.36211154336728768, -22.82360444498405272 ) ) ;
#64309 = LINE ( 'NONE', #42166, #43235 ) ;
#64310 = DIRECTION ( 'NONE',  ( 1.000000000000000000, 0.000000000000000000, 0.000000000000000000 ) ) ;
#64312 = EDGE_LOOP ( 'NONE', ( #19839, #61962, #10262, #33782 ) ) ;
#64311 = CARTESIAN_POINT ( 'NONE',  ( 152.2924710224604894, 54.98503313872888754, 15.49619585574763647 ) ) ;
#64313 = CARTESIAN_POINT ( 'NONE',  ( -173.9548930713591233, 88.06040582145364226, 30.85644618464981903 ) ) ;
#64314 = EDGE_CURVE ( 'NONE', #40256, #34571, #43942, .T. ) ;
#64315 = FACE_OUTER_BOUND ( 'NONE', #60153, .T. ) ;
#64316 = DIRECTION ( 'NONE',  ( -1.000000000000000000, 0.000000000000000000, 0.000000000000000000 ) ) ;
#64317 = ORIENTED_EDGE ( 'NONE', *, *, #67684, .F. ) ;
#64318 = PLANE ( 'NONE',  #27721 ) ;
#64319 = CARTESIAN_POINT ( 'NONE',  ( 70.65683382808231272, -25.18281821780013274, 170.0000000000000000 ) ) ;
#64320 = CARTESIAN_POINT ( 'NONE',  ( -167.1534554062404254, 80.72263015867909530, 42.87160806905835386 ) ) ;
#64321 = CARTESIAN_POINT ( 'NONE',  ( 126.3580464630938707, 38.22944795020838171, 63.55427522717772604 ) ) ;
#64322 = ADVANCED_FACE ( 'NONE', ( #5287 ), #59772, .T. ) ;
#64323 = VERTEX_POINT ( 'NONE', #26745 ) ;
#64324 = ORIENTED_EDGE ( 'NONE', *, *, #21899, .F. ) ;
#64325 = ORIENTED_EDGE ( 'NONE', *, *, #29262, .T. ) ;
#64326 = AXIS2_PLACEMENT_3D ( 'NONE', #69484, #64209, #15685 ) ;
#64327 = CARTESIAN_POINT ( 'NONE',  ( -47.56977615209015653, 12.80198389319791019, 90.90604448902824686 ) ) ;
#64328 = DIRECTION ( 'NONE',  ( -0.000000000000000000, -0.000000000000000000, -1.000000000000000000 ) ) ;
#64329 = CIRCLE ( 'NONE', #20542, 65.36598343705435354 ) ;
#64330 = PLANE ( 'NONE',  #14222 ) ;
#64331 = CARTESIAN_POINT ( 'NONE',  ( 68.80232419139076683, 14.08965771880099993, 86.21917338003288478 ) ) ;
#64332 = DIRECTION ( 'NONE',  ( -0.5407162030609373726, -0.6444004775717707689, 0.5407162030609373726 ) ) ;
#64333 = CARTESIAN_POINT ( 'NONE',  ( -132.8123438040340147, 51.22132183644642112, 67.87186335099937651 ) ) ;
#64334 = CARTESIAN_POINT ( 'NONE',  ( -11.76013725602017779, 57.14197687341855669, 27.58472315868181113 ) ) ;
#64335 = ORIENTED_EDGE ( 'NONE', *, *, #56885, .T. ) ;
#64336 = CARTESIAN_POINT ( 'NONE',  ( -96.46212652430689616, 31.03670207994726837, -91.46549339891737418 ) ) ;
#64337 = ORIENTED_EDGE ( 'NONE', *, *, #65380, .T. ) ;
#64338 = CARTESIAN_POINT ( 'NONE',  ( -71.42007367207963853, 20.75704712149298103, 62.76318509112267918 ) ) ;
#64339 = CARTESIAN_POINT ( 'NONE',  ( 188.4904153916303642, 86.42965364612514634, 35.58917660675626848 ) ) ;
#64340 = CARTESIAN_POINT ( 'NONE',  ( 55.51597771111714508, 11.05737652677076355, -69.56553093680295774 ) ) ;
#64341 = CARTESIAN_POINT ( 'NONE',  ( -35.82706824995756278, 10.35287135866583164, -90.42014361026066638 ) ) ;
#64342 = FACE_OUTER_BOUND ( 'NONE', #33621, .T. ) ;
#64343 = AXIS2_PLACEMENT_3D ( 'NONE', #32500, #36401, #58873 ) ;
#64344 = CARTESIAN_POINT ( 'NONE',  ( 197.9740529046198390, 97.55632647424226889, 93.72595611219642819 ) ) ;
#64345 = LINE ( 'NONE', #10529, #34444 ) ;
#64346 = VERTEX_POINT ( 'NONE', #54140 ) ;
#64347 = CARTESIAN_POINT ( 'NONE',  ( -14.86595946518020739, 20.25193917588078563, 3.061616997868437868E-16 ) ) ;
#64348 = CARTESIAN_POINT ( 'NONE',  ( -74.52723870109949189, 7.962625360374199879, 41.38025477438755928 ) ) ;
#64349 = ORIENTED_EDGE ( 'NONE', *, *, #66343, .T. ) ;
#64350 = VERTEX_POINT ( 'NONE', #64364 ) ;
#64351 = CARTESIAN_POINT ( 'NONE',  ( -23.99957301099517437, 9.503061049698468210, -70.64423604567282666 ) ) ;
#64352 = PLANE ( 'NONE',  #60260 ) ;
#64353 = CARTESIAN_POINT ( 'NONE',  ( -24.70911172866235006, 8.583078995053028848, 61.21438271965689637 ) ) ;
#64354 = CARTESIAN_POINT ( 'NONE',  ( -144.9439644317224349, 60.40328483334189968, 5.419750871863752373 ) ) ;
#64355 = VERTEX_POINT ( 'NONE', #53797 ) ;
#64356 = ORIENTED_EDGE ( 'NONE', *, *, #38290, .F. ) ;
#64357 = CARTESIAN_POINT ( 'NONE',  ( -61.29635759142585982, -21.66977272663579868, 3.061616997868437868E-16 ) ) ;
#64358 = ORIENTED_EDGE ( 'NONE', *, *, #40738, .F. ) ;
#64359 = DIRECTION ( 'NONE',  ( 1.000000000000000000, 0.000000000000000000, 0.000000000000000000 ) ) ;
#64360 = DIRECTION ( 'NONE',  ( -1.000000000000000000, 0.000000000000000000, 0.000000000000000000 ) ) ;
#64361 = CARTESIAN_POINT ( 'NONE',  ( 56.53776994993149430, 11.26292242501182628, 67.94548126311852343 ) ) ;
#64362 = EDGE_CURVE ( 'NONE', #36151, #43433, #42051, .T. ) ;
#64363 = CARTESIAN_POINT ( 'NONE',  ( 29.99999999999999645, -30.00000000000000355, 0.000000000000000000 ) ) ;
#64364 = CARTESIAN_POINT ( 'NONE',  ( -858.3301948030079984, -622.0000000000060254, 0.000000000000000000 ) ) ;
#64365 = ADVANCED_FACE ( 'NONE', ( #66141 ), #60134, .T. ) ;
#64366 = COLOUR_RGB ( '',0.7921568627450980005, 0.8196078431372548767, 0.9333333333333333481 ) ;
#64367 = CARTESIAN_POINT ( 'NONE',  ( -29.68020330876228385, 70.00000000000000000, 4.368699068434031219 ) ) ;
#64368 = ORIENTED_EDGE ( 'NONE', *, *, #1192, .F. ) ;
#64369 = ORIENTED_EDGE ( 'NONE', *, *, #24546, .T. ) ;
#64370 = LINE ( 'NONE', #16187, #45747 ) ;
#64371 = LINE ( 'NONE', #32031, #68697 ) ;
#64372 = AXIS2_PLACEMENT_3D ( 'NONE', #36321, #53852, #42624 ) ;
#64373 = FACE_OUTER_BOUND ( 'NONE', #20296, .T. ) ;
#64374 = PLANE ( 'NONE',  #49964 ) ;
#64375 = DIRECTION ( 'NONE',  ( 1.000000000000000000, 0.000000000000000000, -0.000000000000000000 ) ) ;
#64376 = CARTESIAN_POINT ( 'NONE',  ( 18.05623392574862862, 7.590818816530167545, 84.04748085494549059 ) ) ;
#64377 = AXIS2_PLACEMENT_3D ( 'NONE', #40377, #62533, #29824 ) ;
#64378 = ORIENTED_EDGE ( 'NONE', *, *, #67508, .T. ) ;
#64380 = EDGE_CURVE ( 'NONE', #65498, #36599, #7383, .T. ) ;
#64379 = AXIS2_PLACEMENT_3D ( 'NONE', #23851, #45289, #57838 ) ;
#64381 = CARTESIAN_POINT ( 'NONE',  ( 84.74140601443110654, 18.78541996275572146, 17.63000419208631087 ) ) ;
#64382 = VERTEX_POINT ( 'NONE', #50291 ) ;
#64383 = AXIS2_PLACEMENT_3D ( 'NONE', #43328, #16605, #56591 ) ;
#64384 = EDGE_CURVE ( 'NONE', #61651, #14003, #49567, .T. ) ;
#64385 = DIRECTION ( 'NONE',  ( 0.000000000000000000, -1.000000000000000000, 0.000000000000000000 ) ) ;
#64386 = ORIENTED_EDGE ( 'NONE', *, *, #38935, .F. ) ;
#64387 = CONICAL_SURFACE ( 'NONE', #3745, 4.999999999999997335, 0.7853981633974482790 ) ;
#64388 = AXIS2_PLACEMENT_3D ( 'NONE', #12892, #17817, #39273 ) ;
#64389 = EDGE_LOOP ( 'NONE', ( #66128, #18411, #11590, #51129 ) ) ;
#64390 = CARTESIAN_POINT ( 'NONE',  ( -120.6420427933462065, 44.31795133507804252, 5.915438131401089095 ) ) ;
#64391 = EDGE_CURVE ( 'NONE', #68664, #45870, #2795, .T. ) ;
#64392 = DIRECTION ( 'NONE',  ( -0.000000000000000000, 1.000000000000000000, -0.000000000000000000 ) ) ;
#64393 = CARTESIAN_POINT ( 'NONE',  ( 126.5880720616305837, 37.20544379858412043, 65.72198726327758322 ) ) ;
#64394 = ORIENTED_EDGE ( 'NONE', *, *, #10636, .T. ) ;
#64395 = B_SPLINE_CURVE_WITH_KNOTS ( 'NONE', 3,
 ( #50352, #23624, #45060, #61252, #13072, #57358, #21111, #15485, #15821, #47135, #52075, #67924, #25363, #26385, #31653, #25705, #68597, #3539, #36939, #35905, #4918, #58043, #30285, #36247, #68267, #47822, #69283, #46443, #42552, #19723, #10188, #41181, #8835, #14450, #20072, #53089, #37263, #15136, #30629, #51733, #57704, #9515, #46798, #20403 ),
 .UNSPECIFIED., .F., .F.,
 ( 4, 2, 2, 2, 2, 2, 2, 2, 2, 2, 2, 2, 2, 2, 2, 2, 2, 2, 2, 2, 2, 4 ),
 ( 0.02432640572110344665, 0.02583721026359363238, 0.02659261253483874432, 0.02734801480608385627, 0.02885881934857403852, 0.02961422161981911577, 0.03036962389106419302, 0.03188042843355437528, 0.03339123297604455753, 0.03414663524728962785, 0.03490203751853469816, 0.03641284206102485266, 0.03716824433226995766, 0.03792364660351505573, 0.03943445114600528656, 0.04094525568849551045, 0.04245606023098574822, 0.04396686477347597211, 0.04472226704472107711, 0.04547766931596618212, 0.04698847385845637825, 0.04849927840094656745 ),
 .UNSPECIFIED. ) ;
#64396 = LINE ( 'NONE', #1079, #66016 ) ;
#64397 = CARTESIAN_POINT ( 'NONE',  ( 150.2794558856211040, 52.26944788078747450, 39.10923047536901720 ) ) ;
#64398 = FACE_OUTER_BOUND ( 'NONE', #3678, .T. ) ;
#64399 = LINE ( 'NONE', #43628, #12325 ) ;
#64400 = DIRECTION ( 'NONE',  ( 0.000000000000000000, 1.000000000000000000, 0.000000000000000000 ) ) ;
#64401 = PLANE ( 'NONE',  #12536 ) ;
#64402 = ADVANCED_FACE ( 'NONE', ( #23903 ), #52671, .T. ) ;
#64403 = CARTESIAN_POINT ( 'NONE',  ( -24.32937228292060539, 8.531905774118435204, 35.27833887421346759 ) ) ;
#64404 = CARTESIAN_POINT ( 'NONE',  ( -142.0227972901369071, 59.36121938936274489, -69.71386678037109164 ) ) ;
#64405 = VERTEX_POINT ( 'NONE', #13014 ) ;
#64406 = EDGE_CURVE ( 'NONE', #11248, #12451, #14523, .T. ) ;
#64407 = EDGE_CURVE ( 'NONE', #57934, #8504, #49924, .T. ) ;
#64408 = CARTESIAN_POINT ( 'NONE',  ( -36.11269837220809364, -15.55634918610397754, 0.000000000000000000 ) ) ;
#64409 = ADVANCED_FACE ( 'NONE', ( #23216 ), #50625, .F. ) ;
#64410 = DIRECTION ( 'NONE',  ( 0.000000000000000000, 0.000000000000000000, 1.000000000000000000 ) ) ;
#64411 = CARTESIAN_POINT ( 'NONE',  ( -174.7817412490652487, 90.52199442492059234, 57.84031650591408180 ) ) ;
#64412 = LINE ( 'NONE', #32414, #63006 ) ;
#64413 = CARTESIAN_POINT ( 'NONE',  ( -44.26023579658939866, 48.10138582123772721, 6.377659838150142091E-18 ) ) ;
#64414 = CARTESIAN_POINT ( 'NONE',  ( -85.64924756730680144, 26.19583280090850153, 8.325405162945308746 ) ) ;
#64415 = DIRECTION ( 'NONE',  ( -0.000000000000000000, -0.000000000000000000, -1.000000000000000000 ) ) ;
#64416 = DIRECTION ( 'NONE',  ( 0.000000000000000000, 1.000000000000000000, 0.000000000000000000 ) ) ;
#64417 = CARTESIAN_POINT ( 'NONE',  ( -125.4463376280758951, 47.40387005565909817, -76.74829057748890193 ) ) ;
#64418 = CARTESIAN_POINT ( 'NONE',  ( 70.51601918574516503, 14.53832276813546542, 10.70683331067295008 ) ) ;
#64419 = CARTESIAN_POINT ( 'NONE',  ( 163.1265310614426767, 62.18610413911356005, 5.133598315962148106 ) ) ;
#64420 = CARTESIAN_POINT ( 'NONE',  ( 92.20490818459946070, 22.47175429302964034, -11.43690497573547660 ) ) ;
#64421 = ORIENTED_EDGE ( 'NONE', *, *, #13379, .T. ) ;
#64422 = VECTOR ( 'NONE', #44906, 1000.000000000000000 ) ;
#64423 = CARTESIAN_POINT ( 'NONE',  ( -31.92572261726341054, 10.69135962481464119, 3.371903815725487252 ) ) ;
#64424 = ORIENTED_EDGE ( 'NONE', *, *, #25831, .T. ) ;
#64425 = CARTESIAN_POINT ( 'NONE',  ( 0.000000000000000000, 0.000000000000000000, 41.38025477438755928 ) ) ;
#64426 = VERTEX_POINT ( 'NONE', #29516 ) ;
#64427 = CARTESIAN_POINT ( 'NONE',  ( 23.04797191264876233, 7.849755664016355716, -71.80966863344457352 ) ) ;
#64428 = CARTESIAN_POINT ( 'NONE',  ( 102.8221746832285675, 26.69056128693217289, 89.65735780395625909 ) ) ;
#64429 = CARTESIAN_POINT ( 'NONE',  ( -147.1538409485623049, 63.51600817366542628, 57.94073712792580011 ) ) ;
#64430 = CARTESIAN_POINT ( 'NONE',  ( 63.50528314073025626, 12.78634332146812547, -8.876140241706053757 ) ) ;
#64431 = CARTESIAN_POINT ( 'NONE',  ( -23.98747857548121942, 9.501432345103355104, -41.83194910379017273 ) ) ;
#64432 = CARTESIAN_POINT ( 'NONE',  ( -52.45048892661850459, 15.03803514841137812, -62.52259457201746073 ) ) ;
#64433 = AXIS2_PLACEMENT_3D ( 'NONE', #40049, #66108, #13658 ) ;
#64434 = CARTESIAN_POINT ( 'NONE',  ( -21.03405120204953960, -13.73704776265678440, 0.000000000000000000 ) ) ;
#64435 = CARTESIAN_POINT ( 'NONE',  ( 444.9999999999999432, 225.0000000000000000, 380.0000000000000000 ) ) ;
#64436 = ORIENTED_EDGE ( 'NONE', *, *, #11600, .T. ) ;
#64437 = VECTOR ( 'NONE', #43211, 1000.000000000000000 ) ;
#64438 = EDGE_LOOP ( 'NONE', ( #43113, #19404, #69508, #21148 ) ) ;
#64439 = VECTOR ( 'NONE', #44754, 1000.000000000000000 ) ;
#64440 = CARTESIAN_POINT ( 'NONE',  ( 38.42095780754793566, 9.297684251045556181, 71.71026093375481025 ) ) ;
#64441 = CARTESIAN_POINT ( 'NONE',  ( 173.7124655175693988, 72.83929305610512017, 89.05859609801423460 ) ) ;
#64442 = AXIS2_PLACEMENT_3D ( 'NONE', #2119, #49579, #13022 ) ;
#64443 = LINE ( 'NONE', #16252, #26278 ) ;
#64444 = CARTESIAN_POINT ( 'NONE',  ( 230.9999999999999432, -57.00000000000007816, 72.99999999999998579 ) ) ;
#64445 = ORIENTED_EDGE ( 'NONE', *, *, #14230, .F. ) ;
#64446 = CARTESIAN_POINT ( 'NONE',  ( 93.32756701508621688, 22.89083686918419502, 13.77822573322123212 ) ) ;
#64447 = B_SPLINE_CURVE_WITH_KNOTS ( 'NONE', 3,
 ( #16602, #5697, #6042, #53184, #5013, #26821, #21531, #27855, #54580, #27501, #10628, #782, #38407, #22234, #33144, #43674, #32100, #65150, #59851, #6405, #49298, #38771, #53536, #26479, #47915, #37358, #21201, #7806, #34197, #2523, #7464, #23297, #17661, #18008, #2869, #6750, #65866, #44377, #66908, #29589, #66221, #8145, #39458, #2185, #34551 ),
 .UNSPECIFIED., .F., .F.,
 ( 4, 2, 2, 2, 2, 2, 2, 2, 1, 2, 2, 2, 2, 2, 2, 2, 2, 2, 2, 2, 2, 2, 4 ),
 ( 1.734723475976807094E-18, 0.001467747071934203101, 0.002201620607901302266, 0.002935494143868401865, 0.004403241215802589786, 0.005870988287736776841, 0.007338735359670963895, 0.008072608895638043111, 0.008806482431605120592, 0.009540355967572199808, 0.01027422950353927902, 0.01174197657547347388, 0.01247585011144059300, 0.01320972364740771211, 0.01467747071934199198, 0.01541134425530912150, 0.01614521779127624929, 0.01761296486321049098, 0.01908071193514473962, 0.01981458547111185353, 0.02054845900707896050, 0.02201620607901318138, 0.02348395315094738839 ),
 .UNSPECIFIED. ) ;
#64448 = CARTESIAN_POINT ( 'NONE',  ( 188.2962140587030149, 87.71627202537837320, -18.95942837431084627 ) ) ;
#64449 = CARTESIAN_POINT ( 'NONE',  ( -65.36598343705435354, 0.000000000000000000, 41.38025477438755928 ) ) ;
#64450 =( NAMED_UNIT ( * ) SI_UNIT ( $, .STERADIAN. ) SOLID_ANGLE_UNIT ( ) );
#64451 = CARTESIAN_POINT ( 'NONE',  ( 86.62931800182293784, -170.0000000000000000, 17.86753698201564688 ) ) ;
#64452 = CARTESIAN_POINT ( 'NONE',  ( 46.13856685535756696, 9.381502944822520007, -12.94178744436969275 ) ) ;
#64454 = DIRECTION ( 'NONE',  ( 1.000000000000000000, 0.000000000000000000, 0.000000000000000000 ) ) ;
#64453 = B_SPLINE_CURVE_WITH_KNOTS ( 'NONE', 3,
 ( #56677, #20082, #14462, #35221 ),
 .UNSPECIFIED., .F., .F.,
 ( 4, 4 ),
 ( 0.1259919275528356697, 0.1829744153748742441 ),
 .UNSPECIFIED. ) ;
#64455 = CARTESIAN_POINT ( 'NONE',  ( 104.9998698049113273, 22.00002958979063550, -0.3253397936368049304 ) ) ;
#64456 = CARTESIAN_POINT ( 'NONE',  ( 164.1352994389932007, 64.33767534192695337, 60.30451892934298286 ) ) ;
#64457 = ADVANCED_FACE ( 'NONE', ( #33765 ), #2447, .T. ) ;
#64458 = ORIENTED_EDGE ( 'NONE', *, *, #43355, .F. ) ;
#64459 = DIRECTION ( 'NONE',  ( 0.000000000000000000, 0.000000000000000000, 1.000000000000000000 ) ) ;
#64460 = CARTESIAN_POINT ( 'NONE',  ( 94.02861641584115659, 23.15570573563315904, -44.57244623153589203 ) ) ;
#64461 = CARTESIAN_POINT ( 'NONE',  ( 55.00000000000000000, 19.13941707223176181, -5.803681084894614095 ) ) ;
#64462 = LINE ( 'NONE', #16273, #48886 ) ;
#64463 = CARTESIAN_POINT ( 'NONE',  ( 155.7262569076171701, 56.30477153194512852, 17.41501643175935143 ) ) ;
#64464 = CARTESIAN_POINT ( 'NONE',  ( -15.22837983954869223, 8.497513067427652445, 92.55061580248207065 ) ) ;
#64465 = ORIENTED_EDGE ( 'NONE', *, *, #38007, .T. ) ;
#64467 = ADVANCED_FACE ( 'NONE', ( #17579 ), #39044, .T. ) ;
#64466 = CARTESIAN_POINT ( 'NONE',  ( -9.929343724188531780E-16, 0.3912769056150340319, 8.000000000000000000 ) ) ;
#64468 = EDGE_CURVE ( 'NONE', #25148, #19844, #44667, .T. ) ;
#64469 = CARTESIAN_POINT ( 'NONE',  ( -56.02027488966933078, 14.94257193099085690, 72.11473951196722965 ) ) ;
#64470 = ORIENTED_EDGE ( 'NONE', *, *, #64616, .T. ) ;
#64471 = EDGE_CURVE ( 'NONE', #57040, #64426, #41319, .T. ) ;
#64472 = EDGE_LOOP ( 'NONE', ( #1601, #42692 ) ) ;
#64473 = DIRECTION ( 'NONE',  ( -0.000000000000000000, 0.000000000000000000, -1.000000000000000000 ) ) ;
#64474 = CARTESIAN_POINT ( 'NONE',  ( -0.4701925472693525565, 38.33111774246623327, 13.32819397642332149 ) ) ;
#64475 = CARTESIAN_POINT ( 'NONE',  ( 107.9301116202191650, 27.82606182274594886, 29.96094684213162651 ) ) ;
#64476 = ORIENTED_EDGE ( 'NONE', *, *, #2955, .F. ) ;
#64477 = EDGE_CURVE ( 'NONE', #7875, #8973, #17885, .T. ) ;
#64478 = CARTESIAN_POINT ( 'NONE',  ( -61.51762070241280611, 16.51067482779404116, -65.75066130139710197 ) ) ;
#64479 = AXIS2_PLACEMENT_3D ( 'NONE', #57531, #42035, #20233 ) ;
#64480 = B_SPLINE_CURVE_WITH_KNOTS ( 'NONE', 3,
 ( #39264, #62361, #62714, #24738, #46874, #56741, #38919, #68338, #12524, #28711, #9243, #14516, #30010, #66013, #19442, #25084, #1985, #55073, #46173, #14175, #23084, #50157, #67312, #45836, #17810, #19098, #8558, #3614, #3967, #35638, #25436, #57089, #8901, #12182, #60366, #30353, #67997, #67646 ),
 .UNSPECIFIED., .F., .F.,
 ( 4, 2, 2, 2, 2, 2, 2, 2, 2, 2, 2, 2, 2, 2, 2, 2, 2, 2, 4 ),
 ( 1.430489624538199204E-17, 0.003908178031105504456, 0.005862267046658207678, 0.007816356062210911768, 0.009770445077763615857, 0.01172453409331631821, 0.01270157860109266158, 0.01367862310886900669, 0.01465566761664534833, 0.01563271212442169170, 0.01660975663219803680, 0.01758680113997438191, 0.01954089015552706865, 0.02051793466330342069, 0.02149497917107977274, 0.02344906818663248030, 0.02540315720218519133, 0.02735724621773790582, 0.03126542424884329319 ),
 .UNSPECIFIED. ) ;
#64481 = CARTESIAN_POINT ( 'NONE',  ( -3.862560291631540021, 7.672660553664875316, 4.398781296712932942 ) ) ;
#64482 = CARTESIAN_POINT ( 'NONE',  ( -417.6627218934913230, 179.4906275429376308, -144.4497041420118819 ) ) ;
#64483 = CARTESIAN_POINT ( 'NONE',  ( 164.7598791907599320, 63.54825436415271867, 92.40245794402351009 ) ) ;
#64484 = AXIS2_PLACEMENT_3D ( 'NONE', #8308, #20571, #35040 ) ;
#64485 = DIRECTION ( 'NONE',  ( 1.000000000000000000, 1.132072239499580971E-16, -1.697513318603925187E-16 ) ) ;
#64486 = VECTOR ( 'NONE', #21187, 1000.000000000000000 ) ;
#64487 = ORIENTED_EDGE ( 'NONE', *, *, #6081, .F. ) ;
#64488 = VECTOR ( 'NONE', #23225, 1000.000000000000000 ) ;
#64489 = CARTESIAN_POINT ( 'NONE',  ( -48.23389383802710739, 13.99288361739331599, -45.84916994387870659 ) ) ;
#64490 = VECTOR ( 'NONE', #20352, 1000.000000000000000 ) ;
#64491 = PLANE ( 'NONE',  #3325 ) ;
#64492 = CARTESIAN_POINT ( 'NONE',  ( 8.763528846667103522, 7.383598436776580343, 40.15354979696406446 ) ) ;
#64493 = CARTESIAN_POINT ( 'NONE',  ( -2.699999999999990408, 0.000000000000000000, -20.30000000000000071 ) ) ;
#64494 = CARTESIAN_POINT ( 'NONE',  ( -82.76871759908607373, 25.01134596399992205, 85.32081939002443960 ) ) ;
#64496 = EDGE_LOOP ( 'NONE', ( #8471, #65141, #66009, #13 ) ) ;
#64495 = FACE_OUTER_BOUND ( 'NONE', #48090, .T. ) ;
#64497 = VERTEX_POINT ( 'NONE', #46041 ) ;
#64498 = EDGE_CURVE ( 'NONE', #29482, #63672, #40418, .T. ) ;
#64499 = EDGE_CURVE ( 'NONE', #30746, #8782, #63115, .T. ) ;
#64500 = ORIENTED_EDGE ( 'NONE', *, *, #31403, .F. ) ;
#64501 = CARTESIAN_POINT ( 'NONE',  ( -5.000000000000073719, -46.66904755831211560, 0.000000000000000000 ) ) ;
#64502 = CARTESIAN_POINT ( 'NONE',  ( -51.77439426130687394, 13.82695438436703306, 44.56726461004345197 ) ) ;
#64503 = FACE_OUTER_BOUND ( 'NONE', #65512, .T. ) ;
#64504 = DIRECTION ( 'NONE',  ( 0.000000000000000000, 0.000000000000000000, 1.000000000000000000 ) ) ;
#64505 = EDGE_CURVE ( 'NONE', #8018, #8573, #34611, .T. ) ;
#64506 = CARTESIAN_POINT ( 'NONE',  ( -60.95805269991215880, 17.39401718769326521, -47.34644918853374662 ) ) ;
#64507 = DIRECTION ( 'NONE',  ( -0.000000000000000000, 1.000000000000000000, -0.000000000000000000 ) ) ;
#64508 = CARTESIAN_POINT ( 'NONE',  ( 151.3309484205705360, 53.03078371058071383, -66.15348108964258245 ) ) ;
#64509 = DIRECTION ( 'NONE',  ( -1.000000000000000000, 0.000000000000000000, 0.000000000000000000 ) ) ;
#64510 = EDGE_LOOP ( 'NONE', ( #31420, #20687, #61677, #44428 ) ) ;
#64511 = CARTESIAN_POINT ( 'NONE',  ( -157.0077369422018023, 70.81157624963286423, -42.59393186173343082 ) ) ;
#64512 = ORIENTED_EDGE ( 'NONE', *, *, #33002, .F. ) ;
#64513 = VERTEX_POINT ( 'NONE', #54410 ) ;
#64514 = CARTESIAN_POINT ( 'NONE',  ( 65.62985354949972816, 14.32996029952553663, -9.342276637876624434 ) ) ;
#64515 = LINE ( 'NONE', #27217, #40607 ) ;
#64516 = CARTESIAN_POINT ( 'NONE',  ( -24.69013852392472685, 9.595969721133672081, 88.11818326750967856 ) ) ;
#64517 = CARTESIAN_POINT ( 'NONE',  ( -149.9471644042847345, 65.87751327280743396, 3.885972380641331547 ) ) ;
#64518 = CARTESIAN_POINT ( 'NONE',  ( 187.9007786055418308, 85.78077355327275200, -40.58561043776339261 ) ) ;
#64519 = CARTESIAN_POINT ( 'NONE',  ( 19.75784582661441391, 6.660183274347810212, 43.88284034533711520 ) ) ;
#64520 = CARTESIAN_POINT ( 'NONE',  ( -149.0793230056187042, 65.13495668545753858, 84.40313663166193692 ) ) ;
#64521 = VERTEX_POINT ( 'NONE', #32293 ) ;
#64522 = VERTEX_POINT ( 'NONE', #63612 ) ;
#64523 = VERTEX_POINT ( 'NONE', #69219 ) ;
#64524 = VECTOR ( 'NONE', #69499, 1000.000000000000000 ) ;
#64525 = CARTESIAN_POINT ( 'NONE',  ( -14.19447842053094000, 7.389800932646227949, 14.73911132003235736 ) ) ;
#64526 = DIRECTION ( 'NONE',  ( -0.000000000000000000, -0.000000000000000000, 1.000000000000000000 ) ) ;
#64527 = MANIFOLD_SOLID_BREP ( 'Cut-Extrude1', #49631 ) ;
#64528 = CARTESIAN_POINT ( 'NONE',  ( -2.645453300864630819E-14, -10.55634918610403439, 2.000000000000001776 ) ) ;
#64529 = CARTESIAN_POINT ( 'NONE',  ( 50.98853755884157124, 395.0000000000065938, -128.9497041420121946 ) ) ;
#64530 = VERTEX_POINT ( 'NONE', #54058 ) ;
#64531 = AXIS2_PLACEMENT_3D ( 'NONE', #29769, #51232, #45248 ) ;
#64532 = CARTESIAN_POINT ( 'NONE',  ( 187.2296622856350723, 86.53808614709454616, 59.34610297735440554 ) ) ;
#64533 = CARTESIAN_POINT ( 'NONE',  ( -154.0718453320784249, 68.14976693162388699, 59.10962140803805198 ) ) ;
#64534 = CARTESIAN_POINT ( 'NONE',  ( 22.15943197741200166, 7.796127622097902332, 6.705548799778502378 ) ) ;
#64535 = CARTESIAN_POINT ( 'NONE',  ( -20.63749999999999929, 0.000000000000000000, 0.000000000000000000 ) ) ;
#64536 = FACE_OUTER_BOUND ( 'NONE', #23611, .T. ) ;
#64537 = CARTESIAN_POINT ( 'NONE',  ( -444.1138056043201914, 394.7873829578389859, -130.7180718971919475 ) ) ;
#64538 = AXIS2_PLACEMENT_3D ( 'NONE', #34366, #44187, #66725 ) ;
#64539 = CARTESIAN_POINT ( 'NONE',  ( 20.36314374176838271, 6.689939636827347158, 58.39567505551136861 ) ) ;
#64540 = DIRECTION ( 'NONE',  ( 1.000000000000000000, 0.000000000000000000, 1.334402673828313339E-16 ) ) ;
#64541 = CARTESIAN_POINT ( 'NONE',  ( 12.69192874957003703, 6.421326776602846564, -76.69892586780029831 ) ) ;
#64542 = VECTOR ( 'NONE', #65053, 1000.000000000000000 ) ;
#64543 = EDGE_CURVE ( 'NONE', #32531, #37758, #7825, .T. ) ;
#64544 = VECTOR ( 'NONE', #20524, 1000.000000000000000 ) ;
#64545 = ORIENTED_EDGE ( 'NONE', *, *, #38093, .F. ) ;
#64546 = LINE ( 'NONE', #32198, #60822 ) ;
#64547 = PRODUCT_CONTEXT ( 'NONE', #43056, 'mechanical' ) ;
#64548 = CARTESIAN_POINT ( 'NONE',  ( 173.5837434292114096, 71.34409607026157119, 36.52054170544656841 ) ) ;
#64549 = CARTESIAN_POINT ( 'NONE',  ( -133.3958821919892728, 51.63629593114585958, -42.92790141718640484 ) ) ;
#64550 = CARTESIAN_POINT ( 'NONE',  ( 46.76970822239468362, 9.482505381172245507, -68.49923864311128341 ) ) ;
#64551 = LINE ( 'NONE', #5797, #23166 ) ;
#64552 = EDGE_LOOP ( 'NONE', ( #38726, #13484, #3090, #447 ) ) ;
#64553 = ORIENTED_EDGE ( 'NONE', *, *, #21405, .T. ) ;
#64555 = EDGE_CURVE ( 'NONE', #19369, #30210, #22769, .T. ) ;
#64554 = DIRECTION ( 'NONE',  ( 0.000000000000000000, 1.000000000000000000, 0.000000000000000000 ) ) ;
#64556 = CARTESIAN_POINT ( 'NONE',  ( 199.9103251464699724, 101.6434290204575746, 15.64108102732007488 ) ) ;
#64557 = ORIENTED_EDGE ( 'NONE', *, *, #18430, .F. ) ;
#64558 = ORIENTED_EDGE ( 'NONE', *, *, #47020, .T. ) ;
#64559 = EDGE_CURVE ( 'NONE', #1423, #40870, #2028, .T. ) ;
#64560 = DIRECTION ( 'NONE',  ( 1.000000000000000000, 0.000000000000000000, 0.000000000000000000 ) ) ;
#64561 = ORIENTED_EDGE ( 'NONE', *, *, #55107, .T. ) ;
#64562 = CARTESIAN_POINT ( 'NONE',  ( 111.1829448509513441, 30.43012797723692486, 71.41128605587280731 ) ) ;
#64563 = CARTESIAN_POINT ( 'NONE',  ( 103.1664446665382826, 26.83710903202776166, -94.59076984783679620 ) ) ;
#64564 = ADVANCED_FACE ( 'NONE', ( #1664 ), #39236, .T. ) ;
#64565 = CARTESIAN_POINT ( 'NONE',  ( -9.964117946889912147, 64.24592483216710548, 43.58025477438756923 ) ) ;
#64566 = CARTESIAN_POINT ( 'NONE',  ( 110.2429982417149574, 29.99119854320845846, -77.76698815611739235 ) ) ;
#64567 = EDGE_CURVE ( 'NONE', #5410, #12998, #45264, .T. ) ;
#64568 = CARTESIAN_POINT ( 'NONE',  ( 85.05122279459726542, 18.88829753553988411, -89.66790706224459484 ) ) ;
#64569 = DIRECTION ( 'NONE',  ( 0.000000000000000000, 0.000000000000000000, 1.000000000000000000 ) ) ;
#64570 = CARTESIAN_POINT ( 'NONE',  ( -55.05276343752908730, 15.72344139423347720, -8.371773407996169425 ) ) ;
#64571 = ORIENTED_EDGE ( 'NONE', *, *, #21371, .F. ) ;
#64572 = EDGE_LOOP ( 'NONE', ( #58670, #53302, #7313, #28113, #55897, #42300, #46967, #45103, #14797 ) ) ;
#64573 = CARTESIAN_POINT ( 'NONE',  ( 8.000000000000000000, -0.7805016046291005649, 1.033380195650246414E-15 ) ) ;
#64574 = AXIS2_PLACEMENT_3D ( 'NONE', #6355, #55946, #24292 ) ;
#64575 = FACE_BOUND ( 'NONE', #30503, .T. ) ;
#64576 = CARTESIAN_POINT ( 'NONE',  ( -142.9756886485677398, 60.11539876121631920, -46.00802361820244357 ) ) ;
#64577 = CARTESIAN_POINT ( 'NONE',  ( -168.1839487819771080, 83.25723186408070831, -63.40587985515518454 ) ) ;
#64578 = AXIS2_PLACEMENT_3D ( 'NONE', #9324, #13909, #55154 ) ;
#64580 = ORIENTED_EDGE ( 'NONE', *, *, #58535, .F. ) ;
#64579 = CARTESIAN_POINT ( 'NONE',  ( -145.9095871962850026, 61.18682730038538864, -35.72809995561637919 ) ) ;
#64581 = PLANE ( 'NONE',  #12879 ) ;
#64582 = CONICAL_SURFACE ( 'NONE', #562, 65.00000000000000000, 0.7853981633974497223 ) ;
#64583 = AXIS2_PLACEMENT_3D ( 'NONE', #21881, #22239, #10632 ) ;
#64584 = ORIENTED_EDGE ( 'NONE', *, *, #20893, .F. ) ;
#64585 = CARTESIAN_POINT ( 'NONE',  ( 56.67004931728209982, 12.31690113431407951, 94.99999999999866418 ) ) ;
#64586 = CARTESIAN_POINT ( 'NONE',  ( -442.6627218934914367, 399.9999999999998863, -136.4497041420118251 ) ) ;
#64587 = ADVANCED_FACE ( 'NONE', ( #23823 ), #58297, .T. ) ;
#64588 = VECTOR ( 'NONE', #67026, 1000.000000000000000 ) ;
#64589 = DIRECTION ( 'NONE',  ( 1.000000000000000000, 0.000000000000000000, 0.000000000000000000 ) ) ;
#64590 = CARTESIAN_POINT ( 'NONE',  ( 92.53566308513175898, 21.52138666710687076, -65.51745770271240588 ) ) ;
#64591 = CARTESIAN_POINT ( 'NONE',  ( -51.33022611924979373, -5.874856440034677441, 26.66469066592268433 ) ) ;
#64592 = AXIS2_PLACEMENT_3D ( 'NONE', #10410, #48037, #43109 ) ;
#64593 = CARTESIAN_POINT ( 'NONE',  ( -99.11448999425215334, 31.20120877265619086, 4.359154089478449734 ) ) ;
#64594 = CARTESIAN_POINT ( 'NONE',  ( -99.97541017369785266, 31.62502926470683917, -62.20652744093037256 ) ) ;
#64595 = EDGE_LOOP ( 'NONE', ( #55720, #29704, #52240, #54436, #8495, #48535, #53435, #60238, #22107 ) ) ;
#64596 = ORIENTED_EDGE ( 'NONE', *, *, #61559, .F. ) ;
#64597 = CARTESIAN_POINT ( 'NONE',  ( -7.329206686002009974E-14, -46.66904755831211560, 85.00100000000000477 ) ) ;
#64598 = CARTESIAN_POINT ( 'NONE',  ( 0.000000000000000000, 50.00000000000000000, 0.000000000000000000 ) ) ;
#64599 = LINE ( 'NONE', #59311, #64942 ) ;
#64600 = DIRECTION ( 'NONE',  ( 1.000000000000000000, 2.220446049250313396E-14, 0.000000000000000000 ) ) ;
#64601 = CARTESIAN_POINT ( 'NONE',  ( 104.7042813665017746, 27.49927371769996753, -65.18629986727883363 ) ) ;
#64602 = CARTESIAN_POINT ( 'NONE',  ( -74.39861643904072253, 21.81123504700007132, -63.28798662571114164 ) ) ;
#64603 = FACE_OUTER_BOUND ( 'NONE', #7723, .T. ) ;
#64604 = CARTESIAN_POINT ( 'NONE',  ( 46.85361596800670725, 10.51535167202354337, -42.13511323660575414 ) ) ;
#64605 = CARTESIAN_POINT ( 'NONE',  ( 412.3372781065085633, 219.4906275429376308, -144.4497041420117682 ) ) ;
#64606 = ORIENTED_EDGE ( 'NONE', *, *, #14912, .F. ) ;
#64607 = CARTESIAN_POINT ( 'NONE',  ( -109.3553681454883844, 36.52260784104392854, -18.21015660155229199 ) ) ;
#64608 = ORIENTED_EDGE ( 'NONE', *, *, #46058, .T. ) ;
#64609 = CARTESIAN_POINT ( 'NONE',  ( -34.74312654625183683, 10.15703162223800327, 4.134442808324870988 ) ) ;
#64610 = CARTESIAN_POINT ( 'NONE',  ( -85.64954339472194533, 25.10532946445850300, 94.41971732200894962 ) ) ;
#64611 = CARTESIAN_POINT ( 'NONE',  ( 90.51709546286271291, 21.85407654229979713, 57.63841953243931471 ) ) ;
#64612 = CARTESIAN_POINT ( 'NONE',  ( 151.7819978880463623, 53.35998893001566046, -21.67396922968716311 ) ) ;
#64613 = DIRECTION ( 'NONE',  ( 0.000000000000000000, 0.000000000000000000, -1.000000000000000000 ) ) ;
#64614 = LINE ( 'NONE', #15736, #51337 ) ;
#64615 = CARTESIAN_POINT ( 'NONE',  ( -9.964117946888929822, -64.24592483216726180, 170.0000000000000000 ) ) ;
#64616 = EDGE_CURVE ( 'NONE', #19565, #23144, #61451, .T. ) ;
#64617 = ORIENTED_EDGE ( 'NONE', *, *, #20976, .T. ) ;
#64618 = DIRECTION ( 'NONE',  ( 1.000000000000000000, 0.000000000000000000, 0.000000000000000000 ) ) ;
#64619 = DIRECTION ( 'NONE',  ( 1.000000000000000000, 0.000000000000000000, 0.000000000000000000 ) ) ;
#64620 = ORIENTED_EDGE ( 'NONE', *, *, #19695, .F. ) ;
#64621 = CARTESIAN_POINT ( 'NONE',  ( 445.3372781065085633, 217.8591479523844612, -111.4497041420119388 ) ) ;
#64622 = CARTESIAN_POINT ( 'NONE',  ( 24.79066879238614263, -3.228426989449305839, 0.000000000000000000 ) ) ;
#64623 = LINE ( 'NONE', #48083, #27462 ) ;
#64624 = EDGE_CURVE ( 'NONE', #56740, #8018, #11865, .T. ) ;
#64625 = CARTESIAN_POINT ( 'NONE',  ( 46.65860211212413589, 10.48377752989033951, -68.00529549296528842 ) ) ;
#64627 = ADVANCED_FACE ( 'NONE', ( #22423 ), #6941, .F. ) ;
#64626 = CARTESIAN_POINT ( 'NONE',  ( -2.355184675731021304, 6.596450510445358795, 32.47880294032771786 ) ) ;
#64628 = LINE ( 'NONE', #17835, #35617 ) ;
#64629 = CARTESIAN_POINT ( 'NONE',  ( 92.18267540243923008, 22.46369443246546638, 85.84941083122645011 ) ) ;
#64630 = VECTOR ( 'NONE', #3442, 1000.000000000000000 ) ;
#64631 = EDGE_CURVE ( 'NONE', #59483, #60423, #12570, .T. ) ;
#64632 = ORIENTED_EDGE ( 'NONE', *, *, #60752, .T. ) ;
#64633 = VECTOR ( 'NONE', #29571, 1000.000000000000000 ) ;
#64634 = CARTESIAN_POINT ( 'NONE',  ( 674.0542565117339109, 995.7769185991946870, 664.1548492967880293 ) ) ;
#64635 = CARTESIAN_POINT ( 'NONE',  ( 8.000000000000003553, -4.618802153517020948, -8.785468820183664818 ) ) ;
#64636 = DIRECTION ( 'NONE',  ( -0.04486483035051863633, 0.9989930665413144784, 0.000000000000000000 ) ) ;
#64637 = CARTESIAN_POINT ( 'NONE',  ( -167.0073208999199323, 82.02183861952782706, -46.56420129388767037 ) ) ;
#64638 = ITEM_DEFINED_TRANSFORMATION ( 'NONE', 'NONE', #66977,  #66832 ) ;
#64639 = CARTESIAN_POINT ( 'NONE',  ( -180.4401457064375904, 95.66269784892554640, 90.33214016306547478 ) ) ;
#64640 = EDGE_LOOP ( 'NONE', ( #43249, #38272 ) ) ;
#64642 = LINE ( 'NONE', #11499, #22132 ) ;
#64641 = VECTOR ( 'NONE', #22572, 1000.000000000000000 ) ;
#64643 = AXIS2_PLACEMENT_3D ( 'NONE', #28660, #44835, #45523 ) ;
#64644 = CARTESIAN_POINT ( 'NONE',  ( 111.9975424824652634, 296.0000000000000000, 420.0000000000000568 ) ) ;
#64645 = CIRCLE ( 'NONE', #45561, 65.36598343705435354 ) ;
#64646 = CARTESIAN_POINT ( 'NONE',  ( -157.0033029063690719, 70.80749022588149444, 92.34162853283143590 ) ) ;
#64647 = AXIS2_PLACEMENT_3D ( 'NONE', #69432, #37417, #54274 ) ;
#64649 = EDGE_CURVE ( 'NONE', #69327, #42318, #14478, .T. ) ;
#64648 = APPLICATION_CONTEXT ( 'automotive_design' ) ;
#64650 = CARTESIAN_POINT ( 'NONE',  ( 136.1081004736419686, 42.80058051492063953, 29.85254608541649191 ) ) ;
#64651 = ORIENTED_EDGE ( 'NONE', *, *, #48317, .T. ) ;
#64652 = LINE ( 'NONE', #54415, #60348 ) ;
#64653 = CARTESIAN_POINT ( 'NONE',  ( -7.825402957745083654, 6.891034867348165172, 56.96013162991089018 ) ) ;
#64654 = EDGE_CURVE ( 'NONE', #49052, #60277, #40438, .T. ) ;
#64655 = CARTESIAN_POINT ( 'NONE',  ( 160.4986104110022893, 61.33701824525266488, 16.93016324216665680 ) ) ;
#64656 = CARTESIAN_POINT ( 'NONE',  ( 23.09119322872580682, 6.844329382916375160, -95.00000000000133582 ) ) ;
#64657 = ORIENTED_EDGE ( 'NONE', *, *, #16765, .T. ) ;
#64658 = DIRECTION ( 'NONE',  ( -0.000000000000000000, -0.000000000000000000, -1.000000000000000000 ) ) ;
#64659 = ORIENTED_EDGE ( 'NONE', *, *, #34581, .T. ) ;
#64660 = CARTESIAN_POINT ( 'NONE',  ( -76.77329340382465261, 21.60914066444071935, -8.497956380613862493 ) ) ;
#64661 = CARTESIAN_POINT ( 'NONE',  ( -59.94781924509481286, 16.04872117907065387, 43.50492361771002692 ) ) ;
#64663 = ORIENTED_EDGE ( 'NONE', *, *, #64995, .F. ) ;
#64662 = CARTESIAN_POINT ( 'NONE',  ( 150.5538013146980347, 53.70974888488126453, 12.97725223995403709 ) ) ;
#64664 = CARTESIAN_POINT ( 'NONE',  ( -173.5394735271662512, 87.59446374803710000, 30.82169460664101734 ) ) ;
#64665 = CARTESIAN_POINT ( 'NONE',  ( 0.000000000000000000, 0.000000000000000000, 17.57656211871651308 ) ) ;
#64666 = DIRECTION ( 'NONE',  ( 0.8805955318567391110, -0.4738686624729965824, 0.000000000000000000 ) ) ;
#64667 = PRODUCT_DEFINITION_SHAPE ( 'NONE', 'NONE',  #69631 ) ;
#64668 = VERTEX_POINT ( 'NONE', #14982 ) ;
#64669 = B_SPLINE_CURVE_WITH_KNOTS ( 'NONE', 3,
 ( #240, #38577, #49109, #1298, #948, #32609 ),
 .UNSPECIFIED., .F., .F.,
 ( 4, 2, 4 ),
 ( 1.095770181108978510E-06, 0.03239442681617710207, 0.06478775786217309818 ),
 .UNSPECIFIED. ) ;
#64670 = CARTESIAN_POINT ( 'NONE',  ( -31.86613092031432259, -10.09122378784736540, 6.893342932236730114 ) ) ;
#64671 = VECTOR ( 'NONE', #42695, 1000.000000000000000 ) ;
#64672 = CARTESIAN_POINT ( 'NONE',  ( 0.000000000000000000, 0.000000000000000000, 41.38025477438755928 ) ) ;
#64673 = CARTESIAN_POINT ( 'NONE',  ( -180.5200658187031593, 97.35517482626555363, 37.05475405369923436 ) ) ;
#64674 = CARTESIAN_POINT ( 'NONE',  ( 130.3281282802763315, 40.49854652972195623, 57.21990522415401159 ) ) ;
#64675 = VERTEX_POINT ( 'NONE', #45620 ) ;
#64676 = EDGE_LOOP ( 'NONE', ( #4094, #32244, #47286, #33865 ) ) ;
#64677 = AXIS2_PLACEMENT_3D ( 'NONE', #33314, #43492, #48403 ) ;
#64678 = ORIENTED_EDGE ( 'NONE', *, *, #30052, .T. ) ;
#64679 = FACE_OUTER_BOUND ( 'NONE', #45820, .T. ) ;
#64680 = CARTESIAN_POINT ( 'NONE',  ( -133.3122825023497171, 52.81354457049841500, -95.00000000000133582 ) ) ;
#64681 = AXIS2_PLACEMENT_3D ( 'NONE', #66646, #54670, #38866 ) ;
#64682 = AXIS2_PLACEMENT_3D ( 'NONE', #10909, #53464, #4600 ) ;
#64683 = CARTESIAN_POINT ( 'NONE',  ( 563.4809901518626702, 0.000000000000000000, 57.79371821540657095 ) ) ;
#64684 = CARTESIAN_POINT ( 'NONE',  ( 69.38689814754611973, 14.24120947374744794, 87.03124869162181199 ) ) ;
#64685 = PLANE ( 'NONE',  #40410 ) ;
#64686 = CARTESIAN_POINT ( 'NONE',  ( 0.000000000000000000, 0.000000000000000000, 40.00000000000003553 ) ) ;
#64687 = DIRECTION ( 'NONE',  ( 1.000000000000000000, 0.000000000000000000, 0.000000000000000000 ) ) ;
#64688 = ORIENTED_EDGE ( 'NONE', *, *, #53799, .T. ) ;
#64690 = AXIS2_PLACEMENT_3D ( 'NONE', #34605, #18403, #34247 ) ;
#64689 = CARTESIAN_POINT ( 'NONE',  ( -444.4229916354184411, 388.0000000000064801, -128.9497041420121093 ) ) ;
#64691 = ORIENTED_EDGE ( 'NONE', *, *, #22700, .F. ) ;
#64692 = CYLINDRICAL_SURFACE ( 'NONE', #46455, 7.500000000000020428 ) ;
#64693 = CARTESIAN_POINT ( 'NONE',  ( 211.3917124729450165, 115.9987099435923597, -67.27654017559783028 ) ) ;
#64694 = CARTESIAN_POINT ( 'NONE',  ( 311.8713128290285113, 188.0000000000000000, 346.5826552340383842 ) ) ;
#64695 = CARTESIAN_POINT ( 'NONE',  ( -71.97434903038468690, 19.88430675376529777, 7.650924302885536044 ) ) ;
#64696 = CARTESIAN_POINT ( 'NONE',  ( -36.50102476951193609, 10.47699908632348276, -90.95548803688076589 ) ) ;
#64697 = DIRECTION ( 'NONE',  ( 1.000000000000000000, 0.000000000000000000, -0.000000000000000000 ) ) ;
#64698 = CARTESIAN_POINT ( 'NONE',  ( 198.2682806192667329, 97.92400992302502516, 86.53030137829317425 ) ) ;
#64699 = CARTESIAN_POINT ( 'NONE',  ( 160.4986104110022893, 61.33701824525265778, -63.60348852922437146 ) ) ;
#64700 = ORIENTED_EDGE ( 'NONE', *, *, #18798, .T. ) ;
#64701 = CARTESIAN_POINT ( 'NONE',  ( 0.000000000000000000, 0.000000000000000000, 0.000000000000000000 ) ) ;
#64702 = CYLINDRICAL_SURFACE ( 'NONE', #68954, 7.500000000000013323 ) ;
#64703 = ORIENTED_EDGE ( 'NONE', *, *, #54622, .F. ) ;
#64704 = EDGE_LOOP ( 'NONE', ( #11567, #29113, #38617, #42457 ) ) ;
#64705 = CARTESIAN_POINT ( 'NONE',  ( -81.00507684688699328, 23.22613445438386748, 45.04825155395133862 ) ) ;
#64707 = EDGE_CURVE ( 'NONE', #46832, #50676, #65082, .T. ) ;
#64706 = DIRECTION ( 'NONE',  ( 0.000000000000000000, 0.000000000000000000, -1.000000000000000000 ) ) ;
#64708 = CARTESIAN_POINT ( 'NONE',  ( 45.89268866913130296, 10.36133864615983136, 41.17961490824062309 ) ) ;
#64709 = CARTESIAN_POINT ( 'NONE',  ( -25.98312968277007329, 8.759224980175247310, 59.40908211529054483 ) ) ;
#64710 = CARTESIAN_POINT ( 'NONE',  ( 24.46491470961361614, -5.710143558202974923, 0.000000000000000000 ) ) ;
#64711 = EDGE_CURVE ( 'NONE', #26921, #24137, #67776, .T. ) ;
#64712 = ORIENTED_EDGE ( 'NONE', *, *, #16655, .T. ) ;
#64713 = ADVANCED_FACE ( 'NONE', ( #36106 ), #46996, .F. ) ;
#64714 = ORIENTED_EDGE ( 'NONE', *, *, #17571, .T. ) ;
#64715 = CARTESIAN_POINT ( 'NONE',  ( -130.1938957973835329, 50.61368074696266461, 31.95741200596453879 ) ) ;
#64716 = ORIENTED_EDGE ( 'NONE', *, *, #11317, .F. ) ;
#64717 = DIRECTION ( 'NONE',  ( -1.000000000000000000, 0.000000000000000000, 0.000000000000000000 ) ) ;
#64718 = CARTESIAN_POINT ( 'NONE',  ( -149.5074843970971017, 65.50121172469319220, 30.72082123989904545 ) ) ;
#64719 = CARTESIAN_POINT ( 'NONE',  ( 59.08638499266953659, 11.79550614876701431, 57.76452535348534667 ) ) ;
#64720 = CARTESIAN_POINT ( 'NONE',  ( -4.502148936856958272, 7.704491846230413721, 71.20160539119055443 ) ) ;
#64721 = PRODUCT_DEFINITION_SHAPE ( 'NONE', 'NONE',  #65913 ) ;
#64722 = CARTESIAN_POINT ( 'NONE',  ( 0.000000000000000000, 0.000000000000000000, 0.000000000000000000 ) ) ;
#64723 = FACE_OUTER_BOUND ( 'NONE', #66784, .T. ) ;
#64724 = CIRCLE ( 'NONE', #37750, 65.00000000000000000 ) ;
#64725 = EDGE_CURVE ( 'NONE', #41104, #49158, #68457, .T. ) ;
#64726 = DIRECTION ( 'NONE',  ( -0.9999168736529502333, 0.000000000000000000, 0.01289363347198224652 ) ) ;
#64727 = VERTEX_POINT ( 'NONE', #3401 ) ;
#64728 = ORIENTED_EDGE ( 'NONE', *, *, #469, .F. ) ;
#64729 = DIRECTION ( 'NONE',  ( 0.000000000000000000, -0.9989683093773507050, -0.04541273895899305274 ) ) ;
#64730 = LINE ( 'NONE', #22511, #42919 ) ;
#64731 = AXIS2_PLACEMENT_3D ( 'NONE', #68853, #20679, #63598 ) ;
#64732 = DIRECTION ( 'NONE',  ( 1.000000000000000000, 0.000000000000000000, 0.000000000000000000 ) ) ;
#64733 = CARTESIAN_POINT ( 'NONE',  ( 136.3292018078238925, 42.93753790426541883, -77.45239417490056155 ) ) ;
#64734 = CARTESIAN_POINT ( 'NONE',  ( 70.45466089417030275, 14.52203022703029589, 38.29938007412685153 ) ) ;
#64735 = VECTOR ( 'NONE', #434, 1000.000000000000000 ) ;
#64736 = AXIS2_PLACEMENT_3D ( 'NONE', #5039, #31776, #44047 ) ;
#64737 = ORIENTED_EDGE ( 'NONE', *, *, #16686, .F. ) ;
#64738 = AXIS2_PLACEMENT_3D ( 'NONE', #11156, #21712, #21367 ) ;
#64739 = VECTOR ( 'NONE', #36223, 1000.000000000000000 ) ;
#64740 = CARTESIAN_POINT ( 'NONE',  ( 80.72161230109723817, 17.48902961068031203, 5.720643767644356892 ) ) ;
#64741 = ORIENTED_EDGE ( 'NONE', *, *, #23968, .T. ) ;
#64742 = CARTESIAN_POINT ( 'NONE',  ( 24.46491470961352732, 5.710143558203322200, 3.061616997868437868E-16 ) ) ;
#64743 = VERTEX_POINT ( 'NONE', #13607 ) ;
#64744 = CIRCLE ( 'NONE', #65875, 4.250000000000000000 ) ;
#64745 = ORIENTED_EDGE ( 'NONE', *, *, #31320, .T. ) ;
#64746 = DIRECTION ( 'NONE',  ( 1.000000000000000000, 0.000000000000000000, 0.000000000000000000 ) ) ;
#64747 = CARTESIAN_POINT ( 'NONE',  ( 93.33480479917548678, 21.81892021443993102, 13.76463275447737900 ) ) ;
#64748 = LINE ( 'NONE', #12675, #22713 ) ;
#64749 = EDGE_LOOP ( 'NONE', ( #25288, #15657, #48851, #40107, #56841, #15843, #2777, #17499, #29027 ) ) ;
#64750 = DIRECTION ( 'NONE',  ( -0.000000000000000000, -0.000000000000000000, 1.000000000000000000 ) ) ;
#64751 = LINE ( 'NONE', #733, #67224 ) ;
#64752 = CARTESIAN_POINT ( 'NONE',  ( 154.0293889979057269, 55.02370422818218287, 30.22901195537932395 ) ) ;
#64753 = DIRECTION ( 'NONE',  ( 0.000000000000000000, 0.000000000000000000, 1.000000000000000000 ) ) ;
#64754 = CYLINDRICAL_SURFACE ( 'NONE', #60630, 125.0000000000000000 ) ;
#64755 = DIRECTION ( 'NONE',  ( -0.000000000000000000, -1.000000000000000000, -0.000000000000000000 ) ) ;
#64756 = DIRECTION ( 'NONE',  ( -1.000000000000000000, 0.000000000000000000, 0.000000000000000000 ) ) ;
#64757 = CARTESIAN_POINT ( 'NONE',  ( 134.7720294983483029, 43.15885542353190374, -62.91010168338426212 ) ) ;
#64758 = CARTESIAN_POINT ( 'NONE',  ( -142.5042386072304055, 59.74110826975216071, -71.89443917550980245 ) ) ;
#64759 = ORIENTED_EDGE ( 'NONE', *, *, #61583, .F. ) ;
#64760 = FACE_BOUND ( 'NONE', #17765, .T. ) ;
#64761 = CARTESIAN_POINT ( 'NONE',  ( 14.59045944429412600, 20.30070179093326743, 0.000000000000000000 ) ) ;
#64762 = CARTESIAN_POINT ( 'NONE',  ( -178.5750994113944614, 94.98114813978521909, 59.99381261644018792 ) ) ;
#64763 = DIRECTION ( 'NONE',  ( -0.000000000000000000, -0.000000000000000000, -1.000000000000000000 ) ) ;
#64764 = CARTESIAN_POINT ( 'NONE',  ( -5.066666666666664653, 0.000000000000000000, 43.13333333333333286 ) ) ;
#64765 = ADVANCED_FACE ( 'NONE', ( #56510, #41725, #29784, #51253, #24859, #24525 ), #57216, .F. ) ;
#64766 = CARTESIAN_POINT ( 'NONE',  ( -82.33596576276350731, 24.83688096733768091, 17.63268983951130764 ) ) ;
#64767 = CARTESIAN_POINT ( 'NONE',  ( -39.29440389294403246, 17.09499999999999886, 4.000000000000000000 ) ) ;
#64768 = CARTESIAN_POINT ( 'NONE',  ( 113.0520942216416387, 21.63891660051134380, -3.973857610334890378 ) ) ;
#64769 = DIRECTION ( 'NONE',  ( -0.000000000000000000, -0.000000000000000000, -1.000000000000000000 ) ) ;
#64770 = CARTESIAN_POINT ( 'NONE',  ( 68.45098769362925850, 13.99935947269948322, 5.294787831159208480 ) ) ;
#64771 = CARTESIAN_POINT ( 'NONE',  ( -84.23336401058607237, 25.60798568215574988, 69.81228689596302672 ) ) ;
#64772 = CARTESIAN_POINT ( 'NONE',  ( 88.28889510440060917, 21.05995314109334160, -9.159055693011952215 ) ) ;
#64773 = ORIENTED_EDGE ( 'NONE', *, *, #29125, .T. ) ;
#64774 = CARTESIAN_POINT ( 'NONE',  ( -34.74563762132952149, 11.17960945723138266, 17.60810679087929032 ) ) ;
#64775 = ORIENTED_EDGE ( 'NONE', *, *, #21591, .T. ) ;
#64776 = CARTESIAN_POINT ( 'NONE',  ( 107.9362503323352627, 27.82881837607799369, -63.11455838136814833 ) ) ;
#64777 = EDGE_LOOP ( 'NONE', ( #69184, #62980, #61389, #53494 ) ) ;
#64778 = CARTESIAN_POINT ( 'NONE',  ( -46.66904755831210139, 6.635317295611287136E-14, 2.000000000000001776 ) ) ;
#64779 = CIRCLE ( 'NONE', #64731, 65.00000000000000000 ) ;
#64780 = CARTESIAN_POINT ( 'NONE',  ( 104.5269485123011606, 27.42246137840687936, 85.93290527890958685 ) ) ;
#64781 = DIRECTION ( 'NONE',  ( 0.000000000000000000, 0.000000000000000000, 1.000000000000000000 ) ) ;
#64782 = CARTESIAN_POINT ( 'NONE',  ( 70.02892116572941461, 14.40944430928136732, -13.70672517636600141 ) ) ;
#64783 = CARTESIAN_POINT ( 'NONE',  ( -24.61094659556677300, 9.585225265507405723, -39.70484628576755881 ) ) ;
#64784 = AXIS2_PLACEMENT_3D ( 'NONE', #5714, #442, #21893 ) ;
#64785 = CARTESIAN_POINT ( 'NONE',  ( 211.2559569222079574, 117.6288368612911768, -93.86917793742070160 ) ) ;
#64786 = VECTOR ( 'NONE', #48542, 1000.000000000000000 ) ;
#64787 = LINE ( 'NONE', #6736, #67927 ) ;
#64788 = CARTESIAN_POINT ( 'NONE',  ( -124.9970785861867881, 47.10847819093959288, -23.01876740222969175 ) ) ;
#64789 = ORIENTED_EDGE ( 'NONE', *, *, #28685, .F. ) ;
#64790 = EDGE_CURVE ( 'NONE', #64201, #22983, #7985, .T. ) ;
#64791 = ORIENTED_EDGE ( 'NONE', *, *, #42105, .F. ) ;
#64793 = EDGE_CURVE ( 'NONE', #16235, #40950, #24515, .T. ) ;
#64792 = CARTESIAN_POINT ( 'NONE',  ( 31.95163392065795449, 8.568192436298476267, 63.26676829875925279 ) ) ;
#64794 = LINE ( 'NONE', #44017, #56320 ) ;
#64795 = VECTOR ( 'NONE', #1729, 1000.000000000000000 ) ;
#64796 = LINE ( 'NONE', #48580, #22917 ) ;
#64797 = PRODUCT_DEFINITION_CONTEXT ( 'detailed design', #435, 'design' ) ;
#64798 = ADVANCED_FACE ( 'NONE', ( #42062 ), #10055, .T. ) ;
#64799 = DIRECTION ( 'NONE',  ( -0.000000000000000000, -0.000000000000000000, -1.000000000000000000 ) ) ;
#64800 = ORIENTED_EDGE ( 'NONE', *, *, #27204, .F. ) ;
#64801 = LINE ( 'NONE', #27500, #55905 ) ;
#64802 = CARTESIAN_POINT ( 'NONE',  ( 187.6511924654682559, 87.00187850361886888, -20.51322464869038242 ) ) ;
#64803 = CARTESIAN_POINT ( 'NONE',  ( 212.1978255065451151, 119.0880569674902745, 10.21206011236483135 ) ) ;
#64804 = B_SPLINE_CURVE_WITH_KNOTS ( 'NONE', 3,
 ( #36409, #10353, #20919, #42372 ),
 .UNSPECIFIED., .F., .F.,
 ( 4, 4 ),
 ( 9.900409499183408838E-07, 0.05658314289920114704 ),
 .UNSPECIFIED. ) ;
#64805 = DIRECTION ( 'NONE',  ( 1.000000000000000000, 0.000000000000000000, 0.000000000000000000 ) ) ;
#64806 = CARTESIAN_POINT ( 'NONE',  ( 45.90128843543705273, 9.343910238294480308, -20.05022534619617858 ) ) ;
#64807 = CARTESIAN_POINT ( 'NONE',  ( 209.9944361927105092, 113.8994774711241433, -22.29641758310334865 ) ) ;
#64808 = CARTESIAN_POINT ( 'NONE',  ( 105.6635354938838844, 21.85802876872917366, -2.510136981039507997 ) ) ;
#64809 = CARTESIAN_POINT ( 'NONE',  ( 164.9706294237033717, 65.04392654036657007, 63.47989634801044900 ) ) ;
#64810 = EDGE_CURVE ( 'NONE', #12453, #48865, #31513, .T. ) ;
#64811 = ORIENTED_EDGE ( 'NONE', *, *, #52860, .T. ) ;
#64812 = DIRECTION ( 'NONE',  ( -0.000000000000000000, -0.000000000000000000, -1.000000000000000000 ) ) ;
#64813 = CARTESIAN_POINT ( 'NONE',  ( 94.11595392909980262, 23.18887043179186946, -42.80727100288617493 ) ) ;
#64814 = DIRECTION ( 'NONE',  ( -0.000000000000000000, -1.000000000000000000, 0.000000000000000000 ) ) ;
#64815 = DIRECTION ( 'NONE',  ( 0.000000000000000000, 0.000000000000000000, -1.000000000000000000 ) ) ;
#64816 = DIRECTION ( 'NONE',  ( -0.000000000000000000, -0.000000000000000000, 1.000000000000000000 ) ) ;
#64817 = EDGE_CURVE ( 'NONE', #52456, #35904, #8958, .T. ) ;
#64818 = EDGE_CURVE ( 'NONE', #40730, #41180, #21634, .T. ) ;
#64819 = CARTESIAN_POINT ( 'NONE',  ( -1.679734956245725552, 7.575464525743545785, 86.95611724131752851 ) ) ;
#64820 = VERTEX_POINT ( 'NONE', #63869 ) ;
#64821 = FACE_OUTER_BOUND ( 'NONE', #32282, .T. ) ;
#64822 = FACE_OUTER_BOUND ( 'NONE', #16663, .T. ) ;
#64823 = ORIENTED_EDGE ( 'NONE', *, *, #32737, .F. ) ;
#64824 = CIRCLE ( 'NONE', #43462, 74.99999999999998579 ) ;
#64825 = EDGE_LOOP ( 'NONE', ( #7438, #59013, #4008, #43010 ) ) ;
#64826 = DIRECTION ( 'NONE',  ( 0.000000000000000000, 0.000000000000000000, -1.000000000000000000 ) ) ;
#64827 = DIRECTION ( 'NONE',  ( 0.000000000000000000, 0.000000000000000000, 1.000000000000000000 ) ) ;
#64828 = CARTESIAN_POINT ( 'NONE',  ( 104.3805245147141818, 26.26278144139197579, 32.40695671971902669 ) ) ;
#64829 = ORIENTED_EDGE ( 'NONE', *, *, #63069, .T. ) ;
#64830 = AXIS2_PLACEMENT_3D ( 'NONE', #40403, #2097, #62205 ) ;
#64831 = CARTESIAN_POINT ( 'NONE',  ( -60.13226458141420494, 16.10241298991027392, -64.03742039381080531 ) ) ;
#64832 = CARTESIAN_POINT ( 'NONE',  ( 33.03722315490661998, 7.666819786578624729, -12.30021257897310605 ) ) ;
#64833 = CARTESIAN_POINT ( 'NONE',  ( -15.76129977463530274, 63.43731725181437042, 43.58025477438756212 ) ) ;
#64834 = CARTESIAN_POINT ( 'NONE',  ( -157.0079874970173819, 72.18249880494042259, -68.88373919596408257 ) ) ;
#64835 = LINE ( 'NONE', #31529, #8128 ) ;
#64836 = CARTESIAN_POINT ( 'NONE',  ( -452.6627218934860366, 395.0000000000064801, -123.9497041420119530 ) ) ;
#64837 = VECTOR ( 'NONE', #19366, 1000.000000000000000 ) ;
#64838 = VERTEX_POINT ( 'NONE', #16364 ) ;
#64839 = CARTESIAN_POINT ( 'NONE',  ( -47.56466076048273095, 13.83435953640667471, -43.20715939977046816 ) ) ;
#64840 = AXIS2_PLACEMENT_3D ( 'NONE', #12433, #28613, #34601 ) ;
#64841 = CYLINDRICAL_SURFACE ( 'NONE', #20188, 7.500000000000013323 ) ;
#64842 = CARTESIAN_POINT ( 'NONE',  ( 8.480977594057447888, 7.382886909400593112, 35.80792500536700373 ) ) ;
#64843 = DIRECTION ( 'NONE',  ( 0.000000000000000000, -1.000000000000000000, 0.000000000000000000 ) ) ;
#64844 = CARTESIAN_POINT ( 'NONE',  ( 79.37480438318435461, 17.07199765243625578, 92.83494011833366244 ) ) ;
#64846 = EDGE_LOOP ( 'NONE', ( #53404, #30204 ) ) ;
#64845 = FACE_OUTER_BOUND ( 'NONE', #23773, .T. ) ;
#64847 = ORIENTED_EDGE ( 'NONE', *, *, #59049, .F. ) ;
#64848 = ORIENTED_EDGE ( 'NONE', *, *, #61099, .F. ) ;
#64849 = CARTESIAN_POINT ( 'NONE',  ( -8.811275908848678284, 6.956777180392054838, -23.52454203392342791 ) ) ;
#64850 = CARTESIAN_POINT ( 'NONE',  ( -169.3240414452573930, 84.46994553661198779, 85.51843480329762315 ) ) ;
#64851 = CARTESIAN_POINT ( 'NONE',  ( -54.57280099357649306, 14.55288945003961487, -23.37177340799619785 ) ) ;
#64852 = EDGE_CURVE ( 'NONE', #62854, #57856, #20599, .T. ) ;
#64853 = DIRECTION ( 'NONE',  ( 0.000000000000000000, 0.000000000000000000, 1.000000000000000000 ) ) ;
#64854 = CARTESIAN_POINT ( 'NONE',  ( -57.65574514524056582, 16.43983577669855833, -49.75425646672815105 ) ) ;
#64855 = CARTESIAN_POINT ( 'NONE',  ( -8.314488422519708877, 7.931352979988702145, -23.57352014148016650 ) ) ;
#64856 = CARTESIAN_POINT ( 'NONE',  ( 154.6667526376337207, 55.50347409140650257, -63.50879352240995956 ) ) ;
#64857 = CARTESIAN_POINT ( 'NONE',  ( 18.21423326326597802, 6.590134686181415624, -9.060803352357556406 ) ) ;
#64859 = EDGE_LOOP ( 'NONE', ( #39798, #20137, #60189, #60691 ) ) ;
#64858 = ADVANCED_FACE ( 'NONE', ( #37127 ), #59265, .T. ) ;
#64860 = LINE ( 'NONE', #49353, #32913 ) ;
#64861 = ORIENTED_EDGE ( 'NONE', *, *, #31843, .F. ) ;
#64862 = ORIENTED_EDGE ( 'NONE', *, *, #33445, .T. ) ;
#64863 = CARTESIAN_POINT ( 'NONE',  ( -145.3233446620410518, 62.00659513626053609, 17.61759092328014731 ) ) ;
#64864 = CARTESIAN_POINT ( 'NONE',  ( -59.45661995832976032, 16.95372133001488990, -90.31914386384646320 ) ) ;
#64865 = CYLINDRICAL_SURFACE ( 'NONE', #26734, 4.999999999999997335 ) ;
#64866 = CARTESIAN_POINT ( 'NONE',  ( -156.6862310659955426, 71.88416263379563986, 13.61984221008611584 ) ) ;
#64868 = DIRECTION ( 'NONE',  ( 0.000000000000000000, 0.000000000000000000, 1.000000000000000000 ) ) ;
#64867 = VECTOR ( 'NONE', #3156, 1000.000000000000000 ) ;
#64869 = CARTESIAN_POINT ( 'NONE',  ( 16.28371206594635012, 6.516665886438622657, 45.01470767270525641 ) ) ;
#64870 = CARTESIAN_POINT ( 'NONE',  ( 157.4703587214989113, 58.92748579479258808, -77.96873488960135035 ) ) ;
#64871 = ORIENTED_EDGE ( 'NONE', *, *, #47863, .F. ) ;
#64872 = EDGE_CURVE ( 'NONE', #40691, #15039, #27254, .T. ) ;
#64873 = ORIENTED_EDGE ( 'NONE', *, *, #47873, .T. ) ;
#64874 = ORIENTED_EDGE ( 'NONE', *, *, #46058, .F. ) ;
#64875 = EDGE_CURVE ( 'NONE', #27414, #22171, #533, .T. ) ;
#64876 = AXIS2_PLACEMENT_3D ( 'NONE', #52429, #41532, #24673 ) ;
#64877 = DIRECTION ( 'NONE',  ( -0.7071067811865476838, 0.000000000000000000, -0.7071067811865474617 ) ) ;
#64878 = CARTESIAN_POINT ( 'NONE',  ( -156.9900125991010214, 72.16580261738673130, -16.05494244269402060 ) ) ;
#64879 = CARTESIAN_POINT ( 'NONE',  ( 33.93974911725172916, 8.773765372885550917, -48.26511037450102037 ) ) ;
#64880 = EDGE_CURVE ( 'NONE', #37023, #6692, #15148, .T. ) ;
#64881 = AXIS2_PLACEMENT_3D ( 'NONE', #51412, #41192, #67938 ) ;
#64882 = CARTESIAN_POINT ( 'NONE',  ( 26.11269837220809364, 20.55634918610396866, 2.000000000000001776 ) ) ;
#64883 = LINE ( 'NONE', #38137, #56576 ) ;
#64884 = VERTEX_POINT ( 'NONE', #49047 ) ;
#64885 = VECTOR ( 'NONE', #47182, 1000.000000000000000 ) ;
#64886 = DIRECTION ( 'NONE',  ( -1.000000000000000000, 0.000000000000000000, 0.000000000000000000 ) ) ;
#64887 = CARTESIAN_POINT ( 'NONE',  ( -154.2585856850056132, 68.31650218414625897, 59.25724188130881487 ) ) ;
#64888 = VECTOR ( 'NONE', #65457, 1000.000000000000000 ) ;
#64889 = DIRECTION ( 'NONE',  ( -1.000000000000000000, -0.000000000000000000, -0.000000000000000000 ) ) ;
#64890 = FACE_OUTER_BOUND ( 'NONE', #48795, .T. ) ;
#64891 = CARTESIAN_POINT ( 'NONE',  ( 410.0000000000000000, 190.0000000000000000, 0.000000000000000000 ) ) ;
#64892 = CYLINDRICAL_SURFACE ( 'NONE', #35324, 65.00000000000000000 ) ;
#64893 = DIRECTION ( 'NONE',  ( -1.334402673828313339E-16, 0.000000000000000000, 1.000000000000000000 ) ) ;
#64894 = CARTESIAN_POINT ( 'NONE',  ( 15.29293866748104413, 6.484959508098438796, -62.36349468914947636 ) ) ;
#64895 = CIRCLE ( 'NONE', #68275, 85.31295361348101380 ) ;
#64896 = ORIENTED_EDGE ( 'NONE', *, *, #61956, .F. ) ;
#64897 = CARTESIAN_POINT ( 'NONE',  ( -74.81012118577224612, 5.477980300262961677, 170.0000000000000000 ) ) ;
#64898 = APPLICATION_PROTOCOL_DEFINITION ( 'draft international standard', 'automotive_design', 1998, #41742 ) ;
#64899 = CARTESIAN_POINT ( 'NONE',  ( -128.7650348665117122, 48.41336321950709731, -62.32582547038258269 ) ) ;
#64900 = CARTESIAN_POINT ( 'NONE',  ( 0.000000000000000000, 0.000000000000000000, 170.0000000000000000 ) ) ;
#64901 = EDGE_CURVE ( 'NONE', #43828, #28243, #1231, .T. ) ;
#64902 = CARTESIAN_POINT ( 'NONE',  ( 41.35041461497707616, 8.670465437677179921, -62.70515334933006102 ) ) ;
#64903 = ADVANCED_FACE ( 'NONE', ( #39221 ), #1575, .F. ) ;
#64904 = CARTESIAN_POINT ( 'NONE',  ( 57.07246224906423038, 12.39953617563782906, -65.46404872146828779 ) ) ;
#64905 = EDGE_CURVE ( 'NONE', #8003, #59605, #65248, .T. ) ;
#64906 = ORIENTED_EDGE ( 'NONE', *, *, #17130, .T. ) ;
#64907 = ORIENTED_EDGE ( 'NONE', *, *, #51043, .T. ) ;
#64908 = ADVANCED_FACE ( 'NONE', ( #66321 ), #6146, .F. ) ;
#64909 = CARTESIAN_POINT ( 'NONE',  ( -23.93880457192868505, 8.479983864459171627, -15.73297272197446439 ) ) ;
#64910 = CARTESIAN_POINT ( 'NONE',  ( 176.7661391921448057, 74.34902671065451329, 84.35726248129530802 ) ) ;
#64911 = VERTEX_POINT ( 'NONE', #27604 ) ;
#64912 = ORIENTED_EDGE ( 'NONE', *, *, #18828, .F. ) ;
#64913 = CARTESIAN_POINT ( 'NONE',  ( 183.7875981612219789, 82.83906702837187197, 43.80766194854361828 ) ) ;
#64914 = CYLINDRICAL_SURFACE ( 'NONE', #14470, 65.00000000000000000 ) ;
#64915 = ORIENTED_EDGE ( 'NONE', *, *, #30493, .T. ) ;
#64916 = CARTESIAN_POINT ( 'NONE',  ( 117.4711568421290195, 33.49899443629672646, 66.02157968639461672 ) ) ;
#64917 = CARTESIAN_POINT ( 'NONE',  ( 137.3861614007145135, 44.78548268714475711, 70.47665649296068580 ) ) ;
#64918 = FACE_OUTER_BOUND ( 'NONE', #64307, .T. ) ;
#64919 = CARTESIAN_POINT ( 'NONE',  ( 81.99350056087827454, 17.89100316059847273, -91.11151605743467030 ) ) ;
#64920 = DIRECTION ( 'NONE',  ( -0.000000000000000000, -0.000000000000000000, 1.000000000000000000 ) ) ;
#64921 = CARTESIAN_POINT ( 'NONE',  ( -189.2826425734429563, 107.1493800926105990, 39.29612140121835040 ) ) ;
#64922 = AXIS2_PLACEMENT_3D ( 'NONE', #37213, #53381, #26670 ) ;
#64923 = ORIENTED_EDGE ( 'NONE', *, *, #1745, .F. ) ;
#64924 = ORIENTED_EDGE ( 'NONE', *, *, #47399, .T. ) ;
#64925 = SHAPE_REPRESENTATION ( 'key', ( #66832 ), #19752 ) ;
#64926 = VECTOR ( 'NONE', #12121, 1000.000000000000000 ) ;
#64927 = CARTESIAN_POINT ( 'NONE',  ( 8.000000000000001776, 0.000000000000000000, 0.000000000000000000 ) ) ;
#64928 = FACE_BOUND ( 'NONE', #21506, .T. ) ;
#64929 = CARTESIAN_POINT ( 'NONE',  ( -147.7925265216585160, 64.04960911618972830, -49.61744604605377873 ) ) ;
#64930 = AXIS2_PLACEMENT_3D ( 'NONE', #49557, #2106, #28471 ) ;
#64931 = CARTESIAN_POINT ( 'NONE',  ( -166.0012244511291328, 80.97916541034754800, -71.43140414274201078 ) ) ;
#64933 = ORIENTED_EDGE ( 'NONE', *, *, #27065, .T. ) ;
#64932 = CARTESIAN_POINT ( 'NONE',  ( -148.4259959918497032, 63.26767374754761875, -34.88804037928592550 ) ) ;
#64934 = LINE ( 'NONE', #43455, #2729 ) ;
#64935 = AXIS2_PLACEMENT_3D ( 'NONE', #29729, #51194, #69068 ) ;
#64936 = ORIENTED_EDGE ( 'NONE', *, *, #5952, .F. ) ;
#64937 = CARTESIAN_POINT ( 'NONE',  ( -130.2196570250629009, 49.40815211106351512, 31.97506308841684941 ) ) ;
#64938 = DIRECTION ( 'NONE',  ( -0.000000000000000000, -0.000000000000000000, -1.000000000000000000 ) ) ;
#64939 = LINE ( 'NONE', #31292, #24224 ) ;
#64940 = CARTESIAN_POINT ( 'NONE',  ( 87.10672734544988316, 20.64813880796636880, 29.71208757247930521 ) ) ;
#64941 = CARTESIAN_POINT ( 'NONE',  ( 81.03898448521320574, 17.58847173596441493, -21.50135784270763040 ) ) ;
#64942 = VECTOR ( 'NONE', #32588, 1000.000000000000000 ) ;
#64943 = PLANE ( 'NONE',  #54412 ) ;
#64944 = EDGE_CURVE ( 'NONE', #61225, #35602, #33251, .T. ) ;
#64945 = CARTESIAN_POINT ( 'NONE',  ( 200.8410151090926377, 101.2014854111317561, 16.30994292411162050 ) ) ;
#64946 = CARTESIAN_POINT ( 'NONE',  ( -94.84390436305042726, 29.16104988397310649, 12.18484969651350447 ) ) ;
#64947 = CARTESIAN_POINT ( 'NONE',  ( -95.86612279493097333, 29.64021615886203875, -65.46366992558145625 ) ) ;
#64948 = VERTEX_POINT ( 'NONE', #61017 ) ;
#64949 = ORIENTED_EDGE ( 'NONE', *, *, #27003, .T. ) ;
#64950 = CARTESIAN_POINT ( 'NONE',  ( 46.70715146412976537, 9.472433765546997009, 35.69789323664132752 ) ) ;
#64951 = CARTESIAN_POINT ( 'NONE',  ( -65.13282190615095146, -1.847197903505587038E-12, -9.999999999999998224 ) ) ;
#64952 = DIRECTION ( 'NONE',  ( -0.000000000000000000, -0.000000000000000000, -1.000000000000000000 ) ) ;
#64953 = DIRECTION ( 'NONE',  ( 1.000000000000000000, 0.000000000000000000, 0.000000000000000000 ) ) ;
#64954 = CARTESIAN_POINT ( 'NONE',  ( 427.4999999999999432, 207.5000000000000284, -2.000000000000000000 ) ) ;
#64955 = CARTESIAN_POINT ( 'NONE',  ( -190.6985136298601731, 109.1272424661242582, -95.00000000000133582 ) ) ;
#64956 = CARTESIAN_POINT ( 'NONE',  ( 10.73115448446747244, -22.57968829347487727, 0.000000000000000000 ) ) ;
#64957 = CARTESIAN_POINT ( 'NONE',  ( -123.6618353044034535, 46.23845779494349273, 30.94497602649078516 ) ) ;
#64958 = CARTESIAN_POINT ( 'NONE',  ( 211.3917124729450165, 115.9987099435923170, 66.94621277672065673 ) ) ;
#64959 = EDGE_CURVE ( 'NONE', #46646, #6777, #11767, .T. ) ;
#64960 = VERTEX_POINT ( 'NONE', #38876 ) ;
#64961 = CARTESIAN_POINT ( 'NONE',  ( -24.71604178686819608, 9.599501655372943532, 7.538451900758993851 ) ) ;
#64962 = VERTEX_POINT ( 'NONE', #12484 ) ;
#64963 = CARTESIAN_POINT ( 'NONE',  ( -35.99432170610150195, 10.38324794858010414, 4.893849840022852504 ) ) ;
#64964 = CARTESIAN_POINT ( 'NONE',  ( -58.00979178563853367, 29.32343869649098878, 40.00000000000003553 ) ) ;
#64965 = EDGE_CURVE ( 'NONE', #45190, #41448, #12139, .T. ) ;
#64966 = CARTESIAN_POINT ( 'NONE',  ( 94.02499804464930833, 23.15433260743125743, 65.32863951667292213 ) ) ;
#64967 = CARTESIAN_POINT ( 'NONE',  ( 150.4544126017350720, 52.39556706174412426, -19.44410150025860773 ) ) ;
#64968 = CARTESIAN_POINT ( 'NONE',  ( 141.9165763529819344, -52.00000000000000711, 108.9999999999999858 ) ) ;
#64969 = EDGE_CURVE ( 'NONE', #7307, #47821, #1065, .T. ) ;
#64970 = CARTESIAN_POINT ( 'NONE',  ( -100.4347360276019430, 32.97716872911836106, -76.64346099625136333 ) ) ;
#64971 = DIRECTION ( 'NONE',  ( 1.000000000000000000, 0.000000000000000000, 0.000000000000000000 ) ) ;
#64972 = CARTESIAN_POINT ( 'NONE',  ( 15.55634918610400241, -15.55634918610406103, 85.00100000000000477 ) ) ;
#64973 = CYLINDRICAL_SURFACE ( 'NONE', #60056, 21.50000000000000000 ) ;
#64974 = VERTEX_POINT ( 'NONE', #1946 ) ;
#64975 = CARTESIAN_POINT ( 'NONE',  ( 55.91494169499917177, 12.16343363043255899, 66.58477365789052271 ) ) ;
#64976 = FILL_AREA_STYLE_COLOUR ( '', #10441 ) ;
#64977 = CARTESIAN_POINT ( 'NONE',  ( -9.765753193741730342, 8.033970690975920093, 3.522221867868848388 ) ) ;
#64978 = CARTESIAN_POINT ( 'NONE',  ( 41.80372346091803593, 9.750024116765242610, -62.85510525679180205 ) ) ;
#64979 = CARTESIAN_POINT ( 'NONE',  ( -62.41990535723909517, 16.78139727964023109, -95.00000000000133582 ) ) ;
#64980 = CARTESIAN_POINT ( 'NONE',  ( 429.8372781065087338, 394.9999999999999432, 96.05029585798857283 ) ) ;
#64981 = VECTOR ( 'NONE', #44209, 1000.000000000000000 ) ;
#64982 = CARTESIAN_POINT ( 'NONE',  ( 79.79351097043134189, 18.25397826796971756, 87.79632269537491140 ) ) ;
#64983 = AXIS2_PLACEMENT_3D ( 'NONE', #5290, #53457, #32717 ) ;
#64984 = ORIENTED_EDGE ( 'NONE', *, *, #66260, .F. ) ;
#64985 = DIRECTION ( 'NONE',  ( 0.000000000000000000, 0.000000000000000000, 1.000000000000000000 ) ) ;
#64986 = DIRECTION ( 'NONE',  ( -4.270088556250601699E-16, -0.000000000000000000, -1.000000000000000000 ) ) ;
#64987 = PLANE ( 'NONE',  #3991 ) ;
#64988 = EDGE_CURVE ( 'NONE', #49065, #39103, #22399, .T. ) ;
#64989 = CARTESIAN_POINT ( 'NONE',  ( 230.9999999999999432, -57.00000000000007816, 72.99999999999998579 ) ) ;
#64990 = VECTOR ( 'NONE', #36578, 1000.000000000000000 ) ;
#64991 = CARTESIAN_POINT ( 'NONE',  ( -129.6079169496900931, 50.20899308323958365, -35.89371998164833144 ) ) ;
#64992 = ORIENTED_EDGE ( 'NONE', *, *, #23312, .T. ) ;
#64993 = CARTESIAN_POINT ( 'NONE',  ( 6.933333333333328241, 8.000000000000000000, -11.86666666666666536 ) ) ;
#64994 = CARTESIAN_POINT ( 'NONE',  ( -41.65447218327533818, -2.493917879428980910, 13.79046340968178441 ) ) ;
#64995 = EDGE_CURVE ( 'NONE', #14111, #27023, #53191, .T. ) ;
#64996 = CARTESIAN_POINT ( 'NONE',  ( 198.2581645178918563, 99.52881771501678543, -13.12609424774730371 ) ) ;
#64997 = CARTESIAN_POINT ( 'NONE',  ( -144.0355355870767653, 59.67305119280410963, 86.74176708214653786 ) ) ;
#64998 = LINE ( 'NONE', #11505, #57154 ) ;
#64999 = ORIENTED_EDGE ( 'NONE', *, *, #42565, .F. ) ;
#65000 = LINE ( 'NONE', #58664, #63719 ) ;
#65001 = CARTESIAN_POINT ( 'NONE',  ( 84.72546926745364715, 19.84015517905186243, 17.63786239785293830 ) ) ;
#65002 = MANIFOLD_SOLID_BREP ( 'Boss-Extrude1', #31666 ) ;
#65003 = CARTESIAN_POINT ( 'NONE',  ( -94.83091526606384036, 30.26550147229323784, 37.00308990492074201 ) ) ;
#65004 = FACE_OUTER_BOUND ( 'NONE', #5718, .T. ) ;
#65005 = VERTEX_POINT ( 'NONE', #62048 ) ;
#65006 = DIRECTION ( 'NONE',  ( 0.000000000000000000, -1.000000000000000000, 0.000000000000000000 ) ) ;
#65007 = ORIENTED_EDGE ( 'NONE', *, *, #42849, .T. ) ;
#65008 = VERTEX_POINT ( 'NONE', #24089 ) ;
#65009 = CARTESIAN_POINT ( 'NONE',  ( -71.56718866013693514, 19.74312628447963647, -13.29964426657915766 ) ) ;
#65010 = CARTESIAN_POINT ( 'NONE',  ( -15.55634918610400597, 15.55634918610405748, 0.000000000000000000 ) ) ;
#65012 = ORIENTED_EDGE ( 'NONE', *, *, #40876, .F. ) ;
#65011 = CARTESIAN_POINT ( 'NONE',  ( 152.1153500913667358, 54.85403770686895086, 15.32190511181030601 ) ) ;
#65013 = CARTESIAN_POINT ( 'NONE',  ( -173.1211646369891355, 87.12891641440857882, 30.82169460664101734 ) ) ;
#65014 = CARTESIAN_POINT ( 'NONE',  ( -22.50000000000003197, -18.06806526123148160, 0.000000000000000000 ) ) ;
#65015 = CARTESIAN_POINT ( 'NONE',  ( -25.87147652227456263, 100.0000000000000000, 129.5802547743875550 ) ) ;
#65016 = ORIENTED_EDGE ( 'NONE', *, *, #54127, .T. ) ;
#65017 = CARTESIAN_POINT ( 'NONE',  ( -142.0747101610765242, 59.40211529287933701, -95.00000000000133582 ) ) ;
#65018 = ADVANCED_FACE ( 'NONE', ( #55741 ), #56427, .F. ) ;
#65019 = CARTESIAN_POINT ( 'NONE',  ( -32.41982179707235900, 9.753975577087185656, -23.42419288917794873 ) ) ;
#65020 = EDGE_CURVE ( 'NONE', #6794, #23524, #30392, .T. ) ;
#65021 = CARTESIAN_POINT ( 'NONE',  ( -180.0154536325056824, 96.73346874014735874, 41.28871520911766879 ) ) ;
#65022 = CARTESIAN_POINT ( 'NONE',  ( 129.1310456962234809, 39.80382822048402147, 58.01066127129433880 ) ) ;
#65023 = ORIENTED_EDGE ( 'NONE', *, *, #24558, .F. ) ;
#65024 = AXIS2_PLACEMENT_3D ( 'NONE', #56095, #24446, #40954 ) ;
#65025 = ORIENTED_EDGE ( 'NONE', *, *, #6808, .F. ) ;
#65026 = ORIENTED_EDGE ( 'NONE', *, *, #53401, .T. ) ;
#65027 = AXIS2_PLACEMENT_3D ( 'NONE', #27778, #11585, #10207 ) ;
#65028 = CARTESIAN_POINT ( 'NONE',  ( -48.26386693105755654, 12.96570170253255405, 94.71075846305346602 ) ) ;
#65029 = DIRECTION ( 'NONE',  ( -2.922263668027335568E-20, -1.000000000000000000, -1.110223024625156294E-16 ) ) ;
#65030 = CARTESIAN_POINT ( 'NONE',  ( 69.54076065159397047, 14.28133484589228175, 94.71504016972204454 ) ) ;
#65031 = FACE_OUTER_BOUND ( 'NONE', #42853, .T. ) ;
#65032 = CARTESIAN_POINT ( 'NONE',  ( -126.8005235842505840, 47.09307471149450919, 72.42308343011845295 ) ) ;
#65033 = CARTESIAN_POINT ( 'NONE',  ( -55.70897216137028352, 15.90023021009871407, 84.00879926019972288 ) ) ;
#65034 = CARTESIAN_POINT ( 'NONE',  ( -39.29440389294403246, 17.09499999999999886, 4.000000000000000000 ) ) ;
#65035 = ORIENTED_EDGE ( 'NONE', *, *, #56538, .T. ) ;
#65036 = CARTESIAN_POINT ( 'NONE',  ( -98.45346891396377487, 31.99841271297070122, -89.74978154278917941 ) ) ;
#65037 = ORIENTED_EDGE ( 'NONE', *, *, #22700, .T. ) ;
#65038 = DIRECTION ( 'NONE',  ( -0.000000000000000000, 1.000000000000000000, -0.000000000000000000 ) ) ;
#65039 = EDGE_CURVE ( 'NONE', #15022, #21328, #20146, .T. ) ;
#65040 = CARTESIAN_POINT ( 'NONE',  ( 209.5118425285948547, 113.1852661712287329, -64.91501104591304738 ) ) ;
#65041 = DIRECTION ( 'NONE',  ( -0.000000000000000000, -0.000000000000000000, -1.000000000000000000 ) ) ;
#65042 = EDGE_CURVE ( 'NONE', #52163, #6017, #7804, .T. ) ;
#65043 = DIRECTION ( 'NONE',  ( -0.000000000000000000, 1.000000000000000000, -0.000000000000000000 ) ) ;
#65044 = CARTESIAN_POINT ( 'NONE',  ( -124.9915686518654638, 47.10215472274616388, 72.46449846362082781 ) ) ;
#65045 = CARTESIAN_POINT ( 'NONE',  ( 22.51849650178395379, 7.817407610814553820, 40.83350911454274268 ) ) ;
#65046 = DIRECTION ( 'NONE',  ( 1.000000000000000000, 1.387778780781448634E-16, -1.387778780781445676E-15 ) ) ;
#65047 = CARTESIAN_POINT ( 'NONE',  ( 99.99999999999997158, 6.000000000000000000, -25.00000000000000000 ) ) ;
#65048 = CARTESIAN_POINT ( 'NONE',  ( 163.7379901688712778, 64.00402364591249693, -66.34155096030688981 ) ) ;
#65049 = ORIENTED_EDGE ( 'NONE', *, *, #4904, .F. ) ;
#65050 = CARTESIAN_POINT ( 'NONE',  ( 200.0000000000000000, 3.000000000000030198, -46.99999999999997158 ) ) ;
#65051 = CARTESIAN_POINT ( 'NONE',  ( -16.35146342289083776, -18.91109843266265500, 0.000000000000000000 ) ) ;
#65052 = VERTEX_POINT ( 'NONE', #24776 ) ;
#65053 = DIRECTION ( 'NONE',  ( -1.000000000000000000, 0.000000000000000000, 0.000000000000000000 ) ) ;
#65054 = SURFACE_SIDE_STYLE ('',( #15573 ) ) ;
#65055 = ORIENTED_EDGE ( 'NONE', *, *, #64707, .T. ) ;
#65056 = CARTESIAN_POINT ( 'NONE',  ( -83.69653436244855982, 24.30167057287991028, 43.48670558365605388 ) ) ;
#65057 = DIRECTION ( 'NONE',  ( 0.000000000000000000, 1.000000000000000000, -0.000000000000000000 ) ) ;
#65058 = CARTESIAN_POINT ( 'NONE',  ( 45.35621884287174765, 10.27694987765648627, 32.82727971635760866 ) ) ;
#65059 = FILL_AREA_STYLE_COLOUR ( '', #4691 ) ;
#65060 = DIRECTION ( 'NONE',  ( -1.000000000000000000, 0.000000000000000000, 0.000000000000000000 ) ) ;
#65061 = ORIENTED_EDGE ( 'NONE', *, *, #15906, .F. ) ;
#65062 = ORIENTED_EDGE ( 'NONE', *, *, #41069, .F. ) ;
#65063 = AXIS2_PLACEMENT_3D ( 'NONE', #62949, #47440, #14758 ) ;
#65064 = CARTESIAN_POINT ( 'NONE',  ( 122.2516123306975402, 190.0000000000000000, -91.28179539054376335 ) ) ;
#65065 = ORIENTED_EDGE ( 'NONE', *, *, #61497, .T. ) ;
#65066 = CARTESIAN_POINT ( 'NONE',  ( 34.83823433017388282, 8.871835168107974567, -22.24740203346240719 ) ) ;
#65067 = CARTESIAN_POINT ( 'NONE',  ( -1.666933348992582609, 64.97862212458815634, 170.0000000000000000 ) ) ;
#65068 = CARTESIAN_POINT ( 'NONE',  ( 59.29615173875418321, 11.84060224810188444, 57.64020183933660491 ) ) ;
#65069 = CARTESIAN_POINT ( 'NONE',  ( -3.862560291631546239, 7.672660553664875316, 58.08788247764030643 ) ) ;
#65070 = CARTESIAN_POINT ( 'NONE',  ( -31.43908319763710679, 10.61114334766713796, -89.00629854612920155 ) ) ;
#65071 = DIRECTION ( 'NONE',  ( 1.000000000000000000, 0.000000000000000000, -0.000000000000000000 ) ) ;
#65072 = ORIENTED_EDGE ( 'NONE', *, *, #36509, .T. ) ;
#65073 = CARTESIAN_POINT ( 'NONE',  ( -119.6995109608660925, 42.54844499216736153, -73.49440844546555240 ) ) ;
#65074 = ORIENTED_EDGE ( 'NONE', *, *, #21903, .F. ) ;
#65075 = VECTOR ( 'NONE', #15006, 1000.000000000000000 ) ;
#65076 = ORIENTED_EDGE ( 'NONE', *, *, #50807, .F. ) ;
#65077 = CARTESIAN_POINT ( 'NONE',  ( 159.2319614735955895, 59.03334608081208046, -24.08327306185856997 ) ) ;
#65078 = FACE_OUTER_BOUND ( 'NONE', #1055, .T. ) ;
#65079 = DIRECTION ( 'NONE',  ( -1.000000000000000000, -0.000000000000000000, -0.000000000000000000 ) ) ;
#65080 = CARTESIAN_POINT ( 'NONE',  ( 140.0614732283738988, 45.29930344725074320, -74.58837468684397720 ) ) ;
#65081 = DIRECTION ( 'NONE',  ( -0.9009688679024155933, -0.4338837391175656699, 0.000000000000000000 ) ) ;
#65082 = CIRCLE ( 'NONE', #26914, 4.999999999999997335 ) ;
#65083 = ORIENTED_EDGE ( 'NONE', *, *, #473, .F. ) ;
#65084 = CARTESIAN_POINT ( 'NONE',  ( 81.03898448521321995, 17.58847173596441849, 5.343192747756050132 ) ) ;
#65085 = LINE ( 'NONE', #53735, #50850 ) ;
#65086 = CARTESIAN_POINT ( 'NONE',  ( -71.59086462055188349, 19.75139532313338364, 35.41821401656284962 ) ) ;
#65087 = VERTEX_POINT ( 'NONE', #4010 ) ;
#65088 = CARTESIAN_POINT ( 'NONE',  ( 412.3372781065086201, 399.9999999999998863, 113.5502958579881891 ) ) ;
#65089 = EDGE_LOOP ( 'NONE', ( #13651, #29946, #69548, #27134, #14405, #48609 ) ) ;
#65090 = CYLINDRICAL_SURFACE ( 'NONE', #10580, 7.500000000000013323 ) ;
#65091 = CIRCLE ( 'NONE', #44866, 25.12245591505646303 ) ;
#65092 = CARTESIAN_POINT ( 'NONE',  ( 86.62931800182293784, 19.42108912189598158, 2.867536982015618019 ) ) ;
#65093 = EDGE_CURVE ( 'NONE', #48407, #11965, #52868, .T. ) ;
#65094 = CARTESIAN_POINT ( 'NONE',  ( 0.000000000000000000, 0.000000000000000000, 0.000000000000000000 ) ) ;
#65095 = ORIENTED_EDGE ( 'NONE', *, *, #68923, .F. ) ;
#65096 = CARTESIAN_POINT ( 'NONE',  ( 0.3167204509598202655, -5.377136764700215288, -6.686525924292707757 ) ) ;
#65097 = EDGE_CURVE ( 'NONE', #26073, #14985, #35335, .T. ) ;
#65098 = CARTESIAN_POINT ( 'NONE',  ( -442.6627218934912662, 394.9999999999998295, 99.85872701201111568 ) ) ;
#65099 = CARTESIAN_POINT ( 'NONE',  ( 31.91383250562745388, 8.564461488297011371, 37.90219752839882972 ) ) ;
#65100 = CARTESIAN_POINT ( 'NONE',  ( 63.99027454648600610, 13.93445177372598742, 29.86079229877851660 ) ) ;
#65101 = EDGE_CURVE ( 'NONE', #55398, #60669, #19039, .T. ) ;
#65102 = CARTESIAN_POINT ( 'NONE',  ( -17.89459634713148262, 72.78390022947087346, 41.38025477438755928 ) ) ;
#65103 = DIRECTION ( 'NONE',  ( 1.000000000000000000, 0.000000000000000000, 0.000000000000000000 ) ) ;
#65104 = DIRECTION ( 'NONE',  ( -1.850371928290090422E-16, 1.000000000000000000, 1.110223024625156171E-16 ) ) ;
#65105 = ORIENTED_EDGE ( 'NONE', *, *, #42256, .F. ) ;
#65106 = CARTESIAN_POINT ( 'NONE',  ( 109.9975424824652634, 18.08738615523480675, 402.4289050101931480 ) ) ;
#65107 = CARTESIAN_POINT ( 'NONE',  ( -148.6471085600699382, 64.76880961642447687, -76.62049576393286543 ) ) ;
#65108 = ORIENTED_EDGE ( 'NONE', *, *, #21582, .T. ) ;
#65110 = MANIFOLD_SOLID_BREP ( 'Shell1', #36198 ) ;
#65109 = EDGE_CURVE ( 'NONE', #4775, #32147, #51164, .T. ) ;
#65111 = VECTOR ( 'NONE', #23262, 1000.000000000000000 ) ;
#65112 = FACE_BOUND ( 'NONE', #56953, .T. ) ;
#65113 = CARTESIAN_POINT ( 'NONE',  ( -2.355184675731015975, 6.596450510445362347, -74.89939942152702201 ) ) ;
#65114 = CARTESIAN_POINT ( 'NONE',  ( -174.7903139851459855, 90.53182997092834228, 72.49021236485279474 ) ) ;
#65115 = CARTESIAN_POINT ( 'NONE',  ( 111.0232121500226299, 29.24301703641567229, -89.61153874658104712 ) ) ;
#65116 = B_SPLINE_CURVE_WITH_KNOTS ( 'NONE', 3,
 ( #14761, #57683, #36913, #9493, #30951, #25683, #53405, #63980, #26698, #31976, #47112, #37238, #68576, #5240, #20377, #41846, #53063, #48131, #36571, #9839, #43809, #52725, #4551, #26016, #68904, #42184, #63652, #10167, #4892, #26359, #47795, #21083, #42527, #45217, #29057, #1977, #55781, #39258, #27989, #49433, #44526, #12175, #23076, #2320 ),
 .UNSPECIFIED., .F., .F.,
 ( 4, 2, 2, 2, 2, 2, 2, 2, 2, 2, 2, 2, 2, 2, 2, 2, 2, 2, 2, 2, 2, 4 ),
 ( 0.000000000000000000, 0.001472974678681650317, 0.002209462018022476885, 0.002945949357363303236, 0.004418924036044937290, 0.005891898714726570042, 0.007364873393408203663, 0.008101360732749023075, 0.008837848072089841620, 0.01031082275077147524, 0.01178379742945310713, 0.01252028476879392047, 0.01325677210813473554, 0.01472974678681636569, 0.01546623412615717556, 0.01620272146549799064, 0.01767569614417961732, 0.01914867082286124400, 0.01988515816220205387, 0.02062164550154286721, 0.02209462018022449042, 0.02356759485890611364 ),
 .UNSPECIFIED. ) ;
#65117 = CARTESIAN_POINT ( 'NONE',  ( -120.5002574492099257, 44.22930148497321312, -37.19622962122973320 ) ) ;
#65118 = CARTESIAN_POINT ( 'NONE',  ( -81.89510452344295288, 24.66033552777454574, 4.287486826232798975 ) ) ;
#65119 = CARTESIAN_POINT ( 'NONE',  ( 0.000000000000000000, 0.000000000000000000, -10.00000000000000000 ) ) ;
#65120 = CARTESIAN_POINT ( 'NONE',  ( 110.0000000000000284, 21.42428528562853529, -5.000000000000004441 ) ) ;
#65121 = CARTESIAN_POINT ( 'NONE',  ( -71.28077210551055032, 19.64439276383075850, -95.00000000000133582 ) ) ;
#65122 = CARTESIAN_POINT ( 'NONE',  ( 74.94097818310312675, -1.250000000000021760, 41.38025477438755928 ) ) ;
#65123 = DIRECTION ( 'NONE',  ( 0.000000000000000000, 0.000000000000000000, 1.000000000000000000 ) ) ;
#65124 = CARTESIAN_POINT ( 'NONE',  ( 86.62931800182293784, 20.48449268398422518, -23.97701360844805407 ) ) ;
#65125 = ORIENTED_EDGE ( 'NONE', *, *, #11570, .F. ) ;
#65126 = LINE ( 'NONE', #16922, #67775 ) ;
#65127 = VERTEX_POINT ( 'NONE', #4687 ) ;
#65128 = CARTESIAN_POINT ( 'NONE',  ( -444.2277112916228816, 394.7494927581580555, 94.61947695070884379 ) ) ;
#65129 = EDGE_CURVE ( 'NONE', #53544, #43521, #37018, .T. ) ;
#65130 = VECTOR ( 'NONE', #14494, 1000.000000000000000 ) ;
#65131 = PLANE ( 'NONE',  #16323 ) ;
#65132 = CARTESIAN_POINT ( 'NONE',  ( 108.0746788553144313, 28.99562660843912099, 83.61346235993913467 ) ) ;
#65133 = LINE ( 'NONE', #16927, #61589 ) ;
#65134 = CARTESIAN_POINT ( 'NONE',  ( 63.01563776193090405, 12.67277567978497643, -8.876140241706053757 ) ) ;
#65136 = CARTESIAN_POINT ( 'NONE',  ( -25.07735481787161191, 9.648965052008776411, -46.79695794318186586 ) ) ;
#65135 = VECTOR ( 'NONE', #46477, 1000.000000000000000 ) ;
#65137 = CARTESIAN_POINT ( 'NONE',  ( -48.71337292867759317, 14.10768470390589435, -65.54550437577125876 ) ) ;
#65138 = DIRECTION ( 'NONE',  ( 0.000000000000000000, -1.000000000000000000, 0.000000000000000000 ) ) ;
#65139 = CARTESIAN_POINT ( 'NONE',  ( -120.6420427933462207, 44.31795133507804962, -20.92911245906258699 ) ) ;
#65140 = EDGE_LOOP ( 'NONE', ( #18474, #56540, #60008, #2359 ) ) ;
#65141 = ORIENTED_EDGE ( 'NONE', *, *, #43815, .T. ) ;
#65142 = CARTESIAN_POINT ( 'NONE',  ( 33.77444274891858811, 8.756048688386671941, 59.29431779835010730 ) ) ;
#65143 = CARTESIAN_POINT ( 'NONE',  ( 181.0840389613909736, 78.60582251573003987, 56.15314469597509373 ) ) ;
#65144 = CARTESIAN_POINT ( 'NONE',  ( -169.1116812882276577, 84.24296059722696839, 71.52038224641596287 ) ) ;
#65145 = CARTESIAN_POINT ( 'NONE',  ( 447.3372781065086201, 0.000000000000000000, 113.5502958579881749 ) ) ;
#65146 = AXIS2_PLACEMENT_3D ( 'NONE', #39424, #60875, #7431 ) ;
#65147 = CARTESIAN_POINT ( 'NONE',  ( 62.53356220515464514, 13.59349015304565000, -23.87614024170608573 ) ) ;
#65148 = ORIENTED_EDGE ( 'NONE', *, *, #29123, .T. ) ;
#65149 = CARTESIAN_POINT ( 'NONE',  ( 93.08073375333745503, 22.79826000593201485, 6.534512623384266305 ) ) ;
#65150 = CARTESIAN_POINT ( 'NONE',  ( -14.92903005859420951, 7.458185427130749723, 66.87855674452464427 ) ) ;
#65151 = CARTESIAN_POINT ( 'NONE',  ( 212.0104729185450765, 118.7959000526602722, 11.55940993411821793 ) ) ;
#65152 = DIRECTION ( 'NONE',  ( 0.6910626489868685329, -0.7227948638273878901, 0.000000000000000000 ) ) ;
#65153 = CARTESIAN_POINT ( 'NONE',  ( 45.34143264614440483, 9.256465810451189213, -20.86148856102304094 ) ) ;
#65154 = CARTESIAN_POINT ( 'NONE',  ( -18.89790202299119315, -62.20684691518632548, 170.0000000000000000 ) ) ;
#65155 = FACE_BOUND ( 'NONE', #61949, .T. ) ;
#65156 = CARTESIAN_POINT ( 'NONE',  ( -55.05276343752909440, 14.68156374112638041, -35.21632399845986328 ) ) ;
#65157 =( REPRESENTATION_RELATIONSHIP ('NONE','NONE', #40274, #64096 ) REPRESENTATION_RELATIONSHIP_WITH_TRANSFORMATION ( #56164 )SHAPE_REPRESENTATION_RELATIONSHIP( ) );
#65158 = ORIENTED_EDGE ( 'NONE', *, *, #14685, .F. ) ;
#65159 = DIRECTION ( 'NONE',  ( -0.000000000000000000, 1.000000000000000000, -0.000000000000000000 ) ) ;
#65160 = CARTESIAN_POINT ( 'NONE',  ( 90.30732934992394689, 21.77797012484620964, -36.76760811582850863 ) ) ;
#65161 = CARTESIAN_POINT ( 'NONE',  ( -55.05276343752909440, 15.72344139423348430, 57.16187836339483397 ) ) ;
#65162 = CYLINDRICAL_SURFACE ( 'NONE', #6235, 75.31295361348099959 ) ;
#65163 = CARTESIAN_POINT ( 'NONE',  ( 152.1327777395850660, 53.61712543276775023, 15.33955938004834607 ) ) ;
#65164 = VECTOR ( 'NONE', #12103, 1000.000000000000000 ) ;
#65165 = DIRECTION ( 'NONE',  ( -0.000000000000000000, 1.000000000000000000, -0.000000000000000000 ) ) ;
#65166 = EDGE_CURVE ( 'NONE', #634, #19763, #36713, .T. ) ;
#65167 = ORIENTED_EDGE ( 'NONE', *, *, #27091, .F. ) ;
#65168 = DIRECTION ( 'NONE',  ( 0.8465179929926601732, 0.5323601107705934199, 0.000000000000000000 ) ) ;
#65169 = PLANE ( 'NONE',  #67570 ) ;
#65170 = EDGE_LOOP ( 'NONE', ( #13625, #28731, #42637, #65479 ) ) ;
#65171 = ORIENTED_EDGE ( 'NONE', *, *, #35244, .F. ) ;
#65172 = FACE_OUTER_BOUND ( 'NONE', #58947, .T. ) ;
#65173 = CARTESIAN_POINT ( 'NONE',  ( 39.40195752203892710, 8.409560354027393103, -62.46436805589144114 ) ) ;
#65174 = CARTESIAN_POINT ( 'NONE',  ( 105.2506154496929298, 26.63995206619727796, 42.71361730424104053 ) ) ;
#65175 = VERTEX_POINT ( 'NONE', #26496 ) ;
#65176 = ORIENTED_EDGE ( 'NONE', *, *, #55743, .F. ) ;
#65177 = CARTESIAN_POINT ( 'NONE',  ( 36.31593203568480988, 8.028139509847019184, -23.11534131364107836 ) ) ;
#65178 = DIRECTION ( 'NONE',  ( -0.000000000000000000, -0.000000000000000000, -1.000000000000000000 ) ) ;
#65179 = AXIS2_PLACEMENT_3D ( 'NONE', #15349, #48704, #20967 ) ;
#65180 = CARTESIAN_POINT ( 'NONE',  ( -154.8006992380338716, 70.15733562427988090, -63.82271102350273395 ) ) ;
#65181 = CARTESIAN_POINT ( 'NONE',  ( 64.94098077424392557, 14.16208887966257102, 3.203578031880352839 ) ) ;
#65182 = CARTESIAN_POINT ( 'NONE',  ( 9.962235950565768050, -64.23203137738408941, 170.0000000000000000 ) ) ;
#65183 = B_SPLINE_CURVE_WITH_KNOTS ( 'NONE', 3,
 ( #38952, #55105, #6929, #18184, #28379, #50538, #49826, #34016, #55458, #50189, #23471, #44910, #35669, #40583, #66649, #13519, #56418, #67340, #14209, #61355, #8934, #8239, #57122, #67000 ),
 .UNSPECIFIED., .F., .F.,
 ( 4, 2, 2, 2, 2, 2, 2, 2, 2, 2, 2, 4 ),
 ( 0.000000000000000000, 0.001398572767507159443, 0.002097859151260731466, 0.002797145535014303273, 0.004195718302521427370, 0.005594291070028550167, 0.006992863837535672963, 0.007692150221289229158, 0.008391436605042785352, 0.009790009372549946312, 0.01048929575630352419, 0.01118858214005710207 ),
 .UNSPECIFIED. ) ;
#65184 = ADVANCED_FACE ( 'NONE', ( #25815, #64122 ), #58161, .T. ) ;
#65185 = CARTESIAN_POINT ( 'NONE',  ( -54.08816720029311398, 15.46531105893042302, -35.26310301817208881 ) ) ;
#65186 = CARTESIAN_POINT ( 'NONE',  ( 63.01563776193091826, 13.70579113808094718, -77.56524142263344856 ) ) ;
#65187 = CARTESIAN_POINT ( 'NONE',  ( -150.3214134925456449, 66.19890482612721883, -88.53518711165342836 ) ) ;
#65188 = DIRECTION ( 'NONE',  ( -0.000000000000000000, -0.000000000000000000, -1.000000000000000000 ) ) ;
#65189 = DIRECTION ( 'NONE',  ( -1.000000000000000000, 0.000000000000000000, 0.000000000000000000 ) ) ;
#65191 = ORIENTED_EDGE ( 'NONE', *, *, #3335, .F. ) ;
#65190 = DIRECTION ( 'NONE',  ( -0.000000000000000000, 1.000000000000000000, -0.000000000000000000 ) ) ;
#65192 = ORIENTED_EDGE ( 'NONE', *, *, #60489, .T. ) ;
#65193 = EDGE_CURVE ( 'NONE', #20959, #21223, #30227, .T. ) ;
#65194 = CIRCLE ( 'NONE', #11254, 65.00000000000000000 ) ;
#65195 = ORIENTED_EDGE ( 'NONE', *, *, #62495, .F. ) ;
#65196 = CARTESIAN_POINT ( 'NONE',  ( -10.46803069297985900, 7.077485182625206761, -9.050212947433250221 ) ) ;
#65197 = CARTESIAN_POINT ( 'NONE',  ( -165.6956608327360811, 80.66498882796977909, 93.08182273110395499 ) ) ;
#65198 = CARTESIAN_POINT ( 'NONE',  ( 4.549306917177319498, -73.43672186181514405, 73.58025477438755502 ) ) ;
#65199 = CARTESIAN_POINT ( 'NONE',  ( 0.000000000000000000, 65.13282190615278466, 5.000000000000000000 ) ) ;
#65200 = CARTESIAN_POINT ( 'NONE',  ( -62.55320287144887459, 17.87319849854531029, -42.47875363776260826 ) ) ;
#65201 = CARTESIAN_POINT ( 'NONE',  ( -11.14668121284976188, 8.139398342256733088, -9.344527173102546769 ) ) ;
#65202 = DIRECTION ( 'NONE',  ( -0.000000000000000000, -0.000000000000000000, 1.000000000000000000 ) ) ;
#65203 = CARTESIAN_POINT ( 'NONE',  ( 23.24028701062093916, 6.853614888934262517, -15.19644949956558655 ) ) ;
#65204 = ORIENTED_EDGE ( 'NONE', *, *, #54193, .T. ) ;
#65205 = FACE_OUTER_BOUND ( 'NONE', #67657, .T. ) ;
#65207 = ORIENTED_EDGE ( 'NONE', *, *, #35262, .T. ) ;
#65206 = B_SPLINE_CURVE_WITH_KNOTS ( 'NONE', 3,
 ( #68176, #40728, #30190, #62888, #25948, #9425, #47378, #56924, #57613, #68833, #30882, #51643, #3451, #57265, #46011, #42117, #52326, #19624, #63575, #8389, #29834, #14357, #25613, #3114, #46346, #24576, #47047, #68506, #41776, #62546, #63232, #22388, #42459, #16068, #64963, #36847, #16758, #64609, #5174, #54027, #58625, #47724, #26969, #15729 ),
 .UNSPECIFIED., .F., .F.,
 ( 4, 2, 2, 2, 2, 2, 2, 2, 2, 2, 2, 2, 2, 2, 2, 2, 2, 2, 2, 2, 2, 4 ),
 ( 7.152448122690996019E-18, 0.001476829494128814504, 0.002215244241193227610, 0.002953658988257641151, 0.004430488482386469966, 0.005907317976515297914, 0.007384147470644126729, 0.008122562217708542004, 0.008860976964772959014, 0.01033780645890178783, 0.01181463595303061838, 0.01255305070009503365, 0.01329146544715945066, 0.01476829494128827948, 0.01550670968835269822, 0.01624512443541711870, 0.01772195392954596660, 0.01919878342367481450, 0.01993719817073924191, 0.02067561291780366586, 0.02215244241193249294, 0.02362927190606132349 ),
 .UNSPECIFIED. ) ;
#65208 = ORIENTED_EDGE ( 'NONE', *, *, #66168, .T. ) ;
#65209 = EDGE_CURVE ( 'NONE', #67138, #33038, #69401, .T. ) ;
#65210 = LINE ( 'NONE', #22997, #7354 ) ;
#65211 = CARTESIAN_POINT ( 'NONE',  ( -59.95908162666859909, 17.10002565866494706, -90.72874173270432152 ) ) ;
#65212 = DIRECTION ( 'NONE',  ( 0.000000000000000000, 0.000000000000000000, -1.000000000000000000 ) ) ;
#65213 = AXIS2_PLACEMENT_3D ( 'NONE', #7963, #12200, #13248 ) ;
#65215 = EDGE_CURVE ( 'NONE', #16185, #64139, #32119, .T. ) ;
#65214 = CARTESIAN_POINT ( 'NONE',  ( -7.825402957745087207, -170.0000000000000000, -62.26262132240749736 ) ) ;
#65216 = LINE ( 'NONE', #44449, #49502 ) ;
#65217 = CARTESIAN_POINT ( 'NONE',  ( 22.53041628628730564, 6.810083298012989061, 40.83674206048191024 ) ) ;
#65218 = CARTESIAN_POINT ( 'NONE',  ( 141.3036441389950539, 47.31002705502925920, -17.71872056072848878 ) ) ;
#65219 = VERTEX_POINT ( 'NONE', #15253 ) ;
#65220 = ORIENTED_EDGE ( 'NONE', *, *, #27041, .F. ) ;
#65221 = VERTEX_POINT ( 'NONE', #9978 ) ;
#65222 = CARTESIAN_POINT ( 'NONE',  ( -55.05276343752909440, 15.72344139423348430, 45.31732777293115788 ) ) ;
#65223 = CARTESIAN_POINT ( 'NONE',  ( -7.825402957745085430, 6.891034867348157178, 18.27103044898354511 ) ) ;
#65224 = CARTESIAN_POINT ( 'NONE',  ( 59.95259601283824225, 11.98300577492411101, -23.22648120359055923 ) ) ;
#65225 = CARTESIAN_POINT ( 'NONE',  ( -38.92726670956012924, 10.94099576009806363, 64.07225517871486886 ) ) ;
#65226 = CARTESIAN_POINT ( 'NONE',  ( 197.3700262219431067, 98.41176242030790888, 65.18205950884318156 ) ) ;
#65227 = ORIENTED_EDGE ( 'NONE', *, *, #12559, .T. ) ;
#65228 = CARTESIAN_POINT ( 'NONE',  ( 188.5653887627528036, 88.01608521313130495, 63.04380369743464740 ) ) ;
#65229 = DIRECTION ( 'NONE',  ( 1.000000000000000000, -1.509903313490212895E-14, 0.000000000000000000 ) ) ;
#65230 = CARTESIAN_POINT ( 'NONE',  ( -0.3255842968951684346, 7.525381170773409956, -42.42579087474055655 ) ) ;
#65231 = DIRECTION ( 'NONE',  ( 1.000000000000000000, 0.000000000000000000, -0.000000000000000000 ) ) ;
#65232 = CARTESIAN_POINT ( 'NONE',  ( -84.96580414052108665, 24.82184094495578819, -38.53758876423822244 ) ) ;
#65233 = CARTESIAN_POINT ( 'NONE',  ( 0.000000000000000000, 0.000000000000000000, 0.000000000000000000 ) ) ;
#65234 = DIRECTION ( 'NONE',  ( -0.000000000000000000, 1.000000000000000000, -0.000000000000000000 ) ) ;
#65235 = CARTESIAN_POINT ( 'NONE',  ( 8.288451200428832877, 6.376395059685423305, -69.37159842231915263 ) ) ;
#65236 = VERTEX_POINT ( 'NONE', #37379 ) ;
#65237 = CARTESIAN_POINT ( 'NONE',  ( 41.49663191311417165, -50.03028622612021792, 40.00000000000003553 ) ) ;
#65238 = APPLICATION_PROTOCOL_DEFINITION ( 'draft international standard', 'automotive_design', 1998, #49323 ) ;
#65239 = VECTOR ( 'NONE', #54663, 1000.000000000000000 ) ;
#65240 = DIRECTION ( 'NONE',  ( 1.000000000000000000, 0.000000000000000000, 0.000000000000000000 ) ) ;
#65241 = LINE ( 'NONE', #42738, #17424 ) ;
#65242 = CARTESIAN_POINT ( 'NONE',  ( 422.4999999999999432, -18.06806526123148160, 0.000000000000000000 ) ) ;
#65243 = FACE_OUTER_BOUND ( 'NONE', #27456, .T. ) ;
#65244 = ORIENTED_EDGE ( 'NONE', *, *, #51181, .T. ) ;
#65245 = MECHANICAL_DESIGN_GEOMETRIC_PRESENTATION_REPRESENTATION (  '', ( #63151 ), #32657 ) ;
#65246 = ADVANCED_FACE ( 'NONE', ( #16281 ), #14896, .F. ) ;
#65247 = EDGE_LOOP ( 'NONE', ( #19297, #7026, #63219, #58176 ) ) ;
#65248 = LINE ( 'NONE', #22684, #43716 ) ;
#65249 = CARTESIAN_POINT ( 'NONE',  ( 178.3973431913384218, 75.93084153045994356, 83.46876488482124046 ) ) ;
#65250 = ORIENTED_EDGE ( 'NONE', *, *, #32094, .T. ) ;
#65251 = CIRCLE ( 'NONE', #40545, 4.999999999999999112 ) ;
#65252 = EDGE_CURVE ( 'NONE', #69309, #60552, #37734, .T. ) ;
#65253 = EDGE_LOOP ( 'NONE', ( #40446, #67515 ) ) ;
#65254 = FACE_OUTER_BOUND ( 'NONE', #35879, .T. ) ;
#65255 = FACE_OUTER_BOUND ( 'NONE', #6114, .T. ) ;
#65256 = ORIENTED_EDGE ( 'NONE', *, *, #6766, .T. ) ;
#65257 = DIRECTION ( 'NONE',  ( 0.04486483035050447404, 0.9989930665413151445, 0.000000000000000000 ) ) ;
#65258 = CARTESIAN_POINT ( 'NONE',  ( 140.9141742510256847, 47.05414327990549594, 61.26423157896623906 ) ) ;
#65259 = CARTESIAN_POINT ( 'NONE',  ( -73.79615177260656367, 20.52570924097572203, -36.89085579558944517 ) ) ;
#65260 = AXIS2_PLACEMENT_3D ( 'NONE', #36486, #63220, #4808 ) ;
#65261 = DIRECTION ( 'NONE',  ( -0.9639628606958512425, -0.2660368455666826670, 0.000000000000000000 ) ) ;
#65262 = DIRECTION ( 'NONE',  ( -1.000000000000000000, -1.001918046209079887E-14, 9.729495617646301779E-15 ) ) ;
#65263 = CARTESIAN_POINT ( 'NONE',  ( -52.67596829228261868, 15.09584868440940220, -23.00177376059447099 ) ) ;
#65264 = EDGE_CURVE ( 'NONE', #60452, #52426, #42667, .T. ) ;
#65265 = VERTEX_POINT ( 'NONE', #58836 ) ;
#65266 = ADVANCED_FACE ( 'NONE', ( #53553 ), #42327, .T. ) ;
#65267 = DIRECTION ( 'NONE',  ( 0.000000000000000000, 1.000000000000000000, 0.000000000000000000 ) ) ;
#65268 = FACE_BOUND ( 'NONE', #54722, .T. ) ;
#65269 = PLANE ( 'NONE',  #10208 ) ;
#65270 = EDGE_CURVE ( 'NONE', #35238, #16646, #66377, .T. ) ;
#65271 = LINE ( 'NONE', #42762, #54485 ) ;
#65273 = ORIENTED_EDGE ( 'NONE', *, *, #52182, .F. ) ;
#65272 = CARTESIAN_POINT ( 'NONE',  ( -130.9590960505229873, 49.92041220780520661, 86.26984079606188516 ) ) ;
#65274 = CARTESIAN_POINT ( 'NONE',  ( 62.04382205963243280, 13.48099884269681148, 17.92121075436126532 ) ) ;
#65275 = EDGE_CURVE ( 'NONE', #19323, #55869, #1860, .T. ) ;
#65276 = EDGE_LOOP ( 'NONE', ( #44669, #67923, #53363, #13508 ) ) ;
#65277 = CARTESIAN_POINT ( 'NONE',  ( -126.3458714439411352, 46.79154809309479646, 30.61994787315707001 ) ) ;
#65278 = LINE ( 'NONE', #17072, #63746 ) ;
#65279 = PLANE ( 'NONE',  #28739 ) ;
#65280 = CARTESIAN_POINT ( 'NONE',  ( 86.62931800182293784, 20.48449268398422518, 29.71208757247930521 ) ) ;
#65281 = CARTESIAN_POINT ( 'NONE',  ( 81.04675113612958626, 17.59091904316106536, -11.44449432899062202 ) ) ;
#65282 = PLANE ( 'NONE',  #46608 ) ;
#65283 = CARTESIAN_POINT ( 'NONE',  ( 89.87518614971253328, 20.55373388674513535, -76.94423166383461421 ) ) ;
#65284 = DIRECTION ( 'NONE',  ( 1.000000000000000000, 0.000000000000000000, 0.000000000000000000 ) ) ;
#65285 = DIRECTION ( 'NONE',  ( -0.000000000000000000, -1.000000000000000000, -0.000000000000000000 ) ) ;
#65286 = ORIENTED_EDGE ( 'NONE', *, *, #31350, .T. ) ;
#65287 = ORIENTED_EDGE ( 'NONE', *, *, #39463, .F. ) ;
#65288 = EDGE_CURVE ( 'NONE', #64530, #40830, #4477, .T. ) ;
#65289 = VECTOR ( 'NONE', #3307, 1000.000000000000000 ) ;
#65290 = CARTESIAN_POINT ( 'NONE',  ( 45.36109889487606495, 9.259412558041159258, 41.99414667629699238 ) ) ;
#65291 = CYLINDRICAL_SURFACE ( 'NONE', #31744, 7.500000000000013323 ) ;
#65292 = FACE_OUTER_BOUND ( 'NONE', #15728, .T. ) ;
#65294 = EDGE_CURVE ( 'NONE', #46298, #58415, #22256, .T. ) ;
#65293 = DIRECTION ( 'NONE',  ( 0.000000000000000000, 0.000000000000000000, -1.000000000000000000 ) ) ;
#65295 = ADVANCED_FACE ( 'NONE', ( #6423 ), #27877, .F. ) ;
#65296 = EDGE_CURVE ( 'NONE', #55255, #32221, #44399, .T. ) ;
#65297 = CARTESIAN_POINT ( 'NONE',  ( 209.6642862813004911, 115.2127693334913801, -49.46362703668027194 ) ) ;
#65298 = AXIS2_PLACEMENT_3D ( 'NONE', #8944, #14220, #24090 ) ;
#65299 = CYLINDRICAL_SURFACE ( 'NONE', #18004, 65.00000000000000000 ) ;
#65300 = CARTESIAN_POINT ( 'NONE',  ( 65.40383840050414221, 14.27443447873231186, -50.34691897934524718 ) ) ;
#65301 = CARTESIAN_POINT ( 'NONE',  ( 39.40195752203891999, 9.424259417798147354, -35.61981746542776506 ) ) ;
#65302 = CARTESIAN_POINT ( 'NONE',  ( 8.000000000000007105, 249.8719672152120381, -95.00000000000133582 ) ) ;
#65303 = PRODUCT_DEFINITION_SHAPE ( 'NONE', 'NONE',  #69599 ) ;
#65304 = ORIENTED_EDGE ( 'NONE', *, *, #27295, .T. ) ;
#65305 = CARTESIAN_POINT ( 'NONE',  ( -4.999999999999936939, 31.11269837220806167, 0.000000000000000000 ) ) ;
#65306 = ORIENTED_EDGE ( 'NONE', *, *, #53600, .F. ) ;
#65307 = AXIS2_PLACEMENT_3D ( 'NONE', #59635, #54715, #44872 ) ;
#65308 = COLOUR_RGB ( '',0.7921568627450980005, 0.8196078431372548767, 0.9333333333333333481 ) ;
#65309 = CARTESIAN_POINT ( 'NONE',  ( 9.962235950564870990, 64.23203137738423152, 73.58025477438756923 ) ) ;
#65310 = DIRECTION ( 'NONE',  ( 0.000000000000000000, 1.000000000000000000, 0.000000000000000000 ) ) ;
#65311 = CARTESIAN_POINT ( 'NONE',  ( 88.28889510440060917, 21.05995314109330963, 71.37459607837911335 ) ) ;
#65312 = CYLINDRICAL_SURFACE ( 'NONE', #17423, 7.500000000000013323 ) ;
#65313 = DIRECTION ( 'NONE',  ( -1.000000000000000000, 0.000000000000000000, 0.000000000000000000 ) ) ;
#65314 = CARTESIAN_POINT ( 'NONE',  ( -142.6736406357357794, 58.59303246027003098, 94.99999999999866418 ) ) ;
#65315 = AXIS2_PLACEMENT_3D ( 'NONE', #36673, #37341, #15561 ) ;
#65316 = PLANE ( 'NONE',  #66396 ) ;
#65317 = DIRECTION ( 'NONE',  ( 0.000000000000000000, -1.000000000000000000, 0.000000000000000000 ) ) ;
#65318 = LINE ( 'NONE', #54036, #41648 ) ;
#65319 = DIRECTION ( 'NONE',  ( 0.000000000000000000, 0.000000000000000000, -1.000000000000000000 ) ) ;
#65320 = ORIENTED_EDGE ( 'NONE', *, *, #40336, .T. ) ;
#65321 = CARTESIAN_POINT ( 'NONE',  ( 0.000000000000000000, 0.000000000000000000, 0.000000000000000000 ) ) ;
#65322 = CARTESIAN_POINT ( 'NONE',  ( 0.000000000000000000, 0.000000000000000000, 43.58025477438756212 ) ) ;
#65323 = CARTESIAN_POINT ( 'NONE',  ( 39.54205320694412507, -51.58901073076707888, 40.00000000000003553 ) ) ;
#65324 = DIRECTION ( 'NONE',  ( 0.000000000000000000, 1.000000000000000000, 0.000000000000000000 ) ) ;
#65325 = CARTESIAN_POINT ( 'NONE',  ( 281.3018128478065023, -21.46140473645479929, 4.838640910132730788 ) ) ;
#65326 = CARTESIAN_POINT ( 'NONE',  ( -108.9136445001389859, 36.28030794288189753, -65.85060173500423275 ) ) ;
#65327 = CARTESIAN_POINT ( 'NONE',  ( 83.49613381502568643, 19.43408251395296205, 84.07914609096779657 ) ) ;
#65328 = ORIENTED_EDGE ( 'NONE', *, *, #42718, .F. ) ;
#65329 = DIRECTION ( 'NONE',  ( -0.4127148655274872069, 0.9108602745606090290, 7.557850055494254020E-15 ) ) ;
#65330 = CARTESIAN_POINT ( 'NONE',  ( -189.2442476610617916, 107.0963225822736007, -14.83136874092102708 ) ) ;
#65331 = LINE ( 'NONE', #5875, #48838 ) ;
#65332 = CARTESIAN_POINT ( 'NONE',  ( -172.7173255566597163, 88.18461381371096763, -49.71195716475001092 ) ) ;
#65333 = ITEM_DEFINED_TRANSFORMATION ( 'NONE', 'NONE', #56872,  #66832 ) ;
#65334 = CARTESIAN_POINT ( 'NONE',  ( -128.9863978264384627, 49.78205252558956317, -35.57704840273653701 ) ) ;
#65335 = EDGE_LOOP ( 'NONE', ( #10166, #13862, #877, #5667 ) ) ;
#65336 = CARTESIAN_POINT ( 'NONE',  ( 204.6977192012829789, -170.0000000000000000, -78.17048162308530834 ) ) ;
#65337 = CARTESIAN_POINT ( 'NONE',  ( -25.10237775011639982, -1.004202417053851937, 0.000000000000000000 ) ) ;
#65338 = CARTESIAN_POINT ( 'NONE',  ( 211.9972138934681425, 190.0000000000000000, 276.7374251518728556 ) ) ;
#65339 = LINE ( 'NONE', #7652, #58501 ) ;
#65340 =( BOUNDED_CURVE ( )  B_SPLINE_CURVE ( 3, ( #23736, #56788, #13189, #2624 ),
 .UNSPECIFIED., .F., .F. ) 
 B_SPLINE_CURVE_WITH_KNOTS ( ( 4, 4 ),
 ( -2.664535259100375697E-15, 1.570796326794896558 ),
 .UNSPECIFIED. ) 
 CURVE ( )  GEOMETRIC_REPRESENTATION_ITEM ( )  RATIONAL_B_SPLINE_CURVE ( ( 1.000000000000000000, 0.8047378541243643824, 0.8047378541243643824, 1.000000000000000000 ) ) 
 REPRESENTATION_ITEM ( '' )  );
#65341 = ADVANCED_FACE ( 'NONE', ( #64821 ), #67404, .F. ) ;
#65342 = CARTESIAN_POINT ( 'NONE',  ( -4.999999999999936939, 36.11269837220805812, 2.000000000000001776 ) ) ;
#65343 = ORIENTED_EDGE ( 'NONE', *, *, #4439, .T. ) ;
#65344 = CARTESIAN_POINT ( 'NONE',  ( 164.2809400227150718, 64.46036035961996902, -94.16440510607482395 ) ) ;
#65345 = DIRECTION ( 'NONE',  ( -1.000000000000000000, 0.000000000000000000, 0.000000000000000000 ) ) ;
#65346 = CARTESIAN_POINT ( 'NONE',  ( 0.000000000000000000, 0.000000000000000000, -5.000000000000000888 ) ) ;
#65347 = VECTOR ( 'NONE', #9272, 1000.000000000000000 ) ;
#65348 = CARTESIAN_POINT ( 'NONE',  ( -173.1211646369891355, -170.0000000000000000, -34.71195716474998960 ) ) ;
#65349 = AXIS2_PLACEMENT_3D ( 'NONE', #31192, #41399, #8700 ) ;
#65351 = ORIENTED_EDGE ( 'NONE', *, *, #28519, .T. ) ;
#65350 = CARTESIAN_POINT ( 'NONE',  ( 117.4711568421290195, 33.49899443629672646, 12.33247850546726454 ) ) ;
#65352 = EDGE_CURVE ( 'NONE', #60210, #25097, #38078, .T. ) ;
#65353 = DIRECTION ( 'NONE',  ( 0.000000000000000000, -0.000000000000000000, -1.000000000000000000 ) ) ;
#65354 = EDGE_CURVE ( 'NONE', #30082, #36722, #50527, .T. ) ;
#65355 = VERTEX_POINT ( 'NONE', #6059 ) ;
#65356 = CONICAL_SURFACE ( 'NONE', #49617, 74.95140232871122521, 0.8777644062502172329 ) ;
#65357 = STYLED_ITEM ( 'NONE', ( #42575 ), #18036 ) ;
#65359 = ORIENTED_EDGE ( 'NONE', *, *, #58057, .T. ) ;
#65358 = EDGE_CURVE ( 'NONE', #32164, #31926, #40862, .T. ) ;
#65360 = CARTESIAN_POINT ( 'NONE',  ( 26.11269837220803325, -10.55634918610409656, 85.00100000000000477 ) ) ;
#65361 = CARTESIAN_POINT ( 'NONE',  ( -35.83016564023557748, 11.37623363089854678, -90.41096227095786730 ) ) ;
#65362 = ADVANCED_FACE ( 'NONE', ( #50386 ), #61960, .F. ) ;
#65364 = VERTEX_POINT ( 'NONE', #2539 ) ;
#65363 = CARTESIAN_POINT ( 'NONE',  ( -15.27594996066617128, 8.502079791899653571, -70.75202261163761364 ) ) ;
#65365 = CARTESIAN_POINT ( 'NONE',  ( -20.55634918610400419, 20.55634918610405748, 2.000000000000001776 ) ) ;
#65366 = VECTOR ( 'NONE', #37571, 1000.000000000000000 ) ;
#65367 = CARTESIAN_POINT ( 'NONE',  ( 209.3223706822284100, 18.00000000000002842, 31.44247402469554942 ) ) ;
#65368 = EDGE_CURVE ( 'NONE', #44265, #67613, #35239, .T. ) ;
#65369 = CARTESIAN_POINT ( 'NONE',  ( -76.10382222627281124, 22.43453174720079701, -35.56271879029210936 ) ) ;
#65370 = ORIENTED_EDGE ( 'NONE', *, *, #46447, .F. ) ;
#65371 = DIRECTION ( 'NONE',  ( -0.000000000000000000, -0.000000000000000000, -1.000000000000000000 ) ) ;
#65372 = CARTESIAN_POINT ( 'NONE',  ( -37.92542950990690542, 10.74638084523341419, -19.74604464320939456 ) ) ;
#65373 = DIRECTION ( 'NONE',  ( -0.000000000000000000, -0.000000000000000000, -1.000000000000000000 ) ) ;
#65374 = CARTESIAN_POINT ( 'NONE',  ( -38.54881010929334906, 10.86689971295294121, -67.22396423449106351 ) ) ;
#65375 = CARTESIAN_POINT ( 'NONE',  ( 18.19858669090300296, 7.596860100017452488, 71.46566277036495762 ) ) ;
#65376 = ORIENTED_EDGE ( 'NONE', *, *, #53398, .T. ) ;
#65377 = ORIENTED_EDGE ( 'NONE', *, *, #25373, .F. ) ;
#65378 = ORIENTED_EDGE ( 'NONE', *, *, #34300, .F. ) ;
#65380 = EDGE_CURVE ( 'NONE', #38832, #7537, #10095, .T. ) ;
#65379 = DIRECTION ( 'NONE',  ( 0.000000000000000000, 0.000000000000000000, 1.000000000000000000 ) ) ;
#65381 = CARTESIAN_POINT ( 'NONE',  ( -46.66904755831210139, 6.635317295611287136E-14, 2.000000000000001776 ) ) ;
#65382 = DIRECTION ( 'NONE',  ( -1.000000000000000000, -1.110223024625155594E-14, 1.110223024625155594E-14 ) ) ;
#65383 = CARTESIAN_POINT ( 'NONE',  ( -34.06864996337442619, 10.03773626259442153, -35.78902194044933083 ) ) ;
#65384 = CARTESIAN_POINT ( 'NONE',  ( -106.7799677022395031, 35.12603236357178815, 85.70035464166211625 ) ) ;
#65385 = EDGE_CURVE ( 'NONE', #1859, #17365, #30338, .T. ) ;
#65386 = CYLINDRICAL_SURFACE ( 'NONE', #60645, 5.000000000000000888 ) ;
#65387 = CARTESIAN_POINT ( 'NONE',  ( -127.6861178856153458, 47.68458428355326362, 72.26108953896540754 ) ) ;
#65388 = CARTESIAN_POINT ( 'NONE',  ( -59.74946260537818432, 17.03883958539088539, 85.65039846766379128 ) ) ;
#65389 = CARTESIAN_POINT ( 'NONE',  ( 79.14242532928585661, 17.00090225993928073, 64.56634896141592606 ) ) ;
#65390 = ORIENTED_EDGE ( 'NONE', *, *, #67854, .F. ) ;
#65391 = LINE ( 'NONE', #672, #10553 ) ;
#65392 = FILL_AREA_STYLE ('',( #6640 ) ) ;
#65393 = ORIENTED_EDGE ( 'NONE', *, *, #50012, .F. ) ;
#65394 = CARTESIAN_POINT ( 'NONE',  ( 211.8476521439973226, 116.6941316755177240, -68.38290356003247439 ) ) ;
#65395 = LINE ( 'NONE', #32344, #36573 ) ;
#65396 = CARTESIAN_POINT ( 'NONE',  ( -72.76696720809547969, 20.16136115364205139, 15.73114799941608588 ) ) ;
#65397 = CARTESIAN_POINT ( 'NONE',  ( -118.6727642982647666, 43.09863379477474865, 62.86749931588654761 ) ) ;
#65398 = CARTESIAN_POINT ( 'NONE',  ( -47.61380558691495679, 12.81230778489788591, 11.95980790945447758 ) ) ;
#65399 = DIRECTION ( 'NONE',  ( 0.000000000000000000, 1.000000000000000000, 0.000000000000000000 ) ) ;
#65400 = LINE ( 'NONE', #66460, #13145 ) ;
#65401 = EDGE_LOOP ( 'NONE', ( #57904, #47098 ) ) ;
#65402 = CARTESIAN_POINT ( 'NONE',  ( 442.3372781065085633, 370.0000000000001137, -146.4497041420116830 ) ) ;
#65403 = CARTESIAN_POINT ( 'NONE',  ( 110.2429982417149574, -170.0000000000000000, -62.76698815611734972 ) ) ;
#65404 = VERTEX_POINT ( 'NONE', #62314 ) ;
#65405 = DIRECTION ( 'NONE',  ( -0.000000000000000000, 1.000000000000000000, -0.000000000000000000 ) ) ;
#65406 = EDGE_LOOP ( 'NONE', ( #62006, #67872, #29911, #46442, #34195, #24442, #32700, #15064, #66601 ) ) ;
#65407 = CARTESIAN_POINT ( 'NONE',  ( -81.23297981660236644, 23.31577157498399089, 44.96949360496901704 ) ) ;
#65408 = CARTESIAN_POINT ( 'NONE',  ( -23.98747857548121942, 9.501432345103358657, -68.67649969425383460 ) ) ;
#65409 = CARTESIAN_POINT ( 'NONE',  ( 45.76405797021008937, 10.34101216371941590, 41.39308771693118416 ) ) ;
#65410 = VECTOR ( 'NONE', #45331, 1000.000000000000000 ) ;
#65411 = CARTESIAN_POINT ( 'NONE',  ( 130.3245512970361233, 39.33195360491887982, -10.04568308804323529 ) ) ;
#65412 = ORIENTED_EDGE ( 'NONE', *, *, #58675, .T. ) ;
#65413 = ORIENTED_EDGE ( 'NONE', *, *, #19891, .T. ) ;
#65414 = CARTESIAN_POINT ( 'NONE',  ( 311.8713128290285113, 190.0000000000000000, 346.5826552340383842 ) ) ;
#65415 = VERTEX_POINT ( 'NONE', #67274 ) ;
#65416 = CARTESIAN_POINT ( 'NONE',  ( 32.38493285958205803, 8.611594965040678673, -18.93455897652550135 ) ) ;
#65417 = CARTESIAN_POINT ( 'NONE',  ( 181.5072453427590347, 79.03352099595184654, 2.464043515047717570 ) ) ;
#65418 = B_SPLINE_CURVE_WITH_KNOTS ( 'NONE', 3,
 ( #1393, #65417, #23900, #66828, #18621, #40076, #22848, #13351, #34810, #62831, #68448, #42400, #41376, #37118, #26225, #42735, #9709, #20945, #57889, #52937, #36789, #14970, #50977, #68774, #15327, #20255, #57550, #20590, #56248, #14631, #46639, #4087, #4763, #36437, #2792, #31502, #42053, #63861, #69117, #53279, #8061, #58230, #10046, #47663 ),
 .UNSPECIFIED., .F., .F.,
 ( 4, 2, 2, 2, 2, 2, 2, 2, 2, 2, 2, 2, 2, 2, 2, 2, 2, 2, 2, 2, 2, 4 ),
 ( 0.02814986980477067122, 0.02995274102020796525, 0.03085417662792662788, 0.03175561223564529051, 0.03355848345108267128, 0.03536135466652005205, 0.03716422588195743282, 0.03896709709739481359, 0.03986853270511350744, 0.04076996831283219436, 0.04167140392055088127, 0.04257283952826957513, 0.04347427513598826898, 0.04437571074370695590, 0.04527714635142565669, 0.04617858195914434360, 0.04798145317458173131, 0.04978432439001910514, 0.05158719560545649285, 0.05339006682089388056, 0.05519293803633126133, 0.05699580925176864904 ),
 .UNSPECIFIED. ) ;
#65419 = CARTESIAN_POINT ( 'NONE',  ( -5.888165822225390755, 7.780336669456523246, 18.02069410080496681 ) ) ;
#65420 = CARTESIAN_POINT ( 'NONE',  ( -1.454841858088672613, 7.566772088227303072, 60.49456332401662451 ) ) ;
#65421 = ADVANCED_FACE ( 'NONE', ( #3571 ), #35935, .F. ) ;
#65422 = SURFACE_SIDE_STYLE ('',( #28838 ) ) ;
#65423 = ORIENTED_EDGE ( 'NONE', *, *, #30249, .T. ) ;
#65424 = EDGE_CURVE ( 'NONE', #42528, #60665, #2890, .T. ) ;
#65425 = CARTESIAN_POINT ( 'NONE',  ( -122.8118341587044995, 44.49743491855738853, -76.11102093153681380 ) ) ;
#65426 = ORIENTED_EDGE ( 'NONE', *, *, #53254, .T. ) ;
#65427 = ORIENTED_EDGE ( 'NONE', *, *, #67681, .T. ) ;
#65428 = DIRECTION ( 'NONE',  ( 0.000000000000000000, -0.04541273895899305968, 0.9989683093773508160 ) ) ;
#65429 = DIRECTION ( 'NONE',  ( 0.000000000000000000, -1.000000000000000000, 0.000000000000000000 ) ) ;
#65430 = CARTESIAN_POINT ( 'NONE',  ( 44.99999999999999289, -22.99999999999998579, 4.000000000000000000 ) ) ;
#65431 = CARTESIAN_POINT ( 'NONE',  ( -128.7359167797845600, 49.61038851545254147, -89.14962691298688924 ) ) ;
#65432 = LINE ( 'NONE', #38699, #31861 ) ;
#65433 = ORIENTED_EDGE ( 'NONE', *, *, #8681, .T. ) ;
#65434 = ADVANCED_FACE ( 'NONE', ( #45090 ), #19753, .T. ) ;
#65435 = DIRECTION ( 'NONE',  ( 0.000000000000000000, 0.000000000000000000, 1.000000000000000000 ) ) ;
#65436 = EDGE_LOOP ( 'NONE', ( #64324, #1925, #503, #28053 ) ) ;
#65437 = B_SPLINE_CURVE_WITH_KNOTS ( 'NONE', 3,
 ( #58044, #16161, #15486, #59067 ),
 .UNSPECIFIED., .F., .F.,
 ( 4, 4 ),
 ( 0.1259919275528359750, 0.1829744153748750768 ),
 .UNSPECIFIED. ) ;
#65438 = CARTESIAN_POINT ( 'NONE',  ( -78.66644367742111399, 22.32174330031316956, 45.41820113967312977 ) ) ;
#65439 = EDGE_LOOP ( 'NONE', ( #40065, #24572, #57578, #2180 ) ) ;
#65440 = CARTESIAN_POINT ( 'NONE',  ( 128.0762755119335452, 38.04197700431935658, -92.41578206806259743 ) ) ;
#65441 = ADVANCED_FACE ( 'NONE', ( #57387 ), #61760, .T. ) ;
#65442 = ADVANCED_FACE ( 'NONE', ( #29272 ), #39823, .F. ) ;
#65443 = AXIS2_PLACEMENT_3D ( 'NONE', #1413, #39398, #23915 ) ;
#65444 = VERTEX_POINT ( 'NONE', #23997 ) ;
#65445 = DIRECTION ( 'NONE',  ( -1.084727855779412860E-16, 2.252460601983934209E-16, 1.000000000000000000 ) ) ;
#65446 = CARTESIAN_POINT ( 'NONE',  ( 89.88695630745282017, 20.55793566325393940, 17.14005976452316560 ) ) ;
#65447 = DIRECTION ( 'NONE',  ( -1.000000000000000000, 0.000000000000000000, 0.000000000000000000 ) ) ;
#65448 = AXIS2_PLACEMENT_3D ( 'NONE', #23862, #8022, #18576 ) ;
#65449 = ORIENTED_EDGE ( 'NONE', *, *, #1558, .T. ) ;
#65450 = FACE_OUTER_BOUND ( 'NONE', #28905, .T. ) ;
#65451 = VECTOR ( 'NONE', #44561, 1000.000000000000000 ) ;
#65452 = CARTESIAN_POINT ( 'NONE',  ( -15.55634918610411077, -41.66904755831209428, 2.000000000000001776 ) ) ;
#65453 = CARTESIAN_POINT ( 'NONE',  ( 31.90170717962883984, 8.563261373066637816, 37.65398698468158756 ) ) ;
#65454 = CARTESIAN_POINT ( 'NONE',  ( -173.9526029538035914, 89.57590038685107459, -49.67757543776112072 ) ) ;
#65455 = CARTESIAN_POINT ( 'NONE',  ( -126.8005235842505840, 47.09307471149450919, -8.110568341272605508 ) ) ;
#65456 = CIRCLE ( 'NONE', #10563, 5.000000000000170530 ) ;
#65457 = DIRECTION ( 'NONE',  ( 0.000000000000000000, 0.000000000000000000, 1.000000000000000000 ) ) ;
#65458 = DIRECTION ( 'NONE',  ( -1.000000000000000000, 0.000000000000000000, 0.000000000000000000 ) ) ;
#65459 = EDGE_LOOP ( 'NONE', ( #31386, #52461, #2997, #37685 ) ) ;
#65460 = CARTESIAN_POINT ( 'NONE',  ( 140.9141742510256563, 47.05414327990548884, -72.95852137335218401 ) ) ;
#65461 = LINE ( 'NONE', #38725, #27624 ) ;
#65462 = ORIENTED_EDGE ( 'NONE', *, *, #44188, .F. ) ;
#65463 = AXIS2_PLACEMENT_3D ( 'NONE', #6101, #32843, #54987 ) ;
#65464 = FACE_BOUND ( 'NONE', #53752, .T. ) ;
#65465 = CARTESIAN_POINT ( 'NONE',  ( -3.868882431147339318, 6.665575841812209745, -76.13890115071046694 ) ) ;
#65466 = SURFACE_SIDE_STYLE ('',( #54182 ) ) ;
#65467 = CARTESIAN_POINT ( 'NONE',  ( -144.2155061717026285, 61.10843690942980544, -10.14790075599239216 ) ) ;
#65468 = CARTESIAN_POINT ( 'NONE',  ( 43.69793103685474023, 27.56441319423685243, 26.66469066592269499 ) ) ;
#65469 = CARTESIAN_POINT ( 'NONE',  ( -0.3255842968951683236, 7.525381170773409067, 38.10786089665049303 ) ) ;
#65470 = CARTESIAN_POINT ( 'NONE',  ( -858.3301948030079984, -622.0000000000060254, 10.00000000000000000 ) ) ;
#65471 = ADVANCED_FACE ( 'NONE', ( #45443, #14131, #29967 ), #29608, .F. ) ;
#65472 = CARTESIAN_POINT ( 'NONE',  ( 110.3268469170084245, 21.42428528562853174, -5.000000000000004441 ) ) ;
#65473 = DIRECTION ( 'NONE',  ( -0.000000000000000000, -0.000000000000000000, -1.000000000000000000 ) ) ;
#65474 = CARTESIAN_POINT ( 'NONE',  ( -14.56151485655250433, 8.434196591921335084, 34.28149470285157463 ) ) ;
#65475 = CARTESIAN_POINT ( 'NONE',  ( 161.7209903610255139, 61.03262545641849357, 16.26150805458010495 ) ) ;
#65476 = CARTESIAN_POINT ( 'NONE',  ( 93.32756701508618846, 22.89083686918419502, -13.06632485724244397 ) ) ;
#65477 = ORIENTED_EDGE ( 'NONE', *, *, #59054, .F. ) ;
#65478 = DIRECTION ( 'NONE',  ( 1.000000000000000000, 0.000000000000000000, 0.000000000000000000 ) ) ;
#65479 = ORIENTED_EDGE ( 'NONE', *, *, #30519, .T. ) ;
#65480 = DIRECTION ( 'NONE',  ( -0.000000000000000000, -0.000000000000000000, 1.000000000000000000 ) ) ;
#65481 = LINE ( 'NONE', #23273, #46706 ) ;
#65482 = CARTESIAN_POINT ( 'NONE',  ( 103.4246886032334061, 26.94746784261150552, 87.65654458658119097 ) ) ;
#65483 = FACE_OUTER_BOUND ( 'NONE', #46835, .T. ) ;
#65484 = CARTESIAN_POINT ( 'NONE',  ( 67.92995549349549833, 13.86623459444476225, -22.06271008403504652 ) ) ;
#65485 = CARTESIAN_POINT ( 'NONE',  ( -29.51272929882556539, 10.30144624948893828, -35.56467666911228065 ) ) ;
#65486 = DIRECTION ( 'NONE',  ( -0.000000000000000000, 0.000000000000000000, -1.000000000000000000 ) ) ;
#65487 = FACE_OUTER_BOUND ( 'NONE', #31582, .T. ) ;
#65488 = CARTESIAN_POINT ( 'NONE',  ( -118.6727642982647666, 43.09863379477475576, -17.66615245550452329 ) ) ;
#65489 = EDGE_LOOP ( 'NONE', ( #64896, #63837 ) ) ;
#65490 = ORIENTED_EDGE ( 'NONE', *, *, #68652, .F. ) ;
#65491 = CARTESIAN_POINT ( 'NONE',  ( 38.90907126433564400, 9.359889524363181224, 71.75838489642698903 ) ) ;
#65492 = CARTESIAN_POINT ( 'NONE',  ( 173.8575673535406452, 71.59843387604337295, 61.62534631081166481 ) ) ;
#65493 = DIRECTION ( 'NONE',  ( -0.000000000000000000, -0.000000000000000000, 1.000000000000000000 ) ) ;
#65494 = CARTESIAN_POINT ( 'NONE',  ( -37.03736084664572559, -19.22364826157912177, 13.79046412329102544 ) ) ;
#65495 = MECHANICAL_DESIGN_GEOMETRIC_PRESENTATION_REPRESENTATION (  '', ( #40936 ), #65648 ) ;
#65496 = DIRECTION ( 'NONE',  ( 0.000000000000000000, 0.000000000000000000, -1.000000000000000000 ) ) ;
#65497 = CARTESIAN_POINT ( 'NONE',  ( 46.66904755831207297, -10.55634918610412853, 2.000000000000001776 ) ) ;
#65498 = VERTEX_POINT ( 'NONE', #19402 ) ;
#65499 = CARTESIAN_POINT ( 'NONE',  ( 94.14197848494937659, 23.19876128416617789, 10.37775773208338492 ) ) ;
#65500 = CARTESIAN_POINT ( 'NONE',  ( 187.0788993276712233, 86.37277723143235164, -21.39429512477833129 ) ) ;
#65501 = CARTESIAN_POINT ( 'NONE',  ( 13.84704553156521811, 7.452804552247568992, 57.11067823459568160 ) ) ;
#65502 = VECTOR ( 'NONE', #30870, 1000.000000000000000 ) ;
#65503 = LINE ( 'NONE', #48590, #360 ) ;
#65504 = CARTESIAN_POINT ( 'NONE',  ( 39.40195752203892710, 8.409560354027385998, -8.775266874964067654 ) ) ;
#65505 = CARTESIAN_POINT ( 'NONE',  ( -49.77357484059193382, 41.82599373102802787, 41.38025477438755928 ) ) ;
#65506 = FACE_BOUND ( 'NONE', #3655, .T. ) ;
#65507 = CARTESIAN_POINT ( 'NONE',  ( -57.43251939610648549, 15.33203492375495181, -49.84526837728627413 ) ) ;
#65508 = EDGE_CURVE ( 'NONE', #23473, #24241, #24353, .T. ) ;
#65509 = AXIS2_PLACEMENT_3D ( 'NONE', #35758, #52267, #13945 ) ;
#65510 = EDGE_CURVE ( 'NONE', #38709, #39038, #46133, .T. ) ;
#65511 = AXIS2_PLACEMENT_3D ( 'NONE', #1894, #36956, #37283 ) ;
#65512 = EDGE_LOOP ( 'NONE', ( #61418, #28822, #8056, #33189 ) ) ;
#65513 = CARTESIAN_POINT ( 'NONE',  ( 6.375108774214766072E-14, 31.11269837220806167, 0.000000000000000000 ) ) ;
#65514 = CARTESIAN_POINT ( 'NONE',  ( 93.08174259058944244, 22.79847752828720786, -39.46674160480419857 ) ) ;
#65515 = ADVANCED_FACE ( 'NONE', ( #57050 ), #8864, .T. ) ;
#65516 = AXIS2_PLACEMENT_3D ( 'NONE', #42712, #37432, #499 ) ;
#65517 = CARTESIAN_POINT ( 'NONE',  ( -50.53243683205840853, 14.55237037207939643, 70.66630208468741614 ) ) ;
#65518 = DIRECTION ( 'NONE',  ( -0.000000000000000000, -0.000000000000000000, -1.000000000000000000 ) ) ;
#65519 = CARTESIAN_POINT ( 'NONE',  ( 208.9585401441655392, 114.1617785893844115, 69.74089473411397933 ) ) ;
#65520 = DIRECTION ( 'NONE',  ( 0.000000000000000000, -0.000000000000000000, 1.000000000000000000 ) ) ;
#65521 = ORIENTED_EDGE ( 'NONE', *, *, #21196, .T. ) ;
#65522 = CARTESIAN_POINT ( 'NONE',  ( 56.66775172211442424, 11.28938863449062069, 14.47032970562600696 ) ) ;
#65523 = CARTESIAN_POINT ( 'NONE',  ( -452.6627218934913799, 399.9999999999953957, 113.5502958579925803 ) ) ;
#65524 = VERTEX_POINT ( 'NONE', #28934 ) ;
#65525 = ORIENTED_EDGE ( 'NONE', *, *, #68082, .F. ) ;
#65526 = CARTESIAN_POINT ( 'NONE',  ( 56.48035995027147749, -49.34540444547771187, 43.58025477438756212 ) ) ;
#65527 = CARTESIAN_POINT ( 'NONE',  ( 116.4569059613810680, 32.98885890446639735, 94.99999999999866418 ) ) ;
#65528 = CARTESIAN_POINT ( 'NONE',  ( 109.3079614081140676, 28.45126415661783525, 44.56732555389881867 ) ) ;
#65529 = EDGE_CURVE ( 'NONE', #31812, #52659, #23651, .T. ) ;
#65530 = ORIENTED_EDGE ( 'NONE', *, *, #32383, .F. ) ;
#65531 = EDGE_CURVE ( 'NONE', #3625, #39103, #63009, .T. ) ;
#65532 = EDGE_CURVE ( 'NONE', #21613, #9937, #983, .T. ) ;
#65533 = ORIENTED_EDGE ( 'NONE', *, *, #46190, .T. ) ;
#65534 = CARTESIAN_POINT ( 'NONE',  ( 39.40195752203891999, 8.409560354027407314, -35.61981746542776506 ) ) ;
#65535 = CARTESIAN_POINT ( 'NONE',  ( 162.0812592823605200, 62.62783216273700049, 42.84411675552712495 ) ) ;
#65536 = CARTESIAN_POINT ( 'NONE',  ( 103.9685899589048148, 27.18106603025991674, 6.150318247617813761 ) ) ;
#65537 = CARTESIAN_POINT ( 'NONE',  ( 65.62985354949977079, 14.32996029952554373, 17.50227395258704277 ) ) ;
#65538 = CARTESIAN_POINT ( 'NONE',  ( 7.347286611336963702, 4.995646404165275278, -9.003039949738251835 ) ) ;
#65539 = CARTESIAN_POINT ( 'NONE',  ( 107.9213359589208920, 28.92595015506874745, -9.430594635280971971 ) ) ;
#65540 = CARTESIAN_POINT ( 'NONE',  ( 61.08522853873727598, 13.26388801693371811, -35.95693286015492163 ) ) ;
#65541 = CARTESIAN_POINT ( 'NONE',  ( -7.825402957745085430, 7.899365992529253866, -89.10717191287116634 ) ) ;
#65542 = CARTESIAN_POINT ( 'NONE',  ( -151.1225012833390338, 66.89247819254583760, -88.66664194563858814 ) ) ;
#65543 = CARTESIAN_POINT ( 'NONE',  ( -173.1211646369891071, 88.63826465341152527, 18.97714401617737323 ) ) ;
#65544 = CARTESIAN_POINT ( 'NONE',  ( 93.82901523493131890, 22.00453947897597828, 88.77271230041061756 ) ) ;
#65546 = ORIENTED_EDGE ( 'NONE', *, *, #2654, .F. ) ;
#65545 = DIRECTION ( 'NONE',  ( 1.000000000000000000, 0.000000000000000000, -1.734723475976805517E-15 ) ) ;
#65547 = ORIENTED_EDGE ( 'NONE', *, *, #6364, .F. ) ;
#65548 = STYLED_ITEM ( 'NONE', ( #27741 ), #39903 ) ;
#65549 = VERTEX_POINT ( 'NONE', #27701 ) ;
#65550 = AXIS2_PLACEMENT_3D ( 'NONE', #2340, #2001, #12196 ) ;
#65551 = FACE_OUTER_BOUND ( 'NONE', #52641, .T. ) ;
#65552 = CARTESIAN_POINT ( 'NONE',  ( -47.80896875121165834, 12.85816703949531359, 39.77673797478080076 ) ) ;
#65553 = DIRECTION ( 'NONE',  ( -0.000000000000000000, 1.000000000000000000, -0.000000000000000000 ) ) ;
#65554 = DIRECTION ( 'NONE',  ( -0.000000000000000000, 0.000000000000000000, -1.000000000000000000 ) ) ;
#65555 = VECTOR ( 'NONE', #41514, 1000.000000000000114 ) ;
#65556 = CARTESIAN_POINT ( 'NONE',  ( -58.75378739419586793, 16.75118858561006618, -49.25797758003430005 ) ) ;
#65557 = AXIS2_PLACEMENT_3D ( 'NONE', #54676, #60660, #65601 ) ;
#65558 = FACE_OUTER_BOUND ( 'NONE', #38707, .T. ) ;
#65559 = CARTESIAN_POINT ( 'NONE',  ( -71.67841390531691559, 19.78168466957078664, -72.19491188520656522 ) ) ;
#65560 = CARTESIAN_POINT ( 'NONE',  ( 7.705764017935865517, 66.19838207530922602, 34.48241823979987686 ) ) ;
#65561 = ORIENTED_EDGE ( 'NONE', *, *, #36767, .F. ) ;
#65562 = CONICAL_SURFACE ( 'NONE', #22873, 65.00000000000000000, 0.7853981633974497223 ) ;
#65563 = DIRECTION ( 'NONE',  ( 0.000000000000000000, 0.000000000000000000, 1.000000000000000000 ) ) ;
#65564 = VERTEX_POINT ( 'NONE', #59700 ) ;
#65565 = VERTEX_POINT ( 'NONE', #38612 ) ;
#65566 = CARTESIAN_POINT ( 'NONE',  ( -143.7133518487517279, 60.70463114991427034, 16.14514466890094724 ) ) ;
#65567 = CARTESIAN_POINT ( 'NONE',  ( -61.90435325615973738, 17.67681010539238429, -93.32376335434845771 ) ) ;
#65568 = CIRCLE ( 'NONE', #423, 5.000000000000004441 ) ;
#65569 = DIRECTION ( 'NONE',  ( 2.220446049250313081E-16, -0.000000000000000000, 1.000000000000000000 ) ) ;
#65570 = CARTESIAN_POINT ( 'NONE',  ( -102.2801239173131052, 32.78103895658057354, -50.01457726497594081 ) ) ;
#65571 = DIRECTION ( 'NONE',  ( -0.9909497617679331460, -0.1342332658176667304, 0.000000000000000000 ) ) ;
#65572 = CARTESIAN_POINT ( 'NONE',  ( 8.904582680624310242, -23.36040254969760355, 0.000000000000000000 ) ) ;
#65573 = CARTESIAN_POINT ( 'NONE',  ( 137.6104751318277124, 44.92718313329110202, -23.17606804121535902 ) ) ;
#65574 = ORIENTED_EDGE ( 'NONE', *, *, #57350, .T. ) ;
#65575 = ORIENTED_EDGE ( 'NONE', *, *, #12015, .F. ) ;
#65576 = ORIENTED_EDGE ( 'NONE', *, *, #18428, .T. ) ;
#65577 = B_SPLINE_CURVE_WITH_KNOTS ( 'NONE', 3,
 ( #30185, #35808, #62883, #51298, #46007, #19268, #67819, #41080, #14353, #57260, #30877, #51974, #14684, #68502, #3789, #25259, #46694, #68172, #4143, #37174, #10436, #26285, #47720, #58969, #48391, #42113, #59653, #21684, #64256, #54377, #10783, #27655, #64958, #227, #52995, #32257, #31907, #53337, #16413, #42787, #69181, #21009, #58621, #16754, #42454, #4816, #26964, #53690, #38215, #43134 ),
 .UNSPECIFIED., .F., .F.,
 ( 4, 2, 2, 2, 2, 2, 2, 2, 2, 2, 2, 2, 2, 2, 2, 2, 2, 2, 2, 2, 2, 2, 2, 2, 4 ),
 ( 0.03126542424884323768, 0.03330676804260256085, 0.03534811183636187709, 0.03738945563012119333, 0.03943079942388051651, 0.04045147132076019197, 0.04147214321763986744, 0.04249281511451954291, 0.04351348701139921837, 0.04555483080515859706, 0.04657550270203830028, 0.04759617459891800351, 0.04810651054735787940, 0.04861684649579775530, 0.04963751839267750710, 0.05065819028955724501, 0.05167886218643699681, 0.05269953408331674166, 0.05372020598019648652, 0.05474087787707623831, 0.05576154977395598317, 0.05780289356771556308, 0.05984423736147514994, 0.06188558115523473679, 0.06392692494899432365 ),
 .UNSPECIFIED. ) ;
#65578 = DIRECTION ( 'NONE',  ( 1.000000000000000000, 0.000000000000000000, 0.000000000000000000 ) ) ;
#65579 = CARTESIAN_POINT ( 'NONE',  ( -156.6862310659956279, 71.88416263379569671, -13.22470838037755492 ) ) ;
#65580 = DIRECTION ( 'NONE',  ( -1.020422603260505347E-14, 1.000000000000000000, 5.551115123125782702E-17 ) ) ;
#65581 = CARTESIAN_POINT ( 'NONE',  ( 55.52750043885183828, 11.05966813607792609, -16.86601971481237072 ) ) ;
#65582 =( REPRESENTATION_RELATIONSHIP ('NONE','NONE', #40274, #22184 ) REPRESENTATION_RELATIONSHIP_WITH_TRANSFORMATION ( #30696 )SHAPE_REPRESENTATION_RELATIONSHIP( ) );
#65583 = UNCERTAINTY_MEASURE_WITH_UNIT (LENGTH_MEASURE( 1.000000000000000082E-05 ), #3143, 'distance_accuracy_value', 'NONE');
#65584 = CARTESIAN_POINT ( 'NONE',  ( -49.45858366215605173, 13.25262207532077952, 32.81574071421050576 ) ) ;
#65585 = CARTESIAN_POINT ( 'NONE',  ( 290.0000000000000568, 5.000000000000000888, 18.50000000000000000 ) ) ;
#65586 = ORIENTED_EDGE ( 'NONE', *, *, #21898, .T. ) ;
#65587 = CARTESIAN_POINT ( 'NONE',  ( -65.00200000000002376, -1.250000000000021760, 43.58025477438756923 ) ) ;
#65588 = CARTESIAN_POINT ( 'NONE',  ( -151.2497169612549044, 65.66843968092749151, 72.41451540298392331 ) ) ;
#65589 = CARTESIAN_POINT ( 'NONE',  ( -6.840165690716690783, 7.836465889224641046, -50.36917416540237724 ) ) ;
#65590 = CARTESIAN_POINT ( 'NONE',  ( 61.91366885787816443, -28.42865614898931881, 170.0000000000000000 ) ) ;
#65591 = CARTESIAN_POINT ( 'NONE',  ( -172.7402246477008703, 86.70495794627620967, -88.40105834567735599 ) ) ;
#65592 = CARTESIAN_POINT ( 'NONE',  ( 55.14772863908675049, -34.40534879854660488, 170.0000000000000000 ) ) ;
#65593 = FACE_BOUND ( 'NONE', #7677, .T. ) ;
#65594 = CARTESIAN_POINT ( 'NONE',  ( -190.6985136298601731, 109.1272424661242582, 87.66052266422059347 ) ) ;
#65595 = EDGE_CURVE ( 'NONE', #60812, #17861, #22432, .T. ) ;
#65596 = VECTOR ( 'NONE', #35250, 1000.000000000000000 ) ;
#65597 = EDGE_CURVE ( 'NONE', #1913, #59098, #47500, .T. ) ;
#65598 = ORIENTED_EDGE ( 'NONE', *, *, #32385, .F. ) ;
#65599 = CARTESIAN_POINT ( 'NONE',  ( -25.99999999999994671, 0.000000000000000000, -104.9999999999999858 ) ) ;
#65600 = EDGE_CURVE ( 'NONE', #28345, #48432, #30658, .T. ) ;
#65601 = DIRECTION ( 'NONE',  ( -1.000000000000000000, 0.000000000000000000, 0.000000000000000000 ) ) ;
#65602 = CARTESIAN_POINT ( 'NONE',  ( -31.11269837220812207, -31.11269837220801193, 2.000000000000001776 ) ) ;
#65603 = CARTESIAN_POINT ( 'NONE',  ( 43.97326221476411945, 9.047815246749999929, -63.99822409915773136 ) ) ;
#65604 = DIRECTION ( 'NONE',  ( -0.000000000000000000, -0.000000000000000000, -1.000000000000000000 ) ) ;
#65605 = ORIENTED_EDGE ( 'NONE', *, *, #47650, .F. ) ;
#65606 = VECTOR ( 'NONE', #23099, 1000.000000000000227 ) ;
#65607 = B_SPLINE_CURVE_WITH_KNOTS ( 'NONE', 3,
 ( #39423, #55601, #11998, #66526, #60874, #7430, #1445, #6371, #22548, #28882, #33472, #50334, #50670, #13057, #45043, #23945, #7772, #29222, #45394, #18672, #61581, #65469, #54894, #30959, #45746, #52061, #30267, #62263, #56997, #67903, #52405, #46425, #8111, #68249, #61907, #24649, #14082, #13731, #56291, #57341, #24994, #15118, #19353 ),
 .UNSPECIFIED., .F., .F.,
 ( 4, 2, 2, 2, 2, 2, 2, 2, 1, 2, 2, 2, 2, 2, 2, 2, 2, 2, 2, 2, 2, 4 ),
 ( 0.000000000000000000, 0.001466540241398137275, 0.002199810362097205912, 0.002933080482796274549, 0.004399620724194417895, 0.005866160965592561241, 0.007332701206990704587, 0.008065971327689776260, 0.008799241448388847933, 0.009532511569087917871, 0.01026578168978698954, 0.01173232193118513289, 0.01319886217258327450, 0.01466540241398141785, 0.01539867253468047911, 0.01613194265537953864, 0.01759848289677766464, 0.01906502313817578717, 0.01979829325887484670, 0.02053156337957390970, 0.02199810362097203223, 0.02346464386237015476 ),
 .UNSPECIFIED. ) ;
#65608 = ORIENTED_EDGE ( 'NONE', *, *, #35967, .F. ) ;
#65609 = VECTOR ( 'NONE', #25789, 1000.000000000000227 ) ;
#65610 = CARTESIAN_POINT ( 'NONE',  ( -132.1053471785562863, 50.72188866504426130, -91.87369984681103574 ) ) ;
#65611 = CIRCLE ( 'NONE', #35277, 89.99999999999997158 ) ;
#65612 = DIRECTION ( 'NONE',  ( 1.000000000000000000, 0.000000000000000000, 0.000000000000000000 ) ) ;
#65613 = EDGE_LOOP ( 'NONE', ( #3530, #56215, #37125, #47145 ) ) ;
#65614 = EDGE_LOOP ( 'NONE', ( #12109, #1824 ) ) ;
#65615 = CIRCLE ( 'NONE', #22929, 65.36598343705435354 ) ;
#65616 = CARTESIAN_POINT ( 'NONE',  ( -15.55634918610396866, 36.11269837220808654, 85.00100000000000477 ) ) ;
#65617 = CARTESIAN_POINT ( 'NONE',  ( 133.8566784816069060, 42.60093787723653236, -24.17876034193199786 ) ) ;
#65618 = EDGE_CURVE ( 'NONE', #2392, #26538, #11515, .T. ) ;
#65619 = ORIENTED_EDGE ( 'NONE', *, *, #24554, .T. ) ;
#65620 = DIRECTION ( 'NONE',  ( 0.000000000000000000, 0.000000000000000000, 1.000000000000000000 ) ) ;
#65621 = CARTESIAN_POINT ( 'NONE',  ( 136.9654665832768217, 44.52067472585214603, 70.68427344918816857 ) ) ;
#65622 = CARTESIAN_POINT ( 'NONE',  ( -71.17819443284078318, 19.60909329639483190, -42.12447784558203523 ) ) ;
#65623 = AXIS2_PLACEMENT_3D ( 'NONE', #1835, #22231, #28196 ) ;
#65624 = PLANE ( 'NONE',  #6625 ) ;
#65625 = CYLINDRICAL_SURFACE ( 'NONE', #29399, 7.500000000000013323 ) ;
#65626 = CARTESIAN_POINT ( 'NONE',  ( -51.77431913897919458, 14.86466849149170777, -9.108735933062128254 ) ) ;
#65627 = ORIENTED_EDGE ( 'NONE', *, *, #14292, .F. ) ;
#65628 = CARTESIAN_POINT ( 'NONE',  ( -124.1033713525885958, 45.32626312604504193, -8.282396413194451412 ) ) ;
#65629 = FACE_BOUND ( 'NONE', #7751, .T. ) ;
#65630 = DIRECTION ( 'NONE',  ( -0.1342332658176522420, -0.9909497617679351444, 0.000000000000000000 ) ) ;
#65631 = CARTESIAN_POINT ( 'NONE',  ( -168.1811549361196967, 83.25427431521136157, -74.70477187311568912 ) ) ;
#65633 = VERTEX_POINT ( 'NONE', #20782 ) ;
#65632 = CARTESIAN_POINT ( 'NONE',  ( -128.9955982454845866, 48.57000285068010470, 84.97439690926448463 ) ) ;
#65634 = CARTESIAN_POINT ( 'NONE',  ( 55.91494169499919309, 12.16343363043255721, 12.89567247696315988 ) ) ;
#65635 = ORIENTED_EDGE ( 'NONE', *, *, #48500, .F. ) ;
#65636 = CARTESIAN_POINT ( 'NONE',  ( -132.0958200534848004, 50.71531800824803327, 33.89524248677182783 ) ) ;
#65637 = CYLINDRICAL_SURFACE ( 'NONE', #47952, 2.999999999999999112 ) ;
#65638 = DIRECTION ( 'NONE',  ( 0.7071067811865476838, -5.551115123125782086E-17, 0.7071067811865473507 ) ) ;
#65639 = CARTESIAN_POINT ( 'NONE',  ( 90.51709546286275554, 21.85407654229979713, 30.79386894197559599 ) ) ;
#65640 = CARTESIAN_POINT ( 'NONE',  ( -447.6627218934914367, 389.9999999999954525, 108.5502958579925235 ) ) ;
#65641 = CARTESIAN_POINT ( 'NONE',  ( -78.66644367742109978, 23.39876645725288640, -23.27090004125422595 ) ) ;
#65642 = CARTESIAN_POINT ( 'NONE',  ( 90.91465859190773813, 20.92790537681859675, -76.32607979879988136 ) ) ;
#65643 = CIRCLE ( 'NONE', #20692, 35.00000000000000000 ) ;
#65644 = CARTESIAN_POINT ( 'NONE',  ( -46.45214378727172999, -35.29454295034832256, 27.58472369410210234 ) ) ;
#65645 = DIRECTION ( 'NONE',  ( 0.000000000000000000, 0.000000000000000000, 1.000000000000000000 ) ) ;
#65646 = EDGE_LOOP ( 'NONE', ( #8702, #44458, #16685, #14997 ) ) ;
#65647 = ORIENTED_EDGE ( 'NONE', *, *, #14825, .T. ) ;
#65648 =( GEOMETRIC_REPRESENTATION_CONTEXT ( 3 ) GLOBAL_UNCERTAINTY_ASSIGNED_CONTEXT ( ( #36693 ) ) GLOBAL_UNIT_ASSIGNED_CONTEXT ( ( #37192, #26309, #10119 ) ) REPRESENTATION_CONTEXT ( 'NONE', 'WORKASPACE' ) );
#65649 = CARTESIAN_POINT ( 'NONE',  ( -72.29721455218913206, 19.95276341750015803, 43.58025477438756212 ) ) ;
#65650 = DIRECTION ( 'NONE',  ( 8.784520486428009340E-17, -2.340627113153416505E-16, 1.000000000000000000 ) ) ;
#65651 = CYLINDRICAL_SURFACE ( 'NONE', #57027, 7.500000000000020428 ) ;
#65652 = DIRECTION ( 'NONE',  ( 0.000000000000000000, 0.000000000000000000, 1.000000000000000000 ) ) ;
#65653 = VECTOR ( 'NONE', #28462, 1000.000000000000000 ) ;
#65654 = CARTESIAN_POINT ( 'NONE',  ( 208.0306608271317828, 112.7988899307265740, -50.54803444713732574 ) ) ;
#65655 = EDGE_CURVE ( 'NONE', #31358, #33561, #49143, .T. ) ;
#65656 = DIRECTION ( 'NONE',  ( -0.5508969814520944253, -0.8345732537213078617, 0.000000000000000000 ) ) ;
#65657 = CARTESIAN_POINT ( 'NONE',  ( -103.2169245450825485, 33.25885825286820818, 57.40773309695661197 ) ) ;
#65658 = VECTOR ( 'NONE', #9169, 1000.000000000000000 ) ;
#65659 = CARTESIAN_POINT ( 'NONE',  ( -24.18258876560172865, 8.512344710720686436, -44.77552165097223025 ) ) ;
#65660 = FACE_OUTER_BOUND ( 'NONE', #65614, .T. ) ;
#65661 = VERTEX_POINT ( 'NONE', #43526 ) ;
#65663 = CARTESIAN_POINT ( 'NONE',  ( -24.71645982722741408, 9.599558729461493911, 14.20614957612933082 ) ) ;
#65662 = VECTOR ( 'NONE', #24187, 1000.000000000000000 ) ;
#65664 = VERTEX_POINT ( 'NONE', #47166 ) ;
#65665 = ADVANCED_FACE ( 'NONE', ( #26416 ), #57736, .T. ) ;
#65666 = CARTESIAN_POINT ( 'NONE',  ( -8.314575874103555364, 6.922894809783096903, -50.41807073194386390 ) ) ;
#65667 = AXIS2_PLACEMENT_3D ( 'NONE', #31190, #43097, #31866 ) ;
#65668 = CARTESIAN_POINT ( 'NONE',  ( -84.22570405563703844, 24.51726571826275602, 69.82089765687976524 ) ) ;
#65669 = CARTESIAN_POINT ( 'NONE',  ( 126.3580464630938422, 38.22944795020833197, 36.70972463671400732 ) ) ;
#65670 = CARTESIAN_POINT ( 'NONE',  ( 38.90907126433565821, 9.359889524363181224, 18.06928371549960133 ) ) ;
#65671 = DIRECTION ( 'NONE',  ( 1.000000000000000000, 0.000000000000000000, 0.000000000000000000 ) ) ;
#65672 = CARTESIAN_POINT ( 'NONE',  ( 117.4396227366912626, 33.48307633470226818, -95.00000000000133582 ) ) ;
#65673 = CARTESIAN_POINT ( 'NONE',  ( 0.000000000000000000, 0.000000000000000000, 43.58025477438756212 ) ) ;
#65674 = CARTESIAN_POINT ( 'NONE',  ( 211.3822731854152721, 115.9841935232942376, 93.81720800102199576 ) ) ;
#65675 = LINE ( 'NONE', #23802, #16225 ) ;
#65676 = ORIENTED_EDGE ( 'NONE', *, *, #51091, .T. ) ;
#65677 = CARTESIAN_POINT ( 'NONE',  ( 55.56634333706183071, 12.09342294753930069, 63.15602334383434169 ) ) ;
#65678 = CARTESIAN_POINT ( 'NONE',  ( 11.81843724556921238, 7.412394300769734379, -63.49552996665384796 ) ) ;
#65679 = CARTESIAN_POINT ( 'NONE',  ( -190.3061188229048639, 108.5745819235681751, -38.23057545279792890 ) ) ;
#65680 = EDGE_CURVE ( 'NONE', #4867, #23369, #15167, .T. ) ;
#65681 = CARTESIAN_POINT ( 'NONE',  ( 281.2988829979104821, -21.46124357533057747, -4.839350883597167474 ) ) ;
#65682 = LINE ( 'NONE', #49825, #12010 ) ;
#65683 = ADVANCED_FACE ( 'NONE', ( #58080 ), #32985, .F. ) ;
#65684 = CARTESIAN_POINT ( 'NONE',  ( 94.11387023963305865, 23.18808022568910943, 91.49174497375973658 ) ) ;
#65685 = VERTEX_POINT ( 'NONE', #54418 ) ;
#65686 = DIRECTION ( 'NONE',  ( 0.000000000000000000, 0.000000000000000000, 1.000000000000000000 ) ) ;
#65687 = ADVANCED_FACE ( 'NONE', ( #52454 ), #48278, .T. ) ;
#65688 = CARTESIAN_POINT ( 'NONE',  ( -189.2352924136013712, 107.0839554967701019, -15.71323334688268858 ) ) ;
#65689 = CARTESIAN_POINT ( 'NONE',  ( -131.6133495896316958, 50.37677745548733554, 16.13319187600255589 ) ) ;
#65690 = CARTESIAN_POINT ( 'NONE',  ( -165.9154624515710168, 80.89088623112733956, -40.11032779023376094 ) ) ;
#65691 = CONTEXT_DEPENDENT_SHAPE_REPRESENTATION ( #1795, #49505 ) ;
#65692 = CARTESIAN_POINT ( 'NONE',  ( -167.3151846658799968, 80.89015936597813550, 87.25299558331532523 ) ) ;
#65693 = ORIENTED_EDGE ( 'NONE', *, *, #29612, .F. ) ;
#65694 = DIRECTION ( 'NONE',  ( 1.697742017499683849E-16, -1.665334536937734564E-16, 1.000000000000000000 ) ) ;
#65695 = CARTESIAN_POINT ( 'NONE',  ( -7.330690860789851548, 6.858814156830896458, -8.573520141480127421 ) ) ;
#65696 = CARTESIAN_POINT ( 'NONE',  ( -145.3279998500303236, 60.71393190715789956, -21.70027410468134121 ) ) ;
#65697 = CARTESIAN_POINT ( 'NONE',  ( -5.183193881612059073, 7.740932022135016410, -62.73915333014450368 ) ) ;
#65698 = AXIS2_PLACEMENT_3D ( 'NONE', #57168, #9319, #41337 ) ;
#65699 = LINE ( 'NONE', #60047, #13371 ) ;
#65700 = ADVANCED_FACE ( 'NONE', ( #9896 ), #53122, .T. ) ;
#65701 = VERTEX_POINT ( 'NONE', #26071 ) ;
#65702 = CARTESIAN_POINT ( 'NONE',  ( -60.47589866267034608, 17.25153113855766662, 5.786362127798294175 ) ) ;
#65703 = CARTESIAN_POINT ( 'NONE',  ( 203.9276061909314706, 105.2889220654479061, -51.32593103262161094 ) ) ;
#65704 = DIRECTION ( 'NONE',  ( 1.000000000000000000, 1.748373411921809651E-16, 2.371692252312040348E-20 ) ) ;
#65705 = EDGE_CURVE ( 'NONE', #36843, #34467, #25735, .T. ) ;
#65706 = EDGE_CURVE ( 'NONE', #67714, #15124, #26958, .T. ) ;
#65707 = CARTESIAN_POINT ( 'NONE',  ( 22.89634831467702369, 6.832298124325687283, -40.61357525750717201 ) ) ;
#65708 = VECTOR ( 'NONE', #40579, 1000.000000000000000 ) ;
#65710 = ORIENTED_EDGE ( 'NONE', *, *, #37079, .T. ) ;
#65709 = CARTESIAN_POINT ( 'NONE',  ( 116.6436511186860372, 33.08230081168869674, 14.18392456913904098 ) ) ;
#65711 = CIRCLE ( 'NONE', #47698, 5.000000000000004441 ) ;
#65712 = CARTESIAN_POINT ( 'NONE',  ( 80.34841469379381351, 18.42674688750400946, 94.99999999999866418 ) ) ;
#65713 = AXIS2_PLACEMENT_3D ( 'NONE', #7366, #44983, #66464 ) ;
#65714 = ORIENTED_EDGE ( 'NONE', *, *, #58454, .F. ) ;
#65715 = VERTEX_POINT ( 'NONE', #4954 ) ;
#65716 = DIRECTION ( 'NONE',  ( 0.000000000000000000, -0.000000000000000000, -1.000000000000000000 ) ) ;
#65717 = AXIS2_PLACEMENT_3D ( 'NONE', #15444, #36895, #5222 ) ;
#65718 = CARTESIAN_POINT ( 'NONE',  ( -149.5074843970971301, -170.0000000000000000, -96.00193171241933499 ) ) ;
#65720 = ORIENTED_EDGE ( 'NONE', *, *, #36455, .T. ) ;
#65719 = DIRECTION ( 'NONE',  ( 0.000000000000000000, 0.000000000000000000, 1.000000000000000000 ) ) ;
#65721 = DIRECTION ( 'NONE',  ( -1.000000000000000000, -0.000000000000000000, -0.000000000000000000 ) ) ;
#65722 = DIRECTION ( 'NONE',  ( -0.8118923937861950435, -0.5838071093367415143, 0.000000000000000000 ) ) ;
#65723 = LINE ( 'NONE', #28065, #261 ) ;
#65724 = ORIENTED_EDGE ( 'NONE', *, *, #8093, .F. ) ;
#65725 = DIRECTION ( 'NONE',  ( 0.000000000000000000, 0.000000000000000000, 1.000000000000000000 ) ) ;
#65726 = CARTESIAN_POINT ( 'NONE',  ( -37.07086358537073778, 10.58360809068249964, -10.99546437007133903 ) ) ;
#65727 = CARTESIAN_POINT ( 'NONE',  ( 112.1009898303695422, 30.86414810229296890, 44.39243416794982977 ) ) ;
#65728 = CARTESIAN_POINT ( 'NONE',  ( -133.0835080491124813, 52.64966140620838786, 9.123835301881490167 ) ) ;
#65729 = CARTESIAN_POINT ( 'NONE',  ( 18.88468164817599160, 7.626722602998419198, 57.52385489813911335 ) ) ;
#65730 = VERTEX_POINT ( 'NONE', #69318 ) ;
#65731 = ORIENTED_EDGE ( 'NONE', *, *, #56960, .F. ) ;
#65732 = EDGE_LOOP ( 'NONE', ( #54349, #53578, #742, #37252, #20914, #66519, #19668, #28056, #45073, #56387, #15184, #30880, #47939, #42086, #36893 ) ) ;
#65733 = CARTESIAN_POINT ( 'NONE',  ( 429.8372781065086201, 395.0000000000042633, 101.0502958579843806 ) ) ;
#65734 = PLANE ( 'NONE',  #51137 ) ;
#65735 = CARTESIAN_POINT ( 'NONE',  ( -102.2801239173131052, 33.91021738430207222, 3.674523915951417585 ) ) ;
#65736 = CARTESIAN_POINT ( 'NONE',  ( -38.87848244732137459, 10.93141945332450149, -43.80061360289953143 ) ) ;
#65737 = ADVANCED_FACE ( 'NONE', ( #65004 ), #16797, .T. ) ;
#65738 = CARTESIAN_POINT ( 'NONE',  ( -94.97822228984884418, 29.22367841510387620, 93.45206955416084327 ) ) ;
#65739 = CARTESIAN_POINT ( 'NONE',  ( -143.7151964745329167, 59.41799441280377181, 33.44955188324686191 ) ) ;
#65740 = CARTESIAN_POINT ( 'NONE',  ( 61.91366885787727625, 28.42865614899003290, 170.0000000000000000 ) ) ;
#65741 = CARTESIAN_POINT ( 'NONE',  ( -71.42546113164833343, 20.75891408601219368, -13.75210804638004447 ) ) ;
#65742 = CARTESIAN_POINT ( 'NONE',  ( 84.73231936899556160, 18.78199960571076232, 56.78476454528978223 ) ) ;
#65743 = VERTEX_POINT ( 'NONE', #28765 ) ;
#65744 = ADVANCED_FACE ( 'NONE', ( #12580 ), #50906, .F. ) ;
#65745 = AXIS2_PLACEMENT_3D ( 'NONE', #10261, #24734, #67992 ) ;
#65746 = CARTESIAN_POINT ( 'NONE',  ( 32.56927464314651388, 7.618924692399913212, 34.31139869032508471 ) ) ;
#65747 =( NAMED_UNIT ( * ) PLANE_ANGLE_UNIT ( ) SI_UNIT ( $, .RADIAN. ) );
#65748 = ORIENTED_EDGE ( 'NONE', *, *, #53684, .T. ) ;
#65749 = CARTESIAN_POINT ( 'NONE',  ( 188.4937788906149194, 86.43336847120863808, 38.00740919242073090 ) ) ;
#65750 = CARTESIAN_POINT ( 'NONE',  ( 427.4999999999999432, -17.50000000000000000, 0.000000000000000000 ) ) ;
#65752 = DIRECTION ( 'NONE',  ( -1.000000000000000000, 0.000000000000000000, -0.000000000000000000 ) ) ;
#65751 = VECTOR ( 'NONE', #35246, 1000.000000000000000 ) ;
#65753 = CARTESIAN_POINT ( 'NONE',  ( 188.9999999999999432, 0.000000000000000000, -2.000000000000000888 ) ) ;
#65754 = CARTESIAN_POINT ( 'NONE',  ( -48.04019567818505010, 12.91272349839805678, 13.64414622740702221 ) ) ;
#65755 = CARTESIAN_POINT ( 'NONE',  ( 150.9184679586218749, 52.73111408630722963, -39.96492359852010168 ) ) ;
#65757 = CARTESIAN_POINT ( 'NONE',  ( -3.816391647148975608E-14, -9.237604307034022355, -8.785468820183664818 ) ) ;
#65756 = VECTOR ( 'NONE', #44368, 1000.000000000000000 ) ;
#65758 = ORIENTED_EDGE ( 'NONE', *, *, #37086, .F. ) ;
#65759 = CYLINDRICAL_SURFACE ( 'NONE', #19601, 5.000000000000004441 ) ;
#65760 = CARTESIAN_POINT ( 'NONE',  ( -25.57361468187733422, -28.55671243481888055, 13.32819299319723783 ) ) ;
#65761 = ORIENTED_EDGE ( 'NONE', *, *, #56538, .F. ) ;
#65762 = LINE ( 'NONE', #55894, #31959 ) ;
#65763 = CARTESIAN_POINT ( 'NONE',  ( -1.666933348991701536, -64.97862212458815634, 40.00000000000003553 ) ) ;
#65764 = VERTEX_POINT ( 'NONE', #38970 ) ;
#65765 = EDGE_CURVE ( 'NONE', #37519, #14111, #6949, .T. ) ;
#65766 = CARTESIAN_POINT ( 'NONE',  ( -84.54326985437107567, 24.64760594531649573, 42.60397884493846732 ) ) ;
#65767 = CIRCLE ( 'NONE', #9566, 243.4957430088094839 ) ;
#65768 = CARTESIAN_POINT ( 'NONE',  ( 153.2523375521184619, 55.69936538551844052, -76.67477878150734227 ) ) ;
#65769 = CARTESIAN_POINT ( 'NONE',  ( 103.8102216002272939, -165.0710086335687379, 10.00000000000000000 ) ) ;
#65770 = EDGE_CURVE ( 'NONE', #19626, #45314, #38691, .T. ) ;
#65771 = CARTESIAN_POINT ( 'NONE',  ( -31.43908319763709969, 9.591432048623765638, 57.06100499665286208 ) ) ;
#65772 = AXIS2_PLACEMENT_3D ( 'NONE', #20550, #40625, #30428 ) ;
#65773 = EDGE_CURVE ( 'NONE', #30991, #69498, #60759, .T. ) ;
#65774 = EDGE_LOOP ( 'NONE', ( #53052, #36203, #57268, #2594 ) ) ;
#65775 = EDGE_LOOP ( 'NONE', ( #38190, #7397, #51383, #66658 ) ) ;
#65776 = FACE_OUTER_BOUND ( 'NONE', #61964, .T. ) ;
#65777 = ORIENTED_EDGE ( 'NONE', *, *, #65600, .F. ) ;
#65778 = CARTESIAN_POINT ( 'NONE',  ( 32.03384598935271299, 8.576372641735996893, -14.81213577935862347 ) ) ;
#65779 = DIRECTION ( 'NONE',  ( 0.000000000000000000, 0.000000000000000000, 1.000000000000000000 ) ) ;
#65780 = FILL_AREA_STYLE_COLOUR ( '', #63335 ) ;
#65781 = CARTESIAN_POINT ( 'NONE',  ( -30.62628708973294422, -68.47330165179167238, 170.0000000000000000 ) ) ;
#65782 = DIRECTION ( 'NONE',  ( 0.000000000000000000, 0.000000000000000000, -1.000000000000000000 ) ) ;
#65783 = DIRECTION ( 'NONE',  ( 0.7071067811865474617, -0.7071067811865474617, -3.951729029292866070E-16 ) ) ;
#65784 = ORIENTED_EDGE ( 'NONE', *, *, #39582, .F. ) ;
#65785 = DIRECTION ( 'NONE',  ( -0.000000000000000000, -1.000000000000000000, -0.000000000000000000 ) ) ;
#65786 = ORIENTED_EDGE ( 'NONE', *, *, #22475, .F. ) ;
#65787 = VERTEX_POINT ( 'NONE', #40002 ) ;
#65788 = CARTESIAN_POINT ( 'NONE',  ( 163.2886151008987952, 62.32020850087169350, -21.51899005548487764 ) ) ;
#65789 = DIRECTION ( 'NONE',  ( -0.000000000000000000, -0.000000000000000000, -1.000000000000000000 ) ) ;
#65790 = CARTESIAN_POINT ( 'NONE',  ( -169.1005390226459326, 82.76152663947084420, -9.020552741055981372 ) ) ;
#65791 = CARTESIAN_POINT ( 'NONE',  ( 141.2470358420065395, 46.06959063280891797, -69.06272708122817505 ) ) ;
#65792 = LINE ( 'NONE', #28132, #29597 ) ;
#65793 = EDGE_CURVE ( 'NONE', #32664, #68152, #34741, .T. ) ;
#65794 = ADVANCED_FACE ( 'NONE', ( #40348 ), #15719, .F. ) ;
#65795 = VERTEX_POINT ( 'NONE', #13615 ) ;
#65796 = EDGE_CURVE ( 'NONE', #62016, #55532, #58388, .T. ) ;
#65797 = CARTESIAN_POINT ( 'NONE',  ( -61.68940124183719576, 17.61226241086874467, 94.99999999999866418 ) ) ;
#65798 = CARTESIAN_POINT ( 'NONE',  ( -125.8938041572051389, -170.0000000000000000, 57.46449846362076386 ) ) ;
#65799 = CARTESIAN_POINT ( 'NONE',  ( 9.057575839850587229, 6.378493414438676012, 40.83252881098174214 ) ) ;
#65800 = ORIENTED_EDGE ( 'NONE', *, *, #18197, .F. ) ;
#65801 = AXIS2_PLACEMENT_3D ( 'NONE', #26010, #68568, #33632 ) ;
#65802 = B_SPLINE_CURVE_WITH_KNOTS ( 'NONE', 3,
 ( #16616, #37728, #48262, #53548 ),
 .UNSPECIFIED., .F., .F.,
 ( 4, 4 ),
 ( 0.1259919275528358362, 0.1829744153748747437 ),
 .UNSPECIFIED. ) ;
#65803 = CARTESIAN_POINT ( 'NONE',  ( 444.4083459183741525, 365.0000000000000000, 110.6213636698541336 ) ) ;
#65804 = CIRCLE ( 'NONE', #23116, 65.00000000000000000 ) ;
#65805 = ORIENTED_EDGE ( 'NONE', *, *, #56144, .F. ) ;
#65806 = CARTESIAN_POINT ( 'NONE',  ( -143.7151964745329735, 59.41799441280379313, -73.92865047860787797 ) ) ;
#65807 = CARTESIAN_POINT ( 'NONE',  ( -149.5074843970971017, 64.17983161892347255, 72.56537183036277838 ) ) ;
#65808 = DIRECTION ( 'NONE',  ( 0.1342332658176667304, -0.9909497617679331460, 0.000000000000000000 ) ) ;
#65809 = VECTOR ( 'NONE', #26754, 1000.000000000000227 ) ;
#65810 = ORIENTED_EDGE ( 'NONE', *, *, #63600, .F. ) ;
#65811 = VECTOR ( 'NONE', #19163, 1000.000000000000000 ) ;
#65812 = DIRECTION ( 'NONE',  ( -0.000000000000000000, -0.000000000000000000, 1.000000000000000000 ) ) ;
#65813 = CARTESIAN_POINT ( 'NONE',  ( 32.29578462738147238, 8.602609172809797755, 39.82485796498851727 ) ) ;
#65814 = CIRCLE ( 'NONE', #1791, 4.999999999999997335 ) ;
#65815 = CARTESIAN_POINT ( 'NONE',  ( -180.5954680880247167, 97.44843622358462198, -42.85213204725202729 ) ) ;
#65816 = CARTESIAN_POINT ( 'NONE',  ( -130.6002960060536111, 49.67125682092488859, -21.42867186308118477 ) ) ;
#65817 = PLANE ( 'NONE',  #69349 ) ;
#65818 = CARTESIAN_POINT ( 'NONE',  ( 0.000000000000000000, 70.00000000000000000, 0.000000000000000000 ) ) ;
#65819 = ORIENTED_EDGE ( 'NONE', *, *, #69087, .F. ) ;
#65820 = CARTESIAN_POINT ( 'NONE',  ( -48.12872802574265307, 43.70867239603709464, 41.38025477438755928 ) ) ;
#65821 = LINE ( 'NONE', #11627, #61336 ) ;
#65822 = EDGE_LOOP ( 'NONE', ( #993, #32436 ) ) ;
#65823 = CARTESIAN_POINT ( 'NONE',  ( -155.1204242627070187, 70.44799358128193489, -47.29331144879449766 ) ) ;
#65824 = CARTESIAN_POINT ( 'NONE',  ( -3.857727530059795740, 6.665032499723452908, -63.39330917866369219 ) ) ;
#65825 = CARTESIAN_POINT ( 'NONE',  ( -179.2210908201801374, 95.76260491022614474, 69.55831908347232684 ) ) ;
#65826 = DIRECTION ( 'NONE',  ( 0.000000000000000000, 0.000000000000000000, -1.000000000000000000 ) ) ;
#65827 = B_SPLINE_CURVE_WITH_KNOTS ( 'NONE', 3,
 ( #35260, #61981, #46151, #9570, #20452, #67976, #8538, #63377, #9220, #29984 ),
 .UNSPECIFIED., .F., .F.,
 ( 4, 2, 2, 2, 4 ),
 ( 0.000000000000000000, 0.001080786818375923915, 0.002161573636751847830, 0.003242360455127771962, 0.004323147273503695660 ),
 .UNSPECIFIED. ) ;
#65828 = DIRECTION ( 'NONE',  ( -3.903127820947816455E-16, 0.000000000000000000, 1.000000000000000000 ) ) ;
#65829 = CARTESIAN_POINT ( 'NONE',  ( 70.26840926437850499, 15.51363403943109631, -95.00000000000133582 ) ) ;
#65830 = CARTESIAN_POINT ( 'NONE',  ( 20.79325243092023001, -13.87950479462515396, 0.000000000000000000 ) ) ;
#65831 = CARTESIAN_POINT ( 'NONE',  ( -422.6627218934914936, 399.9999999999998863, -141.4497041420118535 ) ) ;
#65832 = DIRECTION ( 'NONE',  ( -0.7071067811865475727, 0.000000000000000000, -0.7071067811865474617 ) ) ;
#65833 = CARTESIAN_POINT ( 'NONE',  ( 117.7447573007802930, 32.50990724960316669, 10.75687092132448086 ) ) ;
#65834 = CARTESIAN_POINT ( 'NONE',  ( -52.74963828369503460, 15.11526739861312940, -89.26458726870900762 ) ) ;
#65835 = ORIENTED_EDGE ( 'NONE', *, *, #26708, .F. ) ;
#65836 = ADVANCED_FACE ( 'NONE', ( #13960 ), #14994, .T. ) ;
#65837 = DIRECTION ( 'NONE',  ( 0.000000000000000000, 0.000000000000000000, -1.000000000000000000 ) ) ;
#65838 = ORIENTED_EDGE ( 'NONE', *, *, #14536, .T. ) ;
#65839 = DIRECTION ( 'NONE',  ( -9.115745035929406798E-64, 3.469446951953612956E-17, -1.000000000000000000 ) ) ;
#65840 = CARTESIAN_POINT ( 'NONE',  ( 80.71682498289318630, 18.54204664833076777, -65.52526976266784686 ) ) ;
#65841 = CARTESIAN_POINT ( 'NONE',  ( 115.9806768122906959, 32.75124074837841448, 85.95842849936387609 ) ) ;
#65842 = LINE ( 'NONE', #44358, #62692 ) ;
#65843 = CARTESIAN_POINT ( 'NONE',  ( 23.05216796272351232, -9.986758404123879274, 0.000000000000000000 ) ) ;
#65844 = CARTESIAN_POINT ( 'NONE',  ( -24.32471770265758693, 9.546495606312143778, -45.24190841075698444 ) ) ;
#65845 = PLANE ( 'NONE',  #17542 ) ;
#65846 = CARTESIAN_POINT ( 'NONE',  ( -149.5074843970971301, -170.0000000000000000, -76.65738112195568021 ) ) ;
#65847 = DIRECTION ( 'NONE',  ( -0.000000000000000000, 1.000000000000000000, -0.000000000000000000 ) ) ;
#65848 = VERTEX_POINT ( 'NONE', #61797 ) ;
#65849 = ORIENTED_EDGE ( 'NONE', *, *, #16352, .F. ) ;
#65850 = EDGE_CURVE ( 'NONE', #41788, #56234, #20238, .T. ) ;
#65851 = DIRECTION ( 'NONE',  ( 1.000000000000000000, 0.000000000000000000, 0.000000000000000000 ) ) ;
#65852 = CARTESIAN_POINT ( 'NONE',  ( 176.4367926094704728, 74.03315361639846515, 57.76155730348418160 ) ) ;
#65853 = DIRECTION ( 'NONE',  ( 1.000000000000000000, 0.000000000000000000, -0.000000000000000000 ) ) ;
#65854 = AXIS2_PLACEMENT_3D ( 'NONE', #5415, #43382, #59210 ) ;
#65855 = CARTESIAN_POINT ( 'NONE',  ( -172.3038663181179970, 87.72015621195183144, 72.66624519710477159 ) ) ;
#65856 = CARTESIAN_POINT ( 'NONE',  ( -166.3205068063721512, 81.30869308872871670, -18.54204906781616558 ) ) ;
#65857 = ADVANCED_FACE ( 'NONE', ( #41397 ), #57909, .F. ) ;
#65858 = EDGE_CURVE ( 'NONE', #5346, #43873, #3073, .T. ) ;
#65859 = AXIS2_PLACEMENT_3D ( 'NONE', #29489, #3456, #23532 ) ;
#65860 = CARTESIAN_POINT ( 'NONE',  ( 254.4165763529819344, -27.00000000000000355, 108.9999999999999858 ) ) ;
#65861 = ORIENTED_EDGE ( 'NONE', *, *, #19401, .F. ) ;
#65862 = EDGE_CURVE ( 'NONE', #40678, #37904, #18987, .T. ) ;
#65863 = CARTESIAN_POINT ( 'NONE',  ( 102.7938674513919040, 26.67851209377773358, -42.41119417710807937 ) ) ;
#65864 = CIRCLE ( 'NONE', #60264, 65.00000000000000000 ) ;
#65865 = VECTOR ( 'NONE', #68550, 1000.000000000000000 ) ;
#65866 = CARTESIAN_POINT ( 'NONE',  ( -11.78792974237933677, 7.181513757308656487, 58.08769183103347444 ) ) ;
#65867 = CARTESIAN_POINT ( 'NONE',  ( 4.999999999999999112, 0.000000000000000000, 3.469446951953614189E-15 ) ) ;
#65868 = CARTESIAN_POINT ( 'NONE',  ( 0.000000000000000000, 0.000000000000000000, 43.58025477438756212 ) ) ;
#65869 = DIRECTION ( 'NONE',  ( -0.000000000000000000, -0.000000000000000000, -1.000000000000000000 ) ) ;
#65870 = CARTESIAN_POINT ( 'NONE',  ( 207.4867844023104340, 110.2451255333963474, -10.00719937993713238 ) ) ;
#65871 = FACE_BOUND ( 'NONE', #27950, .T. ) ;
#65872 = AXIS2_PLACEMENT_3D ( 'NONE', #54756, #38955, #38238 ) ;
#65873 = CARTESIAN_POINT ( 'NONE',  ( -59.95707852844799390, 16.05120821151901822, -48.41212873588224141 ) ) ;
#65874 = VECTOR ( 'NONE', #25758, 1000.000000000000114 ) ;
#65875 = AXIS2_PLACEMENT_3D ( 'NONE', #25009, #45767, #35556 ) ;
#65876 = EDGE_LOOP ( 'NONE', ( #49573, #20406, #35766, #62857 ) ) ;
#65877 = LINE ( 'NONE', #13095, #8703 ) ;
#65878 = DIRECTION ( 'NONE',  ( -1.000000000000000000, 0.000000000000000000, 2.775557561562891844E-16 ) ) ;
#65879 = DIRECTION ( 'NONE',  ( -1.000000000000000000, 0.000000000000000000, 0.000000000000000000 ) ) ;
#65880 = CARTESIAN_POINT ( 'NONE',  ( -48.00000000000000000, 19.99999999999996447, 4.000000000000000000 ) ) ;
#65881 = CARTESIAN_POINT ( 'NONE',  ( 209.6642862813005763, 115.2127693334914085, 57.91457532517448215 ) ) ;
#65882 = DIRECTION ( 'NONE',  ( 1.000000000000000000, 0.000000000000000000, 0.000000000000000000 ) ) ;
#65883 = ORIENTED_EDGE ( 'NONE', *, *, #43046, .F. ) ;
#65884 = EDGE_CURVE ( 'NONE', #19391, #58062, #25875, .T. ) ;
#65885 = CARTESIAN_POINT ( 'NONE',  ( -61.41100614348627573, -43.07262267896732766, 170.0000000000000000 ) ) ;
#65886 = DIRECTION ( 'NONE',  ( -0.000000000000000000, 0.000000000000000000, 1.000000000000000000 ) ) ;
#65887 = ORIENTED_EDGE ( 'NONE', *, *, #51856, .T. ) ;
#65888 = DIRECTION ( 'NONE',  ( -2.220446049250313081E-16, 0.000000000000000000, -1.000000000000000000 ) ) ;
#65889 = EDGE_LOOP ( 'NONE', ( #11307, #65393, #56123, #2202 ) ) ;
#65890 = LINE ( 'NONE', #60935, #38738 ) ;
#65891 = DIRECTION ( 'NONE',  ( 1.000000000000000000, -0.000000000000000000, -0.000000000000000000 ) ) ;
#65892 = CARTESIAN_POINT ( 'NONE',  ( 102.8518012651273779, 25.61025413220827929, 38.40957065262233527 ) ) ;
#65893 = ORIENTED_EDGE ( 'NONE', *, *, #43336, .F. ) ;
#65894 = VERTEX_POINT ( 'NONE', #62144 ) ;
#65895 = DIRECTION ( 'NONE',  ( -0.000000000000000000, -0.000000000000000000, -1.000000000000000000 ) ) ;
#65896 = CARTESIAN_POINT ( 'NONE',  ( 164.0073343966822392, 64.23003864582457823, 40.59522386251838100 ) ) ;
#65897 = CARTESIAN_POINT ( 'NONE',  ( 107.9342863085848023, 28.93180871323604109, 3.115243763729523163 ) ) ;
#65898 = CARTESIAN_POINT ( 'NONE',  ( 63.50537371531942199, 13.81987663608982864, 17.96841034875761878 ) ) ;
#65899 = CARTESIAN_POINT ( 'NONE',  ( 10.78925482157266913, -22.68765681156003566, 0.000000000000000000 ) ) ;
#65900 = PRODUCT ( 'rotor', 'rotor', '', ( #69118 ) ) ;
#65901 = DIRECTION ( 'NONE',  ( -0.9639628606958512425, -0.2660368455666826670, 0.000000000000000000 ) ) ;
#65902 = VECTOR ( 'NONE', #41424, 1000.000000000000000 ) ;
#65903 = CARTESIAN_POINT ( 'NONE',  ( -149.5074843970971017, 65.50121172469319220, -7.968279941028269420 ) ) ;
#65904 = CARTESIAN_POINT ( 'NONE',  ( -131.6399667378751417, 51.62465701391630546, -10.72301646190411795 ) ) ;
#65905 = CARTESIAN_POINT ( 'NONE',  ( 196.9999999999999716, 2.999999999999969802, 0.000000000000000000 ) ) ;
#65906 = CARTESIAN_POINT ( 'NONE',  ( 2.999999999999992450, 0.000000000000000000, 0.000000000000000000 ) ) ;
#65907 = CARTESIAN_POINT ( 'NONE',  ( 80.27305752291051988, 17.34925310068689441, 86.90588607176617586 ) ) ;
#65908 = AXIS2_PLACEMENT_3D ( 'NONE', #57024, #3900, #46106 ) ;
#65910 = VERTEX_POINT ( 'NONE', #51602 ) ;
#65909 = DIRECTION ( 'NONE',  ( 0.000000000000000000, -1.000000000000000000, 0.000000000000000000 ) ) ;
#65911 = ORIENTED_EDGE ( 'NONE', *, *, #40488, .F. ) ;
#65912 = VECTOR ( 'NONE', #56087, 1000.000000000000000 ) ;
#65914 = ORIENTED_EDGE ( 'NONE', *, *, #56052, .F. ) ;
#65913 = PRODUCT_DEFINITION ( 'UNKNOWN', '', #68124, #31743 ) ;
#65915 = DIRECTION ( 'NONE',  ( -0.000000000000000000, 1.000000000000000000, -0.000000000000000000 ) ) ;
#65916 = CARTESIAN_POINT ( 'NONE',  ( -174.2736917738521925, 89.94190505570455230, 84.59568540053871288 ) ) ;
#65917 = CARTESIAN_POINT ( 'NONE',  ( -50.14771795543004629, 13.42081263859818208, -21.56642457232588939 ) ) ;
#65918 = DIRECTION ( 'NONE',  ( 0.08963930890342654279, 0.9959742939952397345, -0.000000000000000000 ) ) ;
#65919 = FACE_OUTER_BOUND ( 'NONE', #32121, .T. ) ;
#65920 = EDGE_CURVE ( 'NONE', #63617, #56134, #56887, .T. ) ;
#65921 = CARTESIAN_POINT ( 'NONE',  ( -58.33157376762795110, 16.63098604184964202, -35.96663671462522416 ) ) ;
#65922 = EDGE_CURVE ( 'NONE', #43301, #17942, #46658, .T. ) ;
#65923 = DIRECTION ( 'NONE',  ( 0.9268618657695262275, 0.3754025596372950191, 0.000000000000000000 ) ) ;
#65924 = CARTESIAN_POINT ( 'NONE',  ( -77.72491324796695267, 21.96482567905606587, -76.91587359936697510 ) ) ;
#65925 = CARTESIAN_POINT ( 'NONE',  ( -15.08468253268399906, 7.472949889606722351, 35.66772536392182502 ) ) ;
#65926 = EDGE_LOOP ( 'NONE', ( #46027, #62653, #1353, #59561, #24899, #59922, #3473 ) ) ;
#65927 = VECTOR ( 'NONE', #25671, 1000.000000000000000 ) ;
#65928 = EDGE_CURVE ( 'NONE', #41738, #15521, #45284, .T. ) ;
#65929 = CARTESIAN_POINT ( 'NONE',  ( -36.60035584460344893, -11.39778684791367702, 13.32819299319725026 ) ) ;
#65930 = EDGE_LOOP ( 'NONE', ( #51666, #29105, #12881, #45133, #45356 ) ) ;
#65931 = VERTEX_POINT ( 'NONE', #11429 ) ;
#65932 = CARTESIAN_POINT ( 'NONE',  ( -146.5309471467636513, 62.99917515507674892, 18.26406283408425324 ) ) ;
#65933 = CARTESIAN_POINT ( 'NONE',  ( -55.05276343752910151, 15.72344139423345588, -88.90542517938717992 ) ) ;
#65934 = CARTESIAN_POINT ( 'NONE',  ( -165.9121868482146454, 80.88751546905565704, 36.23135190961774299 ) ) ;
#65935 = CARTESIAN_POINT ( 'NONE',  ( 112.1100957124161539, 30.86846953551572170, -23.85696266999899606 ) ) ;
#65936 = CARTESIAN_POINT ( 'NONE',  ( -109.6829043543429236, 36.70322915510440254, -95.00000000000133582 ) ) ;
#65937 = DIRECTION ( 'NONE',  ( -1.000000000000000000, 0.000000000000000000, 0.000000000000000000 ) ) ;
#65938 = DIRECTION ( 'NONE',  ( 1.000000000000000000, 0.000000000000000000, 0.000000000000000000 ) ) ;
#65939 = ORIENTED_EDGE ( 'NONE', *, *, #39483, .T. ) ;
#65940 = ORIENTED_EDGE ( 'NONE', *, *, #27929, .F. ) ;
#65941 = ORIENTED_EDGE ( 'NONE', *, *, #27801, .T. ) ;
#65942 = DIRECTION ( 'NONE',  ( -0.000000000000000000, -0.000000000000000000, -1.000000000000000000 ) ) ;
#65943 = CARTESIAN_POINT ( 'NONE',  ( -14.32120159453990205, 7.401444311907545703, 7.013986508477913162 ) ) ;
#65944 = CARTESIAN_POINT ( 'NONE',  ( 35.65685430025423841, 7.951642554322392087, -63.44794714536580926 ) ) ;
#65945 = CARTESIAN_POINT ( 'NONE',  ( 62.53328835682437159, 12.56090025569836932, -23.87614024170609639 ) ) ;
#65946 = EDGE_CURVE ( 'NONE', #44768, #28503, #48357, .T. ) ;
#65947 = EDGE_CURVE ( 'NONE', #56201, #57172, #39434, .T. ) ;
#65948 = CARTESIAN_POINT ( 'NONE',  ( -47.55360235114367384, 12.79819361309568393, 37.30471606777894067 ) ) ;
#65949 = CARTESIAN_POINT ( 'NONE',  ( 204.6977192012829789, 108.0580384837234931, 71.05227132923315025 ) ) ;
#65950 = ORIENTED_EDGE ( 'NONE', *, *, #2444, .T. ) ;
#65951 = DIRECTION ( 'NONE',  ( 1.000000000000000000, 0.000000000000000000, 0.000000000000000000 ) ) ;
#65952 = CARTESIAN_POINT ( 'NONE',  ( 203.1414537950836063, 105.9225671689748509, -63.32313587288669510 ) ) ;
#65953 = FACE_OUTER_BOUND ( 'NONE', #19882, .T. ) ;
#65954 = CARTESIAN_POINT ( 'NONE',  ( -167.9853834315979668, 81.58767916550901589, 16.96324577511894560 ) ) ;
#65955 = CARTESIAN_POINT ( 'NONE',  ( -81.90020664963799391, 23.57971581008656869, -49.38679830630213274 ) ) ;
#65956 = FACE_BOUND ( 'NONE', #52865, .T. ) ;
#65957 = CARTESIAN_POINT ( 'NONE',  ( -190.3787397234653724, 108.6757967724292513, 88.09417750515896728 ) ) ;
#65958 = VECTOR ( 'NONE', #33316, 1000.000000000000000 ) ;
#65959 = ORIENTED_EDGE ( 'NONE', *, *, #6995, .T. ) ;
#65960 = CIRCLE ( 'NONE', #46852, 243.4957430088094839 ) ;
#65961 = CARTESIAN_POINT ( 'NONE',  ( -48.00000000000000711, -20.00000000000000355, 0.000000000000000000 ) ) ;
#65962 = CARTESIAN_POINT ( 'NONE',  ( -132.4819073909166036, 50.98736898418874119, -65.63572201618941904 ) ) ;
#65963 = CARTESIAN_POINT ( 'NONE',  ( -104.5740066103012964, 35.09687312794778080, -76.50358383647001403 ) ) ;
#65964 = CARTESIAN_POINT ( 'NONE',  ( 45.36109889487606495, 9.259412558041157482, -65.38405568555769776 ) ) ;
#65965 = CARTESIAN_POINT ( 'NONE',  ( 15.78827728214693416, 6.500811158483328356, 18.17015708224157322 ) ) ;
#65966 = ORIENTED_EDGE ( 'NONE', *, *, #1303, .T. ) ;
#65967 = CIRCLE ( 'NONE', #51395, 4.999999999999996447 ) ;
#65968 = LINE ( 'NONE', #31612, #9569 ) ;
#65969 = VERTEX_POINT ( 'NONE', #38173 ) ;
#65970 = DIRECTION ( 'NONE',  ( 0.000000000000000000, 1.000000000000000000, 0.000000000000000000 ) ) ;
#65971 = CARTESIAN_POINT ( 'NONE',  ( 177.2960928338502242, 74.86012380916936593, 84.01690539734444485 ) ) ;
#65972 = ORIENTED_EDGE ( 'NONE', *, *, #61391, .T. ) ;
#65973 = CIRCLE ( 'NONE', #36786, 60.00000000000000000 ) ;
#65974 = VERTEX_POINT ( 'NONE', #26589 ) ;
#65975 = CARTESIAN_POINT ( 'NONE',  ( 174.9053416555736646, 72.57849647436444229, -48.00675063682053434 ) ) ;
#65976 = CARTESIAN_POINT ( 'NONE',  ( -175.9852529046322331, 90.37283472601130541, -62.11202431634223586 ) ) ;
#65977 = DIRECTION ( 'NONE',  ( -1.000000000000000000, 0.000000000000000000, 0.000000000000000000 ) ) ;
#65978 = EDGE_LOOP ( 'NONE', ( #27225, #48447 ) ) ;
#65979 = CARTESIAN_POINT ( 'NONE',  ( -30.00000000000000355, 29.99999999999999645, 15.00000000000000000 ) ) ;
#65980 = CARTESIAN_POINT ( 'NONE',  ( -174.7869898116916545, 88.99756909636809610, 18.83855922235676772 ) ) ;
#65981 = CARTESIAN_POINT ( 'NONE',  ( 8.000000000000007105, 249.8719672152120381, -95.00000000000133582 ) ) ;
#65982 = CARTESIAN_POINT ( 'NONE',  ( 11.30618213853385967, 74.15344055032308290, 170.0000000000000000 ) ) ;
#65983 = CARTESIAN_POINT ( 'NONE',  ( 69.72313848477121212, 27.50266661387133738, 41.38025477438755928 ) ) ;
#65984 = CARTESIAN_POINT ( 'NONE',  ( -189.7334103489410211, 107.7745063523401257, 35.72630607762302191 ) ) ;
#65985 = EDGE_LOOP ( 'NONE', ( #53755, #5814, #10893, #48302 ) ) ;
#65986 = DIRECTION ( 'NONE',  ( 1.000000000000000000, 0.000000000000000000, 0.000000000000000000 ) ) ;
#65987 = CARTESIAN_POINT ( 'NONE',  ( -72.21947956767114363, 21.03570528348188873, 7.233083253217232667 ) ) ;
#65988 = PLANE ( 'NONE',  #50639 ) ;
#65989 = DIRECTION ( 'NONE',  ( -0.000000000000000000, 1.000000000000000000, -1.224646799147353207E-16 ) ) ;
#65991 = ORIENTED_EDGE ( 'NONE', *, *, #24880, .T. ) ;
#65990 = CARTESIAN_POINT ( 'NONE',  ( -132.1645230123639010, 50.76361971363044745, 87.68261071308809562 ) ) ;
#65992 = CARTESIAN_POINT ( 'NONE',  ( 81.76092782665033099, 17.81692437267513895, -37.61113886829519259 ) ) ;
#65993 = EDGE_CURVE ( 'NONE', #51688, #62713, #36962, .T. ) ;
#65994 = ORIENTED_EDGE ( 'NONE', *, *, #1597, .F. ) ;
#65995 = CARTESIAN_POINT ( 'NONE',  ( -142.6264002846224059, 58.55577336362197371, 62.06999168838819259 ) ) ;
#65996 = AXIS2_PLACEMENT_3D ( 'NONE', #5969, #38338, #5627 ) ;
#65997 = CARTESIAN_POINT ( 'NONE',  ( 79.91920957766409117, 18.29292522273512489, 40.60004261239478041 ) ) ;
#65998 = DIRECTION ( 'NONE',  ( 0.000000000000000000, -3.469446951953614805E-17, 1.000000000000000000 ) ) ;
#65999 = CARTESIAN_POINT ( 'NONE',  ( 185.1647878987786271, 82.82967084668432278, -23.18872253868788391 ) ) ;
#66000 = EDGE_CURVE ( 'NONE', #15856, #55870, #58431, .T. ) ;
#66001 = CARTESIAN_POINT ( 'NONE',  ( 135.6842057900327347, 42.53841116629840968, -9.390205697492525871 ) ) ;
#66002 = VECTOR ( 'NONE', #12025, 1000.000000000000000 ) ;
#66003 = DIRECTION ( 'NONE',  ( -0.000000000000000000, -0.000000000000000000, -1.000000000000000000 ) ) ;
#66004 = CARTESIAN_POINT ( 'NONE',  ( 87.11228333101216492, 19.58587579906928866, -62.66611478937539204 ) ) ;
#66005 = EDGE_CURVE ( 'NONE', #49272, #9033, #32699, .T. ) ;
#66006 = LINE ( 'NONE', #33291, #30668 ) ;
#66007 = ORIENTED_EDGE ( 'NONE', *, *, #53660, .F. ) ;
#66008 = APPLICATION_CONTEXT ( 'automotive_design' ) ;
#66009 = ORIENTED_EDGE ( 'NONE', *, *, #24705, .T. ) ;
#66010 = AXIS2_PLACEMENT_3D ( 'NONE', #25376, #37628, #26399 ) ;
#66011 = ADVANCED_FACE ( 'NONE', ( #12152 ), #29368, .F. ) ;
#66012 = CARTESIAN_POINT ( 'NONE',  ( 39.88971011078924533, 8.472992116645421845, 29.91383430596324189 ) ) ;
#66013 = CARTESIAN_POINT ( 'NONE',  ( 197.6316695787931792, 97.13022718399022892, -14.44928575426319028 ) ) ;
#66014 = FACE_OUTER_BOUND ( 'NONE', #55796, .T. ) ;
#66015 = CARTESIAN_POINT ( 'NONE',  ( 0.000000000000000000, 0.000000000000000000, 41.38025477438755928 ) ) ;
#66016 = VECTOR ( 'NONE', #48200, 1000.000000000000000 ) ;
#66017 = CARTESIAN_POINT ( 'NONE',  ( 206.3053863259449656, 110.3084416756849464, -36.45535708260618435 ) ) ;
#66018 = CARTESIAN_POINT ( 'NONE',  ( -71.17984086584777970, 20.67393782512344202, -68.94505476070409600 ) ) ;
#66019 = VECTOR ( 'NONE', #28508, 1000.000000000000000 ) ;
#66020 = CARTESIAN_POINT ( 'NONE',  ( -102.7456062648101494, 33.01749955571777662, 57.36362509687879907 ) ) ;
#66021 = CARTESIAN_POINT ( 'NONE',  ( -24.70911172866234651, 8.583078995053025295, -46.16381964219784351 ) ) ;
#66022 = CARTESIAN_POINT ( 'NONE',  ( 164.0158927577712973, 62.92463143894075017, -74.16841973653133380 ) ) ;
#66023 = VERTEX_POINT ( 'NONE', #1243 ) ;
#66024 = DIRECTION ( 'NONE',  ( -0.000000000000000000, -0.000000000000000000, 1.000000000000000000 ) ) ;
#66025 = VERTEX_POINT ( 'NONE', #50478 ) ;
#66027 = VECTOR ( 'NONE', #67984, 1000.000000000000000 ) ;
#66026 = CARTESIAN_POINT ( 'NONE',  ( 0.000000000000000000, 0.000000000000000000, 40.00000000000003553 ) ) ;
#66028 = CARTESIAN_POINT ( 'NONE',  ( -71.70022581596595046, 19.78923414567082517, 94.40528620588804642 ) ) ;
#66029 = CARTESIAN_POINT ( 'NONE',  ( -81.00507684688696486, 23.22613445438386393, 71.89280214441502892 ) ) ;
#66030 = EDGE_CURVE ( 'NONE', #26757, #40830, #12498, .T. ) ;
#66031 = CARTESIAN_POINT ( 'NONE',  ( -30.26163407093831381, -23.53144909134785578, 13.32819299319723605 ) ) ;
#66032 = DIRECTION ( 'NONE',  ( -0.000000000000000000, -1.000000000000000000, -0.000000000000000000 ) ) ;
#66033 = CARTESIAN_POINT ( 'NONE',  ( 10.55634918610403084, -3.079134169858832593E-14, 2.000000000000001776 ) ) ;
#66034 = CARTESIAN_POINT ( 'NONE',  ( -22.50000000000003197, 207.5000000000000284, 378.0000000000000000 ) ) ;
#66035 = CARTESIAN_POINT ( 'NONE',  ( 68.07999999999999829, 0.000000000000000000, 30.00000000000000000 ) ) ;
#66036 = CARTESIAN_POINT ( 'NONE',  ( 39.08370485336855182, 8.368158338059329182, 83.60250626382003247 ) ) ;
#66037 = ORIENTED_EDGE ( 'NONE', *, *, #22963, .T. ) ;
#66038 = CARTESIAN_POINT ( 'NONE',  ( 58.08938767906775524, 12.61185010801508710, 69.83399136998372114 ) ) ;
#66039 = DIRECTION ( 'NONE',  ( 0.000000000000000000, 0.000000000000000000, -1.000000000000000000 ) ) ;
#66040 = CARTESIAN_POINT ( 'NONE',  ( -12.78319349481551370, 8.274445259016799170, 16.41990438160611987 ) ) ;
#66041 = CARTESIAN_POINT ( 'NONE',  ( 281.6144526446208829, -21.48289790755742956, -4.743601953786250824 ) ) ;
#66042 = CARTESIAN_POINT ( 'NONE',  ( 0.000000000000000000, 0.000000000000000000, 0.000000000000000000 ) ) ;
#66043 = CARTESIAN_POINT ( 'NONE',  ( 126.3732561463888970, 38.23795180971329444, -17.24332148280019439 ) ) ;
#66044 = ORIENTED_EDGE ( 'NONE', *, *, #12713, .F. ) ;
#66045 = CARTESIAN_POINT ( 'NONE',  ( 596.8028725243567578, 845.2602351936943705, 622.5068267248695975 ) ) ;
#66046 = CARTESIAN_POINT ( 'NONE',  ( -31.11269837220804035, 15.55634918610408945, 0.000000000000000000 ) ) ;
#66047 = CARTESIAN_POINT ( 'NONE',  ( -37.39246151129641049, 11.66872370876246201, -38.22934263161189250 ) ) ;
#66048 = LINE ( 'NONE', #55465, #42429 ) ;
#66049 = ITEM_DEFINED_TRANSFORMATION ( 'NONE', 'NONE', #22004,  #66832 ) ;
#66050 = CARTESIAN_POINT ( 'NONE',  ( -166.5806157913017387, 80.13147666146447534, 88.32463021072648246 ) ) ;
#66051 = VERTEX_POINT ( 'NONE', #49759 ) ;
#66052 = CARTESIAN_POINT ( 'NONE',  ( -118.4553071845215015, 41.78724769484931301, -43.51166089188798480 ) ) ;
#66053 = DIRECTION ( 'NONE',  ( 0.000000000000000000, 1.000000000000000000, -0.000000000000000000 ) ) ;
#66054 = VECTOR ( 'NONE', #51260, 1000.000000000000114 ) ;
#66055 = CARTESIAN_POINT ( 'NONE',  ( -142.5211356634642073, 58.47296527616904882, -18.20987446567380985 ) ) ;
#66056 = CARTESIAN_POINT ( 'NONE',  ( -1.455067768715154530, 7.566780179921183347, -65.79655557177798642 ) ) ;
#66057 = AXIS2_PLACEMENT_3D ( 'NONE', #3224, #67940, #8849 ) ;
#66058 = CARTESIAN_POINT ( 'NONE',  ( 0.000000000000000000, 0.000000000000000000, 40.00000000000003553 ) ) ;
#66059 = B_SPLINE_CURVE_WITH_KNOTS ( 'NONE', 3,
 ( #12017, #12715, #39792, #54910, #8132, #23959, #28901, #18331 ),
 .UNSPECIFIED., .F., .F.,
 ( 4, 2, 2, 4 ),
 ( 0.004673709593152168724, 0.005837709341827655544, 0.007001709090503143232, 0.009329708587854116872 ),
 .UNSPECIFIED. ) ;
#66060 = EDGE_LOOP ( 'NONE', ( #3599, #53159 ) ) ;
#66061 = DIRECTION ( 'NONE',  ( 0.000000000000000000, 0.000000000000000000, 1.000000000000000000 ) ) ;
#66062 = CARTESIAN_POINT ( 'NONE',  ( 204.6977192012829789, 106.3443248447423599, -51.32593103262161094 ) ) ;
#66063 = VECTOR ( 'NONE', #34725, 999.9999999999998863 ) ;
#66064 = DIRECTION ( 'NONE',  ( 0.000000000000000000, 0.000000000000000000, 1.000000000000000000 ) ) ;
#66065 = CARTESIAN_POINT ( 'NONE',  ( 16.77391662606471456, 6.533867394142988339, -35.56755799161265941 ) ) ;
#66066 =( GEOMETRIC_REPRESENTATION_CONTEXT ( 3 ) GLOBAL_UNCERTAINTY_ASSIGNED_CONTEXT ( ( #7882 ) ) GLOBAL_UNIT_ASSIGNED_CONTEXT ( ( #14926, #19874, #53234 ) ) REPRESENTATION_CONTEXT ( 'NONE', 'WORKASPACE' ) );
#66068 = ORIENTED_EDGE ( 'NONE', *, *, #4904, .T. ) ;
#66067 = CARTESIAN_POINT ( 'NONE',  ( 117.0069443446175512, 33.26475960880694061, 13.51689491381812402 ) ) ;
#66069 = ADVANCED_FACE ( 'NONE', ( #11786 ), #30388, .T. ) ;
#66070 = CARTESIAN_POINT ( 'NONE',  ( 179.4074606910091347, 78.34362448405025248, 71.01390593598598855 ) ) ;
#66071 = ORIENTED_EDGE ( 'NONE', *, *, #67282, .F. ) ;
#66072 = VERTEX_POINT ( 'NONE', #44134 ) ;
#66073 = AXIS2_PLACEMENT_3D ( 'NONE', #59832, #38044, #64781 ) ;
#66074 = CARTESIAN_POINT ( 'NONE',  ( -71.22878586122432409, 19.62649588091170116, -14.77281325402038448 ) ) ;
#66075 = DIRECTION ( 'NONE',  ( -0.000000000000000000, -0.000000000000000000, 1.000000000000000000 ) ) ;
#66077 = VERTEX_POINT ( 'NONE', #22350 ) ;
#66076 = CARTESIAN_POINT ( 'NONE',  ( 39.40195752203892710, -170.0000000000000000, 37.41383430596326320 ) ) ;
#66078 = CARTESIAN_POINT ( 'NONE',  ( 162.6190874793280443, 61.76782592053313437, 31.45076619963536757 ) ) ;
#66079 = LINE ( 'NONE', #11526, #50940 ) ;
#66080 = FACE_BOUND ( 'NONE', #26398, .T. ) ;
#66081 = VERTEX_POINT ( 'NONE', #43786 ) ;
#66082 = DIRECTION ( 'NONE',  ( 1.000000000000000000, 0.000000000000000000, 0.000000000000000000 ) ) ;
#66083 = ADVANCED_FACE ( 'NONE', ( #33958 ), #65624, .T. ) ;
#66084 = CARTESIAN_POINT ( 'NONE',  ( -33.83558513595455253, 9.996963989836508802, -8.861627575112802191 ) ) ;
#66085 = CARTESIAN_POINT ( 'NONE',  ( 110.2429982417149574, 29.99119854320843714, 44.61121420573733332 ) ) ;
#66086 = DIRECTION ( 'NONE',  ( -0.000000000000000000, -0.000000000000000000, -1.000000000000000000 ) ) ;
#66087 = CARTESIAN_POINT ( 'NONE',  ( 0.000000000000000000, 0.000000000000000000, 41.38025477438755928 ) ) ;
#66088 = ORIENTED_EDGE ( 'NONE', *, *, #21073, .T. ) ;
#66089 = EDGE_LOOP ( 'NONE', ( #54038, #44595, #45536, #11068, #10452, #57295 ) ) ;
#66090 = ORIENTED_EDGE ( 'NONE', *, *, #30646, .F. ) ;
#66091 = ADVANCED_FACE ( 'NONE', ( #55045 ), #27971, .F. ) ;
#66092 = CARTESIAN_POINT ( 'NONE',  ( 50.98853755884140071, 400.0000000000071054, 101.0502958579881465 ) ) ;
#66093 = CARTESIAN_POINT ( 'NONE',  ( -108.6622665321722963, 37.28993738537008795, 7.227033062257481433 ) ) ;
#66094 = CARTESIAN_POINT ( 'NONE',  ( -102.2801239173131194, -170.0000000000000000, 11.17452391595143091 ) ) ;
#66095 = CARTESIAN_POINT ( 'NONE',  ( 163.5430354047457229, -170.0000000000000000, 94.99999999999866418 ) ) ;
#66096 = DIRECTION ( 'NONE',  ( 1.000000000000000000, 0.000000000000000000, 0.000000000000000000 ) ) ;
#66097 = DIRECTION ( 'NONE',  ( 0.6234898018587431423, -0.7818314824680220321, 0.000000000000000000 ) ) ;
#66098 = CARTESIAN_POINT ( 'NONE',  ( -126.7989199172159260, 47.09198523267864545, 57.50526014522036178 ) ) ;
#66099 = CARTESIAN_POINT ( 'NONE',  ( -73.81801970646054656, 21.60231032711190835, -10.04354702328394922 ) ) ;
#66100 = ORIENTED_EDGE ( 'NONE', *, *, #33150, .T. ) ;
#66101 = FACE_OUTER_BOUND ( 'NONE', #15255, .T. ) ;
#66102 = ORIENTED_EDGE ( 'NONE', *, *, #39483, .F. ) ;
#66103 = AXIS2_PLACEMENT_3D ( 'NONE', #18194, #65694, #39303 ) ;
#66104 = CARTESIAN_POINT ( 'NONE',  ( -173.9048502674867507, 88.00429107724478683, -88.43178570352854706 ) ) ;
#66105 = DIRECTION ( 'NONE',  ( 0.000000000000000000, 0.000000000000000000, 1.000000000000000000 ) ) ;
#66106 =( REPRESENTATION_RELATIONSHIP ('NONE','NONE', #40274, #64096 ) REPRESENTATION_RELATIONSHIP_WITH_TRANSFORMATION ( #66049 )SHAPE_REPRESENTATION_RELATIONSHIP( ) );
#66107 = ORIENTED_EDGE ( 'NONE', *, *, #29230, .T. ) ;
#66108 = DIRECTION ( 'NONE',  ( -0.000000000000000000, -0.000000000000000000, -1.000000000000000000 ) ) ;
#66109 = EDGE_CURVE ( 'NONE', #24416, #34646, #60682, .T. ) ;
#66110 = LINE ( 'NONE', #8394, #68114 ) ;
#66111 = AXIS2_PLACEMENT_3D ( 'NONE', #19311, #8426, #34814 ) ;
#66112 = PLANE ( 'NONE',  #8435 ) ;
#66113 = DIRECTION ( 'NONE',  ( 1.387778780781445922E-16, -1.000000000000000000, -1.232595164407830946E-32 ) ) ;
#66114 = DIRECTION ( 'NONE',  ( 0.000000000000000000, -1.000000000000000000, 0.000000000000000000 ) ) ;
#66115 = EDGE_CURVE ( 'NONE', #55869, #6058, #60331, .T. ) ;
#66116 = CARTESIAN_POINT ( 'NONE',  ( 437.3372781065084496, 395.0000000000043201, 103.5502958579839259 ) ) ;
#66117 = EDGE_CURVE ( 'NONE', #33721, #59065, #6867, .T. ) ;
#66118 = B_SPLINE_CURVE_WITH_KNOTS ( 'NONE', 3,
 ( #54357, #10767, #54716, #26947, #49432, #38195, #6544, #918, #48725, #32578, #31887, #21668, #37851, #65281, #6184, #38545, #16736, #43461, #54002, #10419, #208, #17076, #5151, #43116, #26608, #59988, #48047, #22367, #27641, #69503, #21323, #43808, #49080, #64941, #1263, #42770, #5494, #22719, #27988, #64237, #32237, #16047, #44157, #15707, #37498 ),
 .UNSPECIFIED., .F., .F.,
 ( 4, 2, 2, 2, 2, 2, 2, 2, 2, 2, 2, 1, 2, 2, 2, 2, 2, 2, 2, 2, 2, 2, 4 ),
 ( 1.440969542111313559E-17, 0.001502898956853370317, 0.002254348435280046584, 0.003005797913706723286, 0.004508696870560116587, 0.005260146348986829284, 0.006011595827413541981, 0.007514494784267002937, 0.009017393741120462158, 0.01052029269797392225, 0.01127174217640064882, 0.01202319165482737540, 0.01277464113325410024, 0.01352609061168082681, 0.01502898956853427996, 0.01578043904696100480, 0.01653188852538773138, 0.01803478748224117759, 0.01953768643909462380, 0.02028913591752134690, 0.02104058539594807348, 0.02254348435280155438, 0.02404638330965503529 ),
 .UNSPECIFIED. ) ;
#66119 = AXIS2_PLACEMENT_3D ( 'NONE', #18746, #28611, #23344 ) ;
#66120 = DIRECTION ( 'NONE',  ( -0.9839295885986321100, 0.1785568947986229116, 0.000000000000000000 ) ) ;
#66121 = ORIENTED_EDGE ( 'NONE', *, *, #39856, .T. ) ;
#66122 = CARTESIAN_POINT ( 'NONE',  ( -107.6591239831840170, 35.59818735115023713, -90.95842461620235042 ) ) ;
#66123 = FACE_OUTER_BOUND ( 'NONE', #60346, .T. ) ;
#66124 = ORIENTED_EDGE ( 'NONE', *, *, #44151, .T. ) ;
#66125 = CARTESIAN_POINT ( 'NONE',  ( 2.051824250824011653, -73.54888393769144272, 73.58025477438755502 ) ) ;
#66126 = LINE ( 'NONE', #69374, #12724 ) ;
#66127 = CYLINDRICAL_SURFACE ( 'NONE', #24131, 7.500000000000020428 ) ;
#66128 = ORIENTED_EDGE ( 'NONE', *, *, #14938, .T. ) ;
#66129 = CARTESIAN_POINT ( 'NONE',  ( -80.54757501605355685, 23.04700348514568020, 45.18237135369550828 ) ) ;
#66130 = CARTESIAN_POINT ( 'NONE',  ( 154.4617654203035784, 56.60942201271839025, -77.35331686145707408 ) ) ;
#66131 = CARTESIAN_POINT ( 'NONE',  ( 46.84154678921878912, 10.51341196666389344, 36.43198548304936679 ) ) ;
#66132 = CARTESIAN_POINT ( 'NONE',  ( -24.41864932425148282, 8.543938959778815345, 67.21142328142714462 ) ) ;
#66133 = ORIENTED_EDGE ( 'NONE', *, *, #46300, .F. ) ;
#66134 = DIRECTION ( 'NONE',  ( -0.1894455408406472141, 0.4181056505533038981, -0.8884244773929820260 ) ) ;
#66135 = CARTESIAN_POINT ( 'NONE',  ( 110.2429982417149574, 29.99119854320846201, 29.61121420573730489 ) ) ;
#66136 = VERTEX_POINT ( 'NONE', #28316 ) ;
#66137 = CARTESIAN_POINT ( 'NONE',  ( 32.89501968360929851, 8.663558833820820482, -12.51357414923122136 ) ) ;
#66138 = DIRECTION ( 'NONE',  ( -0.6579387259397136978, 0.7530714660036099684, 2.500042656554810340E-16 ) ) ;
#66139 = FACE_OUTER_BOUND ( 'NONE', #21685, .T. ) ;
#66140 = CARTESIAN_POINT ( 'NONE',  ( 141.3340962699191437, 47.33011414407334883, 91.38631405835374721 ) ) ;
#66141 = FACE_OUTER_BOUND ( 'NONE', #32904, .T. ) ;
#66142 = PLANE ( 'NONE',  #25936 ) ;
#66143 = ORIENTED_EDGE ( 'NONE', *, *, #51686, .T. ) ;
#66144 = B_SPLINE_CURVE_WITH_KNOTS ( 'NONE', 3,
 ( #21330, #58611, #64246, #37507, #41762, #26275, #15024, #69510, #58960, #52650, #42445, #16404, #10775, #63562, #32247, #37165, #31896, #37861, #59309, #10427, #53680, #53328, #48382, #25932, #11121, #26954, #31549, #58273, #218, #57936, #4474, #47363, #21676, #25601, #32586, #68820, #20641, #47711, #47035, #42102, #68493, #20298, #15372, #36834 ),
 .UNSPECIFIED., .F., .F.,
 ( 4, 2, 2, 2, 2, 2, 2, 2, 2, 2, 2, 2, 2, 2, 2, 2, 2, 2, 2, 2, 2, 4 ),
 ( 0.02814986980477066775, 0.02995274102020799301, 0.03085417662792663829, 0.03175561223564528357, 0.03355848345108266434, 0.03536135466652004511, 0.03716422588195742588, 0.03896709709739480665, 0.03986853270511349356, 0.04076996831283218048, 0.04167140392055087433, 0.04257283952826956125, 0.04347427513598825510, 0.04437571074370694202, 0.04527714635142563587, 0.04617858195914432973, 0.04798145317458170356, 0.04978432439001907739, 0.05158719560545646510, 0.05339006682089383893, 0.05519293803633121970, 0.05699580925176860047 ),
 .UNSPECIFIED. ) ;
#66145 = LINE ( 'NONE', #61193, #40234 ) ;
#66146 = ORIENTED_EDGE ( 'NONE', *, *, #8738, .T. ) ;
#66147 = FACE_BOUND ( 'NONE', #10937, .T. ) ;
#66148 = CARTESIAN_POINT ( 'NONE',  ( 0.000000000000000000, 0.000000000000000000, 85.00000000000000000 ) ) ;
#66149 = CARTESIAN_POINT ( 'NONE',  ( 70.51601918574516503, 14.53832276813545121, 64.39593449160031469 ) ) ;
#66150 = CARTESIAN_POINT ( 'NONE',  ( -126.7183033021620844, 48.24754605562520027, -88.63661005779232482 ) ) ;
#66151 = CARTESIAN_POINT ( 'NONE',  ( 6.837602017663892973, -41.16505738580269735, 13.79046412288134249 ) ) ;
#66152 = VERTEX_POINT ( 'NONE', #29037 ) ;
#66153 = EDGE_CURVE ( 'NONE', #38085, #63883, #1591, .T. ) ;
#66154 = CARTESIAN_POINT ( 'NONE',  ( -125.8938041572051389, -170.0000000000000000, 91.80904905408446837 ) ) ;
#66155 = CARTESIAN_POINT ( 'NONE',  ( 8.288451200428832877, 6.376395059685423305, 38.00660393953555172 ) ) ;
#66156 = ORIENTED_EDGE ( 'NONE', *, *, #47078, .T. ) ;
#66157 = EDGE_CURVE ( 'NONE', #22868, #56240, #55392, .T. ) ;
#66158 = CARTESIAN_POINT ( 'NONE',  ( -62.48965350618345838, 16.80247907725181733, -68.55831454992926410 ) ) ;
#66159 = CARTESIAN_POINT ( 'NONE',  ( 130.9163507021337409, 39.67702886032468967, -90.30179768571910870 ) ) ;
#66160 = VECTOR ( 'NONE', #68788, 1000.000000000000000 ) ;
#66161 = EDGE_LOOP ( 'NONE', ( #64657, #43779, #27602, #40640 ) ) ;
#66162 = CARTESIAN_POINT ( 'NONE',  ( -452.6627218934914367, 399.9999999999998863, -116.4497041420118393 ) ) ;
#66163 = CARTESIAN_POINT ( 'NONE',  ( 94.12811352634520290, 22.11743943276050928, 9.843555910658421837 ) ) ;
#66164 = AXIS2_PLACEMENT_3D ( 'NONE', #45745, #61906, #4899 ) ;
#66165 = DIRECTION ( 'NONE',  ( 1.000000000000000000, -0.000000000000000000, -0.000000000000000000 ) ) ;
#66166 = VERTEX_POINT ( 'NONE', #44850 ) ;
#66167 = CARTESIAN_POINT ( 'NONE',  ( 410.0000000000000000, 190.0000000000000000, -2.000000000000000000 ) ) ;
#66168 = EDGE_CURVE ( 'NONE', #34548, #16719, #66673, .T. ) ;
#66169 = EDGE_CURVE ( 'NONE', #15908, #29791, #61375, .T. ) ;
#66170 = CARTESIAN_POINT ( 'NONE',  ( 68.80707543459442377, 15.13014033538981984, 86.22508746598937535 ) ) ;
#66171 = CARTESIAN_POINT ( 'NONE',  ( 0.000000000000000000, 0.000000000000000000, 380.0000000000000000 ) ) ;
#66172 = CARTESIAN_POINT ( 'NONE',  ( -178.5750994113943761, 94.98114813978523330, -47.38438974541455195 ) ) ;
#66173 = CARTESIAN_POINT ( 'NONE',  ( -179.7387526106833775, 96.39435599882348527, -92.36184407879430580 ) ) ;
#66174 = CARTESIAN_POINT ( 'NONE',  ( -143.3263687017172288, 59.10892259956421668, -91.74752380608748581 ) ) ;
#66175 = DIRECTION ( 'NONE',  ( 0.000000000000000000, 0.000000000000000000, 1.000000000000000000 ) ) ;
#66177 = EDGE_LOOP ( 'NONE', ( #31230, #54653 ) ) ;
#66176 = EDGE_CURVE ( 'NONE', #33459, #14549, #60358, .T. ) ;
#66178 = CYLINDRICAL_SURFACE ( 'NONE', #41054, 7.500000000000013323 ) ;
#66179 = CARTESIAN_POINT ( 'NONE',  ( 11.05669727962760085, 70.00000000000000000, -27.88815958909220782 ) ) ;
#66180 = ORIENTED_EDGE ( 'NONE', *, *, #22710, .F. ) ;
#66181 = EDGE_CURVE ( 'NONE', #62240, #61608, #12415, .T. ) ;
#66182 = CARTESIAN_POINT ( 'NONE',  ( -155.1359377029286009, 70.46175948311802983, -37.33043500810457260 ) ) ;
#66183 = DIRECTION ( 'NONE',  ( -0.000000000000000000, 1.000000000000000000, -0.000000000000000000 ) ) ;
#66184 = CARTESIAN_POINT ( 'NONE',  ( -36.38071096718370967, 11.47804921491337993, 43.37945295078770158 ) ) ;
#66185 = DIRECTION ( 'NONE',  ( 0.000000000000000000, 0.000000000000000000, 1.000000000000000000 ) ) ;
#66186 = PLANE ( 'NONE',  #44491 ) ;
#66187 = CARTESIAN_POINT ( 'NONE',  ( -12.85736381479377499, 7.270939470456537101, -91.02940243108859875 ) ) ;
#66188 = DIRECTION ( 'NONE',  ( -1.000000000000000000, 0.000000000000000000, 0.000000000000000000 ) ) ;
#66189 = PLANE ( 'NONE',  #9216 ) ;
#66190 = CARTESIAN_POINT ( 'NONE',  ( -13.47517652744367034, 8.334971000693560228, 42.57234634832188647 ) ) ;
#66191 = CARTESIAN_POINT ( 'NONE',  ( 111.1767565371974626, 29.31586421952251698, 2.810169317169238568 ) ) ;
#66192 = CARTESIAN_POINT ( 'NONE',  ( -53.37047711001667949, 15.27679796346806640, -89.09340216910368326 ) ) ;
#66193 = ORIENTED_EDGE ( 'NONE', *, *, #43009, .T. ) ;
#66194 = DIRECTION ( 'NONE',  ( 1.000000000000000000, 0.000000000000000000, 0.000000000000000000 ) ) ;
#66195 = ORIENTED_EDGE ( 'NONE', *, *, #61211, .T. ) ;
#66196 = CARTESIAN_POINT ( 'NONE',  ( 41.66904755831208007, -15.55634918610412853, 2.000000000000000000 ) ) ;
#66197 = EDGE_CURVE ( 'NONE', #24194, #11802, #25982, .T. ) ;
#66198 = CARTESIAN_POINT ( 'NONE',  ( 309.8720357909272707, 18.00000000000002842, 256.6193948016162381 ) ) ;
#66199 = CARTESIAN_POINT ( 'NONE',  ( 46.42281973867196854, 9.426811321855158354, 66.90762843771246082 ) ) ;
#66200 = DIRECTION ( 'NONE',  ( 0.000000000000000000, 1.000000000000000000, 0.000000000000000000 ) ) ;
#66201 = LINE ( 'NONE', #23958, #38977 ) ;
#66202 = VECTOR ( 'NONE', #26612, 1000.000000000000000 ) ;
#66203 = ADVANCED_FACE ( 'NONE', ( #8957 ), #51859, .F. ) ;
#66204 = EDGE_CURVE ( 'NONE', #49653, #9355, #25143, .T. ) ;
#66205 = LINE ( 'NONE', #17994, #41150 ) ;
#66206 = CARTESIAN_POINT ( 'NONE',  ( -173.1211646369891355, 87.12891641440857882, -49.71195716475001092 ) ) ;
#66207 = CARTESIAN_POINT ( 'NONE',  ( 39.40195752203891999, 9.424259417798142024, -62.46436805589144114 ) ) ;
#66208 = EDGE_LOOP ( 'NONE', ( #68369, #61626, #43814, #12022 ) ) ;
#66209 = ORIENTED_EDGE ( 'NONE', *, *, #65773, .F. ) ;
#66210 = DIRECTION ( 'NONE',  ( 1.000000000000000000, 0.000000000000000000, 0.000000000000000000 ) ) ;
#66211 = CARTESIAN_POINT ( 'NONE',  ( 178.1999009735082495, 75.73911533785327777, 70.57996378539579041 ) ) ;
#66212 = B_SPLINE_CURVE_WITH_KNOTS ( 'NONE', 3,
 ( #43670, #65147, #46111, #34886, #51409, #19037, #67583, #56324, #40838, #19382, #2520, #55988, #45778, #3220, #62297, #29945, #24677, #45425, #66905, #40491, #35219, #14108, #3550, #51056, #18700, #35570, #57030, #13083, #8845, #61942, #30295, #51744, #50703, #40155, #25021, #23973, #34547, #7802, #29252, #61607, #13422, #8142, #29586 ),
 .UNSPECIFIED., .F., .F.,
 ( 4, 2, 2, 2, 2, 2, 2, 2, 2, 2, 2, 2, 1, 2, 2, 2, 2, 2, 2, 2, 2, 4 ),
 ( 0.02379577142314830140, 0.02527778373276529794, 0.02601878988757378580, 0.02675979604238227366, 0.02824180835199925285, 0.02972382066161623204, 0.03046482681642473031, 0.03120583297123322858, 0.03268784528085023899, 0.03416985759046724247, 0.03565186990008424595, 0.03639287605489275462, 0.03713388220970126330, 0.03787488836450975810, 0.03861589451931826678, 0.04009790682893527719, 0.04157991913855228761, 0.04306193144816929802, 0.04380293760297780670, 0.04454394375778630843, 0.04602595606740331191, 0.04750796837702032926 ),
 .UNSPECIFIED. ) ;
#66213 = DIRECTION ( 'NONE',  ( 1.000000000000000000, 0.000000000000000000, -0.000000000000000000 ) ) ;
#66214 = CARTESIAN_POINT ( 'NONE',  ( -29.55217150403795401, -15.61897105721054757, 6.893342933764143865 ) ) ;
#66215 = CARTESIAN_POINT ( 'NONE',  ( -48.12872802574198516, -43.70867239603780519, 41.38025477438755928 ) ) ;
#66216 = AXIS2_PLACEMENT_3D ( 'NONE', #17561, #49910, #60813 ) ;
#66217 = CARTESIAN_POINT ( 'NONE',  ( -20.00000000000002842, -6.319444444444441089, 4.000000000000000000 ) ) ;
#66218 = ORIENTED_EDGE ( 'NONE', *, *, #48424, .T. ) ;
#66219 = AXIS2_PLACEMENT_3D ( 'NONE', #49132, #39305, #38602 ) ;
#66220 = CARTESIAN_POINT ( 'NONE',  ( 103.8325688302027174, 27.12251147381402561, -47.32372234173669057 ) ) ;
#66221 = CARTESIAN_POINT ( 'NONE',  ( -10.23867141318106100, 7.059827648235816433, 57.34201402450064222 ) ) ;
#66222 = CARTESIAN_POINT ( 'NONE',  ( 14.81290967676421921, 7.477658233646008235, 56.90665333537696569 ) ) ;
#66223 = DIRECTION ( 'NONE',  ( -0.000000000000000000, -0.000000000000000000, -1.000000000000000000 ) ) ;
#66224 = DIRECTION ( 'NONE',  ( 0.7530714660036196273, -0.6579387259397027066, 0.000000000000000000 ) ) ;
#66225 = FACE_BOUND ( 'NONE', #27040, .T. ) ;
#66226 = EDGE_LOOP ( 'NONE', ( #66711, #67935, #33167, #34035 ) ) ;
#66227 = FACE_OUTER_BOUND ( 'NONE', #50971, .T. ) ;
#66228 = DIRECTION ( 'NONE',  ( 0.000000000000000000, -0.9999993111447558203, 0.001173758924898823551 ) ) ;
#66229 = CARTESIAN_POINT ( 'NONE',  ( 0.000000000000000000, 0.000000000000000000, 43.58025477438756212 ) ) ;
#66230 = CARTESIAN_POINT ( 'NONE',  ( -179.5109681715917986, 96.11572638569519711, 7.512143929769561801 ) ) ;
#66231 = CARTESIAN_POINT ( 'NONE',  ( 153.2282895792478996, 54.42637815496157572, 3.875255574263929859 ) ) ;
#66232 = VECTOR ( 'NONE', #4547, 1000.000000000000000 ) ;
#66233 = CARTESIAN_POINT ( 'NONE',  ( 0.000000000000000000, 0.000000000000000000, 170.0000000000000000 ) ) ;
#66234 = ORIENTED_EDGE ( 'NONE', *, *, #25519, .F. ) ;
#66235 = CARTESIAN_POINT ( 'NONE',  ( 58.09607305250594322, 11.58497620657514915, 4.785656767381915699 ) ) ;
#66236 = CARTESIAN_POINT ( 'NONE',  ( -62.15799747763099248, 16.70234469631020247, 62.20972612752362352 ) ) ;
#66237 = VERTEX_POINT ( 'NONE', #19855 ) ;
#66238 = DIRECTION ( 'NONE',  ( 0.000000000000000000, 1.000000000000000000, 0.000000000000000000 ) ) ;
#66239 = EDGE_LOOP ( 'NONE', ( #44700, #843, #20335, #7035 ) ) ;
#66240 = EDGE_CURVE ( 'NONE', #37469, #40902, #57487, .T. ) ;
#66241 = LINE ( 'NONE', #49669, #31910 ) ;
#66242 = CARTESIAN_POINT ( 'NONE',  ( 7.762887554996211747E-14, 46.66904755831208718, 2.000000000000001776 ) ) ;
#66243 = DIRECTION ( 'NONE',  ( -0.000000000000000000, 1.000000000000000000, -0.000000000000000000 ) ) ;
#66244 = EDGE_LOOP ( 'NONE', ( #20109, #40435, #51685, #54956 ) ) ;
#66245 = ORIENTED_EDGE ( 'NONE', *, *, #7211, .T. ) ;
#66246 = CARTESIAN_POINT ( 'NONE',  ( 45.04020069093781586, 10.22779424730543241, 69.22824337619731239 ) ) ;
#66247 = CIRCLE ( 'NONE', #52746, 2.999999999999981792 ) ;
#66248 = FACE_OUTER_BOUND ( 'NONE', #49367, .T. ) ;
#66249 = CARTESIAN_POINT ( 'NONE',  ( -156.9262190792699414, 72.10659547035876926, -68.01882500604709492 ) ) ;
#66250 = CARTESIAN_POINT ( 'NONE',  ( 69.49112875363887554, 15.30845942322121367, 6.676346884528112646 ) ) ;
#66251 = FACE_OUTER_BOUND ( 'NONE', #8220, .T. ) ;
#66252 = ORIENTED_EDGE ( 'NONE', *, *, #14777, .T. ) ;
#66253 = EDGE_CURVE ( 'NONE', #53230, #16637, #2993, .T. ) ;
#66254 = DIRECTION ( 'NONE',  ( 1.000000000000000000, 0.000000000000000000, 0.000000000000000000 ) ) ;
#66255 = CARTESIAN_POINT ( 'NONE',  ( 63.01563776193090405, 13.70579113808098271, -35.72069083216973695 ) ) ;
#66256 = CARTESIAN_POINT ( 'NONE',  ( -131.2955621888335429, 51.38237199780172659, -20.79447557564050797 ) ) ;
#66257 = DIRECTION ( 'NONE',  ( -1.000000000000000000, 0.000000000000000000, 0.000000000000000000 ) ) ;
#66258 = CARTESIAN_POINT ( 'NONE',  ( 114.4640969196985907, 30.88424258798505306, -22.78190138875784143 ) ) ;
#66259 = VECTOR ( 'NONE', #22272, 1000.000000000000000 ) ;
#66260 = EDGE_CURVE ( 'NONE', #55579, #366, #46229, .T. ) ;
#66261 = B_SPLINE_CURVE_WITH_KNOTS ( 'NONE', 3,
 ( #17685, #55657, #50035, #22958, #11695, #1151 ),
 .UNSPECIFIED., .F., .F.,
 ( 4, 2, 4 ),
 ( 2.380731629584203697E-07, 0.002336973833157565510, 0.004673709593152172194 ),
 .UNSPECIFIED. ) ;
#66262 = CARTESIAN_POINT ( 'NONE',  ( 91.48187668755954860, 21.13368548676794845, 85.14416980506385357 ) ) ;
#66264 = EDGE_LOOP ( 'NONE', ( #6088, #50328, #39663, #44208, #10688, #29992, #40818, #67222, #2584, #15042, #11175, #25576, #26749 ) ) ;
#66263 = CARTESIAN_POINT ( 'NONE',  ( -67.57266509268116295, -32.54128043381741975, 0.000000000000000000 ) ) ;
#66265 = ORIENTED_EDGE ( 'NONE', *, *, #31450, .T. ) ;
#66266 = MECHANICAL_DESIGN_GEOMETRIC_PRESENTATION_REPRESENTATION (  '', ( #68453 ), #35918 ) ;
#66267 = EDGE_LOOP ( 'NONE', ( #5872, #65108, #55141, #38880, #49400, #11625, #14606 ) ) ;
#66268 = CARTESIAN_POINT ( 'NONE',  ( -17.89459634713148262, 72.78390022947087346, 41.38025477438755928 ) ) ;
#66269 = CARTESIAN_POINT ( 'NONE',  ( 177.0110682437508274, 75.98481089748381123, 3.650247767581047409 ) ) ;
#66270 = CARTESIAN_POINT ( 'NONE',  ( -50.51700111023805562, 13.51182830536852997, -9.878698120772499536 ) ) ;
#66271 = CARTESIAN_POINT ( 'NONE',  ( 106.6228877857910646, 27.24245963308691998, -9.992007454249797860 ) ) ;
#66272 = CARTESIAN_POINT ( 'NONE',  ( -2.116120943111181152, -74.98056102853681182, 43.58025477438756923 ) ) ;
#66273 = CARTESIAN_POINT ( 'NONE',  ( 211.0188980202574101, 117.2649575585887050, 94.44936189044236130 ) ) ;
#66274 = DIRECTION ( 'NONE',  ( -0.000000000000000000, 1.000000000000000000, -0.000000000000000000 ) ) ;
#66275 = CARTESIAN_POINT ( 'NONE',  ( 21.27121078971612889, 61.42097029141972087, 170.0000000000000000 ) ) ;
#66276 = CARTESIAN_POINT ( 'NONE',  ( 188.9999999999999432, -57.00000000000007816, 72.99999999999998579 ) ) ;
#66277 = ORIENTED_EDGE ( 'NONE', *, *, #44634, .T. ) ;
#66278 = FACE_OUTER_BOUND ( 'NONE', #11258, .T. ) ;
#66279 = ORIENTED_EDGE ( 'NONE', *, *, #46121, .T. ) ;
#66280 = ORIENTED_EDGE ( 'NONE', *, *, #20089, .T. ) ;
#66281 = CARTESIAN_POINT ( 'NONE',  ( 63.49941241090381538, 13.81848793187418245, -23.87614024170608928 ) ) ;
#66282 = CARTESIAN_POINT ( 'NONE',  ( 182.7686108735401262, 81.77235358504609053, -77.89035669591841327 ) ) ;
#66283 = CARTESIAN_POINT ( 'NONE',  ( -167.6566265204789659, 82.70140535081091571, 43.46458241691903623 ) ) ;
#66284 = VECTOR ( 'NONE', #4979, 1000.000000000000114 ) ;
#66285 = CARTESIAN_POINT ( 'NONE',  ( 2.645508037661883360, 7.710219529346608702, -9.431901280394573206 ) ) ;
#66286 = EDGE_CURVE ( 'NONE', #41408, #50492, #68717, .T. ) ;
#66287 = LINE ( 'NONE', #27221, #31504 ) ;
#66288 = CARTESIAN_POINT ( 'NONE',  ( -179.9997297618090784, -170.0000000000000000, 94.99999999999866418 ) ) ;
#66289 = EDGE_CURVE ( 'NONE', #66579, #35686, #54923, .T. ) ;
#66290 = DIRECTION ( 'NONE',  ( -1.000000000000000000, 0.000000000000000000, 0.000000000000000000 ) ) ;
#66291 = ORIENTED_EDGE ( 'NONE', *, *, #1209, .F. ) ;
#66292 = EDGE_LOOP ( 'NONE', ( #62063, #43240, #15568, #3963 ) ) ;
#66293 = EDGE_LOOP ( 'NONE', ( #18056, #11294, #44039, #40414, #31590, #43948, #22792, #26712, #48238 ) ) ;
#66294 = B_SPLINE_CURVE_WITH_KNOTS ( 'NONE', 3,
 ( #66819, #62566, #14379, #13342, #35833, #57286, #23551, #18614, #34799, #56237, #67171, #2781, #18959, #40405, #42810, #9442, #42476, #25632, #46722, #26651, #53017, #53360, #36516, #64278, #41796, #25967, #68195, #31250, #51999, #48086, #69544, #57971, #41455, #21363, #14711, #36865, #20000, #10460, #16086, #25283, #4505, #20331, #62907, #63253 ),
 .UNSPECIFIED., .F., .F.,
 ( 4, 2, 2, 2, 2, 2, 2, 2, 2, 2, 2, 2, 2, 2, 2, 2, 2, 2, 2, 2, 2, 4 ),
 ( 0.02495775893651561508, 0.02650251144344302479, 0.02804726395037043796, 0.02959201645729784766, 0.03113676896422525736, 0.03268152147115267053, 0.03345389772461636324, 0.03422627397808006289, 0.03577102648500746218, 0.03654340273847116877, 0.03731577899193487535, 0.03808815524539857500, 0.03886053149886228159, 0.04040528400578970170, 0.04117766025925340828, 0.04195003651271711487, 0.04349478901964453498, 0.04503954152657195509, 0.04581191778003566861, 0.04658429403349938214, 0.04812904654042685082, 0.04967379904735432644 ),
 .UNSPECIFIED. ) ;
#66295 = DIRECTION ( 'NONE',  ( -0.000000000000000000, 1.000000000000000000, -0.000000000000000000 ) ) ;
#66296 = CARTESIAN_POINT ( 'NONE',  ( -12.39701069459754201, 7.231688578592714300, 4.805392785045681237 ) ) ;
#66297 = DIRECTION ( 'NONE',  ( -1.000000000000000000, 0.000000000000000000, 0.000000000000000000 ) ) ;
#66298 = CARTESIAN_POINT ( 'NONE',  ( 93.23851390434869302, 22.85739692998905070, -93.44079555661757297 ) ) ;
#66299 = UNCERTAINTY_MEASURE_WITH_UNIT (LENGTH_MEASURE( 1.000000000000000082E-05 ), #52001, 'distance_accuracy_value', 'NONE');
#66300 = DIRECTION ( 'NONE',  ( -0.000000000000000000, -0.000000000000000000, -1.000000000000000000 ) ) ;
#66301 = VECTOR ( 'NONE', #21762, 1000.000000000000000 ) ;
#66302 = CARTESIAN_POINT ( 'NONE',  ( 198.8732368717152212, 100.3103976497390875, 68.28400160539764840 ) ) ;
#66303 = VERTEX_POINT ( 'NONE', #11010 ) ;
#66304 = CARTESIAN_POINT ( 'NONE',  ( -57.42826130032241849, 16.37596353166460617, -76.67885148864655775 ) ) ;
#66305 = CARTESIAN_POINT ( 'NONE',  ( 202.7506655727288774, 105.3943386412348815, -63.41604910222725522 ) ) ;
#66306 =( NAMED_UNIT ( * ) PLANE_ANGLE_UNIT ( ) SI_UNIT ( $, .RADIAN. ) );
#66307 = CARTESIAN_POINT ( 'NONE',  ( -180.4654253355437277, 95.69358270527506249, -43.76251724624543726 ) ) ;
#66308 = CARTESIAN_POINT ( 'NONE',  ( -15.55634918610403439, 2.818925648462311528E-14, 85.00100000000000477 ) ) ;
#66309 = CARTESIAN_POINT ( 'NONE',  ( -165.6398193834832000, 79.16932278174806470, 10.86641610212712905 ) ) ;
#66310 = DIRECTION ( 'NONE',  ( -1.000000000000000000, 0.000000000000000000, 0.000000000000000000 ) ) ;
#66311 = FACE_BOUND ( 'NONE', #64192, .T. ) ;
#66312 = CARTESIAN_POINT ( 'NONE',  ( -189.2375912283856394, 107.0871308750787563, 91.70900086444785870 ) ) ;
#66313 = ORIENTED_EDGE ( 'NONE', *, *, #4660, .T. ) ;
#66314 = CARTESIAN_POINT ( 'NONE',  ( 276.2331853604025014, 21.75170065437620437, -3.304351318131944826 ) ) ;
#66315 = CARTESIAN_POINT ( 'NONE',  ( -132.6161619568759420, 51.08240647571223292, -72.59421541500523745 ) ) ;
#66316 = LINE ( 'NONE', #29348, #69089 ) ;
#66317 = PLANE ( 'NONE',  #12115 ) ;
#66318 = AXIS2_PLACEMENT_3D ( 'NONE', #38255, #28051, #44222 ) ;
#66319 = CARTESIAN_POINT ( 'NONE',  ( 157.4703587214989113, 57.65129005721575339, 44.40946747225338953 ) ) ;
#66320 = ORIENTED_EDGE ( 'NONE', *, *, #534, .T. ) ;
#66321 = FACE_OUTER_BOUND ( 'NONE', #33059, .T. ) ;
#66322 = EDGE_CURVE ( 'NONE', #5206, #40354, #7902, .T. ) ;
#66323 = CARTESIAN_POINT ( 'NONE',  ( 187.8308247327058211, 85.70400899947037487, 93.79355304541221017 ) ) ;
#66324 = EDGE_LOOP ( 'NONE', ( #42566, #696, #40005, #53459 ) ) ;
#66325 = ORIENTED_EDGE ( 'NONE', *, *, #42021, .T. ) ;
#66326 = EDGE_CURVE ( 'NONE', #17944, #67205, #35199, .T. ) ;
#66327 = CARTESIAN_POINT ( 'NONE',  ( 176.6214367443247681, 74.20967084876664899, -37.67839354686518760 ) ) ;
#66328 = CARTESIAN_POINT ( 'NONE',  ( -179.2262621278717631, 94.19039042964666919, -64.67118848797289843 ) ) ;
#66329 = CARTESIAN_POINT ( 'NONE',  ( 0.000000000000000000, 0.000000000000000000, 380.0000000000000000 ) ) ;
#66330 = VERTEX_POINT ( 'NONE', #64833 ) ;
#66331 = DIRECTION ( 'NONE',  ( -0.000000000000000000, 1.000000000000000000, -0.000000000000000000 ) ) ;
#66332 = CARTESIAN_POINT ( 'NONE',  ( -180.2244609727085844, 95.39945930389649220, 9.053060466247467630 ) ) ;
#66333 = CARTESIAN_POINT ( 'NONE',  ( 313.9975424824652350, 307.8795515535290974, 6.994434899193393562 ) ) ;
#66334 = CIRCLE ( 'NONE', #43835, 10.00000000000000178 ) ;
#66335 = DIRECTION ( 'NONE',  ( -0.000000000000000000, 1.000000000000000000, -0.000000000000000000 ) ) ;
#66336 = CARTESIAN_POINT ( 'NONE',  ( -29.04400972079232091, 10.22852224114065223, -8.861140687333856292 ) ) ;
#66337 = CARTESIAN_POINT ( 'NONE',  ( -53.14657859411973106, 15.21831473227210374, -8.614006834922252054 ) ) ;
#66338 = EDGE_CURVE ( 'NONE', #4893, #10403, #13527, .T. ) ;
#66339 = ORIENTED_EDGE ( 'NONE', *, *, #27009, .F. ) ;
#66340 = B_SPLINE_CURVE_WITH_KNOTS ( 'NONE', 3,
 ( #44078, #23356, #65929, #11376 ),
 .UNSPECIFIED., .F., .F.,
 ( 4, 4 ),
 ( 9.900409499190005107E-07, 0.05658314289920114010 ),
 .UNSPECIFIED. ) ;
#66341 = CARTESIAN_POINT ( 'NONE',  ( 110.2429982417149432, 28.88204397445229077, -35.92243756565368784 ) ) ;
#66342 = LINE ( 'NONE', #13548, #39282 ) ;
#66343 = EDGE_CURVE ( 'NONE', #52913, #65764, #11621, .T. ) ;
#66344 = CARTESIAN_POINT ( 'NONE',  ( 46.90141780929662474, 9.503798448769774865, -43.62445339352620977 ) ) ;
#66345 = EDGE_CURVE ( 'NONE', #50424, #62726, #2213, .T. ) ;
#66346 = CARTESIAN_POINT ( 'NONE',  ( 414.4083459183745504, 395.0000000000065938, -113.5207719538776843 ) ) ;
#66348 = ORIENTED_EDGE ( 'NONE', *, *, #10065, .F. ) ;
#66347 = CARTESIAN_POINT ( 'NONE',  ( -124.8192061951466485, 45.78944360187998086, 84.36447601993580747 ) ) ;
#66349 = CARTESIAN_POINT ( 'NONE',  ( 79.82127737190242556, 17.20935440217363421, -46.47800199947357669 ) ) ;
#66350 = VECTOR ( 'NONE', #49801, 1000.000000000000000 ) ;
#66351 = ORIENTED_EDGE ( 'NONE', *, *, #40417, .F. ) ;
#66352 = CARTESIAN_POINT ( 'NONE',  ( -126.7989199172159829, 47.09198523267866676, 30.66070955475667148 ) ) ;
#66353 = CARTESIAN_POINT ( 'NONE',  ( 79.54836217416617217, 18.17815803851262402, 34.72743815142386836 ) ) ;
#66354 = CARTESIAN_POINT ( 'NONE',  ( 309.8720357909272707, 172.0000000000000284, 256.6193948016162381 ) ) ;
#66355 = CARTESIAN_POINT ( 'NONE',  ( 35.39413431650373099, 0.000000000000000000, 5.000000000000000000 ) ) ;
#66356 = DIRECTION ( 'NONE',  ( 0.000000000000000000, 0.000000000000000000, -1.000000000000000000 ) ) ;
#66357 = DIRECTION ( 'NONE',  ( -1.000000000000000000, 0.000000000000000000, 0.000000000000000000 ) ) ;
#66358 = CARTESIAN_POINT ( 'NONE',  ( -180.0154536325057109, 96.73346874014735874, -12.40038597180966917 ) ) ;
#66359 = CARTESIAN_POINT ( 'NONE',  ( -417.6627218934913230, 179.4906275429376308, -144.4497041420118819 ) ) ;
#66360 = ORIENTED_EDGE ( 'NONE', *, *, #49927, .F. ) ;
#66361 = ORIENTED_EDGE ( 'NONE', *, *, #31396, .F. ) ;
#66362 = CARTESIAN_POINT ( 'NONE',  ( 39.40195752203892710, 8.409560354027384221, 44.91383430596327742 ) ) ;
#66363 = DIRECTION ( 'NONE',  ( -0.8191520442889916875, 0.000000000000000000, -0.5735764363510462704 ) ) ;
#66364 = CARTESIAN_POINT ( 'NONE',  ( -8.712114576423861223, 23.56346432108866651, 0.000000000000000000 ) ) ;
#66365 = CARTESIAN_POINT ( 'NONE',  ( 208.9583973663597476, 114.1615900753670445, -50.01439015974929703 ) ) ;
#66366 = DIRECTION ( 'NONE',  ( -0.000000000000000000, -0.000000000000000000, -1.000000000000000000 ) ) ;
#66367 = CARTESIAN_POINT ( 'NONE',  ( -109.5025362253418280, 36.60371748273997383, 66.95027869359381612 ) ) ;
#66368 = CARTESIAN_POINT ( 'NONE',  ( -23.93965512371324067, 8.480096402797094868, -43.32224293081845445 ) ) ;
#66369 = EDGE_CURVE ( 'NONE', #65221, #45932, #44413, .T. ) ;
#66370 = DIRECTION ( 'NONE',  ( -1.000000000000000000, 0.000000000000000000, 0.000000000000000000 ) ) ;
#66371 = ORIENTED_EDGE ( 'NONE', *, *, #18423, .F. ) ;
#66372 = ORIENTED_EDGE ( 'NONE', *, *, #22596, .F. ) ;
#66373 = EDGE_LOOP ( 'NONE', ( #68720, #60805, #30432, #924 ) ) ;
#66374 = DIRECTION ( 'NONE',  ( 0.000000000000000000, -0.000000000000000000, 1.000000000000000000 ) ) ;
#66375 = DIRECTION ( 'NONE',  ( 0.000000000000000000, 0.000000000000000000, 1.000000000000000000 ) ) ;
#66376 = CARTESIAN_POINT ( 'NONE',  ( -86.17927900504984962, 25.32700542568493418, 64.77477121631265788 ) ) ;
#66377 = B_SPLINE_CURVE_WITH_KNOTS ( 'NONE', 3,
 ( #48267, #10999, #21549, #32461, #53894, #5716, #27172, #68378, #63092, #38430, #50028, #55649, #54948, #65522, #16959, #28215, #17317, #49316, #59873, #60235, #60581, #1147, #6769, #39474, #11690, #33164, #23313, #43348, #43690, #12049, #27520, #17678, #44040, #66235, #7483, #48607, #12749, #32808, #28575, #39143, #38791, #44760, #445, #22953 ),
 .UNSPECIFIED., .F., .F.,
 ( 4, 2, 2, 2, 2, 2, 2, 2, 2, 2, 2, 2, 2, 2, 2, 2, 2, 2, 2, 2, 2, 4 ),
 ( 1.471961680016038988E-17, 0.001482469635030012013, 0.002223704452545010972, 0.002964939270060010582, 0.004447408905090008933, 0.005929878540120007285, 0.007412348175150002168, 0.008153582992665003512, 0.008894817810180005724, 0.01037728744521001709, 0.01185975708024002845, 0.01260099189775503760, 0.01334222671527004501, 0.01482469635030006158, 0.01556593116781506379, 0.01630716598533006600, 0.01778963562036006349, 0.01927210525539005403, 0.02001334007290505104, 0.02075457489042004805, 0.02223704452545005941, 0.02371951416048007424 ),
 .UNSPECIFIED. ) ;
#66378 = FACE_OUTER_BOUND ( 'NONE', #10236, .T. ) ;
#66379 = LINE ( 'NONE', #39281, #13082 ) ;
#66380 = LINE ( 'NONE', #12903, #23316 ) ;
#66381 = VECTOR ( 'NONE', #28729, 1000.000000000000227 ) ;
#66382 = CARTESIAN_POINT ( 'NONE',  ( -97.86516199987806885, 31.71158167298307617, -21.75180431999427810 ) ) ;
#66383 = CARTESIAN_POINT ( 'NONE',  ( 38.42384008295177722, 8.283891555743466029, 71.71024313779651038 ) ) ;
#66384 = CARTESIAN_POINT ( 'NONE',  ( 32.99392442438140449, 7.662387294680161887, 94.99999999999866418 ) ) ;
#66385 = VECTOR ( 'NONE', #65783, 1000.000000000000114 ) ;
#66386 = DIRECTION ( 'NONE',  ( -0.04486483035050447404, -0.9989930665413151445, 0.000000000000000000 ) ) ;
#66387 = VERTEX_POINT ( 'NONE', #50397 ) ;
#66388 = CARTESIAN_POINT ( 'NONE',  ( 59.94652978725887493, 13.01168383647461546, 71.00508481107152647 ) ) ;
#66389 = DIRECTION ( 'NONE',  ( 0.000000000000000000, 0.000000000000000000, 1.000000000000000000 ) ) ;
#66390 = CARTESIAN_POINT ( 'NONE',  ( -10.24974837193994404, 8.069704751038628388, 17.88514665569731577 ) ) ;
#66391 = DIRECTION ( 'NONE',  ( -1.020422603260505347E-14, 1.000000000000000000, 5.551115123125782702E-17 ) ) ;
#66392 = CARTESIAN_POINT ( 'NONE',  ( 76.57571471437145760, 6.000000000000000000, 0.000000000000000000 ) ) ;
#66393 = AXIS2_PLACEMENT_3D ( 'NONE', #35865, #51696, #2129 ) ;
#66394 = CARTESIAN_POINT ( 'NONE',  ( 126.3580464630938422, 38.22944795020838882, -16.97937654421329867 ) ) ;
#66395 = ORIENTED_EDGE ( 'NONE', *, *, #37299, .F. ) ;
#66396 = AXIS2_PLACEMENT_3D ( 'NONE', #17102, #33317, #31923 ) ;
#66397 = CARTESIAN_POINT ( 'NONE',  ( -189.2346268516247392, 107.0830361517165130, -15.05455062662797339 ) ) ;
#66398 = CARTESIAN_POINT ( 'NONE',  ( -33.38294402636582703, 10.93918551420889784, -35.55683350427927536 ) ) ;
#66399 = CARTESIAN_POINT ( 'NONE',  ( -8.000000000000000000, -4.618802153517023612, -9.500000000000000000 ) ) ;
#66400 = EDGE_CURVE ( 'NONE', #45368, #23473, #33869, .T. ) ;
#66401 = CONTEXT_DEPENDENT_SHAPE_REPRESENTATION ( #26030, #5678 ) ;
#66402 = CARTESIAN_POINT ( 'NONE',  ( -165.9814687844695129, 79.51750121246506353, 94.33608907707005642 ) ) ;
#66403 = VERTEX_POINT ( 'NONE', #55311 ) ;
#66404 = CARTESIAN_POINT ( 'NONE',  ( 40.13282190615316836, 1.842283050316774879E-12, 5.000000000000000000 ) ) ;
#66405 = CARTESIAN_POINT ( 'NONE',  ( -143.2471548081023229, 59.04577938365769540, -19.63009637662464613 ) ) ;
#66406 = ADVANCED_FACE ( 'NONE', ( #11351 ), #16973, .T. ) ;
#66407 = DIRECTION ( 'NONE',  ( 0.000000000000000000, 0.000000000000000000, 1.000000000000000000 ) ) ;
#66408 = EDGE_CURVE ( 'NONE', #16482, #55258, #59883, .T. ) ;
#66409 = DIRECTION ( 'NONE',  ( 0.000000000000000000, 0.000000000000000000, 1.000000000000000000 ) ) ;
#66410 = EDGE_LOOP ( 'NONE', ( #43199, #17894, #51266, #3658 ) ) ;
#66411 = DIRECTION ( 'NONE',  ( -0.000000000000000000, -0.000000000000000000, -1.000000000000000000 ) ) ;
#66412 = CARTESIAN_POINT ( 'NONE',  ( 412.3372781065085633, 179.4906275429376024, -146.4497041420117682 ) ) ;
#66413 = ADVANCED_FACE ( 'NONE', ( #66248 ), #6779, .T. ) ;
#66414 = CARTESIAN_POINT ( 'NONE',  ( -149.5074843970971017, 65.50121172469319220, 30.72082123989904545 ) ) ;
#66415 = CARTESIAN_POINT ( 'NONE',  ( 19.53470118933706701, 6.649487981843462236, -49.52081999872682161 ) ) ;
#66417 = EDGE_LOOP ( 'NONE', ( #28495, #23004, #52535, #63011 ) ) ;
#66416 = CARTESIAN_POINT ( 'NONE',  ( 116.9197133427647231, 33.22079464767577406, 6.812707058480746092 ) ) ;
#66418 = CARTESIAN_POINT ( 'NONE',  ( 60.62939143133408493, 12.13148391928981162, 30.18601119527468413 ) ) ;
#66419 = ORIENTED_EDGE ( 'NONE', *, *, #13497, .F. ) ;
#66420 = ORIENTED_EDGE ( 'NONE', *, *, #21836, .F. ) ;
#66421 = FACE_OUTER_BOUND ( 'NONE', #42766, .T. ) ;
#66422 = ADVANCED_FACE ( 'NONE', ( #68310 ), #56022, .T. ) ;
#66423 = LINE ( 'NONE', #65010, #28190 ) ;
#66424 = EDGE_CURVE ( 'NONE', #12796, #18218, #14146, .T. ) ;
#66426 = VERTEX_POINT ( 'NONE', #41226 ) ;
#66425 = CARTESIAN_POINT ( 'NONE',  ( -13.45956523846224684, 8.333781915634247639, -74.71914061966306519 ) ) ;
#66427 = DIRECTION ( 'NONE',  ( -1.156482317317871725E-15, 0.000000000000000000, -1.000000000000000000 ) ) ;
#66428 = AXIS2_PLACEMENT_3D ( 'NONE', #17662, #18349, #61265 ) ;
#66429 = CARTESIAN_POINT ( 'NONE',  ( 183.2136430849847955, 6.000000000000000000, -41.68900338898720292 ) ) ;
#66430 = CARTESIAN_POINT ( 'NONE',  ( -71.17984086584780812, 20.67393782512344558, -42.10050417024042702 ) ) ;
#66431 = ORIENTED_EDGE ( 'NONE', *, *, #1876, .T. ) ;
#66432 = CONICAL_SURFACE ( 'NONE', #68649, 8.000000000000001776, 1.047197551196595855 ) ;
#66433 = CARTESIAN_POINT ( 'NONE',  ( -2.000000000000000000, -2.000000000000000000, 378.0000000000000000 ) ) ;
#66434 = VECTOR ( 'NONE', #39845, 1000.000000000000000 ) ;
#66435 = AXIS2_PLACEMENT_3D ( 'NONE', #21194, #20841, #42640 ) ;
#66436 = CARTESIAN_POINT ( 'NONE',  ( 139.6326990672751549, 46.22017155708127945, 32.21984060566606445 ) ) ;
#66437 = CARTESIAN_POINT ( 'NONE',  ( -178.5848962563134137, 94.99295350784005620, 43.48377260447168879 ) ) ;
#66438 = CARTESIAN_POINT ( 'NONE',  ( 313.9975424824652350, 296.0000000000000000, 418.0000000000000000 ) ) ;
#66439 = CARTESIAN_POINT ( 'NONE',  ( 17.72748965151694023, 7.577488030789626627, 71.60839833991708758 ) ) ;
#66440 = VERTEX_POINT ( 'NONE', #9212 ) ;
#66441 = ORIENTED_EDGE ( 'NONE', *, *, #34961, .F. ) ;
#66442 = VERTEX_POINT ( 'NONE', #62687 ) ;
#66443 = VECTOR ( 'NONE', #45571, 1000.000000000000000 ) ;
#66444 = CARTESIAN_POINT ( 'NONE',  ( 211.5877208647112866, 116.2968205280715637, -94.50629413778540311 ) ) ;
#66445 = CARTESIAN_POINT ( 'NONE',  ( -32.41627406084105445, 9.753381371531506971, -35.36528594626865640 ) ) ;
#66446 = CARTESIAN_POINT ( 'NONE',  ( -95.42918619675315028, 29.43458666617156183, 88.58648633754481239 ) ) ;
#66447 = CARTESIAN_POINT ( 'NONE',  ( -142.0081215801269821, 58.07066293384867350, 37.92100431141785322 ) ) ;
#66448 = CARTESIAN_POINT ( 'NONE',  ( -133.1527834403229917, 51.46311219732124442, 66.86934462543963775 ) ) ;
#66449 = CARTESIAN_POINT ( 'NONE',  ( -75.65611349188964141, 22.26947559308020175, -22.64443753553979377 ) ) ;
#66450 = ORIENTED_EDGE ( 'NONE', *, *, #67137, .F. ) ;
#66451 = CARTESIAN_POINT ( 'NONE',  ( 86.62931800182293784, 19.42108912189599579, 71.55663816294304524 ) ) ;
#66452 = ORIENTED_EDGE ( 'NONE', *, *, #62806, .F. ) ;
#66453 = CARTESIAN_POINT ( 'NONE',  ( -94.91535552559176381, 30.30508792700360488, -94.76622093189627094 ) ) ;
#66454 = CARTESIAN_POINT ( 'NONE',  ( 184.3994103300443612, 82.02159554764421046, 43.55099592434475397 ) ) ;
#66455 = CARTESIAN_POINT ( 'NONE',  ( 26.11269837220803325, -15.55634918610409656, 85.00100000000000477 ) ) ;
#66456 = PLANE ( 'NONE',  #19207 ) ;
#66457 = DIRECTION ( 'NONE',  ( 1.000000000000000000, 0.000000000000000000, 0.000000000000000000 ) ) ;
#66458 = CARTESIAN_POINT ( 'NONE',  ( -10.23531775138760835, 8.068923942586303966, -50.02458151933852548 ) ) ;
#66459 = CARTESIAN_POINT ( 'NONE',  ( 442.3372781065084496, 390.0000000000043201, 108.5502958579838690 ) ) ;
#66460 = CARTESIAN_POINT ( 'NONE',  ( 111.9975424824652634, 20.00000000000003197, 401.6295345748407613 ) ) ;
#66461 = EDGE_LOOP ( 'NONE', ( #45453, #66209, #59137, #65449 ) ) ;
#66462 = CARTESIAN_POINT ( 'NONE',  ( -106.6583005646425732, 35.06113698500919895, -90.11032198025695550 ) ) ;
#66463 = ORIENTED_EDGE ( 'NONE', *, *, #55018, .F. ) ;
#66464 = DIRECTION ( 'NONE',  ( 0.000000000000000000, 0.000000000000000000, 1.000000000000000000 ) ) ;
#66465 = CARTESIAN_POINT ( 'NONE',  ( -31.90315521289150524, 56.64813493366005304, 170.0000000000000000 ) ) ;
#66466 = FACE_OUTER_BOUND ( 'NONE', #20669, .T. ) ;
#66467 = ORIENTED_EDGE ( 'NONE', *, *, #7047, .T. ) ;
#66468 = DIRECTION ( 'NONE',  ( -0.000000000000000000, -0.000000000000000000, -1.000000000000000000 ) ) ;
#66469 = CARTESIAN_POINT ( 'NONE',  ( -11.57931195747592312, 7.164335452024273465, -63.25124850868342463 ) ) ;
#66470 = CARTESIAN_POINT ( 'NONE',  ( -36.37663950036512261, 10.45389057208229033, 43.38300827802142834 ) ) ;
#66471 = CARTESIAN_POINT ( 'NONE',  ( 139.3067271572849677, 44.81402783181199823, -38.36495864216608709 ) ) ;
#66472 = ORIENTED_EDGE ( 'NONE', *, *, #19769, .T. ) ;
#66473 = VECTOR ( 'NONE', #6751, 1000.000000000000000 ) ;
#66474 = CARTESIAN_POINT ( 'NONE',  ( 418.1699113293248615, 221.5915846175138313, 697.9565308668837815 ) ) ;
#66475 = LINE ( 'NONE', #22845, #35722 ) ;
#66476 = VERTEX_POINT ( 'NONE', #3936 ) ;
#66477 = CARTESIAN_POINT ( 'NONE',  ( 35.44311777160621091, 8.940232499250166498, -9.900466562469301124 ) ) ;
#66478 = DIRECTION ( 'NONE',  ( 1.000000000000000000, 2.465190328815661345E-32, 0.000000000000000000 ) ) ;
#66479 = CIRCLE ( 'NONE', #30504, 242.4895526022646379 ) ;
#66480 = CARTESIAN_POINT ( 'NONE',  ( -1.327237339235001645, 7.561837009978233048, 68.21302253756950051 ) ) ;
#66481 = PRODUCT ( 'Bush', 'Bush', '', ( #32882 ) ) ;
#66482 = CARTESIAN_POINT ( 'NONE',  ( 0.000000000000000000, -31.50328976398030534, -5.000000000000000000 ) ) ;
#66483 = EDGE_CURVE ( 'NONE', #12851, #63560, #19766, .T. ) ;
#66484 = AXIS2_PLACEMENT_3D ( 'NONE', #27987, #50149, #60351 ) ;
#66486 = COLOUR_RGB ( '',0.7921568627450980005, 0.8196078431372548767, 0.9333333333333333481 ) ;
#66485 = DIRECTION ( 'NONE',  ( -0.000000000000000000, 1.000000000000000000, -0.000000000000000000 ) ) ;
#66487 = CARTESIAN_POINT ( 'NONE',  ( -124.3331814159187303, 45.47486189329072914, -76.59758970666941025 ) ) ;
#66488 = ORIENTED_EDGE ( 'NONE', *, *, #36205, .T. ) ;
#66489 = CARTESIAN_POINT ( 'NONE',  ( 162.0835148203877054, 61.32844276806160622, -22.71226385295197048 ) ) ;
#66490 = DIRECTION ( 'NONE',  ( 0.000000000000000000, 0.000000000000000000, -1.000000000000000000 ) ) ;
#66491 = LINE ( 'NONE', #39739, #20707 ) ;
#66492 = DIRECTION ( 'NONE',  ( -0.8345732537213079727, 0.5508969814520945363, 5.102127870520021999E-18 ) ) ;
#66493 = EDGE_CURVE ( 'NONE', #27445, #39748, #50732, .T. ) ;
#66494 = LINE ( 'NONE', #28848, #40851 ) ;
#66495 = VECTOR ( 'NONE', #5758, 1000.000000000000000 ) ;
#66496 = VERTEX_POINT ( 'NONE', #18729 ) ;
#66497 = LINE ( 'NONE', #50638, #2509 ) ;
#66498 = CARTESIAN_POINT ( 'NONE',  ( -149.5074843970971301, -170.0000000000000000, 38.22082123989905966 ) ) ;
#66499 = ORIENTED_EDGE ( 'NONE', *, *, #24472, .T. ) ;
#66500 = CARTESIAN_POINT ( 'NONE',  ( 66.73467315386237431, 14.60276727483218018, 70.68858689679898077 ) ) ;
#66501 = CARTESIAN_POINT ( 'NONE',  ( 1.118033988749894458, 0.000000000000000000, 0.000000000000000000 ) ) ;
#66502 = EDGE_CURVE ( 'NONE', #9869, #45363, #33611, .T. ) ;
#66503 = EDGE_LOOP ( 'NONE', ( #68629, #58282, #17723, #5004 ) ) ;
#66504 = CARTESIAN_POINT ( 'NONE',  ( 163.2911130186310800, 63.63047778106600560, -38.88797379336740789 ) ) ;
#66505 = CARTESIAN_POINT ( 'NONE',  ( 444.9999999999999432, -35.00000000000000000, 0.000000000000000000 ) ) ;
#66506 = CARTESIAN_POINT ( 'NONE',  ( 157.4703587214989113, 57.65129005721575339, -36.12418429913763163 ) ) ;
#66507 = EDGE_LOOP ( 'NONE', ( #60201, #67559, #56491, #36023 ) ) ;
#66508 = CARTESIAN_POINT ( 'NONE',  ( -71.96466849523049802, -21.15771699337099321, 170.0000000000000000 ) ) ;
#66509 = CARTESIAN_POINT ( 'NONE',  ( 70.52174251456412435, 15.58109049973242932, 90.85735943127390613 ) ) ;
#66510 = CARTESIAN_POINT ( 'NONE',  ( 32.03384598935271299, 8.576372641735984459, 38.87696540156872516 ) ) ;
#66511 = CARTESIAN_POINT ( 'NONE',  ( -175.1895962157336726, 90.99110972060687175, -49.43342400943532766 ) ) ;
#66512 = CARTESIAN_POINT ( 'NONE',  ( -131.7724154034330297, 50.48821165954356616, -10.90495122044228182 ) ) ;
#66513 = CARTESIAN_POINT ( 'NONE',  ( 152.3102623290679674, 53.74757787434987222, 69.20218478440308729 ) ) ;
#66514 =( REPRESENTATION_RELATIONSHIP ('NONE','NONE', #40274, #50551 ) REPRESENTATION_RELATIONSHIP_WITH_TRANSFORMATION ( #11496 )SHAPE_REPRESENTATION_RELATIONSHIP( ) );
#66515 = CARTESIAN_POINT ( 'NONE',  ( 129.4987365823222092, 38.85470922756775281, -76.47662530583420448 ) ) ;
#66516 = ORIENTED_EDGE ( 'NONE', *, *, #16349, .T. ) ;
#66517 = CARTESIAN_POINT ( 'NONE',  ( 137.4031600461560458, 44.79620770172218869, -76.98055282418557965 ) ) ;
#66518 = CARTESIAN_POINT ( 'NONE',  ( -13.45956523846224684, 8.333781915634252968, 59.50361233265537919 ) ) ;
#66519 = ORIENTED_EDGE ( 'NONE', *, *, #34022, .T. ) ;
#66520 = VECTOR ( 'NONE', #65429, 1000.000000000000000 ) ;
#66521 = CARTESIAN_POINT ( 'NONE',  ( -152.9143627383494959, 68.46626892668653852, -35.61578214405540876 ) ) ;
#66522 = DIRECTION ( 'NONE',  ( -1.000000000000000000, 0.000000000000000000, 0.000000000000000000 ) ) ;
#66523 =( NAMED_UNIT ( * ) PLANE_ANGLE_UNIT ( ) SI_UNIT ( $, .RADIAN. ) );
#66524 = AXIS2_PLACEMENT_3D ( 'NONE', #39756, #13037, #34500 ) ;
#66525 = CARTESIAN_POINT ( 'NONE',  ( -123.6618353044033967, 46.23845779494347852, -49.58867574490025731 ) ) ;
#66526 = CARTESIAN_POINT ( 'NONE',  ( -6.125624616441582404, 7.794071945221087816, 44.92450289403895169 ) ) ;
#66527 = DIRECTION ( 'NONE',  ( 1.000000000000000000, 0.000000000000000000, 0.000000000000000000 ) ) ;
#66528 = CARTESIAN_POINT ( 'NONE',  ( -47.68743014591520080, 12.82957810971108259, -68.08236959171381386 ) ) ;
#66529 = CARTESIAN_POINT ( 'NONE',  ( -1.455067768715152310, 7.566780179921178906, -12.10745439085062714 ) ) ;
#66531 = CARTESIAN_POINT ( 'NONE',  ( -11.78188048797445475, 8.190559674012726887, 31.23928352507218165 ) ) ;
#66530 = CIRCLE ( 'NONE', #54126, 65.00000000000000000 ) ;
#66532 = AXIS2_PLACEMENT_3D ( 'NONE', #1757, #8067, #39045 ) ;
#66533 = CARTESIAN_POINT ( 'NONE',  ( 112.5554747942045992, 29.96654954475020460, 3.128152278745223835 ) ) ;
#66534 = EDGE_LOOP ( 'NONE', ( #69357, #4692 ) ) ;
#66535 = CARTESIAN_POINT ( 'NONE',  ( -95.05323930133205579, 30.36974142673411592, -40.44390620904788136 ) ) ;
#66536 = EDGE_LOOP ( 'NONE', ( #38867, #53896, #12338, #66991, #53056, #59035, #62845, #31774, #14786 ) ) ;
#66537 = CARTESIAN_POINT ( 'NONE',  ( 105.4375968828853587, 26.72149058755206141, -64.50356492661067875 ) ) ;
#66538 = AXIS2_PLACEMENT_3D ( 'NONE', #25321, #21399, #42844 ) ;
#66539 = CARTESIAN_POINT ( 'NONE',  ( 39.89582146299186860, 9.488756994579086168, -8.775266874964069430 ) ) ;
#66540 = CARTESIAN_POINT ( 'NONE',  ( 43.97326221476411945, 9.047815246749991047, 70.22452885316067750 ) ) ;
#66541 = DIRECTION ( 'NONE',  ( -0.000000000000000000, -0.000000000000000000, -1.000000000000000000 ) ) ;
#66542 = CARTESIAN_POINT ( 'NONE',  ( 10.55634918610409656, 31.11269837220803325, 2.000000000000001776 ) ) ;
#66543 = CLOSED_SHELL ( 'NONE', ( #151, #56880, #43562, #8432, #14504, #53655, #53321, #35433, #21837, #49864, #35900, #30612, #34740, #24889, #3254, #66732, #47374, #8359, #56388, #29235, #68693, #51545, #38501, #42473, #6410, #40362, #9353, #24314 ) ) ;
#66544 = DIRECTION ( 'NONE',  ( 0.000000000000000000, 0.000000000000000000, 1.000000000000000000 ) ) ;
#66545 = EDGE_CURVE ( 'NONE', #49086, #20757, #15005, .T. ) ;
#66546 = FACE_OUTER_BOUND ( 'NONE', #26760, .T. ) ;
#66547 = CARTESIAN_POINT ( 'NONE',  ( -166.3175803736862690, 79.86140754556167565, 68.33441179371222063 ) ) ;
#66548 = VERTEX_POINT ( 'NONE', #3251 ) ;
#66549 = VERTEX_POINT ( 'NONE', #51440 ) ;
#66550 = FACE_OUTER_BOUND ( 'NONE', #57204, .T. ) ;
#66551 = CARTESIAN_POINT ( 'NONE',  ( 174.9053416555736646, 72.57849647436444229, 59.37145172503423396 ) ) ;
#66552 = CARTESIAN_POINT ( 'NONE',  ( -46.66904755831210139, 6.635317295611287136E-14, 2.000000000000001776 ) ) ;
#66553 = ADVANCED_FACE ( 'NONE', ( #24364 ), #61973, .F. ) ;
#66554 = CARTESIAN_POINT ( 'NONE',  ( 107.9342863085848165, 28.93180871323605885, 56.80434494465688999 ) ) ;
#66555 = CARTESIAN_POINT ( 'NONE',  ( -169.1122507277982834, 84.24359299875007423, -21.72154401521961020 ) ) ;
#66556 = DIRECTION ( 'NONE',  ( -0.000000000000000000, 1.000000000000000000, -0.000000000000000000 ) ) ;
#66557 = ORIENTED_EDGE ( 'NONE', *, *, #13276, .T. ) ;
#66558 = CARTESIAN_POINT ( 'NONE',  ( 104.3759779378692656, 27.35691041569132764, -38.72384540243022144 ) ) ;
#66559 = CARTESIAN_POINT ( 'NONE',  ( 17.72748965151693312, 7.577488030789625739, -35.76980402193765940 ) ) ;
#66560 = PLANE ( 'NONE',  #66428 ) ;
#66561 = DIRECTION ( 'NONE',  ( 1.000000000000000000, -0.000000000000000000, 0.000000000000000000 ) ) ;
#66562 = CARTESIAN_POINT ( 'NONE',  ( 424.8372781065089612, 400.0000000000066507, 91.05029585798857283 ) ) ;
#66563 = FACE_BOUND ( 'NONE', #52324, .T. ) ;
#66564 = ADVANCED_FACE ( 'NONE', ( #24712 ), #46145, .T. ) ;
#66565 = EDGE_CURVE ( 'NONE', #4587, #61856, #6780, .T. ) ;
#66566 = ORIENTED_EDGE ( 'NONE', *, *, #50161, .F. ) ;
#66567 = DIRECTION ( 'NONE',  ( 1.000000000000000000, 0.000000000000000000, 0.000000000000000000 ) ) ;
#66568 = FACE_OUTER_BOUND ( 'NONE', #52490, .T. ) ;
#66569 = AXIS2_PLACEMENT_3D ( 'NONE', #46303, #14991, #3750 ) ;
#66570 = CARTESIAN_POINT ( 'NONE',  ( 32.03384598935269878, 8.576372641736000446, -68.50123696028599340 ) ) ;
#66571 = DIRECTION ( 'NONE',  ( 0.000000000000000000, 0.000000000000000000, 1.000000000000000000 ) ) ;
#66572 = ADVANCED_FACE ( 'NONE', ( #51778 ), #3584, .T. ) ;
#66573 = CARTESIAN_POINT ( 'NONE',  ( 208.0306608271317543, 112.7988899307265598, 56.83016791471741413 ) ) ;
#66574 = CARTESIAN_POINT ( 'NONE',  ( 81.76092782665035941, 17.81692437267514251, -64.45568945875886868 ) ) ;
#66575 = VECTOR ( 'NONE', #49520, 1000.000000000000000 ) ;
#66576 = ORIENTED_EDGE ( 'NONE', *, *, #57130, .F. ) ;
#66577 = CARTESIAN_POINT ( 'NONE',  ( 149.4165763529819344, 225.8585178651493663, 138.9999999999999716 ) ) ;
#66578 = CARTESIAN_POINT ( 'NONE',  ( -36.11269837220804391, 15.55634918610408945, 2.000000000000001776 ) ) ;
#66579 = VERTEX_POINT ( 'NONE', #68968 ) ;
#66580 = VECTOR ( 'NONE', #44963, 1000.000000000000000 ) ;
#66581 = LINE ( 'NONE', #2895, #57621 ) ;
#66582 = ORIENTED_EDGE ( 'NONE', *, *, #61298, .F. ) ;
#66583 = CARTESIAN_POINT ( 'NONE',  ( -85.75222301046100881, 25.14826148333819944, -66.95125014471969394 ) ) ;
#66584 = FACE_OUTER_BOUND ( 'NONE', #15475, .T. ) ;
#66586 = ORIENTED_EDGE ( 'NONE', *, *, #60925, .T. ) ;
#66585 = EDGE_CURVE ( 'NONE', #48880, #68633, #25117, .T. ) ;
#66587 = ORIENTED_EDGE ( 'NONE', *, *, #55662, .T. ) ;
#66588 = DIRECTION ( 'NONE',  ( -0.9839295885986295565, -0.1785568947986370392, 0.000000000000000000 ) ) ;
#66589 = EDGE_CURVE ( 'NONE', #34631, #44954, #32044, .T. ) ;
#66591 = EDGE_CURVE ( 'NONE', #18335, #56454, #48196, .T. ) ;
#66590 = CARTESIAN_POINT ( 'NONE',  ( 164.8433205901838789, 64.93586312665799198, 38.31213353503791552 ) ) ;
#66592 = CARTESIAN_POINT ( 'NONE',  ( 107.0447263249840972, 28.53200276018955250, 17.05477231794132109 ) ) ;
#66593 = VERTEX_POINT ( 'NONE', #5642 ) ;
#66594 = DIRECTION ( 'NONE',  ( 0.000000000000000000, 0.000000000000000000, 1.000000000000000000 ) ) ;
#66595 = CARTESIAN_POINT ( 'NONE',  ( -47.56466076048272384, 13.83435953640667293, 10.48194178115690534 ) ) ;
#66596 = CARTESIAN_POINT ( 'NONE',  ( -129.4036885357273547, 50.06837984316181434, -8.937056684793262207 ) ) ;
#66597 = CARTESIAN_POINT ( 'NONE',  ( -152.2894885175273032, 67.91392929472267781, -89.02504389548720098 ) ) ;
#66598 = LINE ( 'NONE', #18386, #66434 ) ;
#66599 = CARTESIAN_POINT ( 'NONE',  ( 78.57571471437144339, 6.000000000000000000, -30.00000000000000355 ) ) ;
#66601 = ORIENTED_EDGE ( 'NONE', *, *, #7857, .F. ) ;
#66600 = DIRECTION ( 'NONE',  ( -0.000000000000000000, 1.000000000000000000, -0.000000000000000000 ) ) ;
#66602 = ORIENTED_EDGE ( 'NONE', *, *, #28194, .F. ) ;
#66603 = VERTEX_POINT ( 'NONE', #16204 ) ;
#66604 = LINE ( 'NONE', #3265, #35824 ) ;
#66605 = CARTESIAN_POINT ( 'NONE',  ( 179.0091171455098333, 77.94933395983137814, 2.743929071994786639 ) ) ;
#66606 = CARTESIAN_POINT ( 'NONE',  ( 0.4964154566687647985, -4.996589667937445078, -7.345652830558659474 ) ) ;
#66607 = DIRECTION ( 'NONE',  ( -1.000000000000000000, 0.000000000000000000, 0.000000000000000000 ) ) ;
#66608 = PLANE ( 'NONE',  #52775 ) ;
#66609 = CARTESIAN_POINT ( 'NONE',  ( 199.7415218581341776, 101.4249224381273535, 84.75794127139820944 ) ) ;
#66610 = DIRECTION ( 'NONE',  ( -0.000000000000000000, -0.000000000000000000, 1.000000000000000000 ) ) ;
#66611 = CARTESIAN_POINT ( 'NONE',  ( -73.81689110552358102, 20.53332132481498817, -75.18638386565793041 ) ) ;
#66612 = CARTESIAN_POINT ( 'NONE',  ( -62.97854483871554976, -16.08424353203763957, 40.00000000000003553 ) ) ;
#66613 = ORIENTED_EDGE ( 'NONE', *, *, #23919, .T. ) ;
#66614 = CARTESIAN_POINT ( 'NONE',  ( 0.000000000000000000, 0.000000000000000000, 170.0000000000000000 ) ) ;
#66615 = ORIENTED_EDGE ( 'NONE', *, *, #4518, .T. ) ;
#66616 = VERTEX_POINT ( 'NONE', #37655 ) ;
#66617 = CARTESIAN_POINT ( 'NONE',  ( -439.4229916354183274, 394.9999999999998295, 96.05029585798874336 ) ) ;
#66618 = CARTESIAN_POINT ( 'NONE',  ( 188.4365915667138722, 87.87248959723055464, -69.06054871186299238 ) ) ;
#66619 = CARTESIAN_POINT ( 'NONE',  ( -38.80556650104458072, 11.94251439360623124, 89.95992065018027972 ) ) ;
#66620 = CARTESIAN_POINT ( 'NONE',  ( -99.11448999425216755, 31.20120877265620507, -49.32994709144890066 ) ) ;
#66621 = CARTESIAN_POINT ( 'NONE',  ( -102.2801239173131052, 32.78103895658058065, 3.674523915951417141 ) ) ;
#66622 = DIRECTION ( 'NONE',  ( 1.000000000000000000, 0.000000000000000000, 0.000000000000000000 ) ) ;
#66623 = CARTESIAN_POINT ( 'NONE',  ( 137.5911612413395630, 44.91497189902067788, -10.17040840536950341 ) ) ;
#66624 = ORIENTED_EDGE ( 'NONE', *, *, #25721, .F. ) ;
#66625 = ORIENTED_EDGE ( 'NONE', *, *, #1020, .T. ) ;
#66626 = CIRCLE ( 'NONE', #23929, 65.36598343705435354 ) ;
#66627 = ADVANCED_FACE ( 'NONE', ( #59108 ), #10920, .T. ) ;
#66628 = CARTESIAN_POINT ( 'NONE',  ( 187.4794072207230897, 86.81249290409115815, 94.43195144249413886 ) ) ;
#66629 = CARTESIAN_POINT ( 'NONE',  ( -24.87827947785777383, -3.494138152041991408, 3.061616997868437868E-16 ) ) ;
#66630 = CARTESIAN_POINT ( 'NONE',  ( -27.38060184144623221, 26.82905581235131010, 13.32819299319723250 ) ) ;
#66631 = CARTESIAN_POINT ( 'NONE',  ( 56.66775172211441003, 11.28938863449062069, -12.37422088483766736 ) ) ;
#66632 = VECTOR ( 'NONE', #21938, 1000.000000000000114 ) ;
#66633 = CARTESIAN_POINT ( 'NONE',  ( -445.5916540816260749, 394.9999999999953957, 106.4792280461270479 ) ) ;
#66634 = CARTESIAN_POINT ( 'NONE',  ( -8.000000000000000000, -4.618802153517024500, -8.785468820183664818 ) ) ;
#66635 = ORIENTED_EDGE ( 'NONE', *, *, #35023, .T. ) ;
#66636 = CARTESIAN_POINT ( 'NONE',  ( 42.03719354205841086, 9.783015072457470040, -62.93830268630524927 ) ) ;
#66637 = PLANE ( 'NONE',  #50317 ) ;
#66638 = CARTESIAN_POINT ( 'NONE',  ( 197.9868529032976312, 99.18611233336802968, -74.03116428711561525 ) ) ;
#66639 = DIRECTION ( 'NONE',  ( -0.1948620228302647139, 0.9808306643139259595, 2.366582715663035416E-30 ) ) ;
#66640 = CARTESIAN_POINT ( 'NONE',  ( -174.7869898116916545, 88.99756909636809610, -34.85054195857060222 ) ) ;
#66641 =( LENGTH_UNIT ( ) NAMED_UNIT ( * ) SI_UNIT ( .MILLI., .METRE. ) );
#66642 = CARTESIAN_POINT ( 'NONE',  ( -167.9889421625799741, 81.59140042431232587, 5.987724995526459537 ) ) ;
#66643 = DIRECTION ( 'NONE',  ( 0.000000000000000000, 6.405132834375902056E-16, -1.000000000000000000 ) ) ;
#66644 = FACE_BOUND ( 'NONE', #14424, .T. ) ;
#66645 = ADVANCED_FACE ( 'NONE', ( #57748 ), #33085, .F. ) ;
#66646 = CARTESIAN_POINT ( 'NONE',  ( -25.87147652227456263, 70.00000000000000000, 77.58025477438755502 ) ) ;
#66647 = EDGE_CURVE ( 'NONE', #58514, #59754, #44685, .T. ) ;
#66648 = ADVANCED_FACE ( 'NONE', ( #27443 ), #38354, .T. ) ;
#66649 = CARTESIAN_POINT ( 'NONE',  ( -99.01681023176691099, 31.15382287136410966, -89.44744109731372816 ) ) ;
#66650 = EDGE_CURVE ( 'NONE', #17510, #1454, #21821, .T. ) ;
#66651 = VERTEX_POINT ( 'NONE', #65807 ) ;
#66652 = B_SPLINE_CURVE_WITH_KNOTS ( 'NONE', 3,
 ( #65121, #48218, #59822, #54547, #10950, #48913, #60537, #751, #21849, #16917, #43293, #11637, #38737, #32068, #1099, #27123, #60181, #59477, #26792, #43 ),
 .UNSPECIFIED., .F., .F.,
 ( 4, 2, 2, 2, 2, 2, 2, 2, 2, 4 ),
 ( 0.000000000000000000, 0.001349456565742324261, 0.002024184848613473382, 0.002698913131484622502, 0.004048369697226901660, 0.005397826262969181686, 0.006747282828711460845, 0.008096739394453740871, 0.009446195960196020897, 0.01079565252593830092 ),
 .UNSPECIFIED. ) ;
#66653 = CYLINDRICAL_SURFACE ( 'NONE', #58597, 5.000000000000004441 ) ;
#66654 = CARTESIAN_POINT ( 'NONE',  ( 150.5538013146980632, 53.70974888488129295, 66.66635342088143545 ) ) ;
#66655 = DIRECTION ( 'NONE',  ( 0.000000000000000000, 1.000000000000000000, 0.000000000000000000 ) ) ;
#66656 = DIRECTION ( 'NONE',  ( 0.5508969814520944253, 0.8345732537213078617, 0.000000000000000000 ) ) ;
#66657 = CARTESIAN_POINT ( 'NONE',  ( -63.00000000000000000, 0.000000000000000000, 40.82842712474622004 ) ) ;
#66658 = ORIENTED_EDGE ( 'NONE', *, *, #17306, .F. ) ;
#66659 = CARTESIAN_POINT ( 'NONE',  ( -127.9486647835774420, 47.86116766339740991, -88.87777986370316796 ) ) ;
#66660 = CARTESIAN_POINT ( 'NONE',  ( -7.825402957745085430, -170.0000000000000000, -50.41807073194384259 ) ) ;
#66661 = ORIENTED_EDGE ( 'NONE', *, *, #58572, .T. ) ;
#66662 = ORIENTED_EDGE ( 'NONE', *, *, #40444, .F. ) ;
#66663 = AXIS2_PLACEMENT_3D ( 'NONE', #61765, #13591, #2691 ) ;
#66664 = CARTESIAN_POINT ( 'NONE',  ( 10.55634918610411432, 46.66904755831205875, 2.000000000000001776 ) ) ;
#66665 = CARTESIAN_POINT ( 'NONE',  ( 150.0516754638056511, 53.34587188591232376, 35.77407304044231751 ) ) ;
#66666 = CARTESIAN_POINT ( 'NONE',  ( -20.00000000000002842, 3.680555555555560243, 0.000000000000000000 ) ) ;
#66667 = ORIENTED_EDGE ( 'NONE', *, *, #5444, .T. ) ;
#66668 = CARTESIAN_POINT ( 'NONE',  ( 116.6681538161788723, 33.09439081574001307, 60.05510480527172490 ) ) ;
#66669 = LINE ( 'NONE', #35339, #41242 ) ;
#66670 = CARTESIAN_POINT ( 'NONE',  ( -0.3747453031323939587, 6.520267647591904137, 9.782624009045733260 ) ) ;
#66671 = AXIS2_PLACEMENT_3D ( 'NONE', #3278, #7251, #19797 ) ;
#66672 = EDGE_CURVE ( 'NONE', #33798, #42059, #27581, .T. ) ;
#66674 = EDGE_CURVE ( 'NONE', #68287, #59320, #40182, .T. ) ;
#66673 = LINE ( 'NONE', #34309, #24773 ) ;
#66675 = CARTESIAN_POINT ( 'NONE',  ( -25.07901552294942960, 9.649193085547777216, -11.99012566281456493 ) ) ;
#66676 = VECTOR ( 'NONE', #25615, 1000.000000000000114 ) ;
#66677 = CARTESIAN_POINT ( 'NONE',  ( 5.000000000000000888, 0.000000000000000000, -9.500000000000000000 ) ) ;
#66678 = EDGE_CURVE ( 'NONE', #29753, #47253, #46404, .T. ) ;
#66679 = ORIENTED_EDGE ( 'NONE', *, *, #56060, .T. ) ;
#66680 = VECTOR ( 'NONE', #17118, 1000.000000000000000 ) ;
#66681 = CARTESIAN_POINT ( 'NONE',  ( 117.6916924104495479, 32.48309187151379973, -42.40661573811005525 ) ) ;
#66682 = VECTOR ( 'NONE', #51072, 1000.000000000000000 ) ;
#66683 = CARTESIAN_POINT ( 'NONE',  ( -75.43271753227891452, 22.18711452892411629, 17.85784068024286952 ) ) ;
#66684 = CARTESIAN_POINT ( 'NONE',  ( 46.13320811200731697, 9.380653113584038749, -46.46381765439975453 ) ) ;
#66685 = CARTESIAN_POINT ( 'NONE',  ( -169.8885678771097787, 85.07765565657315676, -75.83859972875634980 ) ) ;
#66687 = ORIENTED_EDGE ( 'NONE', *, *, #58801, .T. ) ;
#66686 = CARTESIAN_POINT ( 'NONE',  ( 70.65683382808232693, -25.18281821780010787, 43.58025477438756923 ) ) ;
#66688 = DIRECTION ( 'NONE',  ( 0.9989930665413151445, -0.04486483035050447404, 2.500042656554809354E-16 ) ) ;
#66689 = VECTOR ( 'NONE', #17449, 1000.000000000000000 ) ;
#66690 = VERTEX_POINT ( 'NONE', #62606 ) ;
#66691 = CARTESIAN_POINT ( 'NONE',  ( 44.99999999999997158, 22.99999999999998579, 0.000000000000000000 ) ) ;
#66692 = DIRECTION ( 'NONE',  ( 1.000000000000000000, 0.000000000000000000, 0.000000000000000000 ) ) ;
#66693 = CARTESIAN_POINT ( 'NONE',  ( 209.3223706822284100, 0.000000000000000000, 276.7520087653757628 ) ) ;
#66694 = FACE_OUTER_BOUND ( 'NONE', #64595, .T. ) ;
#66695 = CARTESIAN_POINT ( 'NONE',  ( 141.0804878838241336, 45.96076546397618756, -14.59318871261416284 ) ) ;
#66696 = CARTESIAN_POINT ( 'NONE',  ( 41.66904755831208007, -15.55634918610412853, 85.00100000000000477 ) ) ;
#66697 = CARTESIAN_POINT ( 'NONE',  ( 15.78827728214693416, 7.507518794609596924, -89.20804527961313113 ) ) ;
#66698 = CARTESIAN_POINT ( 'NONE',  ( -152.2964402771108894, 66.58174574061953876, -35.34709794641883462 ) ) ;
#66699 = EDGE_LOOP ( 'NONE', ( #1378, #38996, #2968, #7237 ) ) ;
#66700 = ORIENTED_EDGE ( 'NONE', *, *, #20562, .T. ) ;
#66701 = CARTESIAN_POINT ( 'NONE',  ( 106.6192711434718916, 27.24117154335862523, 57.38488479179707724 ) ) ;
#66702 = CARTESIAN_POINT ( 'NONE',  ( 309.8720357909272707, 18.00000000000002842, 536.6193948016162949 ) ) ;
#66703 = CARTESIAN_POINT ( 'NONE',  ( 47.70222499156757578, 57.81185381817647340, 41.38025477438755928 ) ) ;
#66704 = CARTESIAN_POINT ( 'NONE',  ( 67.55134213333076332, 13.77030723107740684, -22.36941340431874892 ) ) ;
#66705 = DIRECTION ( 'NONE',  ( 0.000000000000000000, 0.000000000000000000, -1.000000000000000000 ) ) ;
#66706 = CARTESIAN_POINT ( 'NONE',  ( -109.3432140528234697, 36.51591785955880454, 67.43805915958625974 ) ) ;
#66707 = DIRECTION ( 'NONE',  ( -0.000000000000000000, 1.000000000000000000, -0.000000000000000000 ) ) ;
#66708 = CARTESIAN_POINT ( 'NONE',  ( 2.905661822261151883E-14, 15.55634918610403084, 85.00100000000000477 ) ) ;
#66709 = ORIENTED_EDGE ( 'NONE', *, *, #14595, .F. ) ;
#66710 = ORIENTED_EDGE ( 'NONE', *, *, #34346, .F. ) ;
#66711 = ORIENTED_EDGE ( 'NONE', *, *, #13298, .T. ) ;
#66712 = CYLINDRICAL_SURFACE ( 'NONE', #29647, 7.500000000000020428 ) ;
#66713 = EDGE_CURVE ( 'NONE', #67398, #17316, #8088, .T. ) ;
#66714 = VECTOR ( 'NONE', #65869, 1000.000000000000000 ) ;
#66715 = CARTESIAN_POINT ( 'NONE',  ( -74.08448404088061068, 20.62888684035922893, 85.66122281550805440 ) ) ;
#66716 = CARTESIAN_POINT ( 'NONE',  ( 125.2194818923508848, 188.0000000000000000, -91.27944787107685443 ) ) ;
#66717 = CARTESIAN_POINT ( 'NONE',  ( -452.6627218934860366, 395.0000000000064801, -123.9497041420121235 ) ) ;
#66718 = DIRECTION ( 'NONE',  ( 0.4338837391175526248, 0.9009688679024218105, -0.000000000000000000 ) ) ;
#66719 = DIRECTION ( 'NONE',  ( -0.000000000000000000, 1.000000000000000000, -0.000000000000000000 ) ) ;
#66720 = PRESENTATION_LAYER_ASSIGNMENT (  '', '', ( #25141 ) ) ;
#66721 = LINE ( 'NONE', #24501, #4553 ) ;
#66722 = VECTOR ( 'NONE', #24332, 1000.000000000000000 ) ;
#66723 = CARTESIAN_POINT ( 'NONE',  ( 62.52762183777209515, 13.59210632617625336, 44.81296093922131263 ) ) ;
#66724 = CARTESIAN_POINT ( 'NONE',  ( 32.03309158115232691, 7.565157987341259549, 92.53824449203030156 ) ) ;
#66725 = DIRECTION ( 'NONE',  ( 1.000000000000000000, 0.000000000000000000, 0.000000000000000000 ) ) ;
#66726 = ORIENTED_EDGE ( 'NONE', *, *, #63546, .T. ) ;
#66727 = CARTESIAN_POINT ( 'NONE',  ( -40.99999999999997868, 0.000000000000000000, -6.071532165918823253E-15 ) ) ;
#66728 = CARTESIAN_POINT ( 'NONE',  ( 39.99999999999997158, 29.79383981485516131, -25.00000000000000000 ) ) ;
#66729 = CARTESIAN_POINT ( 'NONE',  ( -11.57950265606958062, 8.174070387114795722, 17.26848926542448126 ) ) ;
#66730 = AXIS2_PLACEMENT_3D ( 'NONE', #38932, #60379, #12194 ) ;
#66731 = CARTESIAN_POINT ( 'NONE',  ( -143.3925773749111841, 59.16144459815139101, 15.72631132447487445 ) ) ;
#66732 = ADVANCED_FACE ( 'NONE', ( #56979, #29537 ), #40785, .T. ) ;
#66733 = CARTESIAN_POINT ( 'NONE',  ( -62.41990535723909517, 16.78139727964023109, -95.00000000000133582 ) ) ;
#66734 = CARTESIAN_POINT ( 'NONE',  ( -109.6660553119434951, 36.69391917620600907, -68.03064822489363905 ) ) ;
#66735 = VECTOR ( 'NONE', #61953, 1000.000000000000000 ) ;
#66736 = CARTESIAN_POINT ( 'NONE',  ( 133.8566784816069060, 42.60093787723653236, -24.17876034193199786 ) ) ;
#66737 = CIRCLE ( 'NONE', #36383, 243.4957430088094839 ) ;
#66738 = EDGE_CURVE ( 'NONE', #69500, #52338, #67884, .T. ) ;
#66739 = EDGE_CURVE ( 'NONE', #43408, #51452, #64245, .T. ) ;
#66740 = VERTEX_POINT ( 'NONE', #51357 ) ;
#66742 = AXIS2_PLACEMENT_3D ( 'NONE', #33040, #60110, #54831 ) ;
#66741 = CARTESIAN_POINT ( 'NONE',  ( 596.8022745978502144, 845.2615548154176395, 694.5068267248691427 ) ) ;
#66743 = CARTESIAN_POINT ( 'NONE',  ( -189.7987719395349302, 107.8653664616570751, -12.38560667400269466 ) ) ;
#66744 = LINE ( 'NONE', #1656, #6176 ) ;
#66745 = LINE ( 'NONE', #66399, #37957 ) ;
#66746 = EDGE_CURVE ( 'NONE', #51430, #19186, #24280, .T. ) ;
#66747 = ORIENTED_EDGE ( 'NONE', *, *, #20562, .F. ) ;
#66748 = CARTESIAN_POINT ( 'NONE',  ( -121.1775535805057018, 43.46577565517551278, -36.56175226999291539 ) ) ;
#66749 = DIRECTION ( 'NONE',  ( -1.000000000000000000, 0.000000000000000000, 0.000000000000000000 ) ) ;
#66750 = CARTESIAN_POINT ( 'NONE',  ( -0.5658006089934851657, 7.533733779014712084, -71.70916268580941733 ) ) ;
#66751 = CARTESIAN_POINT ( 'NONE',  ( 150.9302598651331664, 53.98378566185801475, 86.91002861488426845 ) ) ;
#66752 = VERTEX_POINT ( 'NONE', #57319 ) ;
#66753 = CARTESIAN_POINT ( 'NONE',  ( 159.9814610548901328, 60.91953805293818647, -90.23667429834375753 ) ) ;
#66754 = CARTESIAN_POINT ( 'NONE',  ( 0.000000000000000000, 0.000000000000000000, 41.38025477438755928 ) ) ;
#66755 = CARTESIAN_POINT ( 'NONE',  ( -156.4966862384868875, 71.70877417666513054, 40.99359700224837155 ) ) ;
#66756 = CARTESIAN_POINT ( 'NONE',  ( 266.9165763529819628, -52.00000000000000711, 108.9999999999999858 ) ) ;
#66758 = VERTEX_POINT ( 'NONE', #3169 ) ;
#66757 = CARTESIAN_POINT ( 'NONE',  ( -78.66644367742111399, -170.0000000000000000, -23.27090004125422595 ) ) ;
#66759 = B_SPLINE_CURVE_WITH_KNOTS ( 'NONE', 3,
 ( #283, #49501, #1339, #55137, #10844, #59373, #60066, #12246, #22442, #66078, #6258, #59027, #17868, #32649, #27360, #6962, #33709, #49155, #16473, #38623, #44233, #644, #28412, #32315, #48802, #22096, #17148, #17507, #49862, #48448, #11185, #53743, #5900, #43190, #43538, #54793, #11525, #22793, #54433, #16808, #37927, #5565, #27019, #38267 ),
 .UNSPECIFIED., .F., .F.,
 ( 4, 2, 2, 2, 2, 2, 2, 2, 2, 2, 2, 2, 2, 2, 2, 2, 2, 2, 2, 2, 2, 4 ),
 ( 0.02638217555535139758, 0.02805347641364865779, 0.02972477727194591801, 0.03139607813024317823, 0.03306737898854043844, 0.03390302941768908590, 0.03473867984683773336, 0.03640998070513500051, 0.03724563113428361327, 0.03808128156343221909, 0.03891693199258083186, 0.03975258242172943768, 0.04058823285087805044, 0.04142388328002666320, 0.04225953370917527596, 0.04309518413832388872, 0.04476648499662110037, 0.04643778585491830507, 0.04810908671321550978, 0.04978038757151272142, 0.05145168842980993307, 0.05312298928810713777 ),
 .UNSPECIFIED. ) ;
#66760 = EDGE_CURVE ( 'NONE', #17378, #14449, #67627, .T. ) ;
#66761 = CARTESIAN_POINT ( 'NONE',  ( 55.51547041749726219, 11.05727559334826715, 37.07079845792744521 ) ) ;
#66762 = ORIENTED_EDGE ( 'NONE', *, *, #43755, .F. ) ;
#66763 = ORIENTED_EDGE ( 'NONE', *, *, #34722, .T. ) ;
#66764 = CARTESIAN_POINT ( 'NONE',  ( 173.7263186949344060, 72.85225335320953377, 35.32616919366697772 ) ) ;
#66765 = VECTOR ( 'NONE', #25505, 1000.000000000000114 ) ;
#66766 = B_SPLINE_CURVE_WITH_KNOTS ( 'NONE', 3,
 ( #11687, #39472, #60233, #28213 ),
 .UNSPECIFIED., .F., .F.,
 ( 4, 4 ),
 ( 9.900409499052487190E-07, 0.05658314289920111928 ),
 .UNSPECIFIED. ) ;
#66767 = CARTESIAN_POINT ( 'NONE',  ( 22.89234820949994287, 6.832052815347871899, -72.28072174863926591 ) ) ;
#66768 = CIRCLE ( 'NONE', #8313, 24.99999999999985434 ) ;
#66770 = ORIENTED_EDGE ( 'NONE', *, *, #55836, .T. ) ;
#66769 = CARTESIAN_POINT ( 'NONE',  ( -9.779603649692306888, 8.034615131607074190, -62.50484457767164770 ) ) ;
#66771 = DIRECTION ( 'NONE',  ( -1.000000000000000000, -0.000000000000000000, 1.156482317317871725E-15 ) ) ;
#66772 = LINE ( 'NONE', #20534, #9366 ) ;
#66773 = FACE_BOUND ( 'NONE', #55379, .T. ) ;
#66774 = CIRCLE ( 'NONE', #39793, 99.99999999999994316 ) ;
#66775 = VERTEX_POINT ( 'NONE', #14413 ) ;
#66776 = CARTESIAN_POINT ( 'NONE',  ( 176.7247530015161772, 75.70727164389336394, -91.29928768740779788 ) ) ;
#66777 = VECTOR ( 'NONE', #60550, 1000.000000000000114 ) ;
#66778 = CONICAL_SURFACE ( 'NONE', #25204, 73.43826238111391547, 0.6747409422235518539 ) ;
#66779 = CARTESIAN_POINT ( 'NONE',  ( 139.6150621148398443, 46.20856238844174158, 41.84163371379585783 ) ) ;
#66780 = CARTESIAN_POINT ( 'NONE',  ( 116.6436511186860798, 33.08230081168869674, 41.02847515960270641 ) ) ;
#66781 = VECTOR ( 'NONE', #47421, 1000.000000000000000 ) ;
#66782 = CARTESIAN_POINT ( 'NONE',  ( 130.7260570116704343, 40.73146260246713268, 70.68603471735700339 ) ) ;
#66783 = CARTESIAN_POINT ( 'NONE',  ( 21.74799039132243905, 7.772294950329605712, 68.93910645723609321 ) ) ;
#66784 = EDGE_LOOP ( 'NONE', ( #42246, #31327, #55881, #61636 ) ) ;
#66785 = ORIENTED_EDGE ( 'NONE', *, *, #42769, .T. ) ;
#66786 = EDGE_LOOP ( 'NONE', ( #41562, #61638, #45001, #37051 ) ) ;
#66787 = DIRECTION ( 'NONE',  ( -0.7071067811865485719, 8.659560562354946417E-17, 0.7071067811865465735 ) ) ;
#66788 = EDGE_CURVE ( 'NONE', #19234, #67613, #24954, .T. ) ;
#66789 = DIRECTION ( 'NONE',  ( 0.000000000000000000, 0.000000000000000000, 1.000000000000000000 ) ) ;
#66790 = CARTESIAN_POINT ( 'NONE',  ( -96.26904753919785662, 29.83064565795647027, 87.21136816703879902 ) ) ;
#66791 = DIRECTION ( 'NONE',  ( 0.000000000000000000, 1.000000000000000000, -0.000000000000000000 ) ) ;
#66792 = ADVANCED_FACE ( 'NONE', ( #24629 ), #40105, .T. ) ;
#66793 = DIRECTION ( 'NONE',  ( 0.000000000000000000, 0.000000000000000000, -1.000000000000000000 ) ) ;
#66794 = CARTESIAN_POINT ( 'NONE',  ( -71.15374617000809110, 20.66492714610672721, -15.76073736046750717 ) ) ;
#66796 = ORIENTED_EDGE ( 'NONE', *, *, #15404, .T. ) ;
#66795 = EDGE_CURVE ( 'NONE', #32221, #38399, #35164, .T. ) ;
#66797 = CARTESIAN_POINT ( 'NONE',  ( -102.2801239173131052, 33.91021738430207932, 30.51907450641510522 ) ) ;
#66798 = ORIENTED_EDGE ( 'NONE', *, *, #32481, .T. ) ;
#66799 = CARTESIAN_POINT ( 'NONE',  ( 0.000000000000000000, 0.000000000000000000, 41.38025477438755928 ) ) ;
#66800 = ADVANCED_FACE ( 'NONE', ( #46064 ), #8444, .F. ) ;
#66801 = DIRECTION ( 'NONE',  ( 1.000000000000000000, 3.108624468950438313E-14, 0.000000000000000000 ) ) ;
#66802 = ORIENTED_EDGE ( 'NONE', *, *, #17219, .F. ) ;
#66803 = CARTESIAN_POINT ( 'NONE',  ( 36.64089410029568228, 65.45232906116417837, 170.0000000000000000 ) ) ;
#66804 = CARTESIAN_POINT ( 'NONE',  ( -60.41792053122248518, -24.01035990323518376, 0.000000000000000000 ) ) ;
#66805 = SURFACE_STYLE_USAGE ( .BOTH. , #61160 ) ;
#66806 = LINE ( 'NONE', #23187, #34537 ) ;
#66807 = CARTESIAN_POINT ( 'NONE',  ( -8.800520192024523070, 7.964629484975262130, -50.37068912721758096 ) ) ;
#66808 = CARTESIAN_POINT ( 'NONE',  ( 151.7819978880463623, 53.35998893001568177, -48.51851982015085696 ) ) ;
#66809 = ORIENTED_EDGE ( 'NONE', *, *, #37677, .F. ) ;
#66810 = DIRECTION ( 'NONE',  ( -1.000000000000000000, 0.000000000000000000, -0.000000000000000000 ) ) ;
#66811 = CARTESIAN_POINT ( 'NONE',  ( -430.1627218934916073, 394.9999999999998295, 91.05029585798840230 ) ) ;
#66812 = VERTEX_POINT ( 'NONE', #8796 ) ;
#66813 = LINE ( 'NONE', #57627, #14884 ) ;
#66814 = DIRECTION ( 'NONE',  ( 0.4738686624730094610, -0.8805955318567321166, 0.000000000000000000 ) ) ;
#66815 = DIRECTION ( 'NONE',  ( 0.000000000000000000, 0.000000000000000000, -1.000000000000000000 ) ) ;
#66816 = VERTEX_POINT ( 'NONE', #23582 ) ;
#66817 = DIRECTION ( 'NONE',  ( -0.000000000000000000, -0.000000000000000000, -1.000000000000000000 ) ) ;
#66818 = CARTESIAN_POINT ( 'NONE',  ( 156.5890478960376413, 58.24007662587944623, -63.00753038278813989 ) ) ;
#66819 = CARTESIAN_POINT ( 'NONE',  ( -102.2801239173131052, 32.78103895658057354, -23.17002667451225406 ) ) ;
#66820 = CARTESIAN_POINT ( 'NONE',  ( -31.43908319763710679, 9.591432048623762086, 72.06100499665289760 ) ) ;
#66821 = AXIS2_PLACEMENT_3D ( 'NONE', #52568, #20217, #41673 ) ;
#66822 = EDGE_CURVE ( 'NONE', #64820, #14003, #20454, .T. ) ;
#66823 = ADVANCED_FACE ( 'NONE', ( #40443 ), #2816, .F. ) ;
#66824 = ORIENTED_EDGE ( 'NONE', *, *, #38999, .F. ) ;
#66825 = CARTESIAN_POINT ( 'NONE',  ( -118.4622862908119032, 41.79153065058248018, 39.16645702020448994 ) ) ;
#66826 = ORIENTED_EDGE ( 'NONE', *, *, #37636, .T. ) ;
#66827 = LINE ( 'NONE', #22847, #42478 ) ;
#66828 = CARTESIAN_POINT ( 'NONE',  ( 182.5617509987553433, 80.11195108039726165, 2.607952352358541948 ) ) ;
#66829 = VECTOR ( 'NONE', #35311, 1000.000000000000000 ) ;
#66830 = CARTESIAN_POINT ( 'NONE',  ( -6.125624616441583292, 7.794071945221086040, 18.07995230357528982 ) ) ;
#66831 = PLANE ( 'NONE',  #18408 ) ;
#66832 = AXIS2_PLACEMENT_3D ( 'NONE', #50530, #44558, #8319 ) ;
#66833 = B_SPLINE_CURVE_WITH_KNOTS ( 'NONE', 3,
 ( #25981, #31947, #59691, #32633, #43170, #37910, #64646, #54059, #4519, #59010, #36883, #69559, #5546, #42823, #27001, #59356, #5885, #58318, #10827, #48430, #5209, #266, #69220, #38248, #47414, #10137, #68868, #27343, #48781, #26665, #32294, #31265, #48101, #52693, #20691, #21722, #21380, #22077, #53725, #43518, #64997, #16790, #42151, #63613, #4860, #15423, #42495, #31595, #53035, #26326, #21047, #63951, #37210, #58660, #53377, #38964, #18542, #49485, #28044, #44922 ),
 .UNSPECIFIED., .F., .F.,
 ( 4, 2, 2, 2, 2, 2, 2, 2, 2, 2, 2, 2, 2, 2, 2, 2, 2, 2, 2, 2, 2, 2, 2, 2, 2, 2, 2, 2, 2, 4 ),
 ( 0.000000000000000000, 0.001056649052740852267, 0.002113298105481704534, 0.003169947158222556367, 0.003698271684592982500, 0.004226596210963409067, 0.005283245263704308171, 0.006339894316445206408, 0.007396543369186105513, 0.008453192421927005484, 0.01056649052740882798, 0.01162313958014971234, 0.01267978863289059670, 0.01479308673837232031, 0.01690638484385404566, 0.01796303389659492308, 0.01901968294933580050, 0.02113298105481760739, 0.02218963010755855073, 0.02324627916029949753, 0.02535957726578140156, 0.02641622631852235531, 0.02747287537126330906, 0.02852952442400426281, 0.02958617347674521655, 0.03011449800311571598, 0.03064282252948621887, 0.03169947158222722466, 0.03275612063496822352, 0.03381276968770922930 ),
 .UNSPECIFIED. ) ;
#66834 = CARTESIAN_POINT ( 'NONE',  ( -60.41792053122281914, 24.01035990323430624, 170.0000000000000000 ) ) ;
#66835 = VECTOR ( 'NONE', #67108, 1000.000000000000000 ) ;
#66836 = DIRECTION ( 'NONE',  ( 1.000000000000000000, 0.000000000000000000, 0.000000000000000000 ) ) ;
#66837 = CIRCLE ( 'NONE', #54383, 23.50000000000000000 ) ;
#66838 = DIRECTION ( 'NONE',  ( 1.000000000000000000, 0.000000000000000000, 0.000000000000000000 ) ) ;
#66839 = ORIENTED_EDGE ( 'NONE', *, *, #8191, .F. ) ;
#66840 = PLANE ( 'NONE',  #24420 ) ;
#66841 = CARTESIAN_POINT ( 'NONE',  ( 1.118033988749894458, 0.000000000000000000, 0.000000000000000000 ) ) ;
#66842 = CARTESIAN_POINT ( 'NONE',  ( 70.02892116572940040, 14.40944430928137088, 66.82692659502507126 ) ) ;
#66843 = CARTESIAN_POINT ( 'NONE',  ( 139.6359093656973869, 45.02518919224744565, -65.58120096399879628 ) ) ;
#66844 = DIRECTION ( 'NONE',  ( 0.000000000000000000, 0.000000000000000000, -1.000000000000000000 ) ) ;
#66845 = VERTEX_POINT ( 'NONE', #29203 ) ;
#66846 = DIRECTION ( 'NONE',  ( -0.000000000000000000, 1.000000000000000000, -0.000000000000000000 ) ) ;
#66847 = DIRECTION ( 'NONE',  ( 1.000000000000000000, 0.000000000000000000, 0.000000000000000000 ) ) ;
#66848 = ORIENTED_EDGE ( 'NONE', *, *, #25030, .F. ) ;
#66849 = DIRECTION ( 'NONE',  ( 0.4738686624730094610, -0.8805955318567321166, 0.000000000000000000 ) ) ;
#66850 = CARTESIAN_POINT ( 'NONE',  ( 25.57615740168605711, -44.89060284968904568, 26.66469066592268433 ) ) ;
#66851 = ORIENTED_EDGE ( 'NONE', *, *, #21265, .T. ) ;
#66852 = CARTESIAN_POINT ( 'NONE',  ( 164.4761273435911733, 64.62485394454745347, -46.35385866967215662 ) ) ;
#66853 = CYLINDRICAL_SURFACE ( 'NONE', #42577, 7.500000000000020428 ) ;
#66854 = DIRECTION ( 'NONE',  ( -1.000000000000000000, -0.000000000000000000, -0.000000000000000000 ) ) ;
#66855 = CARTESIAN_POINT ( 'NONE',  ( 158.3604774538084712, 58.34594647925807465, -36.16383203810991631 ) ) ;
#66856 = EDGE_LOOP ( 'NONE', ( #52086, #62619 ) ) ;
#66857 = CARTESIAN_POINT ( 'NONE',  ( -95.52093927227215886, 30.58993121475387866, 14.43474828004453236 ) ) ;
#66858 = CARTESIAN_POINT ( 'NONE',  ( 63.69010119909405887, 13.86368654881940188, 83.52517702392452748 ) ) ;
#66859 = DIRECTION ( 'NONE',  ( -0.000000000000000000, -0.000000000000000000, -1.000000000000000000 ) ) ;
#66860 = AXIS2_PLACEMENT_3D ( 'NONE', #26874, #7523, #18757 ) ;
#66861 = CARTESIAN_POINT ( 'NONE',  ( 84.72546926745363294, 19.84015517905183401, -9.206688192610737786 ) ) ;
#66862 = CARTESIAN_POINT ( 'NONE',  ( -126.3508039230932525, 46.79479538767115798, -8.069153307770244865 ) ) ;
#66863 = CARTESIAN_POINT ( 'NONE',  ( 37.36156881963844256, 9.166256500377349070, -89.57976542891690031 ) ) ;
#66864 = CARTESIAN_POINT ( 'NONE',  ( 129.6961120139403363, 38.96846414226715893, -76.61255697058514613 ) ) ;
#66865 = ORIENTED_EDGE ( 'NONE', *, *, #59715, .F. ) ;
#66866 = DIRECTION ( 'NONE',  ( 0.000000000000000000, 0.000000000000000000, 1.000000000000000000 ) ) ;
#66867 = CARTESIAN_POINT ( 'NONE',  ( -15.13464256769235838, 8.488509377255649468, 66.15861208254587211 ) ) ;
#66868 = ORIENTED_EDGE ( 'NONE', *, *, #19067, .F. ) ;
#66869 = VECTOR ( 'NONE', #299, 1000.000000000000000 ) ;
#66870 = CARTESIAN_POINT ( 'NONE',  ( -152.2873556200145231, 67.91256772393731467, -49.28212837332362284 ) ) ;
#66871 = CARTESIAN_POINT ( 'NONE',  ( 207.8407634284390895, 112.5209879629463927, -10.15859321470372123 ) ) ;
#66872 = AXIS2_PLACEMENT_3D ( 'NONE', #32497, #42699, #53588 ) ;
#66873 = CARTESIAN_POINT ( 'NONE',  ( -35.99414836699284592, 11.40630460607620478, 31.73781940164764492 ) ) ;
#66874 = DIRECTION ( 'NONE',  ( -0.000000000000000000, 1.000000000000000000, -0.000000000000000000 ) ) ;
#66875 = CARTESIAN_POINT ( 'NONE',  ( -8.673273193496447320, 6.947386154991765039, -89.14335558532187065 ) ) ;
#66876 = CARTESIAN_POINT ( 'NONE',  ( -47.80193682758675067, 12.85650137125658787, -71.54144132489784624 ) ) ;
#66877 = CARTESIAN_POINT ( 'NONE',  ( -6.840165690716682789, 7.836465889224659698, -23.52462357493867273 ) ) ;
#66878 = VECTOR ( 'NONE', #22612, 1000.000000000000000 ) ;
#66879 = EDGE_CURVE ( 'NONE', #18030, #51247, #52985, .T. ) ;
#66880 = DIRECTION ( 'NONE',  ( -0.000000000000000000, 1.000000000000000000, -0.000000000000000000 ) ) ;
#66881 = CARTESIAN_POINT ( 'NONE',  ( -60.66241560458684035, 16.25736033771447708, 5.970147805581513367 ) ) ;
#66882 = EDGE_LOOP ( 'NONE', ( #43111, #29380, #4147, #11081 ) ) ;
#66884 = AXIS2_PLACEMENT_3D ( 'NONE', #49773, #1599, #18824 ) ;
#66883 = DIRECTION ( 'NONE',  ( -0.000000000000000000, -1.000000000000000000, -0.000000000000000000 ) ) ;
#66886 = EDGE_LOOP ( 'NONE', ( #7579, #64487 ) ) ;
#66885 = ADVANCED_FACE ( 'NONE', ( #13375, #34838 ), #13711, .T. ) ;
#66887 = CARTESIAN_POINT ( 'NONE',  ( 107.9301116202192077, 27.82606182274594175, -77.41725551972304231 ) ) ;
#66888 = B_SPLINE_CURVE_WITH_KNOTS ( 'NONE', 3,
 ( #32439, #65855, #32782, #27148, #17653, #65144, #53867, #37704, #54210, #60557, #7093, #12374, #43318, #49288, #6034, #28553, #49999, #17291, #27495, #59843, #1831, #23289, #776, #1125, #28192, #44734, #59153, #10973, #60206, #11664, #48579, #33496, #21871, #22228, #25018, #46451, #13418, #55625, #60902, #51741, #3548, #61605, #34881, #45776, #62294, #39803 ),
 .UNSPECIFIED., .F., .F.,
 ( 4, 2, 2, 2, 2, 2, 2, 2, 2, 2, 2, 2, 2, 2, 2, 2, 2, 2, 2, 2, 2, 2, 4 ),
 ( 1.387778780781445676E-17, 0.003635178948345809194, 0.005452768422518706852, 0.007270357896691604510, 0.008179152633778018211, 0.009087947370864430177, 0.01090553684503732870, 0.01181433158212377016, 0.01272312631921020988, 0.01363192105629665134, 0.01454071579338309106, 0.01544951053046953078, 0.01635830526755597050, 0.01726710000464240849, 0.01817589474172884648, 0.01908468947881530181, 0.01999348421590176061, 0.02090227895298821595, 0.02181107369007466781, 0.02362866316424764440, 0.02544625263842061405, 0.02726384211259358370, 0.02908143158676655682 ),
 .UNSPECIFIED. ) ;
#66889 = CARTESIAN_POINT ( 'NONE',  ( 39.40195752203891999, 9.424259417798147354, -8.775266874964067654 ) ) ;
#66890 = CARTESIAN_POINT ( 'NONE',  ( 41.81982603358025585, 8.735900550613189708, 71.37462574018115902 ) ) ;
#66891 = CARTESIAN_POINT ( 'NONE',  ( -34.96012151086515019, 55.23134702900888016, 43.58025477438756212 ) ) ;
#66892 = ADVANCED_FACE ( 'NONE', ( #52383 ), #37274, .T. ) ;
#66893 = CARTESIAN_POINT ( 'NONE',  ( -15.22778517348776361, 7.486636596785420039, 92.55426355724088694 ) ) ;
#66894 = DIRECTION ( 'NONE',  ( -0.8160245890732938934, -0.5780171883497599028, 0.000000000000000000 ) ) ;
#66895 = CARTESIAN_POINT ( 'NONE',  ( -439.4229916354183274, 388.0000000000064801, -123.9497041420119530 ) ) ;
#66896 = DIRECTION ( 'NONE',  ( 0.000000000000000000, -0.000000000000000000, 1.000000000000000000 ) ) ;
#66897 = EDGE_LOOP ( 'NONE', ( #12729, #25960, #68959, #68694 ) ) ;
#66898 = ORIENTED_EDGE ( 'NONE', *, *, #45038, .F. ) ;
#66899 = DIRECTION ( 'NONE',  ( 0.000000000000000000, 0.000000000000000000, -1.000000000000000000 ) ) ;
#66900 = DIRECTION ( 'NONE',  ( -0.7071067811865474617, 0.000000000000000000, 0.7071067811865474617 ) ) ;
#66901 = CARTESIAN_POINT ( 'NONE',  ( 45.23132793708834498, 9.239011044489725322, -92.01594079018720151 ) ) ;
#66902 = CARTESIAN_POINT ( 'NONE',  ( 110.2429982417149432, 29.99119854320847267, 56.45576479620100940 ) ) ;
#66903 = DIRECTION ( 'NONE',  ( 1.000000000000000000, 0.000000000000000000, 0.000000000000000000 ) ) ;
#66904 = ADVANCED_FACE ( 'NONE', ( #4879 ), #61983, .T. ) ;
#66905 = CARTESIAN_POINT ( 'NONE',  ( 55.76255201544532980, 12.13275766515752352, -18.34786871411591136 ) ) ;
#66906 = ORIENTED_EDGE ( 'NONE', *, *, #9830, .T. ) ;
#66907 = FACE_OUTER_BOUND ( 'NONE', #29313, .T. ) ;
#66908 = CARTESIAN_POINT ( 'NONE',  ( -11.14445507968271265, 7.129894202659275315, 57.73002498924695658 ) ) ;
#66909 = CARTESIAN_POINT ( 'NONE',  ( -84.55373779407985069, 24.65190748253135666, -20.44369671590408188 ) ) ;
#66910 = DIRECTION ( 'NONE',  ( 0.000000000000000000, 0.000000000000000000, 1.000000000000000000 ) ) ;
#66911 = CARTESIAN_POINT ( 'NONE',  ( 174.9161599490639958, 73.97365196673300147, -21.15566724134466980 ) ) ;
#66912 = CARTESIAN_POINT ( 'NONE',  ( 8.711335105127083978, 6.377209569302061176, -94.18985153538824306 ) ) ;
#66913 = VECTOR ( 'NONE', #44692, 1000.000000000000000 ) ;
#66914 = VERTEX_POINT ( 'NONE', #31968 ) ;
#66915 = CARTESIAN_POINT ( 'NONE',  ( 0.000000000000000000, 0.000000000000000000, 0.000000000000000000 ) ) ;
#66916 = PLANE ( 'NONE',  #56352 ) ;
#66917 = CIRCLE ( 'NONE', #29840, 60.00000000000000000 ) ;
#66918 = CARTESIAN_POINT ( 'NONE',  ( 32.38493285958206513, 8.611594965040680449, -72.62366015745288905 ) ) ;
#66919 = CYLINDRICAL_SURFACE ( 'NONE', #18649, 7.500000000000020428 ) ;
#66920 = DIRECTION ( 'NONE',  ( -0.7530714660036196273, 0.6579387259397027066, 0.000000000000000000 ) ) ;
#66921 = CARTESIAN_POINT ( 'NONE',  ( 79.19345177405119784, 17.01649702043280143, -69.15554048193783387 ) ) ;
#66922 = AXIS2_PLACEMENT_3D ( 'NONE', #3197, #55965, #2499 ) ;
#66923 = AXIS2_PLACEMENT_3D ( 'NONE', #3567, #41208, #3234 ) ;
#66924 = ORIENTED_EDGE ( 'NONE', *, *, #37730, .T. ) ;
#66925 = AXIS2_PLACEMENT_3D ( 'NONE', #25637, #35838, #4849 ) ;
#66926 = DIRECTION ( 'NONE',  ( -0.000000000000000000, -1.000000000000000000, -0.000000000000000000 ) ) ;
#66927 = CARTESIAN_POINT ( 'NONE',  ( 198.4045886930828999, 99.71425793793706305, -47.91473179564368934 ) ) ;
#66928 = ORIENTED_EDGE ( 'NONE', *, *, #60485, .F. ) ;
#66929 = DIRECTION ( 'NONE',  ( -0.000000000000000000, -0.000000000000000000, -1.000000000000000000 ) ) ;
#66930 = ORIENTED_EDGE ( 'NONE', *, *, #6430, .F. ) ;
#66931 = CARTESIAN_POINT ( 'NONE',  ( -81.90266786693713641, 23.58030232261292269, -62.67706780553669432 ) ) ;
#66932 = DIRECTION ( 'NONE',  ( 0.000000000000000000, 0.000000000000000000, -1.000000000000000000 ) ) ;
#66933 = DIRECTION ( 'NONE',  ( -0.5407162030609373726, -0.6444004775717707689, -0.5407162030609373726 ) ) ;
#66934 =( REPRESENTATION_RELATIONSHIP ('NONE','NONE', #40274, #34334 ) REPRESENTATION_RELATIONSHIP_WITH_TRANSFORMATION ( #31049 )SHAPE_REPRESENTATION_RELATIONSHIP( ) );
#66935 = VERTEX_POINT ( 'NONE', #9827 ) ;
#66936 = ORIENTED_EDGE ( 'NONE', *, *, #13490, .F. ) ;
#66937 = CARTESIAN_POINT ( 'NONE',  ( 9.962235950564870990, 64.23203137738423152, 170.0000000000000000 ) ) ;
#66938 = DIRECTION ( 'NONE',  ( -0.9362348706397417564, 0.3513748240813305279, 0.000000000000000000 ) ) ;
#66939 = CARTESIAN_POINT ( 'NONE',  ( 23.03578842369135060, 6.840884649289439956, 8.724805532731496172 ) ) ;
#66940 = ORIENTED_EDGE ( 'NONE', *, *, #33510, .F. ) ;
#66941 = ADVANCED_FACE ( 'NONE', ( #5228 ), #62941, .T. ) ;
#66942 = CARTESIAN_POINT ( 'NONE',  ( -53.13788504024111603, 15.21566150156364472, -49.98378873765529562 ) ) ;
#66943 = CARTESIAN_POINT ( 'NONE',  ( -51.34562532494749831, 14.75613283840037226, 17.51063492481643635 ) ) ;
#66944 = CARTESIAN_POINT ( 'NONE',  ( -133.3316503378477194, 52.82738260200862612, -16.67245717274693817 ) ) ;
#66945 = CARTESIAN_POINT ( 'NONE',  ( 116.5096233816162226, 31.89062767870469273, -20.70603978022794678 ) ) ;
#66946 = CARTESIAN_POINT ( 'NONE',  ( 81.76212856587197564, 18.87332718082998184, -49.03296493046755700 ) ) ;
#66948 = VERTEX_POINT ( 'NONE', #58008 ) ;
#66947 = DIRECTION ( 'NONE',  ( 0.000000000000000000, 0.000000000000000000, 1.000000000000000000 ) ) ;
#66949 = VERTEX_POINT ( 'NONE', #10157 ) ;
#66950 = ORIENTED_EDGE ( 'NONE', *, *, #26983, .T. ) ;
#66951 = CARTESIAN_POINT ( 'NONE',  ( -6.802008071587399840, 24.18409554641266368, 3.061616997868437868E-16 ) ) ;
#66952 = CARTESIAN_POINT ( 'NONE',  ( -177.1171839969303790, 93.24095453296547475, 85.64081015030684796 ) ) ;
#66953 = FACE_OUTER_BOUND ( 'NONE', #36260, .T. ) ;
#66954 = CARTESIAN_POINT ( 'NONE',  ( 110.2429982417149432, 28.88204397445231564, -9.077886975189997543 ) ) ;
#66955 = CARTESIAN_POINT ( 'NONE',  ( -15.55634918610411077, -46.66904755831208718, 85.00100000000000477 ) ) ;
#66956 = CARTESIAN_POINT ( 'NONE',  ( -149.5074843970971017, 65.50121172469320641, -88.50193171241930656 ) ) ;
#66957 = PLANE ( 'NONE',  #40645 ) ;
#66958 = ADVANCED_FACE ( 'NONE', ( #20036 ), #25668, .F. ) ;
#66959 = CARTESIAN_POINT ( 'NONE',  ( -54.64247938334378318, 38.15500013578019889, 34.48241823999801881 ) ) ;
#66960 = CARTESIAN_POINT ( 'NONE',  ( -35.00000000000000000, 0.000000000000000000, 30.00000000000000000 ) ) ;
#66961 = CARTESIAN_POINT ( 'NONE',  ( -12.77647591501652258, 7.263973827022343954, 31.96032565673792547 ) ) ;
#66962 = ORIENTED_EDGE ( 'NONE', *, *, #69547, .T. ) ;
#66963 = CARTESIAN_POINT ( 'NONE',  ( 14.80291736570134198, 7.477373894757625372, -8.722967785034317245 ) ) ;
#66964 = ORIENTED_EDGE ( 'NONE', *, *, #60699, .F. ) ;
#66965 = ORIENTED_EDGE ( 'NONE', *, *, #20529, .T. ) ;
#66966 = PLANE ( 'NONE',  #59037 ) ;
#66967 = CIRCLE ( 'NONE', #51240, 498.0000000000000000 ) ;
#66968 = PLANE ( 'NONE',  #11365 ) ;
#66969 = CARTESIAN_POINT ( 'NONE',  ( -34.56507149095983777, 11.14725472196901102, 84.58056017436020113 ) ) ;
#66970 = EDGE_CURVE ( 'NONE', #33219, #11967, #60270, .T. ) ;
#66971 = CARTESIAN_POINT ( 'NONE',  ( 208.5889601154909485, 111.8333159387241551, -77.09575200716440690 ) ) ;
#66972 = EDGE_CURVE ( 'NONE', #13791, #4404, #10845, .T. ) ;
#66973 = CIRCLE ( 'NONE', #42244, 5.000000000000000888 ) ;
#66974 = VECTOR ( 'NONE', #63365, 1000.000000000000000 ) ;
#66975 = CARTESIAN_POINT ( 'NONE',  ( -102.7456062648101920, 33.01749955571781925, 3.674523915951419362 ) ) ;
#66976 = DIRECTION ( 'NONE',  ( 0.000000000000000000, 0.000000000000000000, -1.000000000000000000 ) ) ;
#66977 = AXIS2_PLACEMENT_3D ( 'NONE', #9446, #68857, #30905 ) ;
#66978 = CARTESIAN_POINT ( 'NONE',  ( 129.5193594945038740, 38.86618897895345981, -37.38643059234041033 ) ) ;
#66979 = VERTEX_POINT ( 'NONE', #63969 ) ;
#66980 = ORIENTED_EDGE ( 'NONE', *, *, #3842, .T. ) ;
#66981 = AXIS2_PLACEMENT_3D ( 'NONE', #33462, #39084, #60524 ) ;
#66982 = CARTESIAN_POINT ( 'NONE',  ( 187.8218355889145244, 87.19036431598357240, 93.79717328677281785 ) ) ;
#66983 = CARTESIAN_POINT ( 'NONE',  ( -13.78709718204646961, 7.352743657744182038, 6.194210338890429490 ) ) ;
#66984 = CARTESIAN_POINT ( 'NONE',  ( 2.645508037661883360, 7.710219529346608702, -0.06809871960542647484 ) ) ;
#66985 = CARTESIAN_POINT ( 'NONE',  ( -23.95096213915836358, 8.481591526885939203, -69.17300232734811516 ) ) ;
#66986 = ADVANCED_FACE ( 'NONE', ( #64315 ), #26347, .T. ) ;
#66987 = UNCERTAINTY_MEASURE_WITH_UNIT (LENGTH_MEASURE( 1.000000000000000082E-05 ), #56756, 'distance_accuracy_value', 'NONE');
#66988 = EDGE_CURVE ( 'NONE', #37405, #32357, #47100, .T. ) ;
#66989 = DIRECTION ( 'NONE',  ( 1.000000000000000000, 0.000000000000000000, 0.000000000000000000 ) ) ;
#66990 = EDGE_CURVE ( 'NONE', #38709, #34764, #24982, .T. ) ;
#66991 = ORIENTED_EDGE ( 'NONE', *, *, #12365, .F. ) ;
#66992 = DIRECTION ( 'NONE',  ( -0.000000000000000000, 1.000000000000000000, -0.000000000000000000 ) ) ;
#66993 = CARTESIAN_POINT ( 'NONE',  ( -62.14837099232446604, 17.75045801599140916, -67.11862576860336560 ) ) ;
#66994 = CARTESIAN_POINT ( 'NONE',  ( 197.3700262219430783, 98.41176242030789467, -69.04069344347526282 ) ) ;
#66995 = CARTESIAN_POINT ( 'NONE',  ( 278.8631335077134281, -21.45382118812038286, 4.871821213770100023 ) ) ;
#66996 = FILL_AREA_STYLE_COLOUR ( '', #62162 ) ;
#66997 = CARTESIAN_POINT ( 'NONE',  ( -172.3555096094762007, 86.27981310770638856, -88.43010234907279710 ) ) ;
#66998 = PLANE ( 'NONE',  #40797 ) ;
#66999 = CARTESIAN_POINT ( 'NONE',  ( -48.04019567818507142, 12.91272349839804612, 67.33324740833442945 ) ) ;
#67000 = CARTESIAN_POINT ( 'NONE',  ( -102.2801239173131052, 32.78103895658057354, -88.70367844590326456 ) ) ;
#67001 = B_SPLINE_CURVE_WITH_KNOTS ( 'NONE', 3,
 ( #64570, #44137, #29039, #6160, #66337, #17412, #23416, #65626, #18129, #28679, #38891, #22353, #28318, #39238, #32903, #27973, #49417, #27622, #39581, #43445, #33960, #49064, #61032, #60334, #44853, #12154, #12857, #50135, #33620, #43788, #49762, #60684, #54341, #1245, #22697, #899, #34311, #55395, #55759, #65263, #54698, #7585, #55048, #11788 ),
 .UNSPECIFIED., .F., .F.,
 ( 4, 2, 2, 2, 2, 2, 2, 2, 2, 2, 2, 2, 2, 2, 2, 2, 2, 2, 2, 2, 2, 4 ),
 ( 7.949501638480626889E-18, 0.001488594467279739410, 0.002232891700919614753, 0.002977188934559490529, 0.004465783401839220831, 0.005954377869118950700, 0.007442972336398679702, 0.008187269570038539432, 0.008931566803678396560, 0.01042016127095812469, 0.01190875573823785109, 0.01265305297187772036, 0.01339735020551758964, 0.01488594467279732124, 0.01563024190643718531, 0.01637453914007705111, 0.01786313360735678271, 0.01935172807463651432, 0.02009602530827637665, 0.02084032254191623551, 0.02232891700919593589, 0.02381751147647563974 ),
 .UNSPECIFIED. ) ;
#67002 = ORIENTED_EDGE ( 'NONE', *, *, #17068, .F. ) ;
#67003 = CARTESIAN_POINT ( 'NONE',  ( 275.0326735325356253, 21.99250842598268463, -0.6579281897535153023 ) ) ;
#67004 = LINE ( 'NONE', #30384, #34131 ) ;
#67005 = DIRECTION ( 'NONE',  ( 0.000000000000000000, 0.000000000000000000, 1.000000000000000000 ) ) ;
#67006 = CARTESIAN_POINT ( 'NONE',  ( -31.11269837220809364, -15.55634918610397754, 85.00100000000000477 ) ) ;
#67007 = DIRECTION ( 'NONE',  ( 0.000000000000000000, 0.000000000000000000, 1.000000000000000000 ) ) ;
#67008 = VERTEX_POINT ( 'NONE', #4541 ) ;
#67009 = CARTESIAN_POINT ( 'NONE',  ( -189.3176006225846777, 107.1977018681081830, -94.62771892500191484 ) ) ;
#67010 = CARTESIAN_POINT ( 'NONE',  ( -38.78626392836186909, 11.93872315530319916, -95.00000000000133582 ) ) ;
#67011 = VERTEX_POINT ( 'NONE', #15101 ) ;
#67012 = CIRCLE ( 'NONE', #54571, 25.00000000000000000 ) ;
#67013 = EDGE_LOOP ( 'NONE', ( #25998, #51402, #76, #33380, #30080, #9407, #65693, #66361, #27548 ) ) ;
#67014 = CARTESIAN_POINT ( 'NONE',  ( 109.9975424824652777, 296.0000000000000000, 418.0000000000000000 ) ) ;
#67015 = CARTESIAN_POINT ( 'NONE',  ( 151.8005253678162489, 54.62151558044535449, 31.97340054755885674 ) ) ;
#67016 = LINE ( 'NONE', #51170, #10001 ) ;
#67017 = VERTEX_POINT ( 'NONE', #37581 ) ;
#67018 = FACE_OUTER_BOUND ( 'NONE', #3790, .T. ) ;
#67019 = VECTOR ( 'NONE', #11572, 1000.000000000000114 ) ;
#67020 = DIRECTION ( 'NONE',  ( -0.3754023374827052950, 0.9268613172740186590, -0.001087912492708085392 ) ) ;
#67021 = LINE ( 'NONE', #57145, #34231 ) ;
#67022 = CARTESIAN_POINT ( 'NONE',  ( 56.28782924480456984, 12.23883190161852141, -39.86895606791594560 ) ) ;
#67023 = CARTESIAN_POINT ( 'NONE',  ( 74.39890044415633952, 7.951074708187157114, 41.38025477438755928 ) ) ;
#67024 = VECTOR ( 'NONE', #34024, 1000.000000000000000 ) ;
#67025 = CARTESIAN_POINT ( 'NONE',  ( 154.5976934653194235, 55.45027480068274173, 83.64124856708572509 ) ) ;
#67026 = DIRECTION ( 'NONE',  ( 1.000000000000000000, 0.000000000000000000, -0.000000000000000000 ) ) ;
#67027 = EDGE_CURVE ( 'NONE', #10200, #32423, #36210, .T. ) ;
#67028 = CARTESIAN_POINT ( 'NONE',  ( -102.2801239173131052, 32.78103895658057354, -50.01457726497594081 ) ) ;
#67029 = EDGE_LOOP ( 'NONE', ( #16463, #36289, #57900 ) ) ;
#67031 = EDGE_CURVE ( 'NONE', #59604, #54421, #69242, .T. ) ;
#67030 = CARTESIAN_POINT ( 'NONE',  ( -180.5668408223793904, 97.41302302526328560, -95.00000000000133582 ) ) ;
#67032 = AXIS2_PLACEMENT_3D ( 'NONE', #12364, #7788, #66894 ) ;
#67033 = CARTESIAN_POINT ( 'NONE',  ( -78.66644367742109978, 23.39876645725288284, 3.573650549209446137 ) ) ;
#67034 = DIRECTION ( 'NONE',  ( 0.000000000000000000, 0.000000000000000000, 1.000000000000000000 ) ) ;
#67035 = PLANE ( 'NONE',  #66884 ) ;
#67037 = ORIENTED_EDGE ( 'NONE', *, *, #51085, .F. ) ;
#67036 = CARTESIAN_POINT ( 'NONE',  ( 8.000000000000003553, -4.618802153517020948, -0.7145311798163346273 ) ) ;
#67038 = DIRECTION ( 'NONE',  ( -0.000000000000000000, 0.000000000000000000, 1.000000000000000000 ) ) ;
#67039 = ORIENTED_EDGE ( 'NONE', *, *, #51552, .F. ) ;
#67040 = CYLINDRICAL_SURFACE ( 'NONE', #60465, 7.500000000000013323 ) ;
#67041 = CARTESIAN_POINT ( 'NONE',  ( 79.52639011421918269, 18.17129627604990461, 39.67221152056748679 ) ) ;
#67042 = CARTESIAN_POINT ( 'NONE',  ( 10.55634918610409656, 36.11269837220803680, 0.000000000000000000 ) ) ;
#67043 = ADVANCED_FACE ( 'NONE', ( #52713 ), #47783, .F. ) ;
#67044 = CARTESIAN_POINT ( 'NONE',  ( 188.2988323915788271, 86.21831227955482291, -14.81084150280703149 ) ) ;
#67045 = EDGE_CURVE ( 'NONE', #48053, #16484, #58680, .T. ) ;
#67046 = CARTESIAN_POINT ( 'NONE',  ( 141.3445468829084746, 46.13338528906590597, -16.17497209548320214 ) ) ;
#67047 = CARTESIAN_POINT ( 'NONE',  ( -85.90077524418997257, 26.30132018890135726, -13.77631410858295880 ) ) ;
#67048 = CARTESIAN_POINT ( 'NONE',  ( -52.45048892661851170, 15.03803514841138167, 44.85560778983723651 ) ) ;
#67049 = EDGE_LOOP ( 'NONE', ( #61476, #40974, #67464, #66586 ) ) ;
#67050 = ORIENTED_EDGE ( 'NONE', *, *, #63366, .T. ) ;
#67051 = EDGE_CURVE ( 'NONE', #31287, #40883, #36191, .T. ) ;
#67052 = FACE_OUTER_BOUND ( 'NONE', #61900, .T. ) ;
#67053 = CARTESIAN_POINT ( 'NONE',  ( 164.8471526211111495, 63.62172173173267709, 65.13593242948432760 ) ) ;
#67054 = EDGE_CURVE ( 'NONE', #7837, #66152, #51901, .T. ) ;
#67055 = CARTESIAN_POINT ( 'NONE',  ( -189.4248691432192686, 107.3461292335514514, 63.53451367963538843 ) ) ;
#67056 = CARTESIAN_POINT ( 'NONE',  ( 188.5645326065591121, 86.51153908883290455, -44.34441675984400177 ) ) ;
#67057 = CARTESIAN_POINT ( 'NONE',  ( -109.7793173546317149, 36.75648380851389874, 65.14726243352887991 ) ) ;
#67058 = CARTESIAN_POINT ( 'NONE',  ( -30.95355748062277002, 9.511738996772324484, -50.31719736520188491 ) ) ;
#67059 = DIRECTION ( 'NONE',  ( -0.000000000000000000, -0.000000000000000000, -1.000000000000000000 ) ) ;
#67060 = EDGE_LOOP ( 'NONE', ( #59686, #64933, #26108, #4300 ) ) ;
#67061 = PRODUCT_DEFINITION_SHAPE ( 'NONE', 'NONE',  #69580 ) ;
#67062 = ORIENTED_EDGE ( 'NONE', *, *, #55986, .F. ) ;
#67063 = VERTEX_POINT ( 'NONE', #21741 ) ;
#67064 = AXIS2_PLACEMENT_3D ( 'NONE', #57781, #34693, #9595 ) ;
#67065 = CARTESIAN_POINT ( 'NONE',  ( 0.000000000000000000, 0.000000000000000000, -2.500000000000002220 ) ) ;
#67066 = CARTESIAN_POINT ( 'NONE',  ( -71.21406923660235577, 19.62143231925333708, 92.51346753887716545 ) ) ;
#67067 = CARTESIAN_POINT ( 'NONE',  ( -80.31691774066408129, 22.95709084517031684, 72.08272523424967915 ) ) ;
#67068 = CARTESIAN_POINT ( 'NONE',  ( 69.74037587279245543, 14.33355757956376131, -39.86277765393460726 ) ) ;
#67069 = DIRECTION ( 'NONE',  ( 0.000000000000000000, 1.000000000000000000, -0.000000000000000000 ) ) ;
#67070 = AXIS2_PLACEMENT_3D ( 'NONE', #5194, #20329, #69542 ) ;
#67071 = CARTESIAN_POINT ( 'NONE',  ( -57.65574514524056582, 16.43983577669857254, 30.77939530466288076 ) ) ;
#67072 = CARTESIAN_POINT ( 'NONE',  ( -96.43817545481739728, 31.02509717589737193, -20.39993158404129403 ) ) ;
#67073 = ADVANCED_FACE ( 'NONE', ( #59374 ), #60887, .T. ) ;
#67074 = EDGE_CURVE ( 'NONE', #33435, #12795, #5566, .T. ) ;
#67075 = EDGE_CURVE ( 'NONE', #66330, #22457, #17149, .T. ) ;
#67076 = AXIS2_PLACEMENT_3D ( 'NONE', #7566, #22680, #55378 ) ;
#67077 = CARTESIAN_POINT ( 'NONE',  ( 55.56634333706183781, 12.09342294753929004, 36.31147275337062297 ) ) ;
#67078 = CARTESIAN_POINT ( 'NONE',  ( 18.19409201603431114, 72.94804796678661774, 133.5802547743875550 ) ) ;
#67079 =( LENGTH_UNIT ( ) NAMED_UNIT ( * ) SI_UNIT ( .MILLI., .METRE. ) );
#67080 = ORIENTED_EDGE ( 'NONE', *, *, #26096, .F. ) ;
#67081 = CARTESIAN_POINT ( 'NONE',  ( -1.876547441458561005, 6.576559737910138814, -47.49213133585988800 ) ) ;
#67082 = CARTESIAN_POINT ( 'NONE',  ( 66.63364081668849792, 1.250000000000013323, 34.48241823979189036 ) ) ;
#67084 = ADVANCED_FACE ( 'NONE', ( #22443 ), #60432, .T. ) ;
#67083 = CARTESIAN_POINT ( 'NONE',  ( -190.0468231512975592, 108.2116162189844601, -45.51018160493545395 ) ) ;
#67085 = DIRECTION ( 'NONE',  ( 0.000000000000000000, 0.000000000000000000, 1.000000000000000000 ) ) ;
#67086 = CARTESIAN_POINT ( 'NONE',  ( 280.3299582524531388, -21.42428528562853174, -4.999999999999992006 ) ) ;
#67087 = CYLINDRICAL_SURFACE ( 'NONE', #25535, 7.500000000000020428 ) ;
#67088 = CARTESIAN_POINT ( 'NONE',  ( 129.1052153257903683, 39.78893484542955150, -10.85527751303051680 ) ) ;
#67089 = VECTOR ( 'NONE', #49159, 1000.000000000000000 ) ;
#67090 = ORIENTED_EDGE ( 'NONE', *, *, #67370, .T. ) ;
#67091 = DIRECTION ( 'NONE',  ( -1.016900719447314392E-14, 3.422269759816594905E-15, -0.9999999999999997780 ) ) ;
#67092 = CARTESIAN_POINT ( 'NONE',  ( 128.0882145863933488, 39.20607399008167704, -48.34255653863539948 ) ) ;
#67093 = CARTESIAN_POINT ( 'NONE',  ( -36.00304714721387001, 11.40794940913595745, -36.84546968814971990 ) ) ;
#67094 = CARTESIAN_POINT ( 'NONE',  ( 447.3372781065084496, 390.0000000000043769, 103.5502958579838264 ) ) ;
#67095 = CARTESIAN_POINT ( 'NONE',  ( -165.7899950883215752, 79.32217045577998249, 93.63443330788398100 ) ) ;
#67096 = ORIENTED_EDGE ( 'NONE', *, *, #19682, .F. ) ;
#67097 = CARTESIAN_POINT ( 'NONE',  ( -124.1033713525886100, 45.32626312604505614, -35.12694700365814526 ) ) ;
#67098 = CARTESIAN_POINT ( 'NONE',  ( -145.3109762780891003, 60.69959559383373460, -9.235023672830337205 ) ) ;
#67099 = CARTESIAN_POINT ( 'NONE',  ( 93.85477471612979627, 22.01426047292340371, -95.00000000000133582 ) ) ;
#67100 = ORIENTED_EDGE ( 'NONE', *, *, #3981, .F. ) ;
#67101 = CARTESIAN_POINT ( 'NONE',  ( 162.1106586665143254, 62.65159119643226404, 84.67060130219428515 ) ) ;
#67102 = ORIENTED_EDGE ( 'NONE', *, *, #66650, .F. ) ;
#67103 = DIRECTION ( 'NONE',  ( -0.000000000000000000, 1.000000000000000000, -0.000000000000000000 ) ) ;
#67104 = CARTESIAN_POINT ( 'NONE',  ( 127.1040286383415321, 37.49395136275127527, 33.73642883490668964 ) ) ;
#67105 = CARTESIAN_POINT ( 'NONE',  ( 204.6977192012829789, 106.3443248447423599, 29.20772073876942088 ) ) ;
#67106 = CARTESIAN_POINT ( 'NONE',  ( 21.88606409348644277, 6.772455198693818623, -47.39240431891337124 ) ) ;
#67107 = CARTESIAN_POINT ( 'NONE',  ( 0.000000000000000000, 0.000000000000000000, 40.00000000000003553 ) ) ;
#67109 = EDGE_LOOP ( 'NONE', ( #31573, #47285 ) ) ;
#67108 = DIRECTION ( 'NONE',  ( 0.000000000000000000, 1.000000000000000000, -0.000000000000000000 ) ) ;
#67110 = VECTOR ( 'NONE', #57379, 1000.000000000000000 ) ;
#67111 = B_SPLINE_CURVE_WITH_KNOTS ( 'NONE', 3,
 ( #7887, #58989, #247, #23714 ),
 .UNSPECIFIED., .F., .F.,
 ( 4, 4 ),
 ( 0.1259919275528356697, 0.1829744153748742441 ),
 .UNSPECIFIED. ) ;
#67112 = CARTESIAN_POINT ( 'NONE',  ( -6.140532312358493172, 7.793717686835318403, -89.24918225055428422 ) ) ;
#67113 = ORIENTED_EDGE ( 'NONE', *, *, #51543, .T. ) ;
#67114 = EDGE_LOOP ( 'NONE', ( #66516, #9686, #69133, #66351 ) ) ;
#67115 = CIRCLE ( 'NONE', #24426, 24.99999999999985434 ) ;
#67117 = EDGE_CURVE ( 'NONE', #60812, #19652, #63156, .T. ) ;
#67116 = CARTESIAN_POINT ( 'NONE',  ( -167.6566265204789943, 82.70140535081094413, 16.62003182645536725 ) ) ;
#67118 = CARTESIAN_POINT ( 'NONE',  ( 23.24028701062094271, 6.853614888934262517, -68.88555068049299734 ) ) ;
#67119 = CIRCLE ( 'NONE', #17689, 25.00000000000395772 ) ;
#67121 = ORIENTED_EDGE ( 'NONE', *, *, #4617, .F. ) ;
#67120 = CYLINDRICAL_SURFACE ( 'NONE', #41049, 7.500000000000013323 ) ;
#67122 = FACE_OUTER_BOUND ( 'NONE', #46090, .T. ) ;
#67123 = CARTESIAN_POINT ( 'NONE',  ( -29.51272929882557960, 10.30144624948894361, 44.96897510227874051 ) ) ;
#67124 = FACE_BOUND ( 'NONE', #67586, .T. ) ;
#67125 = CIRCLE ( 'NONE', #53566, 65.00000000000000000 ) ;
#67126 = EDGE_LOOP ( 'NONE', ( #26697, #40710, #18308, #14738 ) ) ;
#67127 = AXIS2_PLACEMENT_3D ( 'NONE', #16154, #49188, #22477 ) ;
#67128 = CARTESIAN_POINT ( 'NONE',  ( 206.2957331585308793, 110.2946564621822887, -78.04361713855180938 ) ) ;
#67129 = EDGE_CURVE ( 'NONE', #192, #22403, #2504, .T. ) ;
#67130 = CIRCLE ( 'NONE', #52491, 5.000000000000004441 ) ;
#67131 = CARTESIAN_POINT ( 'NONE',  ( 140.9141742510256847, 47.05414327990549594, 34.41968098850252744 ) ) ;
#67132 = LINE ( 'NONE', #62869, #61729 ) ;
#67133 = CARTESIAN_POINT ( 'NONE',  ( -133.3316503378477762, 52.82738260200861902, 10.17209341771672193 ) ) ;
#67134 = EDGE_CURVE ( 'NONE', #39251, #57393, #59762, .T. ) ;
#67135 = CARTESIAN_POINT ( 'NONE',  ( 69.72564955710448942, 15.37006465677309563, -66.70557166199922960 ) ) ;
#67136 = ORIENTED_EDGE ( 'NONE', *, *, #56377, .T. ) ;
#67137 = EDGE_CURVE ( 'NONE', #41887, #52905, #17732, .T. ) ;
#67138 = VERTEX_POINT ( 'NONE', #27714 ) ;
#67139 = CARTESIAN_POINT ( 'NONE',  ( -2.645453300864630819E-14, -10.55634918610403439, 85.00100000000000477 ) ) ;
#67140 = CARTESIAN_POINT ( 'NONE',  ( 209.8254370498217725, 113.6481017352174518, -92.02841627014599624 ) ) ;
#67141 = CARTESIAN_POINT ( 'NONE',  ( -49.98055992077275533, 13.37998597487507801, -90.87642535906408625 ) ) ;
#67142 = CARTESIAN_POINT ( 'NONE',  ( -65.13282190615095146, -1.847197903505587038E-12, -9.999999999999998224 ) ) ;
#67143 = CARTESIAN_POINT ( 'NONE',  ( -147.7860806339124622, 62.73248524776226276, 30.90810370450622102 ) ) ;
#67144 = CARTESIAN_POINT ( 'NONE',  ( -128.9925397612932443, 48.56800623462824973, 58.13062048391246606 ) ) ;
#67145 = CARTESIAN_POINT ( 'NONE',  ( -76.33235143960692426, 22.51916353135073834, -8.639353371581263374 ) ) ;
#67146 = ORIENTED_EDGE ( 'NONE', *, *, #27089, .T. ) ;
#67147 = CARTESIAN_POINT ( 'NONE',  ( 70.34686579112809568, 18.11777090454216577, 170.0000000000000000 ) ) ;
#67148 = EDGE_LOOP ( 'NONE', ( #38966, #28632, #12305, #63210 ) ) ;
#67149 = CARTESIAN_POINT ( 'NONE',  ( 34.45817031441433897, 7.817703378455677310, 31.75217239037434780 ) ) ;
#67150 = CARTESIAN_POINT ( 'NONE',  ( 209.9999999999999716, 0.000000000000000000, 72.99999999999998579 ) ) ;
#67151 = EDGE_LOOP ( 'NONE', ( #46265, #41729, #30007, #9948 ) ) ;
#67152 = CARTESIAN_POINT ( 'NONE',  ( 188.5662303205146486, 86.51341602961785782, 37.40710550623141728 ) ) ;
#67153 = DIRECTION ( 'NONE',  ( 0.000000000000000000, -1.000000000000000000, 0.000000000000000000 ) ) ;
#67154 = LINE ( 'NONE', #2765, #30465 ) ;
#67155 = FACE_OUTER_BOUND ( 'NONE', #65613, .T. ) ;
#67156 = LINE ( 'NONE', #3804, #16517 ) ;
#67157 = DIRECTION ( 'NONE',  ( 0.000000000000000000, 1.000000000000000000, 0.000000000000000000 ) ) ;
#67158 = EDGE_CURVE ( 'NONE', #9035, #7351, #37928, .T. ) ;
#67159 = ORIENTED_EDGE ( 'NONE', *, *, #49221, .F. ) ;
#67160 = CIRCLE ( 'NONE', #13269, 5.000000000000170530 ) ;
#67161 = CARTESIAN_POINT ( 'NONE',  ( 60.58000000000000540, -26.09918303830819397, 20.41169613715280207 ) ) ;
#67162 = CARTESIAN_POINT ( 'NONE',  ( -156.7487895666416478, 70.57327586518562157, -17.44133594024488332 ) ) ;
#67163 = ORIENTED_EDGE ( 'NONE', *, *, #57121, .F. ) ;
#67164 = LINE ( 'NONE', #36167, #64294 ) ;
#67165 = CARTESIAN_POINT ( 'NONE',  ( -60.95805269991219433, 17.39401718769329364, 60.03175317332093641 ) ) ;
#67167 = EDGE_CURVE ( 'NONE', #30638, #37226, #33365, .T. ) ;
#67166 = CARTESIAN_POINT ( 'NONE',  ( 74.39890044415633952, 7.951074708187157114, 43.58025477438756923 ) ) ;
#67168 = ORIENTED_EDGE ( 'NONE', *, *, #68839, .T. ) ;
#67169 = CARTESIAN_POINT ( 'NONE',  ( 8.000000000000000000, 4.618802153517024500, -0.7145311798163346273 ) ) ;
#67170 = CARTESIAN_POINT ( 'NONE',  ( 447.3372781065085633, 395.0000000000043769, 101.0502958579842101 ) ) ;
#67171 = CARTESIAN_POINT ( 'NONE',  ( -96.45845418068300603, 29.92035703021965531, -20.42477309577358824 ) ) ;
#67172 = VECTOR ( 'NONE', #28370, 1000.000000000000000 ) ;
#67173 = CARTESIAN_POINT ( 'NONE',  ( 141.3445468829085030, 46.13338528906591307, -43.01952268594691020 ) ) ;
#67174 = AXIS2_PLACEMENT_3D ( 'NONE', #11942, #28116, #39036 ) ;
#67175 = VERTEX_POINT ( 'NONE', #65014 ) ;
#67176 = CARTESIAN_POINT ( 'NONE',  ( -155.7457403566965866, 71.01814553754118720, 60.87164375294486263 ) ) ;
#67177 = CARTESIAN_POINT ( 'NONE',  ( -122.3963566076408540, 44.23346594671848919, 31.46867208311915221 ) ) ;
#67178 = CIRCLE ( 'NONE', #13232, 5.000000000000000888 ) ;
#67179 = FACE_OUTER_BOUND ( 'NONE', #53449, .T. ) ;
#67180 = ORIENTED_EDGE ( 'NONE', *, *, #62910, .T. ) ;
#67181 = DIRECTION ( 'NONE',  ( -0.8118923937861950435, -0.5838071093367415143, 0.000000000000000000 ) ) ;
#67182 = CARTESIAN_POINT ( 'NONE',  ( 424.8372781065088475, 394.9999999999999432, 91.05029585798857283 ) ) ;
#67183 = CARTESIAN_POINT ( 'NONE',  ( 116.9200705848630548, 32.09536795999727588, 40.56517214532210858 ) ) ;
#67184 = CARTESIAN_POINT ( 'NONE',  ( 93.85477471612979627, 22.01426047292340371, -95.00000000000133582 ) ) ;
#67185 = CARTESIAN_POINT ( 'NONE',  ( -52.73319225379935205, 53.34578647582052469, 170.0000000000000000 ) ) ;
#67186 = ORIENTED_EDGE ( 'NONE', *, *, #54960, .F. ) ;
#67187 = CARTESIAN_POINT ( 'NONE',  ( 164.9559213734324885, 63.71338633026439879, -16.23612744046200618 ) ) ;
#67188 = CARTESIAN_POINT ( 'NONE',  ( -24.09190246691234805, -170.0000000000000000, -95.00000000000133582 ) ) ;
#67189 = CARTESIAN_POINT ( 'NONE',  ( 65.41496713438824884, 13.24164235279044988, 71.27981269759310123 ) ) ;
#67190 = CARTESIAN_POINT ( 'NONE',  ( 134.3135005523731706, 42.87884033955815255, 2.676193764966367628 ) ) ;
#67191 = LINE ( 'NONE', #46050, #61137 ) ;
#67192 = PRODUCT_DEFINITION ( 'UNKNOWN', '', #41145, #16253 ) ;
#67193 = ORIENTED_EDGE ( 'NONE', *, *, #21212, .T. ) ;
#67194 = EDGE_CURVE ( 'NONE', #47684, #68905, #16809, .T. ) ;
#67195 = DIRECTION ( 'NONE',  ( -0.000000000000000000, -1.000000000000000000, -0.000000000000000000 ) ) ;
#67196 = ORIENTED_EDGE ( 'NONE', *, *, #29771, .T. ) ;
#67198 = EDGE_CURVE ( 'NONE', #55194, #38457, #66079, .T. ) ;
#67197 = CARTESIAN_POINT ( 'NONE',  ( 68.94309019697860208, 15.16533147648752156, 68.77903629494470295 ) ) ;
#67199 = CARTESIAN_POINT ( 'NONE',  ( 0.000000000000000000, 192.0000000000000000, 0.000000000000000000 ) ) ;
#67200 = VERTEX_POINT ( 'NONE', #6616 ) ;
#67201 = CARTESIAN_POINT ( 'NONE',  ( 162.6205203824432033, 63.07332653227187791, -38.16676261939332448 ) ) ;
#67202 = CARTESIAN_POINT ( 'NONE',  ( 47.99999999999997158, -19.99999999999997868, 0.000000000000000000 ) ) ;
#67203 = DIRECTION ( 'NONE',  ( 0.000000000000000000, 1.000000000000000000, 0.000000000000000000 ) ) ;
#67204 = DIRECTION ( 'NONE',  ( -1.000000000000000000, 0.000000000000000000, 0.000000000000000000 ) ) ;
#67205 = VERTEX_POINT ( 'NONE', #28063 ) ;
#67206 = CARTESIAN_POINT ( 'NONE',  ( -95.21085197937823352, 30.44372064875429018, 13.73146625934893095 ) ) ;
#67207 = ADVANCED_FACE ( 'NONE', ( #995 ), #17508, .T. ) ;
#67209 =( BOUNDED_CURVE ( )  B_SPLINE_CURVE ( 3, ( #27452, #48203, #10239, #58425 ),
 .UNSPECIFIED., .F., .F. ) 
 B_SPLINE_CURVE_WITH_KNOTS ( ( 4, 4 ),
 ( 1.570796326794874131, 3.141592653589778461 ),
 .UNSPECIFIED. ) 
 CURVE ( )  GEOMETRIC_REPRESENTATION_ITEM ( )  RATIONAL_B_SPLINE_CURVE ( ( 1.000000000000000000, 0.8047378541243631611, 0.8047378541243631611, 1.000000000000000000 ) ) 
 REPRESENTATION_ITEM ( '' )  );
#67208 = CARTESIAN_POINT ( 'NONE',  ( 70.50774432417125581, 15.57735247846618165, 90.51896257976297022 ) ) ;
#67210 = CIRCLE ( 'NONE', #15522, 25.00000000000000000 ) ;
#67211 = CARTESIAN_POINT ( 'NONE',  ( 209.3223706822284100, 172.0000000000000284, 31.44247402469554942 ) ) ;
#67212 = CARTESIAN_POINT ( 'NONE',  ( 84.26390409839194717, 19.68678207880319420, -9.343633932740562642 ) ) ;
#67213 = CARTESIAN_POINT ( 'NONE',  ( -165.9122696334865168, 79.44688201528256855, 36.23136382548763379 ) ) ;
#67214 = CARTESIAN_POINT ( 'NONE',  ( -147.9110140428198861, 62.83667129753960268, -88.66273618399704048 ) ) ;
#67215 = ADVANCED_FACE ( 'NONE', ( #22794, #44234 ), #38984, .F. ) ;
#67216 = CARTESIAN_POINT ( 'NONE',  ( 132.9440032680862487, 40.87616997986734191, -77.81562762824698609 ) ) ;
#67217 = EDGE_LOOP ( 'NONE', ( #55784, #10785, #36684, #14261 ) ) ;
#67218 = CARTESIAN_POINT ( 'NONE',  ( -95.63694837622351486, 30.64472169584719552, 68.35390755590003664 ) ) ;
#67219 = VECTOR ( 'NONE', #50463, 1000.000000000000114 ) ;
#67221 = EDGE_CURVE ( 'NONE', #60636, #61740, #44597, .T. ) ;
#67220 = CARTESIAN_POINT ( 'NONE',  ( -14.33060720034883673, 8.412649192293191192, 60.69540906425582705 ) ) ;
#67222 = ORIENTED_EDGE ( 'NONE', *, *, #3205, .T. ) ;
#67223 = CARTESIAN_POINT ( 'NONE',  ( -152.4930836497867688, 68.09400557494207362, -49.19664785734511980 ) ) ;
#67224 = VECTOR ( 'NONE', #16556, 1000.000000000000000 ) ;
#67225 = CARTESIAN_POINT ( 'NONE',  ( 47.99999999999997158, -20.00000000000000355, 4.000000000000000000 ) ) ;
#67226 = CARTESIAN_POINT ( 'NONE',  ( -38.45778834351241926, 11.87434869453507247, 40.37145622466209716 ) ) ;
#67227 = CARTESIAN_POINT ( 'NONE',  ( -152.5046761101291963, 66.76407727525179325, -62.27860238260412018 ) ) ;
#67228 = DIRECTION ( 'NONE',  ( -0.000000000000000000, 1.000000000000000000, -0.000000000000000000 ) ) ;
#67229 = CARTESIAN_POINT ( 'NONE',  ( -51.34325167237333432, 13.71819364263222241, -63.03792477884681489 ) ) ;
#67230 = LINE ( 'NONE', #28529, #18210 ) ;
#67231 = CARTESIAN_POINT ( 'NONE',  ( 175.8855729601531834, 73.50624012737692681, 4.536635858610266858 ) ) ;
#67232 = CARTESIAN_POINT ( 'NONE',  ( -61.75956139478100937, 16.58288496614413177, 7.606635706506060579 ) ) ;
#67233 = ORIENTED_EDGE ( 'NONE', *, *, #40186, .T. ) ;
#67234 = VECTOR ( 'NONE', #24129, 1000.000000000000000 ) ;
#67235 = CARTESIAN_POINT ( 'NONE',  ( -99.99439884168255332, 32.75762661251358310, -35.35557488724050756 ) ) ;
#67236 = ORIENTED_EDGE ( 'NONE', *, *, #45702, .T. ) ;
#67237 = CARTESIAN_POINT ( 'NONE',  ( 106.6192711434718490, 27.24117154335862168, -76.83786816052128188 ) ) ;
#67238 = CARTESIAN_POINT ( 'NONE',  ( 46.85361596800670725, 10.51535167202354160, -15.29056264614206384 ) ) ;
#67239 = CARTESIAN_POINT ( 'NONE',  ( 74.39890044415651005, -7.951074708186092188, 3.061616997868437868E-16 ) ) ;
#67240 = FACE_OUTER_BOUND ( 'NONE', #10787, .T. ) ;
#67241 = DIRECTION ( 'NONE',  ( 0.000000000000000000, -7.395570986446983486E-32, -1.000000000000000000 ) ) ;
#67242 = CARTESIAN_POINT ( 'NONE',  ( 15.55634918610396511, -46.66904755831214402, 85.00100000000000477 ) ) ;
#67243 = B_SPLINE_CURVE_WITH_KNOTS ( 'NONE', 3,
 ( #29561, #41507, #62959, #14766, #67227, #36231, #57688, #9498, #29916, #24304, #19011, #3192, #40463, #25690, #68582, #20383, #41852, #35189, #56644, #8464, #51375, #21089, #20736, #5917, #31983, #11202, #26021, #32332, #10514, #42534, #37245, #48138, #32671, #26705, #58026, #48465, #42193, #4900, #63987, #63657, #36579, #4558, #43555, #47451 ),
 .UNSPECIFIED., .F., .F.,
 ( 4, 2, 2, 2, 2, 2, 2, 2, 2, 2, 2, 2, 2, 2, 2, 2, 2, 2, 2, 2, 2, 4 ),
 ( 0.000000000000000000, 0.003433139681083573636, 0.004291424601354481248, 0.005149709521625388427, 0.006866279362167105639, 0.007724564282437977256, 0.008582849202708844535, 0.009441134122979715285, 0.01029941904325058430, 0.01201598888379235702, 0.01373255872433412975, 0.01459084364460501611, 0.01544912856487590420, 0.01630741348514679057, 0.01716569840541767866, 0.01888226824595941669, 0.02059883808650115472, 0.02145712300677206016, 0.02231540792704296561, 0.02403197776758486323, 0.02574854760812675739, 0.02746511744866865501 ),
 .UNSPECIFIED. ) ;
#67244 = CARTESIAN_POINT ( 'NONE',  ( 57.80731956814545214, 12.55178936583606131, -91.45004045484938615 ) ) ;
#67245 = CARTESIAN_POINT ( 'NONE',  ( -73.43826238111391547, 8.993593295997464589E-15, 26.24939009510892518 ) ) ;
#67246 = VERTEX_POINT ( 'NONE', #53744 ) ;
#67247 = VERTEX_POINT ( 'NONE', #39328 ) ;
#67248 = DIRECTION ( 'NONE',  ( -0.000000000000000000, -0.000000000000000000, -1.000000000000000000 ) ) ;
#67249 = FACE_OUTER_BOUND ( 'NONE', #48964, .T. ) ;
#67250 = CARTESIAN_POINT ( 'NONE',  ( 442.3372781065089612, 370.0000000000065938, -141.4497041420121661 ) ) ;
#67251 = CARTESIAN_POINT ( 'NONE',  ( 103.8055367708241477, 27.11070767929349756, 67.83620103106419208 ) ) ;
#67252 = CARTESIAN_POINT ( 'NONE',  ( 39.77028211725738061, 51.87520073220942152, 43.58025477438756212 ) ) ;
#67253 = DIRECTION ( 'NONE',  ( 0.000000000000000000, 0.000000000000000000, 1.000000000000000000 ) ) ;
#67254 = ORIENTED_EDGE ( 'NONE', *, *, #58667, .F. ) ;
#67255 = CARTESIAN_POINT ( 'NONE',  ( 109.7732660198864210, 29.77277639096405792, -35.92243756565368784 ) ) ;
#67256 = CARTESIAN_POINT ( 'NONE',  ( 22.51849650178395024, 7.817407610814548491, -39.70014265684829269 ) ) ;
#67257 = DIRECTION ( 'NONE',  ( 0.000000000000000000, -0.7071067811865475727, -0.7071067811865475727 ) ) ;
#67258 = DIRECTION ( 'NONE',  ( -1.000000000000000000, 0.000000000000000000, 0.000000000000000000 ) ) ;
#67259 = FACE_BOUND ( 'NONE', #1045, .T. ) ;
#67260 = VECTOR ( 'NONE', #16787, 1000.000000000000000 ) ;
#67261 = ORIENTED_EDGE ( 'NONE', *, *, #33113, .T. ) ;
#67262 = B_SPLINE_CURVE_WITH_KNOTS ( 'NONE', 3,
 ( #20971, #36118, #68472, #25574 ),
 .UNSPECIFIED., .F., .F.,
 ( 4, 4 ),
 ( 9.900409498943429581E-07, 0.05658314289920114704 ),
 .UNSPECIFIED. ) ;
#67263 = CIRCLE ( 'NONE', #6585, 24.99999999999985434 ) ;
#67264 = ORIENTED_EDGE ( 'NONE', *, *, #37541, .T. ) ;
#67265 = LINE ( 'NONE', #56687, #9803 ) ;
#67266 = DIRECTION ( 'NONE',  ( -1.000000000000000000, 0.000000000000000000, 0.000000000000000000 ) ) ;
#67267 = CARTESIAN_POINT ( 'NONE',  ( 64.97411640938599930, 37.36411256620309018, 41.38025477438755928 ) ) ;
#67268 = CARTESIAN_POINT ( 'NONE',  ( -174.7903139851459287, 90.53182997092831386, 18.80111118392543190 ) ) ;
#67269 = CARTESIAN_POINT ( 'NONE',  ( 8.722750525486095086, 6.377265220791373146, 88.66693184439566267 ) ) ;
#67270 = CARTESIAN_POINT ( 'NONE',  ( 0.000000000000000000, 35.00000000000000000, 0.000000000000000000 ) ) ;
#67271 = EDGE_CURVE ( 'NONE', #5944, #43828, #31856, .T. ) ;
#67272 = PRESENTATION_LAYER_ASSIGNMENT (  '', '', ( #5476 ) ) ;
#67273 = EDGE_LOOP ( 'NONE', ( #55484, #37949, #25585, #59995 ) ) ;
#67274 = CARTESIAN_POINT ( 'NONE',  ( 422.4999999999999432, -17.50000000000000000, 0.000000000000000000 ) ) ;
#67275 = LINE ( 'NONE', #66578, #63090 ) ;
#67276 = EDGE_CURVE ( 'NONE', #48157, #65219, #52211, .T. ) ;
#67277 = ORIENTED_EDGE ( 'NONE', *, *, #58848, .T. ) ;
#67278 = CARTESIAN_POINT ( 'NONE',  ( -40.53976227448249858, 9.891533029231922569, 13.79046412299628344 ) ) ;
#67279 = ORIENTED_EDGE ( 'NONE', *, *, #54648, .F. ) ;
#67280 = CARTESIAN_POINT ( 'NONE',  ( -81.67992981004169906, 23.49232121719085953, -76.33213373116126377 ) ) ;
#67281 = CARTESIAN_POINT ( 'NONE',  ( -417.6627218934913230, 1.665334536937734811E-13, 113.5502958579881749 ) ) ;
#67282 = EDGE_CURVE ( 'NONE', #23514, #27926, #2050, .T. ) ;
#67283 = LINE ( 'NONE', #29617, #25780 ) ;
#67284 = ORIENTED_EDGE ( 'NONE', *, *, #29712, .F. ) ;
#67285 = ADVANCED_FACE ( 'NONE', ( #23502 ), #4376, .F. ) ;
#67286 = ORIENTED_EDGE ( 'NONE', *, *, #63136, .T. ) ;
#67287 = CARTESIAN_POINT ( 'NONE',  ( 40.38495044702528247, 9.554194848483442470, 56.80706957984675398 ) ) ;
#67288 = DIRECTION ( 'NONE',  ( 0.000000000000000000, 0.000000000000000000, 1.000000000000000000 ) ) ;
#67289 = CARTESIAN_POINT ( 'NONE',  ( 23.09784929786603058, 6.844738137842330872, 12.36717293848776400 ) ) ;
#67290 = ORIENTED_EDGE ( 'NONE', *, *, #47530, .F. ) ;
#67291 = CYLINDRICAL_SURFACE ( 'NONE', #26675, 21.00000000000000355 ) ;
#67292 = CARTESIAN_POINT ( 'NONE',  ( -51.13576748034040520, 14.70354244225167051, 4.572286290533843278 ) ) ;
#67293 = DIRECTION ( 'NONE',  ( 1.000000000000000000, 0.000000000000000000, 0.000000000000000000 ) ) ;
#67294 = EDGE_CURVE ( 'NONE', #45287, #629, #50570, .T. ) ;
#67295 = CARTESIAN_POINT ( 'NONE',  ( 116.6734749296698652, 31.97209464358269315, -12.68594914507928451 ) ) ;
#67296 = CARTESIAN_POINT ( 'NONE',  ( 81.74250361646210195, 18.86685472882139081, -37.61107281654683732 ) ) ;
#67297 = FACE_OUTER_BOUND ( 'NONE', #63571, .T. ) ;
#67298 = VERTEX_POINT ( 'NONE', #29462 ) ;
#67299 = ORIENTED_EDGE ( 'NONE', *, *, #36787, .T. ) ;
#67300 = CARTESIAN_POINT ( 'NONE',  ( 76.57571471437145760, 10.00000000000000000, -20.00000000000000000 ) ) ;
#67301 = CARTESIAN_POINT ( 'NONE',  ( 180.2565361171341181, 79.19912802278403774, 2.497854800821170951 ) ) ;
#67302 = CARTESIAN_POINT ( 'NONE',  ( -52.66507163626138777, 14.05394608175175186, -8.745596592972852079 ) ) ;
#67303 = CARTESIAN_POINT ( 'NONE',  ( 201.6034029841261770, 102.1956603101140644, 16.70862505107374218 ) ) ;
#67304 = CARTESIAN_POINT ( 'NONE',  ( -30.58710862550656273, 9.453045329524901064, -89.05181077067686601 ) ) ;
#67305 = CARTESIAN_POINT ( 'NONE',  ( 204.4529252293439754, 107.7183975564644953, 82.89604892619028931 ) ) ;
#67306 = CARTESIAN_POINT ( 'NONE',  ( 210.0055645826033413, 115.7254585628713954, 31.38593627897014215 ) ) ;
#67307 = CARTESIAN_POINT ( 'NONE',  ( -73.09185868250597196, 20.27574131633382137, -64.41869867121339155 ) ) ;
#67308 = CARTESIAN_POINT ( 'NONE',  ( -14.19493007850031319, 7.389842975086042820, 33.64835350072206666 ) ) ;
#67309 = ORIENTED_EDGE ( 'NONE', *, *, #14830, .F. ) ;
#67310 = CARTESIAN_POINT ( 'NONE',  ( 13.84704553156522344, 7.452804552247568104, -23.42297353679536442 ) ) ;
#67311 = VERTEX_POINT ( 'NONE', #39670 ) ;
#67312 = CARTESIAN_POINT ( 'NONE',  ( 197.3685896092615621, 96.80423329231979324, -18.60473238905292703 ) ) ;
#67313 = EDGE_LOOP ( 'NONE', ( #37629, #47794, #21508, #67452 ) ) ;
#67314 = VECTOR ( 'NONE', #27890, 1000.000000000000000 ) ;
#67315 = CARTESIAN_POINT ( 'NONE',  ( -145.5195986658808351, 62.16746116576785397, 5.020210888928557935 ) ) ;
#67316 = CARTESIAN_POINT ( 'NONE',  ( 185.7267155939802876, 84.90388481853126734, -76.46461293044741581 ) ) ;
#67317 = CARTESIAN_POINT ( 'NONE',  ( -38.94425962551733988, 11.96984520263672636, 91.57215036848938894 ) ) ;
#67318 = CARTESIAN_POINT ( 'NONE',  ( -101.8145602049405767, 32.54453702486150490, -35.01457726497591239 ) ) ;
#67319 = CARTESIAN_POINT ( 'NONE',  ( 8.113421703707349053, 0.000000000000000000, 5.845715376051984435 ) ) ;
#67320 = DIRECTION ( 'NONE',  ( 1.000000000000000000, 0.000000000000000000, 0.000000000000000000 ) ) ;
#67321 = CARTESIAN_POINT ( 'NONE',  ( 9.689943677145725687, 7.388265075009368132, -47.39164370131542370 ) ) ;
#67322 = CARTESIAN_POINT ( 'NONE',  ( 133.8566784816069628, 41.42467568809806977, -36.02331093239566684 ) ) ;
#67323 = EDGE_LOOP ( 'NONE', ( #36750, #54351 ) ) ;
#67324 = VERTEX_POINT ( 'NONE', #25839 ) ;
#67325 = CARTESIAN_POINT ( 'NONE',  ( 188.5857024137486349, 88.03875867569850300, 90.36958172790924948 ) ) ;
#67326 = CYLINDRICAL_SURFACE ( 'NONE', #11699, 65.36598343705435354 ) ;
#67327 = DIRECTION ( 'NONE',  ( -0.000000000000000000, 1.000000000000000000, -0.000000000000000000 ) ) ;
#67328 = CARTESIAN_POINT ( 'NONE',  ( -25.81763596640059433, 8.735969132042862739, -74.63268230678318105 ) ) ;
#67329 = CARTESIAN_POINT ( 'NONE',  ( 447.3372781065086770, 400.0000000000000568, -146.4497041420117966 ) ) ;
#67330 = ORIENTED_EDGE ( 'NONE', *, *, #45326, .T. ) ;
#67331 = CARTESIAN_POINT ( 'NONE',  ( 45.35621884287174055, 10.27694987765648271, -74.55092264549712411 ) ) ;
#67332 = DIRECTION ( 'NONE',  ( -1.000000000000000000, -1.387778780781446169E-16, 0.000000000000000000 ) ) ;
#67333 = CARTESIAN_POINT ( 'NONE',  ( 199.9103251464699724, 101.6434290204575746, -64.89257074407096582 ) ) ;
#67334 = EDGE_CURVE ( 'NONE', #40287, #63181, #40849, .T. ) ;
#67335 = CARTESIAN_POINT ( 'NONE',  ( -179.8996803435689174, 95.00451760716445904, -38.99053287237702392 ) ) ;
#67336 = CARTESIAN_POINT ( 'NONE',  ( 410.0000000000000000, 190.0000000000000000, 380.0000000000000000 ) ) ;
#67337 = CARTESIAN_POINT ( 'NONE',  ( -24.18158274621863413, 9.527343002918314596, 62.60597738986891869 ) ) ;
#67338 = LINE ( 'NONE', #14205, #29547 ) ;
#67339 = CARTESIAN_POINT ( 'NONE',  ( -47.68742944762959013, 12.82957801017945698, 66.14038351141603300 ) ) ;
#67340 = CARTESIAN_POINT ( 'NONE',  ( -100.2050497862850023, 31.73888266434120453, -88.98404108870900586 ) ) ;
#67341 = EDGE_LOOP ( 'NONE', ( #51656, #37150 ) ) ;
#67342 = LINE ( 'NONE', #17759, #68646 ) ;
#67343 = CARTESIAN_POINT ( 'NONE',  ( -130.2196570250629293, 49.40815211106346538, -75.40313927343784428 ) ) ;
#67344 = CARTESIAN_POINT ( 'NONE',  ( -109.3386876948163859, 37.66246927061207828, -71.94451923632995261 ) ) ;
#67345 = CARTESIAN_POINT ( 'NONE',  ( -54.08504625707234936, 14.42374043447185983, -35.26311519142592488 ) ) ;
#67346 = DIRECTION ( 'NONE',  ( -0.9009688679024218105, 0.4338837391175525693, 0.000000000000000000 ) ) ;
#67347 = LINE ( 'NONE', #25474, #1888 ) ;
#67348 = EDGE_LOOP ( 'NONE', ( #36618, #15021, #30422, #436 ) ) ;
#67349 = DIRECTION ( 'NONE',  ( -0.000000000000000000, 1.000000000000000000, -0.000000000000000000 ) ) ;
#67350 = DIRECTION ( 'NONE',  ( -4.314083075427411048E-32, -1.000000000000000000, -6.123233995736763571E-17 ) ) ;
#67351 = EDGE_CURVE ( 'NONE', #60423, #54755, #55397, .T. ) ;
#67352 = EDGE_LOOP ( 'NONE', ( #44932, #13573, #19417, #37231 ) ) ;
#67353 = ORIENTED_EDGE ( 'NONE', *, *, #67510, .T. ) ;
#67354 = CARTESIAN_POINT ( 'NONE',  ( 0.000000000000000000, 0.000000000000000000, 0.000000000000000000 ) ) ;
#67355 = CARTESIAN_POINT ( 'NONE',  ( 152.6804161981488619, 55.27286404993343183, 31.13324756182342412 ) ) ;
#67356 = PLANE ( 'NONE',  #65024 ) ;
#67357 = ORIENTED_EDGE ( 'NONE', *, *, #31315, .F. ) ;
#67358 = PLANE ( 'NONE',  #8753 ) ;
#67359 = VECTOR ( 'NONE', #16981, 1000.000000000000000 ) ;
#67360 = CARTESIAN_POINT ( 'NONE',  ( -176.3896317155479778, 90.84057090619019448, 4.712634550793983301 ) ) ;
#67361 = DIRECTION ( 'NONE',  ( 1.000000000000000000, 0.000000000000000000, 0.000000000000000000 ) ) ;
#67362 = EDGE_CURVE ( 'NONE', #25726, #35180, #66772, .T. ) ;
#67363 = CYLINDRICAL_SURFACE ( 'NONE', #16318, 19.99999999999999289 ) ;
#67364 = DIRECTION ( 'NONE',  ( -0.9362348706397369824, -0.3513748240813435175, 0.000000000000000000 ) ) ;
#67365 = CARTESIAN_POINT ( 'NONE',  ( 158.1697021771102527, 58.19565064619519745, 83.10739206537702728 ) ) ;
#67366 = CARTESIAN_POINT ( 'NONE',  ( 204.6977192012829789, -170.0000000000000000, 2.363170148305746565 ) ) ;
#67367 = ORIENTED_EDGE ( 'NONE', *, *, #53236, .T. ) ;
#67368 = CARTESIAN_POINT ( 'NONE',  ( -20.55634918610405748, -15.55634918610400774, 85.00100000000000477 ) ) ;
#67369 = CARTESIAN_POINT ( 'NONE',  ( 12.46704290855393182, 6.417105965824394076, 57.63022159756878438 ) ) ;
#67370 = EDGE_CURVE ( 'NONE', #51909, #64139, #53476, .T. ) ;
#67371 = CARTESIAN_POINT ( 'NONE',  ( 447.3372781065085633, 395.0000000000043769, 101.0502958579842243 ) ) ;
#67372 = CARTESIAN_POINT ( 'NONE',  ( -71.15968973604427106, 20.66697821823242265, 91.53401883404465877 ) ) ;
#67374 = ORIENTED_EDGE ( 'NONE', *, *, #49373, .F. ) ;
#67373 = PLANE ( 'NONE',  #24248 ) ;
#67375 = CARTESIAN_POINT ( 'NONE',  ( 82.94943325692331371, 18.19803534719805782, -49.86125457933553662 ) ) ;
#67376 = VECTOR ( 'NONE', #8373, 1000.000000000000000 ) ;
#67377 = ADVANCED_FACE ( 'NONE', ( #21237 ), #47607, .F. ) ;
#67378 = ORIENTED_EDGE ( 'NONE', *, *, #321, .F. ) ;
#67379 = DIRECTION ( 'NONE',  ( 0.000000000000000000, 0.000000000000000000, 1.000000000000000000 ) ) ;
#67380 = DIRECTION ( 'NONE',  ( -0.000000000000000000, 1.000000000000000000, -0.000000000000000000 ) ) ;
#67381 = CARTESIAN_POINT ( 'NONE',  ( 447.3372781065085064, 400.0000000000001137, -146.4497041420118535 ) ) ;
#67382 = CARTESIAN_POINT ( 'NONE',  ( 181.9406741394862479, 79.47484497224792221, -9.417459808242304220 ) ) ;
#67383 = CARTESIAN_POINT ( 'NONE',  ( -120.1259246007803370, 42.81147313035988589, 69.78542509041207609 ) ) ;
#67384 = CARTESIAN_POINT ( 'NONE',  ( -85.10909119100207931, 25.97025675005452428, -19.64294555054678426 ) ) ;
#67385 = CARTESIAN_POINT ( 'NONE',  ( -180.4651598106648294, 97.28730001475651079, -13.81580514006593674 ) ) ;
#67386 = CARTESIAN_POINT ( 'NONE',  ( -54.57263979903869711, 15.59415114099631161, 30.31732777293113656 ) ) ;
#67387 = ORIENTED_EDGE ( 'NONE', *, *, #43361, .T. ) ;
#67388 = VERTEX_POINT ( 'NONE', #16642 ) ;
#67389 = CARTESIAN_POINT ( 'NONE',  ( -109.7156874346697748, 37.87149323084329211, 12.19027536507073783 ) ) ;
#67390 = DIRECTION ( 'NONE',  ( 0.000000000000000000, 0.000000000000000000, 1.000000000000000000 ) ) ;
#67391 = CARTESIAN_POINT ( 'NONE',  ( 164.3577270662354124, 63.21061577643035179, 60.77331709976006380 ) ) ;
#67392 = CYLINDRICAL_SURFACE ( 'NONE', #23926, 7.500000000000013323 ) ;
#67393 = CARTESIAN_POINT ( 'NONE',  ( -4.164416015345870470, 64.86646004871185767, 40.00000000000003553 ) ) ;
#67394 = CARTESIAN_POINT ( 'NONE',  ( 15.55634918610406103, 15.55634918610400241, 2.000000000000001776 ) ) ;
#67395 = CARTESIAN_POINT ( 'NONE',  ( 311.8713128290285113, 190.0000000000000000, -151.4173447659616443 ) ) ;
#67396 = VERTEX_POINT ( 'NONE', #5404 ) ;
#67397 = ORIENTED_EDGE ( 'NONE', *, *, #26229, .F. ) ;
#67398 = VERTEX_POINT ( 'NONE', #26858 ) ;
#67399 = CARTESIAN_POINT ( 'NONE',  ( 177.3657905147444467, 74.92740221268464040, -90.88983617643496871 ) ) ;
#67400 = CARTESIAN_POINT ( 'NONE',  ( 38.31361596636786260, -1.250000000000021982, 13.32819397642333570 ) ) ;
#67401 = CARTESIAN_POINT ( 'NONE',  ( -67.57266509268163190, 32.54128043381644630, 43.58025477438756212 ) ) ;
#67402 = CARTESIAN_POINT ( 'NONE',  ( -60.98168946575805904, 17.40090852531920262, 42.43695973922503129 ) ) ;
#67403 = DIRECTION ( 'NONE',  ( -0.000000000000000000, -0.000000000000000000, -1.000000000000000000 ) ) ;
#67404 = TOROIDAL_SURFACE ( 'NONE', #24723, 5.400000000000001243, 0.4000000000000000222 ) ;
#67405 = DIRECTION ( 'NONE',  ( 0.7660444431189771253, 0.6427876096865404731, 1.661094098900087138E-16 ) ) ;
#67406 = CARTESIAN_POINT ( 'NONE',  ( 41.04298124592206420, 8.628434602995477931, 83.77720471021285675 ) ) ;
#67408 = ORIENTED_EDGE ( 'NONE', *, *, #62082, .T. ) ;
#67407 = EDGE_CURVE ( 'NONE', #40972, #52786, #63808, .T. ) ;
#67409 = LINE ( 'NONE', #30458, #55352 ) ;
#67410 = CARTESIAN_POINT ( 'NONE',  ( 447.3372781065085064, 395.0000000000043769, 103.5502958579838264 ) ) ;
#67411 = CARTESIAN_POINT ( 'NONE',  ( -119.5576859660651081, 42.46117483543969939, 7.254307368285498825 ) ) ;
#67412 = DIRECTION ( 'NONE',  ( 1.000000000000000000, 0.000000000000000000, 0.000000000000000000 ) ) ;
#67413 = CARTESIAN_POINT ( 'NONE',  ( 132.9440032680863624, 40.87616997986732770, -24.12652644731961615 ) ) ;
#67414 = CARTESIAN_POINT ( 'NONE',  ( 20.35964562795319921, 7.697260051881320564, -10.20843155924452539 ) ) ;
#67415 = CARTESIAN_POINT ( 'NONE',  ( -108.9452487746634262, 36.29752968355630571, -72.83582910382180842 ) ) ;
#67416 = EDGE_CURVE ( 'NONE', #15171, #5460, #38096, .T. ) ;
#67417 = ORIENTED_EDGE ( 'NONE', *, *, #23437, .T. ) ;
#67418 = DIRECTION ( 'NONE',  ( -0.9108602745606085849, -0.4127148655274885947, 6.688014089868687434E-15 ) ) ;
#67419 = CARTESIAN_POINT ( 'NONE',  ( 132.2818448028687612, 41.65267246304673421, -50.85966255019037874 ) ) ;
#67420 = CARTESIAN_POINT ( 'NONE',  ( -127.6992109187851980, 47.69334801994794759, 3.981565830366440739 ) ) ;
#67421 = CARTESIAN_POINT ( 'NONE',  ( 412.3372781065085633, 219.4906275429376308, 111.5502958579881749 ) ) ;
#67422 = CARTESIAN_POINT ( 'NONE',  ( 188.2086267457325448, 87.61890531228284829, -46.08538211307052990 ) ) ;
#67423 = EDGE_LOOP ( 'NONE', ( #48189, #32338, #6177, #9901 ) ) ;
#67424 = ORIENTED_EDGE ( 'NONE', *, *, #8268, .T. ) ;
#67425 = EDGE_CURVE ( 'NONE', #63280, #44375, #17490, .T. ) ;
#67426 = CARTESIAN_POINT ( 'NONE',  ( -31.43908319763709969, 9.591432048623758533, -23.47264677473818395 ) ) ;
#67427 = CYLINDRICAL_SURFACE ( 'NONE', #15837, 498.0000000000000000 ) ;
#67428 = ADVANCED_FACE ( 'NONE', ( #38810 ), #60603, .F. ) ;
#67429 = ORIENTED_EDGE ( 'NONE', *, *, #49048, .T. ) ;
#67430 =( REPRESENTATION_RELATIONSHIP ('NONE','NONE', #46031, #48255 ) REPRESENTATION_RELATIONSHIP_WITH_TRANSFORMATION ( #36102 )SHAPE_REPRESENTATION_RELATIONSHIP( ) );
#67431 = CARTESIAN_POINT ( 'NONE',  ( 150.2755237883188499, 53.50786132674227247, 92.72454620485628141 ) ) ;
#67432 = EDGE_CURVE ( 'NONE', #64960, #11163, #34233, .T. ) ;
#67433 = ORIENTED_EDGE ( 'NONE', *, *, #43753, .T. ) ;
#67434 = CARTESIAN_POINT ( 'NONE',  ( 129.1310456962234809, 39.80382822048401437, -76.21209168102404874 ) ) ;
#67435 = CARTESIAN_POINT ( 'NONE',  ( 0.000000000000000000, 0.000000000000000000, 41.38025477438755928 ) ) ;
#67436 = CARTESIAN_POINT ( 'NONE',  ( -156.9919426121902575, 72.16759471857101005, 38.78368848896538879 ) ) ;
#67437 = EDGE_CURVE ( 'NONE', #16812, #57236, #17704, .T. ) ;
#67438 = VECTOR ( 'NONE', #57784, 1000.000000000000000 ) ;
#67439 = EDGE_CURVE ( 'NONE', #38815, #13387, #11712, .T. ) ;
#67440 = DIRECTION ( 'NONE',  ( -0.8090169943749422332, -0.5877852522924802425, 0.000000000000000000 ) ) ;
#67441 = DIRECTION ( 'NONE',  ( 1.000000000000000000, 0.000000000000000000, 0.000000000000000000 ) ) ;
#67443 = ORIENTED_EDGE ( 'NONE', *, *, #19603, .T. ) ;
#67442 = CARTESIAN_POINT ( 'NONE',  ( 15.78827728214693416, -170.0000000000000000, -23.67439350822212774 ) ) ;
#67444 = B_SPLINE_CURVE_WITH_KNOTS ( 'NONE', 3,
 ( #22549, #29223, #28163, #39094 ),
 .UNSPECIFIED., .F., .F.,
 ( 4, 4 ),
 ( 9.900409499097199942E-07, 0.05658314289920114010 ),
 .UNSPECIFIED. ) ;
#67445 = CARTESIAN_POINT ( 'NONE',  ( 56.30011474572736319, 11.21470186335419861, 33.96431529039685415 ) ) ;
#67446 = ORIENTED_EDGE ( 'NONE', *, *, #45966, .F. ) ;
#67447 = ORIENTED_EDGE ( 'NONE', *, *, #57972, .F. ) ;
#67448 = CARTESIAN_POINT ( 'NONE',  ( -166.2065256787326177, 81.19093426984588291, 14.39615283784645072 ) ) ;
#67449 = EDGE_CURVE ( 'NONE', #24801, #13412, #28323, .T. ) ;
#67450 = CARTESIAN_POINT ( 'NONE',  ( 18.89064107370902690, 6.619789970027396997, -63.03085641855517451 ) ) ;
#67452 = ORIENTED_EDGE ( 'NONE', *, *, #23379, .F. ) ;
#67451 = LINE ( 'NONE', #57924, #21954 ) ;
#67453 = DIRECTION ( 'NONE',  ( 0.000000000000000000, 0.000000000000000000, 1.000000000000000000 ) ) ;
#67454 = EDGE_CURVE ( 'NONE', #32990, #32477, #49763, .T. ) ;
#67455 = ADVANCED_FACE ( 'NONE', ( #28603 ), #28239, .T. ) ;
#67456 = VECTOR ( 'NONE', #39578, 1000.000000000000000 ) ;
#67457 = FACE_BOUND ( 'NONE', #39864, .T. ) ;
#67458 = VERTEX_POINT ( 'NONE', #1882 ) ;
#67459 = CARTESIAN_POINT ( 'NONE',  ( 211.3757499519975909, 117.8130818709823302, -67.24546217480406085 ) ) ;
#67460 = CARTESIAN_POINT ( 'NONE',  ( 139.1306635769909121, 45.89653412152166823, 31.67232335441821078 ) ) ;
#67461 = CYLINDRICAL_SURFACE ( 'NONE', #6696, 7.500000000000020428 ) ;
#67462 = CARTESIAN_POINT ( 'NONE',  ( -125.8938041572051389, 47.69968343338780414, 18.77539728269342945 ) ) ;
#67463 = LINE ( 'NONE', #19255, #37373 ) ;
#67464 = ORIENTED_EDGE ( 'NONE', *, *, #26766, .T. ) ;
#67465 = ORIENTED_EDGE ( 'NONE', *, *, #48505, .F. ) ;
#67466 = CARTESIAN_POINT ( 'NONE',  ( -17.90772993695116355, 72.84144224619130625, 73.58025477438756923 ) ) ;
#67467 = DIRECTION ( 'NONE',  ( -0.000000000000000000, -0.000000000000000000, -1.000000000000000000 ) ) ;
#67468 = CARTESIAN_POINT ( 'NONE',  ( -49.66937262962775890, 13.30390939630160929, -91.17893582821346854 ) ) ;
#67469 = CARTESIAN_POINT ( 'NONE',  ( -48.85164209420741344, 14.14099498278764244, -92.18124229352110888 ) ) ;
#67470 = DIRECTION ( 'NONE',  ( 0.7227948638273878901, 0.6910626489868685329, 0.000000000000000000 ) ) ;
#67471 = CARTESIAN_POINT ( 'NONE',  ( 70.46579300139244140, 15.56614468937218909, -42.22221902765776491 ) ) ;
#67472 = CARTESIAN_POINT ( 'NONE',  ( -118.3948752128398638, 42.92869324237091178, 38.41731472785173906 ) ) ;
#67473 = CARTESIAN_POINT ( 'NONE',  ( -166.7068579965637127, 80.26142964949320913, -72.95228584046991216 ) ) ;
#67474 = VERTEX_POINT ( 'NONE', #23336 ) ;
#67475 = CARTESIAN_POINT ( 'NONE',  ( -5.000000000000026645, -15.55634918610403616, 0.000000000000000000 ) ) ;
#67476 = VERTEX_POINT ( 'NONE', #65905 ) ;
#67477 = CARTESIAN_POINT ( 'NONE',  ( -180.2625951943601024, 95.44595303765449046, -93.59349302508864810 ) ) ;
#67478 = CARTESIAN_POINT ( 'NONE',  ( 81.57915404881514121, 18.81499384983930057, 58.50637853310414727 ) ) ;
#67479 = VERTEX_POINT ( 'NONE', #39164 ) ;
#67480 = CARTESIAN_POINT ( 'NONE',  ( 86.62931800182293784, 19.42108912189597092, -50.82156419891174437 ) ) ;
#67481 = PLANE ( 'NONE',  #766 ) ;
#67482 = DIRECTION ( 'NONE',  ( -1.000000000000000000, 0.000000000000000000, 0.000000000000000000 ) ) ;
#67483 = DIRECTION ( 'NONE',  ( 0.000000000000000000, 0.000000000000000000, 1.000000000000000000 ) ) ;
#67484 = CARTESIAN_POINT ( 'NONE',  ( 36.76746179515744473, 8.081433644308900099, 17.59563346917418869 ) ) ;
#67485 = CARTESIAN_POINT ( 'NONE',  ( -15.27594996066617483, 8.502079791899657124, -43.90747202117393755 ) ) ;
#67486 = CIRCLE ( 'NONE', #52840, 65.36598343705435354 ) ;
#67487 = CARTESIAN_POINT ( 'NONE',  ( 73.79471914489741380, -13.39176710989671726, 43.58025477438756212 ) ) ;
#67488 = EDGE_LOOP ( 'NONE', ( #14303, #20062, #17988, #36639 ) ) ;
#67489 = CARTESIAN_POINT ( 'NONE',  ( -109.4059773746700444, 36.55056299043143753, -93.85300586226982489 ) ) ;
#67490 = EDGE_LOOP ( 'NONE', ( #30980, #53245, #16871, #69475 ) ) ;
#67491 = CARTESIAN_POINT ( 'NONE',  ( -4.999999999999971578, 15.55634918610403084, 2.000000000000001776 ) ) ;
#67492 = CARTESIAN_POINT ( 'NONE',  ( -57.43883374585517032, 16.37892664338858850, 71.77631074466216887 ) ) ;
#67493 = CARTESIAN_POINT ( 'NONE',  ( 15.78827728214693416, -170.0000000000000000, -96.70804527961315955 ) ) ;
#67494 = EDGE_LOOP ( 'NONE', ( #10868, #3086 ) ) ;
#67495 = LINE ( 'NONE', #56942, #31104 ) ;
#67496 = CARTESIAN_POINT ( 'NONE',  ( -56.73992761491503245, 15.14028026131270366, -89.09451971216485333 ) ) ;
#67497 = CARTESIAN_POINT ( 'NONE',  ( -37.92542950990691963, 10.74638084523341952, 33.94305653771795761 ) ) ;
#67498 = CARTESIAN_POINT ( 'NONE',  ( 139.6359093656974153, 45.02518919224743144, -38.73665037353510598 ) ) ;
#67499 = EDGE_CURVE ( 'NONE', #67779, #60980, #18047, .T. ) ;
#67500 = B_SPLINE_CURVE_WITH_KNOTS ( 'NONE', 3,
 ( #12157, #43104, #43791, #48712, #64573, #64927 ),
 .UNSPECIFIED., .F., .F.,
 ( 4, 2, 4 ),
 ( 0.008240550023493531037, 0.01057684187039406240, 0.01291313371729459203 ),
 .UNSPECIFIED. ) ;
#67501 = VERTEX_POINT ( 'NONE', #54194 ) ;
#67502 = CARTESIAN_POINT ( 'NONE',  ( -153.1031717208031750, 68.63449618039562949, 58.47953369091288067 ) ) ;
#67503 = CARTESIAN_POINT ( 'NONE',  ( 110.2429982417149290, 28.88204397445231209, 29.61121420573730489 ) ) ;
#67504 = CARTESIAN_POINT ( 'NONE',  ( -58.10608953386397246, 15.52134062643864354, -49.57095537761784954 ) ) ;
#67505 = ORIENTED_EDGE ( 'NONE', *, *, #29153, .T. ) ;
#67506 = CARTESIAN_POINT ( 'NONE',  ( -179.5109681715918555, 96.11572638569523974, -73.02150784162149932 ) ) ;
#67507 = CARTESIAN_POINT ( 'NONE',  ( 129.1998560374819647, 39.84370217048449092, 84.81121093761140628 ) ) ;
#67508 = EDGE_CURVE ( 'NONE', #6711, #26511, #21507, .T. ) ;
#67510 = EDGE_CURVE ( 'NONE', #47754, #59735, #38418, .T. ) ;
#67509 = DIRECTION ( 'NONE',  ( -1.000000000000000000, -1.387778780781445922E-16, 0.000000000000000000 ) ) ;
#67511 = FILL_AREA_STYLE ('',( #51676 ) ) ;
#67512 = ADVANCED_FACE ( 'NONE', ( #43298 ), #38038, .T. ) ;
#67513 = CARTESIAN_POINT ( 'NONE',  ( 133.8566784816069344, 41.42467568809808398, 29.51034083899533300 ) ) ;
#67514 = EDGE_CURVE ( 'NONE', #55844, #41662, #65126, .T. ) ;
#67515 = ORIENTED_EDGE ( 'NONE', *, *, #1922, .F. ) ;
#67516 = CARTESIAN_POINT ( 'NONE',  ( 197.8436586345020203, 97.39326576892285914, 33.60968991493576397 ) ) ;
#67517 = CARTESIAN_POINT ( 'NONE',  ( 111.8699272271189358, 29.64190505307782075, -77.59217791608018899 ) ) ;
#67518 = CARTESIAN_POINT ( 'NONE',  ( 110.2429982417149432, 29.99119854320846201, -35.92243756565368784 ) ) ;
#67519 = CARTESIAN_POINT ( 'NONE',  ( 182.4910189501783577, 80.03877586733645444, -90.03880345596023460 ) ) ;
#67520 = DIRECTION ( 'NONE',  ( 0.000000000000000000, 1.000000000000000000, 0.000000000000000000 ) ) ;
#67521 = AXIS2_PLACEMENT_3D ( 'NONE', #46528, #39871, #2253 ) ;
#67522 = AXIS2_PLACEMENT_3D ( 'NONE', #11419, #32890, #54327 ) ;
#67523 = ORIENTED_EDGE ( 'NONE', *, *, #53176, .T. ) ;
#67524 = DIRECTION ( 'NONE',  ( -0.000000000000000000, 1.000000000000000000, -0.000000000000000000 ) ) ;
#67525 = AXIS2_PLACEMENT_3D ( 'NONE', #25233, #13293, #34749 ) ;
#67526 = ORIENTED_EDGE ( 'NONE', *, *, #40648, .T. ) ;
#67527 = CARTESIAN_POINT ( 'NONE',  ( 63.01563776193091826, 13.70579113808095251, 56.65751152968497451 ) ) ;
#67528 = CARTESIAN_POINT ( 'NONE',  ( 139.9689050549367266, 45.23922256703520617, 86.29823414930417869 ) ) ;
#67530 = VERTEX_POINT ( 'NONE', #59827 ) ;
#67529 = CARTESIAN_POINT ( 'NONE',  ( -783.0172411895269988, -622.0000000000060254, 0.000000000000000000 ) ) ;
#67531 = CARTESIAN_POINT ( 'NONE',  ( 164.9706294237034001, 65.04392654036659849, -43.89830601384430508 ) ) ;
#67532 = AXIS2_PLACEMENT_3D ( 'NONE', #4133, #48056, #9756 ) ;
#67533 = DIRECTION ( 'NONE',  ( -1.000000000000000000, 0.000000000000000000, 0.000000000000000000 ) ) ;
#67534 = EDGE_CURVE ( 'NONE', #26255, #28668, #21704, .T. ) ;
#67535 = EDGE_CURVE ( 'NONE', #19652, #66051, #49271, .T. ) ;
#67536 = CARTESIAN_POINT ( 'NONE',  ( 164.6406716478538783, 63.44801348349341197, -45.84013439700346026 ) ) ;
#67537 = ORIENTED_EDGE ( 'NONE', *, *, #18444, .F. ) ;
#67538 = ADVANCED_FACE ( 'NONE', ( #8472 ), #39102, .F. ) ;
#67539 = FACE_OUTER_BOUND ( 'NONE', #69570, .T. ) ;
#67540 = CARTESIAN_POINT ( 'NONE',  ( 55.92717366837369042, 12.16587666349906982, 88.52872284767667566 ) ) ;
#67541 = DIRECTION ( 'NONE',  ( -0.8345732537212999791, -0.5508969814521065267, 2.500042656554809847E-16 ) ) ;
#67542 = CARTESIAN_POINT ( 'NONE',  ( 79.13041963748369767, 18.04952109592811738, -16.99722329755391570 ) ) ;
#67543 = CARTESIAN_POINT ( 'NONE',  ( -173.1211646369891355, 88.63826465341151106, -88.40105834567734178 ) ) ;
#67544 = CARTESIAN_POINT ( 'NONE',  ( -33.83558513595455253, 9.996963989836508802, -62.55072875604015792 ) ) ;
#67545 = CARTESIAN_POINT ( 'NONE',  ( 88.28889510440058075, 21.05995314109330963, 44.53004548791538753 ) ) ;
#67546 = ORIENTED_EDGE ( 'NONE', *, *, #13977, .T. ) ;
#67547 = CARTESIAN_POINT ( 'NONE',  ( -101.3537077702550988, 33.43904726487055257, 72.32055988684196279 ) ) ;
#67548 = CARTESIAN_POINT ( 'NONE',  ( -15.07533778868020313, 8.482826962130836534, 66.39636851612516466 ) ) ;
#67549 = ORIENTED_EDGE ( 'NONE', *, *, #44739, .T. ) ;
#67550 = CARTESIAN_POINT ( 'NONE',  ( 151.6178224291901131, 54.48737267587417676, -12.08258827898731802 ) ) ;
#67551 = CARTESIAN_POINT ( 'NONE',  ( 211.8382652195006983, 118.5282575235990095, -14.66487468951659068 ) ) ;
#67552 = CARTESIAN_POINT ( 'NONE',  ( -33.83721310978700103, 11.01869210665938681, 30.60599803115480810 ) ) ;
#67553 = DIRECTION ( 'NONE',  ( -0.000000000000000000, 1.000000000000000000, -0.000000000000000000 ) ) ;
#67554 = CARTESIAN_POINT ( 'NONE',  ( 61.72676562228498653, 12.37728358935400941, 83.60623520330705105 ) ) ;
#67555 = DIRECTION ( 'NONE',  ( 1.000000000000000000, -1.232595164407830946E-32, -7.703719777548943412E-34 ) ) ;
#67556 = CARTESIAN_POINT ( 'NONE',  ( -0.7211439451572427828, 7.539282923622933730, -13.65695759729669234 ) ) ;
#67557 = CARTESIAN_POINT ( 'NONE',  ( 174.6176230994777541, 72.30829341023246570, 13.80334415398240111 ) ) ;
#67558 = CARTESIAN_POINT ( 'NONE',  ( -56.96214175905167565, 15.20165595797839586, 18.22969659526463815 ) ) ;
#67559 = ORIENTED_EDGE ( 'NONE', *, *, #42926, .F. ) ;
#67560 = FACE_OUTER_BOUND ( 'NONE', #43982, .T. ) ;
#67561 = ORIENTED_EDGE ( 'NONE', *, *, #30027, .T. ) ;
#67562 = CARTESIAN_POINT ( 'NONE',  ( 102.8458551240039611, 25.60773946375956456, -71.53149621033008998 ) ) ;
#67563 = DIRECTION ( 'NONE',  ( 1.000000000000000000, 0.000000000000000000, -0.000000000000000000 ) ) ;
#67564 = CARTESIAN_POINT ( 'NONE',  ( 45.36109889487607205, 9.259412558041161034, 68.83869726676070400 ) ) ;
#67565 = DIRECTION ( 'NONE',  ( 0.1342332658176522420, 0.9909497617679352555, 0.000000000000000000 ) ) ;
#67566 = CARTESIAN_POINT ( 'NONE',  ( -0.9745282055893963458, 6.541451027421887332, 94.42703022882983532 ) ) ;
#67567 = CIRCLE ( 'NONE', #33866, 5.000000000000000888 ) ;
#67568 = CARTESIAN_POINT ( 'NONE',  ( -109.7156874346698174, 37.87149323084328500, -14.65427522539294536 ) ) ;
#67569 = ORIENTED_EDGE ( 'NONE', *, *, #57328, .T. ) ;
#67570 = AXIS2_PLACEMENT_3D ( 'NONE', #12401, #54599, #6425 ) ;
#67571 = DIRECTION ( 'NONE',  ( -0.9009688679024218105, 0.4338837391175525693, 0.000000000000000000 ) ) ;
#67572 = CARTESIAN_POINT ( 'NONE',  ( -166.2028193222418793, 79.74385139484273566, 62.25590132581950087 ) ) ;
#67573 = ORIENTED_EDGE ( 'NONE', *, *, #67499, .T. ) ;
#67574 = EDGE_LOOP ( 'NONE', ( #68662, #65994 ) ) ;
#67575 = DIRECTION ( 'NONE',  ( 0.000000000000000000, -0.000000000000000000, 1.000000000000000000 ) ) ;
#67576 = CARTESIAN_POINT ( 'NONE',  ( 0.000000000000000000, 0.000000000000000000, 0.000000000000000000 ) ) ;
#67578 = CARTESIAN_POINT ( 'NONE',  ( 141.9165763529819344, 192.0000000000000000, 108.9999999999999289 ) ) ;
#67577 = VECTOR ( 'NONE', #30, 1000.000000000000000 ) ;
#67579 = CARTESIAN_POINT ( 'NONE',  ( 103.1695711638930959, 26.83837309506526481, 61.41201509413315307 ) ) ;
#67580 = EDGE_CURVE ( 'NONE', #60980, #7875, #45402, .T. ) ;
#67581 = DIRECTION ( 'NONE',  ( 0.000000000000000000, 0.000000000000000000, 1.000000000000000000 ) ) ;
#67582 = AXIS2_PLACEMENT_3D ( 'NONE', #35642, #13826, #34614 ) ;
#67583 = CARTESIAN_POINT ( 'NONE',  ( 60.40531521312253460, 13.11276739283242421, -23.41139328403251696 ) ) ;
#67584 = EDGE_LOOP ( 'NONE', ( #35135, #32207, #68447, #31432 ) ) ;
#67585 = DIRECTION ( 'NONE',  ( 1.000000000000000000, -0.000000000000000000, 0.000000000000000000 ) ) ;
#67586 = EDGE_LOOP ( 'NONE', ( #4316, #64009, #50324, #59524 ) ) ;
#67587 = CARTESIAN_POINT ( 'NONE',  ( 22.51798020284706681, 7.817376421459703018, -46.33885551830132243 ) ) ;
#67588 = CARTESIAN_POINT ( 'NONE',  ( -142.8556048422594813, 60.01994222009840030, 41.69565126987502168 ) ) ;
#67589 = CARTESIAN_POINT ( 'NONE',  ( 211.8476521439974078, 116.6941316755177525, 38.99529880182225838 ) ) ;
#67590 = FACE_BOUND ( 'NONE', #29100, .T. ) ;
#67591 = EDGE_CURVE ( 'NONE', #66072, #17942, #1551, .T. ) ;
#67592 = EDGE_CURVE ( 'NONE', #29614, #10617, #39690, .T. ) ;
#67593 = ORIENTED_EDGE ( 'NONE', *, *, #6886, .F. ) ;
#67594 = EDGE_CURVE ( 'NONE', #20715, #4283, #23375, .T. ) ;
#67595 = VERTEX_POINT ( 'NONE', #24313 ) ;
#67596 = LINE ( 'NONE', #40854, #14320 ) ;
#67597 = CARTESIAN_POINT ( 'NONE',  ( -132.6540878434535955, 52.34298938643414090, 88.49361340196719539 ) ) ;
#67598 = CARTESIAN_POINT ( 'NONE',  ( 33.46033188299909256, 8.722678254080101112, -74.54781320571061087 ) ) ;
#67599 = CARTESIAN_POINT ( 'NONE',  ( 18.89356949897823768, 62.19351277735707839, 170.0000000000000000 ) ) ;
#67600 = CARTESIAN_POINT ( 'NONE',  ( 22.45676458343273296, 6.805709986489419272, 87.75587017291512382 ) ) ;
#67601 = CARTESIAN_POINT ( 'NONE',  ( 6.400000000000000355, 0.000000000000000000, 0.000000000000000000 ) ) ;
#67602 = ORIENTED_EDGE ( 'NONE', *, *, #56361, .F. ) ;
#67603 = DIRECTION ( 'NONE',  ( -0.000000000000000000, -1.000000000000000000, -0.000000000000000000 ) ) ;
#67604 = CARTESIAN_POINT ( 'NONE',  ( 197.9868529032976028, 99.18611233336802968, -47.18661369665191785 ) ) ;
#67605 = ORIENTED_EDGE ( 'NONE', *, *, #43505, .T. ) ;
#67606 =( BOUNDED_CURVE ( )  B_SPLINE_CURVE ( 3, ( #3703, #24822, #57866, #20227 ),
 .UNSPECIFIED., .F., .F. ) 
 B_SPLINE_CURVE_WITH_KNOTS ( ( 4, 4 ),
 ( -8.881784197001252323E-16, 1.570796326794886344 ),
 .UNSPECIFIED. ) 
 CURVE ( )  GEOMETRIC_REPRESENTATION_ITEM ( )  RATIONAL_B_SPLINE_CURVE ( ( 1.000000000000000000, 0.8047378541243671579, 0.8047378541243671579, 1.000000000000000000 ) ) 
 REPRESENTATION_ITEM ( '' )  );
#67607 = CARTESIAN_POINT ( 'NONE',  ( 110.2429982417149574, 29.99119854320845846, -89.61153874658103291 ) ) ;
#67608 = EDGE_LOOP ( 'NONE', ( #3142, #61142, #11832, #17958 ) ) ;
#67609 = CARTESIAN_POINT ( 'NONE',  ( -83.14462298835726983, 24.07775853418029754, -75.49557268907416585 ) ) ;
#67610 = LINE ( 'NONE', #57056, #41039 ) ;
#67611 = EDGE_LOOP ( 'NONE', ( #50994, #69199, #9308, #44531 ) ) ;
#67612 = CIRCLE ( 'NONE', #50729, 5.000000000000000888 ) ;
#67613 = VERTEX_POINT ( 'NONE', #56652 ) ;
#67614 = CARTESIAN_POINT ( 'NONE',  ( 39.88975917505626256, 9.487965272711656795, 56.75838489642696771 ) ) ;
#67615 = CARTESIAN_POINT ( 'NONE',  ( 0.000000000000000000, 0.000000000000000000, 170.0000000000000000 ) ) ;
#67616 = CARTESIAN_POINT ( 'NONE',  ( 104.7042813665017178, 27.49927371769997464, 15.34735190411218575 ) ) ;
#67617 = CIRCLE ( 'NONE', #4684, 75.31295361348104223 ) ;
#67618 = EDGE_LOOP ( 'NONE', ( #10815, #49472, #49902, #34721, #69467, #14055, #10228, #31598, #64268 ) ) ;
#67619 = ADVANCED_FACE ( 'NONE', ( #29923 ), #60884, .F. ) ;
#67620 = PRODUCT ( 'cutting blade', 'cutting blade', '', ( #10378 ) ) ;
#67621 = AXIS2_PLACEMENT_3D ( 'NONE', #51197, #19521, #61048 ) ;
#67622 = STYLED_ITEM ( 'NONE', ( #59072 ), #17808 ) ;
#67623 = CARTESIAN_POINT ( 'NONE',  ( -33.96986881321595320, 10.02034822982698437, 84.33807109151561576 ) ) ;
#67624 = CARTESIAN_POINT ( 'NONE',  ( -54.57263979903869711, 15.59415114099631161, 3.472777182467472468 ) ) ;
#67625 = CARTESIAN_POINT ( 'NONE',  ( 92.91022130985207639, -170.0000000000000000, 94.99999999999866418 ) ) ;
#67626 = CARTESIAN_POINT ( 'NONE',  ( 422.4999999999999432, 207.5000000000000284, 378.0000000000000000 ) ) ;
#67627 = CIRCLE ( 'NONE', #3596, 299.9999999999999432 ) ;
#67628 = CARTESIAN_POINT ( 'NONE',  ( 85.67165909753201447, 20.15791549876374589, -35.86735994369028191 ) ) ;
#67629 = DIRECTION ( 'NONE',  ( 0.000000000000000000, 0.000000000000000000, 1.000000000000000000 ) ) ;
#67630 = ORIENTED_EDGE ( 'NONE', *, *, #53666, .F. ) ;
#67631 = CLOSED_SHELL ( 'NONE', ( #52164, #66422, #24102, #3116, #44603, #34960, #18100, #10536, #2487, #14923, #3632, #12408, #12414, #65665, #24412, #45742, #33024, #48858, #57490, #68757 ) ) ;
#67632 = VERTEX_POINT ( 'NONE', #13401 ) ;
#67633 = CARTESIAN_POINT ( 'NONE',  ( 46.70715146412977958, 9.472433765547009443, 8.853342646177644326 ) ) ;
#67634 = CARTESIAN_POINT ( 'NONE',  ( -180.1186349629460892, 96.86022136641703639, 89.28841826848275787 ) ) ;
#67635 = CARTESIAN_POINT ( 'NONE',  ( 86.62931800182293784, -170.0000000000000000, -50.82156419891174437 ) ) ;
#67636 = CARTESIAN_POINT ( 'NONE',  ( -190.6985136298601731, 109.1272424661242582, 60.81597207375692449 ) ) ;
#67637 = CARTESIAN_POINT ( 'NONE',  ( 135.3579907212798901, 42.33677458448931930, -89.82451751908253357 ) ) ;
#67638 = CARTESIAN_POINT ( 'NONE',  ( 39.40195752203892710, 8.409560354027387774, -89.30891864635511013 ) ) ;
#67639 = CARTESIAN_POINT ( 'NONE',  ( 212.1325383547231525, 118.9860748747654640, 91.47708763404254739 ) ) ;
#67640 = CARTESIAN_POINT ( 'NONE',  ( 208.0306608271318680, 112.7988899307265740, 29.98561732425369897 ) ) ;
#67641 = CARTESIAN_POINT ( 'NONE',  ( 63.01563776193091826, -170.0000000000000000, -50.72069083216976537 ) ) ;
#67642 = CARTESIAN_POINT ( 'NONE',  ( -109.7290872258107157, 36.72869630780159156, 36.99980377389978514 ) ) ;
#67643 = EDGE_LOOP ( 'NONE', ( #61467, #43741, #44965, #21263 ) ) ;
#67644 = DIRECTION ( 'NONE',  ( -0.000000000000000000, 1.000000000000000000, -0.000000000000000000 ) ) ;
#67645 = ORIENTED_EDGE ( 'NONE', *, *, #27694, .T. ) ;
#67646 = CARTESIAN_POINT ( 'NONE',  ( 204.6977192012829789, 106.3443248447423599, -24.48138044215792419 ) ) ;
#67647 = EDGE_LOOP ( 'NONE', ( #38429, #50167, #5239, #24642 ) ) ;
#67648 = CARTESIAN_POINT ( 'NONE',  ( -144.7530445311634253, 61.54314312182903279, 5.570716979441686867 ) ) ;
#67649 = B_SPLINE_CURVE_WITH_KNOTS ( 'NONE', 3,
 ( #17061, #21658, #16389, #38897, #23061, #33276, #55054, #22011, #16723, #27978, #44860, #62428, #29722, #40615, #56108, #56808, #66684, #24798, #51532, #18823, #55767, #39928, #66344, #61386, #46235, #1964, #18478, #13208, #40280, #35350, #30077, #19161, #29044, #23421, #45202, #12864, #34672, #24460, #50830, #62067, #24111, #7924, #2308, #57153, #18133 ),
 .UNSPECIFIED., .F., .F.,
 ( 4, 2, 2, 2, 2, 2, 2, 2, 2, 2, 2, 2, 2, 1, 2, 2, 2, 2, 2, 2, 2, 2, 4 ),
 ( 0.02352719711393055912, 0.02499986300757016042, 0.02573619595438996974, 0.02647252890120978253, 0.02794519479484938035, 0.02941786068848897817, 0.03015419363530878749, 0.03089052658212860375, 0.03236319247576824321, 0.03309952542258805946, 0.03383585836940787572, 0.03530852426304752906, 0.03604485720986734532, 0.03678119015668715464, 0.03751752310350696396, 0.03825385605032678021, 0.03972652194396640579, 0.04119918783760603831, 0.04267185373124567083, 0.04340818667806546627, 0.04414451962488526171, 0.04561718551852485259, 0.04708985141216444348 ),
 .UNSPECIFIED. ) ;
#67650 = CARTESIAN_POINT ( 'NONE',  ( 188.0103583326377645, 87.39896620268125105, -67.67879652845185490 ) ) ;
#67651 = CARTESIAN_POINT ( 'NONE',  ( -145.3233446620410518, 62.00659513626053609, 71.30669210420751369 ) ) ;
#67652 = DIRECTION ( 'NONE',  ( 0.000000000000000000, 0.000000000000000000, 1.000000000000000000 ) ) ;
#67653 = CARTESIAN_POINT ( 'NONE',  ( 33.03722315490659867, 7.666819786578623841, -39.14476316943679990 ) ) ;
#67654 = CARTESIAN_POINT ( 'NONE',  ( -107.7893514267588415, 35.66840175773125310, 6.061804979893113732 ) ) ;
#67655 = CARTESIAN_POINT ( 'NONE',  ( 9.837735240994037511, 7.389327806910505281, -47.59081060985023015 ) ) ;
#67656 = CARTESIAN_POINT ( 'NONE',  ( 127.2202105166096402, 37.55913282978156786, -47.02660944393614528 ) ) ;
#67657 = EDGE_LOOP ( 'NONE', ( #10626, #69049, #23179, #55621 ) ) ;
#67658 = EDGE_CURVE ( 'NONE', #28608, #4543, #56301, .T. ) ;
#67660 = ORIENTED_EDGE ( 'NONE', *, *, #1349, .T. ) ;
#67659 = B_SPLINE_CURVE_WITH_KNOTS ( 'NONE', 3,
 ( #34009, #12910, #55810, #7277 ),
 .UNSPECIFIED., .F., .F.,
 ( 4, 4 ),
 ( 0.1259919275528362803, 0.1829744153748757984 ),
 .UNSPECIFIED. ) ;
#67661 = ADVANCED_FACE ( 'NONE', ( #30967 ), #4907, .F. ) ;
#67662 = DIRECTION ( 'NONE',  ( 2.497525279955783991E-16, 1.121639896553914790E-17, 1.000000000000000000 ) ) ;
#67663 = CARTESIAN_POINT ( 'NONE',  ( 0.000000000000000000, 0.000000000000000000, 170.0000000000000000 ) ) ;
#67664 = ADVANCED_FACE ( 'NONE', ( #26027 ), #47459, .F. ) ;
#67665 = CARTESIAN_POINT ( 'NONE',  ( -24.93568128341082968, 8.613819379861709535, -65.89388286627800539 ) ) ;
#67667 = EDGE_CURVE ( 'NONE', #36637, #17944, #62966, .T. ) ;
#67666 = UNCERTAINTY_MEASURE_WITH_UNIT (LENGTH_MEASURE( 1.000000000000000082E-05 ), #33451, 'distance_accuracy_value', 'NONE');
#67668 = VECTOR ( 'NONE', #51261, 1000.000000000000000 ) ;
#67669 = CARTESIAN_POINT ( 'NONE',  ( 13.14401442664830810, 6.430459733718340232, 17.69285561637535409 ) ) ;
#67670 = FACE_OUTER_BOUND ( 'NONE', #21835, .T. ) ;
#67671 = DIRECTION ( 'NONE',  ( 1.000000000000000000, -4.352074256530614270E-14, 0.000000000000000000 ) ) ;
#67672 = CARTESIAN_POINT ( 'NONE',  ( 210.0122310839192039, 115.7355030290287630, 15.17826746070574373 ) ) ;
#67673 = CIRCLE ( 'NONE', #15932, 243.4957430088094839 ) ;
#67674 = CARTESIAN_POINT ( 'NONE',  ( -59.94154301275507635, -45.09516516490467808, 170.0000000000000000 ) ) ;
#67675 = CARTESIAN_POINT ( 'NONE',  ( 94.12988949694086216, 22.11811104795078009, -16.24132341548559921 ) ) ;
#67676 = CARTESIAN_POINT ( 'NONE',  ( -23.98747857548121232, 9.501432345103353327, 65.54625325806455294 ) ) ;
#67677 = DIRECTION ( 'NONE',  ( 1.000000000000000000, -2.753353101070388220E-14, 0.000000000000000000 ) ) ;
#67678 = CARTESIAN_POINT ( 'NONE',  ( -49.43915770973591606, 13.24768844696976089, 69.65966800992838159 ) ) ;
#67679 = AXIS2_PLACEMENT_3D ( 'NONE', #17892, #61825, #34773 ) ;
#67680 = EDGE_CURVE ( 'NONE', #7537, #21176, #14090, .T. ) ;
#67681 = EDGE_CURVE ( 'NONE', #54939, #48080, #9854, .T. ) ;
#67682 = CARTESIAN_POINT ( 'NONE',  ( -3.252497086158844919, 6.636017118948018378, 58.49502237739417154 ) ) ;
#67683 = VERTEX_POINT ( 'NONE', #47124 ) ;
#67684 = EDGE_CURVE ( 'NONE', #20962, #66740, #15126, .T. ) ;
#67685 = DIRECTION ( 'NONE',  ( -1.000000000000000000, 0.000000000000000000, 0.000000000000000000 ) ) ;
#67686 = AXIS2_PLACEMENT_3D ( 'NONE', #16465, #61116, #18208 ) ;
#67687 = CARTESIAN_POINT ( 'NONE',  ( 152.1381498073141358, 54.87048121475570639, 58.45773527022319627 ) ) ;
#67688 = CARTESIAN_POINT ( 'NONE',  ( 75.00000000000000000, -1.250000000000021094, 170.0000000000000000 ) ) ;
#67689 = CARTESIAN_POINT ( 'NONE',  ( -49.14234466229832776, 13.17605306081208560, -47.33992328543903483 ) ) ;
#67690 = DIRECTION ( 'NONE',  ( -1.000000000000000000, 0.000000000000000000, 0.000000000000000000 ) ) ;
#67691 = LINE ( 'NONE', #47244, #29991 ) ;
#67692 = EDGE_LOOP ( 'NONE', ( #43059, #17649, #55407, #36117 ) ) ;
#67693 = CARTESIAN_POINT ( 'NONE',  ( -15.67984581961064450, 63.08044415722863363, 40.00000000000003553 ) ) ;
#67694 = CARTESIAN_POINT ( 'NONE',  ( -46.66904755831212981, -10.55634918610397222, 2.000000000000001776 ) ) ;
#67695 = VERTEX_POINT ( 'NONE', #46091 ) ;
#67696 = ORIENTED_EDGE ( 'NONE', *, *, #65858, .F. ) ;
#67697 = CARTESIAN_POINT ( 'NONE',  ( 179.4279766878530324, 76.94722012158234747, -51.05200850905019649 ) ) ;
#67698 = DIRECTION ( 'NONE',  ( 0.000000000000000000, 0.000000000000000000, 1.000000000000000000 ) ) ;
#67699 = DIRECTION ( 'NONE',  ( 0.000000000000000000, 1.000000000000000000, -0.000000000000000000 ) ) ;
#67700 = ORIENTED_EDGE ( 'NONE', *, *, #791, .F. ) ;
#67701 = CARTESIAN_POINT ( 'NONE',  ( -66.50000000000000000, 8.143901214329899974E-15, -0.002000000000002000178 ) ) ;
#67702 = CARTESIAN_POINT ( 'NONE',  ( 311.9975424824652350, 172.0000000000000284, 420.0000000000000568 ) ) ;
#67703 = CARTESIAN_POINT ( 'NONE',  ( -7.825402957745083654, 6.891034867348166060, 3.271030448983516692 ) ) ;
#67704 = DIRECTION ( 'NONE',  ( 0.000000000000000000, 1.000000000000000000, -1.479221584281239571E-31 ) ) ;
#67705 = CARTESIAN_POINT ( 'NONE',  ( -85.36298448216594181, 26.07611629625834127, 41.33332117284104612 ) ) ;
#67706 = CARTESIAN_POINT ( 'NONE',  ( -31.43908319763709969, 10.61114334766716105, -23.47264677473818395 ) ) ;
#67707 = CARTESIAN_POINT ( 'NONE',  ( 137.3958226571047021, 43.60243650158410844, 3.536823183464083087 ) ) ;
#67708 = VERTEX_POINT ( 'NONE', #14772 ) ;
#67709 = CARTESIAN_POINT ( 'NONE',  ( 116.6457744947906576, 31.95847117670280113, -47.33623488816716218 ) ) ;
#67710 = CARTESIAN_POINT ( 'NONE',  ( 8.288451200428832877, 6.376395059685424194, 64.85115452999926333 ) ) ;
#67711 = DIRECTION ( 'NONE',  ( -1.000000000000000000, -0.000000000000000000, -0.000000000000000000 ) ) ;
#67712 = CARTESIAN_POINT ( 'NONE',  ( -72.19799221038252313, 21.02813487613374477, 87.79774528419648050 ) ) ;
#67714 = VERTEX_POINT ( 'NONE', #68917 ) ;
#67713 = CARTESIAN_POINT ( 'NONE',  ( 447.3372781065084496, 399.9999999999998863, 113.5502958579881465 ) ) ;
#67715 = DIRECTION ( 'NONE',  ( -0.2225209339563042066, -0.9749279121818259508, 0.000000000000000000 ) ) ;
#67716 = ORIENTED_EDGE ( 'NONE', *, *, #67334, .F. ) ;
#67717 = AXIS2_PLACEMENT_3D ( 'NONE', #32215, #52955, #31189 ) ;
#67718 = VERTEX_POINT ( 'NONE', #40817 ) ;
#67719 = MECHANICAL_DESIGN_GEOMETRIC_PRESENTATION_REPRESENTATION (  '', ( #24993 ), #16028 ) ;
#67720 = CARTESIAN_POINT ( 'NONE',  ( -143.8566410313463564, 59.53044870492035301, 70.02296563317230493 ) ) ;
#67721 = DIRECTION ( 'NONE',  ( 1.000000000000000000, 0.000000000000000000, -0.000000000000000000 ) ) ;
#67722 = DIRECTION ( 'NONE',  ( -1.000000000000000000, 0.000000000000000000, 0.000000000000000000 ) ) ;
#67723 = LINE ( 'NONE', #56459, #31660 ) ;
#67724 = AXIS2_PLACEMENT_3D ( 'NONE', #19555, #68105, #13932 ) ;
#67725 = CARTESIAN_POINT ( 'NONE',  ( -123.4416615615272974, 44.90042688650400038, 72.05607892409608439 ) ) ;
#67726 = LINE ( 'NONE', #57167, #41147 ) ;
#67727 = DIRECTION ( 'NONE',  ( 0.000000000000000000, 0.000000000000000000, 1.000000000000000000 ) ) ;
#67728 = CONICAL_SURFACE ( 'NONE', #16189, 74.95140232871122521, 0.8777644062502172329 ) ;
#67729 = CARTESIAN_POINT ( 'NONE',  ( -47.80251179448168841, 13.89045662648309154, 39.80133545766267389 ) ) ;
#67730 = ORIENTED_EDGE ( 'NONE', *, *, #6986, .T. ) ;
#67731 = VERTEX_POINT ( 'NONE', #68588 ) ;
#67732 = CARTESIAN_POINT ( 'NONE',  ( 412.0000000000000000, 0.000000000000000000, 380.0000000000000000 ) ) ;
#67733 = CARTESIAN_POINT ( 'NONE',  ( 105.4193882736795871, 26.71329717705293305, 58.19139437044036356 ) ) ;
#67734 = AXIS2_PLACEMENT_3D ( 'NONE', #12880, #55783, #54363 ) ;
#67735 = CARTESIAN_POINT ( 'NONE',  ( 164.9709596662455340, 63.72607097915128094, 64.01767799798439285 ) ) ;
#67736 = CARTESIAN_POINT ( 'NONE',  ( 259.4165763529819060, 225.8585178651493948, 138.9999999999999716 ) ) ;
#67737 = CARTESIAN_POINT ( 'NONE',  ( -60.67627457812130132, 44.08389392193514311, 43.58025477438756212 ) ) ;
#67738 = DIRECTION ( 'NONE',  ( -1.000000000000000000, 0.000000000000000000, 0.000000000000000000 ) ) ;
#67739 = CARTESIAN_POINT ( 'NONE',  ( 164.0298848570287191, 62.93631132702880393, -66.79358054371351727 ) ) ;
#67740 = EDGE_LOOP ( 'NONE', ( #18966, #45108, #14319, #28346 ) ) ;
#67741 = EDGE_LOOP ( 'NONE', ( #27645, #1496 ) ) ;
#67742 = ADVANCED_FACE ( 'NONE', ( #67560 ), #35892, .T. ) ;
#67743 = ORIENTED_EDGE ( 'NONE', *, *, #35948, .F. ) ;
#67744 = CARTESIAN_POINT ( 'NONE',  ( 442.3372781065085633, 400.0000000000000568, -116.4497041420118393 ) ) ;
#67745 = EDGE_CURVE ( 'NONE', #39369, #23191, #59901, .T. ) ;
#67746 = CARTESIAN_POINT ( 'NONE',  ( -78.66644367742111399, 22.32174330031318377, 57.26275173013680586 ) ) ;
#67747 = CARTESIAN_POINT ( 'NONE',  ( 444.9999999999999432, 225.0000000000000000, 378.0000000000000000 ) ) ;
#67748 = CARTESIAN_POINT ( 'NONE',  ( 105.0330373230561918, -21.99242646597928896, 0.6602422734858272024 ) ) ;
#67749 = CARTESIAN_POINT ( 'NONE',  ( -56.02289203441037557, 15.98631679403369965, 45.27020485907997482 ) ) ;
#67750 = EDGE_CURVE ( 'NONE', #21034, #47508, #10180, .T. ) ;
#67751 = CARTESIAN_POINT ( 'NONE',  ( -33.12994257348895388, 10.89587983539684934, -76.97276311505544300 ) ) ;
#67752 = CARTESIAN_POINT ( 'NONE',  ( 33.03722315490661998, 7.666819786578624729, 68.23343919241794708 ) ) ;
#67753 = CARTESIAN_POINT ( 'NONE',  ( 9.823983574062877366, 6.382904402091118534, -20.74781057506424631 ) ) ;
#67754 = SHAPE_REPRESENTATION_RELATIONSHIP ( 'NONE' , 'NONE' ,  #15003, #21404 ) ;
#67755 = ORIENTED_EDGE ( 'NONE', *, *, #52351, .T. ) ;
#67756 = CARTESIAN_POINT ( 'NONE',  ( -2.355184675731019528, 6.596450510445359683, -48.05484883106331040 ) ) ;
#67757 = CARTESIAN_POINT ( 'NONE',  ( 26.11269837220812562, 31.11269837220800483, 2.000000000000000000 ) ) ;
#67758 = DIRECTION ( 'NONE',  ( 0.000000000000000000, -0.000000000000000000, -1.000000000000000000 ) ) ;
#67759 = CARTESIAN_POINT ( 'NONE',  ( 63.98971758354224448, 12.90030016320049100, -62.61274705208756330 ) ) ;
#67760 = CARTESIAN_POINT ( 'NONE',  ( 133.8566784816069344, 41.42467568809809109, -24.17876034193199786 ) ) ;
#67761 = CARTESIAN_POINT ( 'NONE',  ( 23.09590709048884349, 7.852755081912510704, -14.46865910473645656 ) ) ;
#67762 = CARTESIAN_POINT ( 'NONE',  ( -109.5142642360664382, 36.61018064014775319, -71.40685367841822995 ) ) ;
#67763 = ADVANCED_FACE ( 'NONE', ( #57006 ), #52738, .F. ) ;
#67764 = B_SPLINE_CURVE_WITH_KNOTS ( 'NONE', 3,
 ( #4579, #26044, #47475, #1039, #48846, #59070, #38313, #42886, #15825, #32012, #38670, #58720, #37973, #26730, #43586, #27060, #21440, #54837, #59417, #65408, #53440, #48159, #18708, #64351, #22138, #16164, #10535, #37618, #60116, #49202, #11936, #17198, #64014, #22490, #10887, #33408, #5604, #5270, #16856, #6658, #32358, #28108, #53782, #49551 ),
 .UNSPECIFIED., .F., .F.,
 ( 4, 2, 2, 2, 2, 2, 2, 2, 2, 2, 2, 2, 2, 2, 2, 2, 2, 2, 2, 2, 2, 4 ),
 ( 0.000000000000000000, 0.001473754749730514079, 0.002210632124595768300, 0.002947509499461028158, 0.004421264249191557416, 0.005895018998922086674, 0.007368773748652615065, 0.008105651123517878393, 0.008842528498383139118, 0.01031628324811366230, 0.01179003799784418549, 0.01252691537270942887, 0.01326379274757467051, 0.01473754749730515207, 0.01547442487217037463, 0.01621130224703559719, 0.01768505699676600762, 0.01915881174649641458, 0.01989568912136160939, 0.02063256649622680419, 0.02210632124595719034, 0.02358007599568757648 ),
 .UNSPECIFIED. ) ;
#67765 = VERTEX_POINT ( 'NONE', #57695 ) ;
#67766 = CIRCLE ( 'NONE', #64372, 25.12245591505646303 ) ;
#67767 = PRODUCT_CONTEXT ( 'NONE', #38134, 'mechanical' ) ;
#67768 = CARTESIAN_POINT ( 'NONE',  ( 130.3281282802763315, 40.49854652972196334, -50.15829713770070697 ) ) ;
#67769 = DIRECTION ( 'NONE',  ( -1.000000000000000000, 0.000000000000000000, 0.000000000000000000 ) ) ;
#67770 = PLANE ( 'NONE',  #14383 ) ;
#67771 = CARTESIAN_POINT ( 'NONE',  ( 188.5838389098763059, 88.03667982118678026, -43.41585238266635827 ) ) ;
#67772 = ORIENTED_EDGE ( 'NONE', *, *, #54937, .F. ) ;
#67773 = AXIS2_PLACEMENT_3D ( 'NONE', #15718, #54013, #58275 ) ;
#67774 = EDGE_LOOP ( 'NONE', ( #8713, #19068 ) ) ;
#67775 = VECTOR ( 'NONE', #38386, 1000.000000000000000 ) ;
#67776 = LINE ( 'NONE', #35764, #11143 ) ;
#67777 = VECTOR ( 'NONE', #22584, 1000.000000000000000 ) ;
#67778 = CARTESIAN_POINT ( 'NONE',  ( -60.00000000000000000, 7.347880794884118356E-15, 10.00000000000000000 ) ) ;
#67779 = VERTEX_POINT ( 'NONE', #42202 ) ;
#67780 = CARTESIAN_POINT ( 'NONE',  ( 164.2142767676857318, 64.40413161136414999, 87.29693986084237167 ) ) ;
#67781 = ORIENTED_EDGE ( 'NONE', *, *, #44934, .F. ) ;
#67782 = CARTESIAN_POINT ( 'NONE',  ( -62.14837099232445894, 17.75045801599140560, 13.41502600278767154 ) ) ;
#67783 = LINE ( 'NONE', #8348, #54110 ) ;
#67784 = CARTESIAN_POINT ( 'NONE',  ( -151.2511071212631464, 67.00426547928871912, 45.52856916683464306 ) ) ;
#67785 = VECTOR ( 'NONE', #58206, 1000.000000000000000 ) ;
#67786 = CARTESIAN_POINT ( 'NONE',  ( -99.98930671699733352, 31.63190627461932181, 30.86207369873248041 ) ) ;
#67787 = DIRECTION ( 'NONE',  ( 0.000000000000000000, 0.000000000000000000, -1.000000000000000000 ) ) ;
#67789 = VERTEX_POINT ( 'NONE', #25352 ) ;
#67788 = CARTESIAN_POINT ( 'NONE',  ( 76.57571471437145760, 0.000000000000000000, -20.00000000000000000 ) ) ;
#67790 = CARTESIAN_POINT ( 'NONE',  ( 56.19211641164835669, 11.19288081156168246, 34.19031576763088509 ) ) ;
#67791 = ORIENTED_EDGE ( 'NONE', *, *, #35206, .F. ) ;
#67792 = ORIENTED_EDGE ( 'NONE', *, *, #50417, .F. ) ;
#67793 = CARTESIAN_POINT ( 'NONE',  ( -170.2951623264596606, 85.51757001115471724, 18.43718488514699416 ) ) ;
#67794 = CARTESIAN_POINT ( 'NONE',  ( 23.03578842369136481, 6.840884649289441732, -71.80884623865955518 ) ) ;
#67796 = ORIENTED_EDGE ( 'NONE', *, *, #37465, .T. ) ;
#67795 = CYLINDRICAL_SURFACE ( 'NONE', #39940, 5.000000000000000888 ) ;
#67797 = CYLINDRICAL_SURFACE ( 'NONE', #30849, 10.00000000000000178 ) ;
#67798 = CARTESIAN_POINT ( 'NONE',  ( 157.4703587214989113, 57.65129005721576760, -51.12418429913766005 ) ) ;
#67799 = EDGE_LOOP ( 'NONE', ( #59469, #50219, #102, #66452, #18052, #21675 ) ) ;
#67800 = EDGE_CURVE ( 'NONE', #35639, #10115, #67913, .T. ) ;
#67801 = CARTESIAN_POINT ( 'NONE',  ( 211.7318474105134385, 118.3631723164074714, -73.28989541382324546 ) ) ;
#67802 = CARTESIAN_POINT ( 'NONE',  ( 137.6104751318277408, 44.92718313329108071, 30.51303313971197895 ) ) ;
#67803 = FACE_OUTER_BOUND ( 'NONE', #67060, .T. ) ;
#67804 = CARTESIAN_POINT ( 'NONE',  ( 563.4809901518626702, 2.000000000000001776, 57.79371821540657095 ) ) ;
#67805 = CARTESIAN_POINT ( 'NONE',  ( -102.2801239173131052, 32.78103895658057354, -76.85912785543962400 ) ) ;
#67806 = ORIENTED_EDGE ( 'NONE', *, *, #27885, .F. ) ;
#67807 = ORIENTED_EDGE ( 'NONE', *, *, #45276, .T. ) ;
#67808 = COLOUR_RGB ( '',0.7921568627450980005, 0.8196078431372548767, 0.9333333333333333481 ) ;
#67809 = FACE_OUTER_BOUND ( 'NONE', #18803, .T. ) ;
#67810 = CARTESIAN_POINT ( 'NONE',  ( -121.5680658099883829, 44.89994870382100345, -48.55882814402620795 ) ) ;
#67811 = DIRECTION ( 'NONE',  ( 1.110223024625156294E-16, 0.000000000000000000, -1.000000000000000000 ) ) ;
#67812 = CARTESIAN_POINT ( 'NONE',  ( -48.39076722402981545, 12.99581395652485405, -92.93256446017095129 ) ) ;
#67813 = DIRECTION ( 'NONE',  ( -0.000000000000000000, -1.000000000000000000, 0.000000000000000000 ) ) ;
#67814 = CARTESIAN_POINT ( 'NONE',  ( 0.000000000000000000, 0.000000000000000000, 0.000000000000000000 ) ) ;
#67815 = CARTESIAN_POINT ( 'NONE',  ( 67.93317348534930034, 14.90531593353392026, -37.53674462394790368 ) ) ;
#67817 = EDGE_CURVE ( 'NONE', #62563, #50848, #36927, .T. ) ;
#67816 = VECTOR ( 'NONE', #58130, 1000.000000000000000 ) ;
#67818 = CARTESIAN_POINT ( 'NONE',  ( -118.6302575928420566, 43.07263081214308897, 40.00705528920811105 ) ) ;
#67819 = CARTESIAN_POINT ( 'NONE',  ( 207.8484262634767106, 110.7633525054914259, 56.73326111006115013 ) ) ;
#67820 = ORIENTED_EDGE ( 'NONE', *, *, #6991, .T. ) ;
#67822 = CARTESIAN_POINT ( 'NONE',  ( -106.6711220790662651, 36.20923238211246797, 31.93402958823944715 ) ) ;
#67821 = CIRCLE ( 'NONE', #3791, 10.00000000000000178 ) ;
#67823 = ADVANCED_FACE ( 'NONE', ( #25002 ), #41172, .T. ) ;
#67824 = EDGE_LOOP ( 'NONE', ( #45771, #27345, #17450, #14042 ) ) ;
#67825 = CARTESIAN_POINT ( 'NONE',  ( 82.80776120605499102, 19.20888523483863963, -90.50563713883087757 ) ) ;
#67826 = VECTOR ( 'NONE', #55215, 1000.000000000000000 ) ;
#67827 = DIRECTION ( 'NONE',  ( -1.000000000000000000, 0.000000000000000000, 0.000000000000000000 ) ) ;
#67828 = ORIENTED_EDGE ( 'NONE', *, *, #58111, .T. ) ;
#67829 = CARTESIAN_POINT ( 'NONE',  ( 8.000000000000007105, 249.8719672152120381, -95.00000000000133582 ) ) ;
#67830 = DIRECTION ( 'NONE',  ( 1.000000000000000000, 0.000000000000000000, 0.000000000000000000 ) ) ;
#67831 = CARTESIAN_POINT ( 'NONE',  ( 37.70910994512003356, 9.209110272746713122, 3.258713980646935404 ) ) ;
#67832 = DIRECTION ( 'NONE',  ( -1.000000000000000000, 0.000000000000000000, 0.000000000000000000 ) ) ;
#67833 = CARTESIAN_POINT ( 'NONE',  ( 35.65685430025423841, 7.951642554322393863, 17.08570462602523321 ) ) ;
#67834 = CARTESIAN_POINT ( 'NONE',  ( -15.07533778868020491, 8.482826962130840087, -40.98183384572956811 ) ) ;
#67835 = AXIS2_PLACEMENT_3D ( 'NONE', #37347, #68675, #57786 ) ;
#67836 = EDGE_CURVE ( 'NONE', #44768, #39465, #36238, .T. ) ;
#67837 = CARTESIAN_POINT ( 'NONE',  ( -35.17718245314463843, 11.25729435722175964, -9.466008116007795792 ) ) ;
#67838 = VERTEX_POINT ( 'NONE', #9159 ) ;
#67839 = DIRECTION ( 'NONE',  ( 0.000000000000000000, 0.000000000000000000, 1.000000000000000000 ) ) ;
#67840 = ORIENTED_EDGE ( 'NONE', *, *, #33424, .T. ) ;
#67841 = CARTESIAN_POINT ( 'NONE',  ( -46.66904755831210139, 5.000000000000066613, 0.000000000000000000 ) ) ;
#67842 = CARTESIAN_POINT ( 'NONE',  ( -55.05276343752908730, 15.72344139423348430, 72.16187836339486239 ) ) ;
#67843 = CARTESIAN_POINT ( 'NONE',  ( -190.0468231512976445, 108.2116162189844744, 8.178919575991894675 ) ) ;
#67844 = ORIENTED_EDGE ( 'NONE', *, *, #62884, .F. ) ;
#67845 = CARTESIAN_POINT ( 'NONE',  ( 57.16566303090297652, -11.64445445351497277, 27.58472315868179692 ) ) ;
#67846 = CARTESIAN_POINT ( 'NONE',  ( 254.4165763529819344, 225.8585178651493948, 138.9999999999999716 ) ) ;
#67847 = CARTESIAN_POINT ( 'NONE',  ( -31.93184248720558926, 9.672312402099827011, 45.21645440618920020 ) ) ;
#67848 = CARTESIAN_POINT ( 'NONE',  ( 155.2870855780215038, 57.23765125306422163, -36.43485218074236087 ) ) ;
#67849 =( REPRESENTATION_RELATIONSHIP ('NONE','NONE', #40274, #64096 ) REPRESENTATION_RELATIONSHIP_WITH_TRANSFORMATION ( #13265 )SHAPE_REPRESENTATION_RELATIONSHIP( ) );
#67850 = EDGE_CURVE ( 'NONE', #30492, #16812, #2693, .T. ) ;
#67851 = ORIENTED_EDGE ( 'NONE', *, *, #632, .T. ) ;
#67852 = CARTESIAN_POINT ( 'NONE',  ( 848.0071894358269446, 1011.991584617519379, 569.0068267248692564 ) ) ;
#67853 = CARTESIAN_POINT ( 'NONE',  ( -156.1477286774994298, 71.38742644140636173, 68.56236523163960328 ) ) ;
#67854 = EDGE_CURVE ( 'NONE', #54785, #24463, #309, .T. ) ;
#67855 = EDGE_CURVE ( 'NONE', #56615, #11952, #5926, .T. ) ;
#67856 = CARTESIAN_POINT ( 'NONE',  ( -118.4063383664799574, 41.75753822095644097, 38.63033520264055198 ) ) ;
#67857 = CARTESIAN_POINT ( 'NONE',  ( 0.000000000000000000, 0.000000000000000000, 170.0000000000000000 ) ) ;
#67858 = ORIENTED_EDGE ( 'NONE', *, *, #29092, .T. ) ;
#67859 = CARTESIAN_POINT ( 'NONE',  ( -174.7903139851460139, 90.53182997092832807, -61.73254058746562123 ) ) ;
#67860 = CARTESIAN_POINT ( 'NONE',  ( 127.0856473832366049, 38.63797330894008297, 87.46917552659634509 ) ) ;
#67861 = CARTESIAN_POINT ( 'NONE',  ( 117.4830770399667585, 32.37795270233553424, 39.13512077466761951 ) ) ;
#67862 = CARTESIAN_POINT ( 'NONE',  ( 412.3372781065086201, 400.0000000000000568, -146.4497041420118251 ) ) ;
#67863 = CIRCLE ( 'NONE', #37500, 65.36598343705435354 ) ;
#67864 = CARTESIAN_POINT ( 'NONE',  ( -118.9468627709229338, 42.08677365399184822, -66.41956046915954914 ) ) ;
#67865 = VERTEX_POINT ( 'NONE', #59052 ) ;
#67866 = CARTESIAN_POINT ( 'NONE',  ( 203.1420903260745945, 104.2307086582027154, 44.08919628120091261 ) ) ;
#67867 = DIRECTION ( 'NONE',  ( -0.000000000000000000, -0.000000000000000000, -1.000000000000000000 ) ) ;
#67868 = CARTESIAN_POINT ( 'NONE',  ( 187.2384682876461852, 86.54721710842891014, 41.12445451989140821 ) ) ;
#67869 = CARTESIAN_POINT ( 'NONE',  ( 185.4689022896543804, 83.15310303704600869, -91.31778852048856265 ) ) ;
#67870 = CARTESIAN_POINT ( 'NONE',  ( 44.99999999999999289, -22.99999999999998579, 0.000000000000000000 ) ) ;
#67871 = AXIS2_PLACEMENT_3D ( 'NONE', #35217, #4254, #37273 ) ;
#67872 = ORIENTED_EDGE ( 'NONE', *, *, #58904, .T. ) ;
#67873 = VECTOR ( 'NONE', #63061, 1000.000000000000000 ) ;
#67874 = CARTESIAN_POINT ( 'NONE',  ( 160.5018603162735360, 61.33906090758087970, -23.65429127533722209 ) ) ;
#67875 = AXIS2_PLACEMENT_3D ( 'NONE', #67354, #8608, #61367 ) ;
#67876 = ORIENTED_EDGE ( 'NONE', *, *, #61637, .T. ) ;
#67877 = CARTESIAN_POINT ( 'NONE',  ( 66.07923263163412742, 14.44036440557998091, 57.30743532950679509 ) ) ;
#67878 = CARTESIAN_POINT ( 'NONE',  ( 128.2147605031037472, 38.12058270760483936, 85.74602399063695657 ) ) ;
#67879 = AXIS2_PLACEMENT_3D ( 'NONE', #53297, #31523, #16024 ) ;
#67880 = VECTOR ( 'NONE', #37708, 1000.000000000000227 ) ;
#67882 = ORIENTED_EDGE ( 'NONE', *, *, #60582, .T. ) ;
#67881 = DIRECTION ( 'NONE',  ( 0.000000000000000000, 0.000000000000000000, 1.000000000000000000 ) ) ;
#67883 = CARTESIAN_POINT ( 'NONE',  ( 162.0862735437575566, 62.63196145447161456, -49.55485834045765614 ) ) ;
#67884 = LINE ( 'NONE', #66505, #49626 ) ;
#67885 = CARTESIAN_POINT ( 'NONE',  ( 157.4703587214989113, 57.65129005721576760, -51.12418429913766005 ) ) ;
#67886 = ORIENTED_EDGE ( 'NONE', *, *, #31290, .T. ) ;
#67887 = ADVANCED_FACE ( 'NONE', ( #43909 ), #48474, .F. ) ;
#67888 = CARTESIAN_POINT ( 'NONE',  ( -95.88693721180811735, 30.76307528361165922, 15.10402982153757989 ) ) ;
#67889 = CARTESIAN_POINT ( 'NONE',  ( -130.1964689553232688, 49.39217932424202218, 44.28062280936351414 ) ) ;
#67890 = EDGE_CURVE ( 'NONE', #13335, #63326, #6288, .T. ) ;
#67891 = DIRECTION ( 'NONE',  ( -0.000000000000000000, -0.000000000000000000, -1.000000000000000000 ) ) ;
#67892 = CARTESIAN_POINT ( 'NONE',  ( -74.81012118577218928, -5.477980300263997293, 170.0000000000000000 ) ) ;
#67893 = CARTESIAN_POINT ( 'NONE',  ( 442.3372781065085633, 367.0710678118655892, -141.4497041420118251 ) ) ;
#67894 = CARTESIAN_POINT ( 'NONE',  ( 151.6192474229129061, 53.24103268919208887, 59.05513162150372608 ) ) ;
#67895 = CARTESIAN_POINT ( 'NONE',  ( 93.32756701508620267, 22.89083686918420568, 40.62277632368491709 ) ) ;
#67896 = ORIENTED_EDGE ( 'NONE', *, *, #18453, .T. ) ;
#67897 = CARTESIAN_POINT ( 'NONE',  ( -99.10674985723790087, 32.31836975419496838, 58.05168674522651884 ) ) ;
#67898 = CARTESIAN_POINT ( 'NONE',  ( -14.56151485655250255, 8.434196591921336861, 61.12604529331529335 ) ) ;
#67899 = ORIENTED_EDGE ( 'NONE', *, *, #21731, .T. ) ;
#67900 = PLANE ( 'NONE',  #58695 ) ;
#67901 = DIRECTION ( 'NONE',  ( -0.000000000000000000, -0.000000000000000000, -1.000000000000000000 ) ) ;
#67902 = CARTESIAN_POINT ( 'NONE',  ( 102.7983318509014907, 26.68040613344516032, 36.06500074359141905 ) ) ;
#67903 = CARTESIAN_POINT ( 'NONE',  ( -1.454841858088672391, 7.566772088227303072, 33.65001273355291289 ) ) ;
#67904 = CARTESIAN_POINT ( 'NONE',  ( 56.30971345544048035, 11.21639176274772431, 94.42806938231223057 ) ) ;
#67905 = CARTESIAN_POINT ( 'NONE',  ( 186.5979919519638202, 85.84756789133382426, 15.05375570133903551 ) ) ;
#67906 = EDGE_CURVE ( 'NONE', #56869, #65730, #43566, .T. ) ;
#67907 = CARTESIAN_POINT ( 'NONE',  ( 209.6525588430077960, 113.3929734759396837, -49.46103483128387523 ) ) ;
#67908 = CARTESIAN_POINT ( 'NONE',  ( 177.7960900018545090, 75.34533826015461955, 16.70855730554400154 ) ) ;
#67910 = EDGE_CURVE ( 'NONE', #61402, #2404, #53421, .T. ) ;
#67909 = CARTESIAN_POINT ( 'NONE',  ( -58.76006735892197952, 15.70681061434693326, 4.448567267148194837 ) ) ;
#67911 = ORIENTED_EDGE ( 'NONE', *, *, #44720, .T. ) ;
#67912 = AXIS2_PLACEMENT_3D ( 'NONE', #56898, #29119, #8365 ) ;
#67913 = LINE ( 'NONE', #19361, #8267 ) ;
#67914 = ORIENTED_EDGE ( 'NONE', *, *, #6319, .F. ) ;
#67915 = CARTESIAN_POINT ( 'NONE',  ( 102.7435092758397843, 25.56449004647816992, -69.99619280892473228 ) ) ;
#67916 = ADVANCED_FACE ( 'NONE', ( #32340 ), #42541, .T. ) ;
#67917 = DIRECTION ( 'NONE',  ( -1.000000000000000000, 0.000000000000000000, 0.000000000000000000 ) ) ;
#67918 = VECTOR ( 'NONE', #22405, 1000.000000000000000 ) ;
#67919 = CARTESIAN_POINT ( 'NONE',  ( -75.01314391403411719, 20.96328762434825066, 4.505560061529784832 ) ) ;
#67920 = LINE ( 'NONE', #35554, #58107 ) ;
#67921 = CARTESIAN_POINT ( 'NONE',  ( -6.538175632604766641, 6.809790034551946647, 83.88688884445680571 ) ) ;
#67922 = CARTESIAN_POINT ( 'NONE',  ( 0.000000000000000000, 0.000000000000000000, 170.0000000000000000 ) ) ;
#67923 = ORIENTED_EDGE ( 'NONE', *, *, #35646, .F. ) ;
#67924 = CARTESIAN_POINT ( 'NONE',  ( -73.81689110552356681, 20.53332132481499883, 59.03636908666045713 ) ) ;
#67925 = CARTESIAN_POINT ( 'NONE',  ( -165.6210506643949145, 79.15024150453835716, 65.46751455689062027 ) ) ;
#67926 = EDGE_LOOP ( 'NONE', ( #25052, #64335, #68600, #5852 ) ) ;
#67927 = VECTOR ( 'NONE', #65138, 1000.000000000000000 ) ;
#67928 = EDGE_LOOP ( 'NONE', ( #26211, #17616, #56111, #64759, #26887, #60781, #25750, #12846, #33770 ) ) ;
#67929 = VECTOR ( 'NONE', #4784, 1000.000000000000000 ) ;
#67930 = CARTESIAN_POINT ( 'NONE',  ( -152.2964402771108894, 66.58174574061952455, 45.18655382497220074 ) ) ;
#67931 = CYLINDRICAL_SURFACE ( 'NONE', #65908, 7.500000000000013323 ) ;
#67932 = CARTESIAN_POINT ( 'NONE',  ( 181.0840389613909736, 78.60582251573003987, -9.380507075415925655 ) ) ;
#67933 = VECTOR ( 'NONE', #24967, 1000.000000000000000 ) ;
#67934 = CARTESIAN_POINT ( 'NONE',  ( -20.55634918610400419, 15.55634918610405748, 85.00100000000000477 ) ) ;
#67935 = ORIENTED_EDGE ( 'NONE', *, *, #15575, .T. ) ;
#67936 = EDGE_CURVE ( 'NONE', #15508, #50826, #5588, .T. ) ;
#67937 = EDGE_CURVE ( 'NONE', #33294, #26166, #48144, .T. ) ;
#67938 = DIRECTION ( 'NONE',  ( 1.000000000000000000, 0.000000000000000000, 0.000000000000000000 ) ) ;
#67939 = EDGE_LOOP ( 'NONE', ( #54407, #15360, #44559, #62434 ) ) ;
#67940 = DIRECTION ( 'NONE',  ( 1.387778780781446169E-16, -1.000000000000000000, -3.469446951953615421E-17 ) ) ;
#67941 = CARTESIAN_POINT ( 'NONE',  ( 12.03162622199373821, 7.415834979634797541, 70.85525387039702139 ) ) ;
#67942 = CARTESIAN_POINT ( 'NONE',  ( 209.9944361927104808, 113.8994774711241433, 31.39268359782400353 ) ) ;
#67943 = CARTESIAN_POINT ( 'NONE',  ( 11.80882841624966773, 6.405741128846195842, -90.33718337654195807 ) ) ;
#67944 = EDGE_CURVE ( 'NONE', #53513, #46155, #4939, .T. ) ;
#67945 = VERTEX_POINT ( 'NONE', #15807 ) ;
#67946 = ORIENTED_EDGE ( 'NONE', *, *, #11204, .F. ) ;
#67947 = CARTESIAN_POINT ( 'NONE',  ( 112.2205320413088145, -21.53693364843037372, 4.491889980468759980 ) ) ;
#67948 = CARTESIAN_POINT ( 'NONE',  ( -118.6791382831902695, 43.10256062345757755, 89.73259551560695968 ) ) ;
#67949 = CARTESIAN_POINT ( 'NONE',  ( 32.15613847490628530, 8.588587416860168133, -71.91613580555670637 ) ) ;
#67950 = CARTESIAN_POINT ( 'NONE',  ( 309.8720357909272707, 172.0000000000000284, 256.6193948016162381 ) ) ;
#67951 = CARTESIAN_POINT ( 'NONE',  ( 11.74169691668609872, 6.404809784504847059, 84.88065130995101981 ) ) ;
#67952 = DIRECTION ( 'NONE',  ( 0.000000000000000000, 0.000000000000000000, -1.000000000000000000 ) ) ;
#67953 = ORIENTED_EDGE ( 'NONE', *, *, #68458, .T. ) ;
#67954 = DIRECTION ( 'NONE',  ( 0.9362348706397369824, 0.3513748240813435175, 0.000000000000000000 ) ) ;
#67955 = CARTESIAN_POINT ( 'NONE',  ( 199.7286177451875346, 101.4075663537892211, -49.46260000570829618 ) ) ;
#67956 = ORIENTED_EDGE ( 'NONE', *, *, #63552, .T. ) ;
#67957 = CARTESIAN_POINT ( 'NONE',  ( -83.69653436244854561, 24.30167057287991028, 16.64215499319238489 ) ) ;
#67958 = ORIENTED_EDGE ( 'NONE', *, *, #66739, .T. ) ;
#67959 = VECTOR ( 'NONE', #56903, 1000.000000000000000 ) ;
#67960 = FACE_OUTER_BOUND ( 'NONE', #39865, .T. ) ;
#67961 = ORIENTED_EDGE ( 'NONE', *, *, #22078, .T. ) ;
#67962 = VECTOR ( 'NONE', #59391, 1000.000000000000000 ) ;
#67963 = ORIENTED_EDGE ( 'NONE', *, *, #40510, .T. ) ;
#67964 = CARTESIAN_POINT ( 'NONE',  ( 9.057575839850585453, 6.378493414438676901, -39.70112296040927902 ) ) ;
#67965 = CARTESIAN_POINT ( 'NONE',  ( -109.1616641287093188, 37.56478347858660527, -93.21238446277425282 ) ) ;
#67966 = CARTESIAN_POINT ( 'NONE',  ( 16.27765348919937338, 6.516472002017813736, 3.170157082241544799 ) ) ;
#67967 = VECTOR ( 'NONE', #33199, 1000.000000000000000 ) ;
#67968 = AXIS2_PLACEMENT_3D ( 'NONE', #2692, #56152, #44563 ) ;
#67969 = B_SPLINE_CURVE_WITH_KNOTS ( 'NONE', 3,
 ( #39109, #44359, #34533, #55974, #66893, #7786, #40141, #8127, #38751, #12013, #33486, #6732, #28179, #68263, #25360, #46440, #13748, #30625, #46792, #51729, #29929, #52745, #3536, #15132, #62278, #56660, #4238, #52072, #14096, #20067, #67921, #19025, #9862, #61921, #57701, #51394, #25007, #40476, #57013, #31319, #19367, #47467, #35555, #8832, #36594, #41868, #9164, #46097, #41520, #25702, #19718, #20398, #41178, #67566, #9511 ),
 .UNSPECIFIED., .F., .F.,
 ( 4, 2, 2, 2, 2, 2, 2, 2, 2, 2, 2, 2, 2, 2, 2, 2, 2, 2, 2, 1, 2, 2, 2, 2, 2, 2, 2, 4 ),
 ( 0.000000000000000000, 0.001947696403339872848, 0.002921544605009829872, 0.003895392806679787330, 0.004869241008349744354, 0.005843089210019701378, 0.006816937411689658402, 0.007790785613359616293, 0.009738482016699530341, 0.01071233021836948823, 0.01168617842003944439, 0.01266002662170940228, 0.01363387482337935844, 0.01460772302504931806, 0.01558157122671927422, 0.01752926763005918306, 0.01850311583172913749, 0.01947696403339909191, 0.02045081223506904633, 0.02142466043673900075, 0.02239850863840895517, 0.02337235684007890613, 0.02434620504174886055, 0.02532005324341881497, 0.02726774964675867871, 0.02824159784842859497, 0.02921544605009850776, 0.03116314245343833333 ),
 .UNSPECIFIED. ) ;
#67970 = ORIENTED_EDGE ( 'NONE', *, *, #60306, .T. ) ;
#67971 = AXIS2_PLACEMENT_3D ( 'NONE', #51692, #30586, #36207 ) ;
#67972 = CARTESIAN_POINT ( 'NONE',  ( -31.77355346681724058, 9.646350159722794970, 83.90614663642915616 ) ) ;
#67973 = EDGE_CURVE ( 'NONE', #24549, #36560, #54817, .T. ) ;
#67974 = CARTESIAN_POINT ( 'NONE',  ( 173.6024011093111028, 72.73634049052010653, -71.17273619272620522 ) ) ;
#67975 = CIRCLE ( 'NONE', #572, 5.000000000000004441 ) ;
#67976 = CARTESIAN_POINT ( 'NONE',  ( -444.1126562889745060, 394.7876926391177790, -127.1788437718730194 ) ) ;
#67977 = CARTESIAN_POINT ( 'NONE',  ( 102.7435092758398270, 25.56449004647818413, -43.15164221846109172 ) ) ;
#67978 = CARTESIAN_POINT ( 'NONE',  ( 86.14890207173841929, 20.31981596387579714, -35.82156419891172305 ) ) ;
#67979 = LINE ( 'NONE', #19779, #15287 ) ;
#67980 = ORIENTED_EDGE ( 'NONE', *, *, #55443, .T. ) ;
#67981 = ORIENTED_EDGE ( 'NONE', *, *, #21796, .F. ) ;
#67982 = CARTESIAN_POINT ( 'NONE',  ( -85.35172689181705152, 26.07142112926220889, -72.89607453545865212 ) ) ;
#67983 = CARTESIAN_POINT ( 'NONE',  ( -0.6829546400373119885, 6.531019546548238353, -94.16435833651152620 ) ) ;
#67984 = DIRECTION ( 'NONE',  ( -0.8090169943749422332, -0.5877852522924802425, 0.000000000000000000 ) ) ;
#67985 = CARTESIAN_POINT ( 'NONE',  ( -125.8938041572051389, -170.0000000000000000, -15.56915330777026973 ) ) ;
#67986 = CARTESIAN_POINT ( 'NONE',  ( 63.01563776193091826, -170.0000000000000000, 29.81296093922127710 ) ) ;
#67987 = CARTESIAN_POINT ( 'NONE',  ( -190.6985136298602015, 109.1272424661243434, 69.71826505393651985 ) ) ;
#67988 = EDGE_CURVE ( 'NONE', #21636, #12229, #34486, .T. ) ;
#67989 = CARTESIAN_POINT ( 'NONE',  ( 198.3462436126384318, 99.64019527131947029, 94.40446352108099859 ) ) ;
#67990 = CARTESIAN_POINT ( 'NONE',  ( 209.6642862813004911, 115.2127693334913374, 31.07002473471074921 ) ) ;
#67991 = CARTESIAN_POINT ( 'NONE',  ( -76.77329340382468104, 21.60914066444073356, -62.18705756154123776 ) ) ;
#67992 = DIRECTION ( 'NONE',  ( 1.000000000000000000, 0.000000000000000000, 0.000000000000000000 ) ) ;
#67993 = ORIENTED_EDGE ( 'NONE', *, *, #32179, .F. ) ;
#67994 = CARTESIAN_POINT ( 'NONE',  ( 11.21312910819263031, 7.403355431336986037, -22.13777925856294360 ) ) ;
#67995 = EDGE_LOOP ( 'NONE', ( #25636, #1886 ) ) ;
#67996 = EDGE_CURVE ( 'NONE', #29979, #43634, #416, .T. ) ;
#67997 = CARTESIAN_POINT ( 'NONE',  ( 203.9276061909314421, 105.2889220654478919, -24.48138044215792419 ) ) ;
#67998 = ORIENTED_EDGE ( 'NONE', *, *, #27891, .F. ) ;
#67999 = EDGE_CURVE ( 'NONE', #46342, #20715, #65391, .T. ) ;
#68000 = B_SPLINE_CURVE_WITH_KNOTS ( 'NONE', 3,
 ( #34649, #3650, #13857, #51836, #2970, #25123, #57125, #8598, #61699, #40939, #61358, #3308, #51159, #67687, #56084, #46553, #62398, #36010, #7899, #13524, #2617, #19477, #40252, #8937, #68034, #29020, #50460, #23728, #45175, #24081, #66654, #18449, #50801, #37727, #10296, #37374, #42322, #47925, #10641, #89, #57811, #15928, #31765, #20863, #63435, #64117, #48261, #20175, #15248, #25810 ),
 .UNSPECIFIED., .F., .F.,
 ( 4, 2, 2, 2, 2, 2, 2, 2, 2, 2, 2, 2, 2, 2, 2, 2, 2, 2, 2, 2, 2, 2, 2, 2, 4 ),
 ( 0.02688458561150013082, 0.02770990876165290578, 0.02853523191180568422, 0.03018587821211125150, 0.03183652451241681530, 0.03266184766256959721, 0.03348717081272237911, 0.03513781711302788741, 0.03678846341333340264, 0.03761378656348616373, 0.03843910971363892481, 0.03926443286379169284, 0.04008975601394445393, 0.04174040231425002467, 0.04256572546440282045, 0.04339104861455563011, 0.04421637176470843283, 0.04504169491486123555, 0.04586701806501403134, 0.04669234121516684100, 0.04834298751547252276, 0.04916831066562538100, 0.04999363381577824617, 0.05164428011608401814, 0.05329492641638979705 ),
 .UNSPECIFIED. ) ;
#68001 = CARTESIAN_POINT ( 'NONE',  ( -48.00000000000000000, 19.99999999999996447, 4.000000000000000000 ) ) ;
#68002 = CYLINDRICAL_SURFACE ( 'NONE', #22101, 65.00000000000000000 ) ;
#68003 = DIRECTION ( 'NONE',  ( 0.000000000000000000, 0.000000000000000000, 1.000000000000000000 ) ) ;
#68004 = CARTESIAN_POINT ( 'NONE',  ( 36.08729376665094435, 8.001156100723207487, -36.37417898027339191 ) ) ;
#68005 = DIRECTION ( 'NONE',  ( 0.000000000000000000, -1.000000000000000000, 0.000000000000000000 ) ) ;
#68006 = CARTESIAN_POINT ( 'NONE',  ( 12.47451846520756291, 7.423604437114561527, -49.75163395661968480 ) ) ;
#68007 = DIRECTION ( 'NONE',  ( -0.000000000000000000, -0.000000000000000000, -1.000000000000000000 ) ) ;
#68008 = ORIENTED_EDGE ( 'NONE', *, *, #63838, .T. ) ;
#68009 = ORIENTED_EDGE ( 'NONE', *, *, #59389, .F. ) ;
#68010 = AXIS2_PLACEMENT_3D ( 'NONE', #14349, #35804, #57256 ) ;
#68011 = CARTESIAN_POINT ( 'NONE',  ( -53.60725281709859757, -37.40286400928327026, 41.38025477438755928 ) ) ;
#68012 = FACE_OUTER_BOUND ( 'NONE', #43531, .T. ) ;
#68013 = CARTESIAN_POINT ( 'NONE',  ( -5.000000000000000000, 5.000000000000000000, 0.000000000000000000 ) ) ;
#68014 = AXIS2_PLACEMENT_3D ( 'NONE', #34514, #14078, #23257 ) ;
#68015 = CARTESIAN_POINT ( 'NONE',  ( 8.480442907658517271, 6.376693431076493113, 12.37499517304073571 ) ) ;
#68016 = LINE ( 'NONE', #35999, #50281 ) ;
#68017 = AXIS2_PLACEMENT_3D ( 'NONE', #40484, #20076, #31328 ) ;
#68018 = CIRCLE ( 'NONE', #26429, 65.00000000000000000 ) ;
#68019 = CYLINDRICAL_SURFACE ( 'NONE', #51431, 65.36598343705435354 ) ;
#68020 = CARTESIAN_POINT ( 'NONE',  ( 177.0075766083212159, 74.58167636505950782, -76.86931686656495799 ) ) ;
#68021 = DIRECTION ( 'NONE',  ( -0.000000000000000000, -0.000000000000000000, -1.000000000000000000 ) ) ;
#68022 = CARTESIAN_POINT ( 'NONE',  ( 88.30010642107258434, 19.99780058782973313, -9.161515012596032292 ) ) ;
#68023 = CARTESIAN_POINT ( 'NONE',  ( -172.3018509397888351, 86.22053936367350957, 18.94384451952671000 ) ) ;
#68024 = DIRECTION ( 'NONE',  ( -0.000000000000000000, -0.000000000000000000, -1.000000000000000000 ) ) ;
#68025 = EDGE_CURVE ( 'NONE', #20757, #26499, #58538, .T. ) ;
#68026 = LINE ( 'NONE', #41284, #26523 ) ;
#68027 = AXIS2_PLACEMENT_3D ( 'NONE', #52556, #31795, #20537 ) ;
#68028 =( BOUNDED_CURVE ( )  B_SPLINE_CURVE ( 3, ( #49592, #732, #1078, #7413 ),
 .UNSPECIFIED., .F., .F. ) 
 B_SPLINE_CURVE_WITH_KNOTS ( ( 4, 4 ),
 ( 1.570796326794902109, 3.141592653589793116 ),
 .UNSPECIFIED. ) 
 CURVE ( )  GEOMETRIC_REPRESENTATION_ITEM ( )  RATIONAL_B_SPLINE_CURVE ( ( 1.000000000000000000, 0.8047378541243662697, 0.8047378541243662697, 1.000000000000000000 ) ) 
 REPRESENTATION_ITEM ( '' )  );
#68029 = B_SPLINE_CURVE_WITH_KNOTS ( 'NONE', 3,
 ( #33483, #22215, #39435, #28175, #11296, #34176, #27837, #32768, #16585, #49274, #49627, #1110, #17273, #16925, #38042, #6729, #11647, #44721, #5672, #1456, #22911, #7080, #33816, #6020, #38748, #60192, #12009, #49987, #44356, #43652, #1817, #65840, #33125, #17638, #60888, #12710, #27135, #54555, #39106, #48568, #48921, #402, #21860, #27480 ),
 .UNSPECIFIED., .F., .F.,
 ( 4, 2, 2, 2, 2, 2, 2, 2, 2, 2, 2, 2, 2, 2, 2, 2, 2, 2, 2, 2, 2, 4 ),
 ( 0.02416815208377490545, 0.02567033257376880734, 0.02642142281876576002, 0.02717251306376271269, 0.02867469355375657641, 0.02942578379875351868, 0.03017687404375045748, 0.03167905453374433855, 0.03318123502373822309, 0.03393232526873516536, 0.03468341551373210763, 0.03618559600372597829, 0.03693668624872289280, 0.03768777649371980731, 0.03918995698371364328, 0.04069213747370747924, 0.04219431796370130133, 0.04369649845369513730, 0.04444758869869204487, 0.04519867894368894551, 0.04670085943368275372, 0.04820303992367654805 ),
 .UNSPECIFIED. ) ;
#68030 = VECTOR ( 'NONE', #63026, 999.9999999999998863 ) ;
#68031 = CARTESIAN_POINT ( 'NONE',  ( -3.857727530059796628, 6.665032499723451132, 70.82944377365473088 ) ) ;
#68032 = EDGE_LOOP ( 'NONE', ( #46638, #18483 ) ) ;
#68033 = PLANE ( 'NONE',  #28278 ) ;
#68034 = CARTESIAN_POINT ( 'NONE',  ( 149.9714610887122035, 53.28792066194170474, 63.44660927195447186 ) ) ;
#68035 = CARTESIAN_POINT ( 'NONE',  ( -109.3585523124448002, 37.67345343047317385, -66.82677446236121455 ) ) ;
#68036 = CARTESIAN_POINT ( 'NONE',  ( -54.57280099357650727, 14.55288945003959178, -50.21632399845989880 ) ) ;
#68037 = CARTESIAN_POINT ( 'NONE',  ( -81.83265147652316784, 46.58665115056957973, 73.58025477438758344 ) ) ;
#68038 = CARTESIAN_POINT ( 'NONE',  ( -190.6985136298601731, 109.1272424661242582, 94.99999999999866418 ) ) ;
#68039 = ORIENTED_EDGE ( 'NONE', *, *, #54850, .F. ) ;
#68040 = SURFACE_SIDE_STYLE ('',( #8943 ) ) ;
#68041 = CARTESIAN_POINT ( 'NONE',  ( 6.400000000000000355, 0.000000000000000000, 5.000000000000000000 ) ) ;
#68042 = ORIENTED_EDGE ( 'NONE', *, *, #61857, .F. ) ;
#68043 = ORIENTED_EDGE ( 'NONE', *, *, #46538, .T. ) ;
#68044 = CARTESIAN_POINT ( 'NONE',  ( 177.7889574972182061, 75.33777460203560850, -50.47746129031760631 ) ) ;
#68045 = CARTESIAN_POINT ( 'NONE',  ( 15.55634918610409656, 31.11269837220803325, 2.000000000000001776 ) ) ;
#68046 = CARTESIAN_POINT ( 'NONE',  ( 138.4714068233401179, 45.47397885319522004, -91.28743950027845244 ) ) ;
#68047 = ORIENTED_EDGE ( 'NONE', *, *, #8491, .T. ) ;
#68048 = DIRECTION ( 'NONE',  ( 1.000000000000000000, 0.000000000000000000, 0.000000000000000000 ) ) ;
#68049 = CARTESIAN_POINT ( 'NONE',  ( -41.50537345350632279, -50.04124777106357413, 170.0000000000000000 ) ) ;
#68050 = DIRECTION ( 'NONE',  ( 0.6427876096865403621, 0.7660444431189770143, 1.393823445737823288E-16 ) ) ;
#68051 = DIRECTION ( 'NONE',  ( 0.000000000000000000, 0.000000000000000000, -1.000000000000000000 ) ) ;
#68052 = DIRECTION ( 'NONE',  ( 0.000000000000000000, 0.000000000000000000, 1.000000000000000000 ) ) ;
#68053 = CARTESIAN_POINT ( 'NONE',  ( -24.61094659556678010, 9.585225265507409276, -12.86029569530389161 ) ) ;
#68054 = PRODUCT_RELATED_PRODUCT_CATEGORY ( 'part', '', ( #5169 ) ) ;
#68055 = CARTESIAN_POINT ( 'NONE',  ( 111.9975424824652634, 172.0000000000002274, 529.9060149868648750 ) ) ;
#68056 = EDGE_CURVE ( 'NONE', #68729, #33041, #2378, .T. ) ;
#68057 = EDGE_LOOP ( 'NONE', ( #51010, #26389, #42715 ) ) ;
#68058 = DIRECTION ( 'NONE',  ( -0.000000000000000000, 1.000000000000000000, -0.000000000000000000 ) ) ;
#68059 = AXIS2_PLACEMENT_3D ( 'NONE', #24290, #52391, #29544 ) ;
#68060 = EDGE_CURVE ( 'NONE', #26272, #21469, #13936, .T. ) ;
#68061 = CARTESIAN_POINT ( 'NONE',  ( 14.80582440982707482, 6.470883766728822373, 71.81066783346395255 ) ) ;
#68062 = CARTESIAN_POINT ( 'NONE',  ( 198.2588776805010582, 99.52972231602375075, 32.85139680164935072 ) ) ;
#68063 = CARTESIAN_POINT ( 'NONE',  ( -79.31924985377354176, 23.64871657882263989, 84.11086250148999000 ) ) ;
#68064 = AXIS2_PLACEMENT_3D ( 'NONE', #2932, #19799, #34946 ) ;
#68066 = ORIENTED_EDGE ( 'NONE', *, *, #65705, .F. ) ;
#68065 = DIRECTION ( 'NONE',  ( 1.334402673828311663E-15, -1.000000000000000000, -1.974915957265903643E-15 ) ) ;
#68067 = CARTESIAN_POINT ( 'NONE',  ( 65.62985354949975658, 14.32996029952554018, 44.34682454305074373 ) ) ;
#68068 = VERTEX_POINT ( 'NONE', #6639 ) ;
#68069 = AXIS2_PLACEMENT_3D ( 'NONE', #57885, #30130, #19561 ) ;
#68070 = ORIENTED_EDGE ( 'NONE', *, *, #23993, .F. ) ;
#68071 = CARTESIAN_POINT ( 'NONE',  ( 112.5612011511789916, 31.08353758940341294, -77.41542351236350328 ) ) ;
#68072 = CARTESIAN_POINT ( 'NONE',  ( -2.000000000000000000, 0.000000000000000000, 380.0000000000000000 ) ) ;
#68073 = CARTESIAN_POINT ( 'NONE',  ( 198.4017331595408677, 98.09114638179337931, -74.75484424362443292 ) ) ;
#68075 = DIRECTION ( 'NONE',  ( -0.000000000000000000, -0.000000000000000000, 1.000000000000000000 ) ) ;
#68074 = VECTOR ( 'NONE', #66600, 1000.000000000000000 ) ;
#68076 = CARTESIAN_POINT ( 'NONE',  ( -118.8689810167775818, 42.03922634358562505, 62.32420629194420059 ) ) ;
#68077 = CARTESIAN_POINT ( 'NONE',  ( -81.00768240531211006, 24.30850321514434143, -22.90011388250445989 ) ) ;
#68078 = DIRECTION ( 'NONE',  ( -3.081487911019579554E-32, -1.000000000000000000, -3.469446951953612956E-17 ) ) ;
#68079 = AXIS2_PLACEMENT_3D ( 'NONE', #13061, #60538, #49267 ) ;
#68080 = CARTESIAN_POINT ( 'NONE',  ( -49.13048465129991627, 14.20828170588045403, 42.44559892615119168 ) ) ;
#68081 = ORIENTED_EDGE ( 'NONE', *, *, #63110, .T. ) ;
#68082 = EDGE_CURVE ( 'NONE', #36640, #18239, #55167, .T. ) ;
#68083 = ORIENTED_EDGE ( 'NONE', *, *, #59197, .F. ) ;
#68084 = EDGE_CURVE ( 'NONE', #56804, #28889, #34283, .T. ) ;
#68085 = FACE_OUTER_BOUND ( 'NONE', #26615, .T. ) ;
#68086 = CARTESIAN_POINT ( 'NONE',  ( 105.4375968828853729, 26.72149058755206852, 69.71918802570772300 ) ) ;
#68087 = CARTESIAN_POINT ( 'NONE',  ( 112.5010186421628049, 29.94054703519628546, 83.64122026741506488 ) ) ;
#68088 = CARTESIAN_POINT ( 'NONE',  ( 8.000000000000000000, 0.7809653281576076633, -9.500000000000001776 ) ) ;
#68089 = DIRECTION ( 'NONE',  ( 0.7071067811865473507, 0.000000000000000000, -0.7071067811865477948 ) ) ;
#68090 = DIRECTION ( 'NONE',  ( 1.000000000000000000, -0.000000000000000000, 0.000000000000000000 ) ) ;
#68091 = CARTESIAN_POINT ( 'NONE',  ( -142.1950298130309420, 59.49693210460241488, 93.72120968998457613 ) ) ;
#68092 = ORIENTED_EDGE ( 'NONE', *, *, #58910, .F. ) ;
#68093 = ORIENTED_EDGE ( 'NONE', *, *, #69395, .F. ) ;
#68094 = ORIENTED_EDGE ( 'NONE', *, *, #35351, .T. ) ;
#68095 = LINE ( 'NONE', #31483, #49859 ) ;
#68096 = CARTESIAN_POINT ( 'NONE',  ( 178.3559415630091678, 75.89137766528514817, -90.41844760944908899 ) ) ;
#68097 = DIRECTION ( 'NONE',  ( 0.000000000000000000, 0.000000000000000000, -1.000000000000000000 ) ) ;
#68098 = CARTESIAN_POINT ( 'NONE',  ( 108.3885044869535079, -21.48423713950020897, 4.736025848076682365 ) ) ;
#68099 = CARTESIAN_POINT ( 'NONE',  ( -62.49137879463568623, 17.85440472148629354, 38.80717417638208389 ) ) ;
#68100 = CARTESIAN_POINT ( 'NONE',  ( -37.07436112751821611, 11.60822760208520421, -64.68853167423618800 ) ) ;
#68101 = CARTESIAN_POINT ( 'NONE',  ( 32.90953848114695290, 7.653665824624201974, 60.49547482373738916 ) ) ;
#68102 = CARTESIAN_POINT ( 'NONE',  ( 46.23333927402088506, 9.396595540482447717, 87.98974472844928130 ) ) ;
#68103 = SHAPE_REPRESENTATION_RELATIONSHIP ( 'NONE' , 'NONE' ,  #57739, #55050 ) ;
#68104 = ORIENTED_EDGE ( 'NONE', *, *, #16038, .F. ) ;
#68105 = DIRECTION ( 'NONE',  ( -0.000000000000000000, 1.000000000000000000, -0.000000000000000000 ) ) ;
#68106 = CARTESIAN_POINT ( 'NONE',  ( 187.5272808203427530, 85.37192123373903030, 59.77628873332410819 ) ) ;
#68107 = CARTESIAN_POINT ( 'NONE',  ( 4.000000000000012434, 6.928203230275504332, 0.000000000000000000 ) ) ;
#68108 = CARTESIAN_POINT ( 'NONE',  ( 68.95451040317567504, 14.12887482153123564, -65.45849180363892117 ) ) ;
#68109 = CARTESIAN_POINT ( 'NONE',  ( 18.19980344696536889, 6.589834367837006823, 57.25328788149280257 ) ) ;
#68110 = CYLINDRICAL_SURFACE ( 'NONE', #68069, 25.00000000000000711 ) ;
#68111 = CARTESIAN_POINT ( 'NONE',  ( 15.78827728214693416, 7.507518794609588042, 3.170157082241545687 ) ) ;
#68112 = AXIS2_PLACEMENT_3D ( 'NONE', #23260, #2492, #49263 ) ;
#68113 = EDGE_LOOP ( 'NONE', ( #5070, #33308, #33913, #45532 ) ) ;
#68114 = VECTOR ( 'NONE', #67153, 1000.000000000000000 ) ;
#68115 = DIRECTION ( 'NONE',  ( -1.000000000000000000, -0.000000000000000000, -0.000000000000000000 ) ) ;
#68116 = APPLICATION_PROTOCOL_DEFINITION ( 'draft international standard', 'automotive_design', 1998, #64648 ) ;
#68117 = CARTESIAN_POINT ( 'NONE',  ( 126.6464677212869248, 38.39096133771043640, -45.65458962762210149 ) ) ;
#68118 = CARTESIAN_POINT ( 'NONE',  ( -128.1219934350341703, 47.97781708504715681, -35.23767964644014938 ) ) ;
#68119 = CARTESIAN_POINT ( 'NONE',  ( -108.1180879163842690, 36.99199941971028238, -37.77984450447672771 ) ) ;
#68120 = CARTESIAN_POINT ( 'NONE',  ( 188.5842358232185632, 88.03712271786932320, -44.02448079173893802 ) ) ;
#68121 = ORIENTED_EDGE ( 'NONE', *, *, #126, .T. ) ;
#68122 = VECTOR ( 'NONE', #34652, 1000.000000000000114 ) ;
#68123 = CIRCLE ( 'NONE', #23167, 5.000000000000004441 ) ;
#68124 = PRODUCT_DEFINITION_FORMATION_WITH_SPECIFIED_SOURCE ( 'ANY', '', #4024, .NOT_KNOWN. ) ;
#68125 = VERTEX_POINT ( 'NONE', #9770 ) ;
#68126 = DIRECTION ( 'NONE',  ( -0.5407162030609373726, -0.6444004775717707689, -0.5407162030609373726 ) ) ;
#68127 = VECTOR ( 'NONE', #11373, 1000.000000000000000 ) ;
#68128 = CARTESIAN_POINT ( 'NONE',  ( 2.905661822261151883E-14, 20.55634918610402906, 85.00100000000000477 ) ) ;
#68129 = ORIENTED_EDGE ( 'NONE', *, *, #34434, .F. ) ;
#68130 = CARTESIAN_POINT ( 'NONE',  ( 158.7714055544899168, 59.95166641265087293, 83.18787582866841035 ) ) ;
#68131 = ORIENTED_EDGE ( 'NONE', *, *, #44151, .F. ) ;
#68132 = CARTESIAN_POINT ( 'NONE',  ( -62.50103539982530521, 17.85731685071834463, 9.961880401615221814 ) ) ;
#68133 = CARTESIAN_POINT ( 'NONE',  ( 126.3541873520043737, 37.07520218256170352, 36.51082573705635070 ) ) ;
#68134 = CARTESIAN_POINT ( 'NONE',  ( -154.6085044440278295, 69.98390342970671441, 32.71756333063028421 ) ) ;
#68136 = EDGE_CURVE ( 'NONE', #56285, #22108, #6030, .T. ) ;
#68135 = CARTESIAN_POINT ( 'NONE',  ( 0.000000000000000000, 0.000000000000000000, 170.0000000000000000 ) ) ;
#68137 = CARTESIAN_POINT ( 'NONE',  ( -18.89790202299119315, -62.20684691518632548, 170.0000000000000000 ) ) ;
#68139 = ORIENTED_EDGE ( 'NONE', *, *, #3344, .T. ) ;
#68138 = LINE ( 'NONE', #36116, #40947 ) ;
#68140 = CYLINDRICAL_SURFACE ( 'NONE', #25008, 65.00000000000000000 ) ;
#68141 = EDGE_CURVE ( 'NONE', #29280, #16199, #14004, .T. ) ;
#68142 = VERTEX_POINT ( 'NONE', #30530 ) ;
#68143 = ORIENTED_EDGE ( 'NONE', *, *, #8530, .F. ) ;
#68144 = LINE ( 'NONE', #26257, #47946 ) ;
#68145 = EDGE_CURVE ( 'NONE', #3775, #44530, #68572, .T. ) ;
#68146 = CARTESIAN_POINT ( 'NONE',  ( -176.3791001330699260, 90.82833141237287577, -8.597446401251650272 ) ) ;
#68148 = ORIENTED_EDGE ( 'NONE', *, *, #1694, .F. ) ;
#68147 = CARTESIAN_POINT ( 'NONE',  ( -125.8938041572051389, 47.69968343338778993, 57.46449846362076386 ) ) ;
#68149 = CARTESIAN_POINT ( 'NONE',  ( -109.4963484765719244, 37.74981983082538761, 93.77794043553710424 ) ) ;
#68150 = EDGE_CURVE ( 'NONE', #38092, #30571, #65206, .T. ) ;
#68151 = FACE_BOUND ( 'NONE', #8368, .T. ) ;
#68152 = VERTEX_POINT ( 'NONE', #59659 ) ;
#68153 = CARTESIAN_POINT ( 'NONE',  ( -58.76005811686689384, 15.70653557534865108, -9.334115721335656701 ) ) ;
#68154 = AXIS2_PLACEMENT_3D ( 'NONE', #50937, #41075, #62535 ) ;
#68155 = CARTESIAN_POINT ( 'NONE',  ( 134.0849965622593061, 42.73957449886184179, 29.51034083899532945 ) ) ;
#68156 = CARTESIAN_POINT ( 'NONE',  ( 114.6659427952414347, 32.10199811723106933, 43.18690178204667518 ) ) ;
#68157 = LINE ( 'NONE', #24896, #42608 ) ;
#68158 = CARTESIAN_POINT ( 'NONE',  ( 70.50376765786474209, 15.57629333413343353, -70.55552223763868369 ) ) ;
#68159 = ADVANCED_FACE ( 'NONE', ( #58974 ), #27660, .F. ) ;
#68160 = VERTEX_POINT ( 'NONE', #65309 ) ;
#68161 = ORIENTED_EDGE ( 'NONE', *, *, #55160, .F. ) ;
#68162 = CARTESIAN_POINT ( 'NONE',  ( 44.99999999999997158, 22.99999999999998579, 4.000000000000000000 ) ) ;
#68163 = DIRECTION ( 'NONE',  ( 1.000000000000000000, 0.000000000000000000, 0.000000000000000000 ) ) ;
#68164 = CARTESIAN_POINT ( 'NONE',  ( 15.55634918610409656, 31.11269837220803325, 2.000000000000001776 ) ) ;
#68165 = AXIS2_PLACEMENT_3D ( 'NONE', #51073, #46826, #9195 ) ;
#68166 = CARTESIAN_POINT ( 'NONE',  ( -49.52089322850377329, 13.26777265051996224, -91.33638462665525992 ) ) ;
#68167 = LINE ( 'NONE', #1812, #46651 ) ;
#68168 = CARTESIAN_POINT ( 'NONE',  ( -37.03736007212398818, 19.22364788858845230, 13.79046340968178619 ) ) ;
#68169 = PRODUCT_DEFINITION_FORMATION_WITH_SPECIFIED_SOURCE ( 'ANY', '', #34472, .NOT_KNOWN. ) ;
#68170 = CARTESIAN_POINT ( 'NONE',  ( -145.3109762780891288, 60.69959559383372039, 44.45407750809701497 ) ) ;
#68171 = DIRECTION ( 'NONE',  ( 1.000000000000000000, 1.748373411921809651E-16, 2.371692252312040348E-20 ) ) ;
#68172 = CARTESIAN_POINT ( 'NONE',  ( 211.5066273949819902, 116.1727691518061647, 60.35867932873075148 ) ) ;
#68173 = VERTEX_POINT ( 'NONE', #52999 ) ;
#68174 = CARTESIAN_POINT ( 'NONE',  ( -109.0291978193666580, 37.49173305805087608, 34.73816087405813846 ) ) ;
#68175 = ORIENTED_EDGE ( 'NONE', *, *, #51474, .T. ) ;
#68177 = AXIS2_PLACEMENT_3D ( 'NONE', #28454, #35168, #29899 ) ;
#68176 = CARTESIAN_POINT ( 'NONE',  ( -31.43908319763709258, 9.591432048623765638, 18.37190381572551701 ) ) ;
#68178 = CARTESIAN_POINT ( 'NONE',  ( 80.15818551272217007, 18.36718314243334049, 67.88017848172013657 ) ) ;
#68179 = EDGE_LOOP ( 'NONE', ( #14160, #21390, #13252, #45221 ) ) ;
#68180 = DIRECTION ( 'NONE',  ( 1.000000000000000000, 0.000000000000000000, 0.000000000000000000 ) ) ;
#68181 = CARTESIAN_POINT ( 'NONE',  ( 31.08057067389502137, 19.16407787157944398, 38.91942932610497508 ) ) ;
#68182 = CARTESIAN_POINT ( 'NONE',  ( 36.09469435220862721, 9.015003538710486097, 3.820264011147788796 ) ) ;
#68183 =( LENGTH_UNIT ( ) NAMED_UNIT ( * ) SI_UNIT ( .MILLI., .METRE. ) );
#68184 = CARTESIAN_POINT ( 'NONE',  ( 32.67604596315970866, 7.629767358313821468, 7.241655292760623475 ) ) ;
#68185 = CARTESIAN_POINT ( 'NONE',  ( 0.000000000000000000, -2.000000000000000000, -0.000000000000000000 ) ) ;
#68186 = CARTESIAN_POINT ( 'NONE',  ( -38.69449158134467126, 11.92067517118076836, -17.93520783166486154 ) ) ;
#68187 = ORIENTED_EDGE ( 'NONE', *, *, #29858, .F. ) ;
#68188 = CARTESIAN_POINT ( 'NONE',  ( -118.6704545714847114, 43.09717372409259184, -94.02806988937946642 ) ) ;
#68189 = EDGE_LOOP ( 'NONE', ( #48951, #64114, #53029, #45051 ) ) ;
#68190 = CARTESIAN_POINT ( 'NONE',  ( 75.31295361348102801, 0.000000000000000000, 2.500000000000030198 ) ) ;
#68191 = CARTESIAN_POINT ( 'NONE',  ( 8.537735592981560373, 7.383000420390737339, -67.92956672507523308 ) ) ;
#68192 = CARTESIAN_POINT ( 'NONE',  ( -189.2352924136013144, 107.0839554967700735, 11.13131724358098573 ) ) ;
#68193 = CARTESIAN_POINT ( 'NONE',  ( -78.66644367742111399, -170.0000000000000000, 30.41820113967310490 ) ) ;
#68194 = CARTESIAN_POINT ( 'NONE',  ( -14.32120159453990205, 7.401444311907545703, -73.51966526291316484 ) ) ;
#68195 = CARTESIAN_POINT ( 'NONE',  ( -95.19652294162978023, 29.32558722310179888, -13.15270443607074036 ) ) ;
#68196 = ORIENTED_EDGE ( 'NONE', *, *, #49399, .T. ) ;
#68197 = DIRECTION ( 'NONE',  ( 9.938230793871127844E-15, -1.000000000000000000, -3.996802888650563546E-15 ) ) ;
#68198 = CARTESIAN_POINT ( 'NONE',  ( -151.6648563624119106, 67.36546864992756412, 57.86878014402077497 ) ) ;
#68199 = CARTESIAN_POINT ( 'NONE',  ( -119.2682179969168317, 42.28333404791698769, 41.67301999128292067 ) ) ;
#68200 = DIRECTION ( 'NONE',  ( 1.000000000000000000, 0.000000000000000000, 0.000000000000000000 ) ) ;
#68201 = ORIENTED_EDGE ( 'NONE', *, *, #5622, .F. ) ;
#68202 = DIRECTION ( 'NONE',  ( -1.000000000000000000, 0.000000000000000000, 0.000000000000000000 ) ) ;
#68203 = ADVANCED_FACE ( 'NONE', ( #38219 ), #55454, .T. ) ;
#68204 = CARTESIAN_POINT ( 'NONE',  ( 135.1592029508519488, 43.39714837287904459, 83.30687946948802391 ) ) ;
#68205 = CARTESIAN_POINT ( 'NONE',  ( 203.0737501689026772, 105.8313166752871410, -90.18532627228834997 ) ) ;
#68206 = DIRECTION ( 'NONE',  ( -0.000000000000000000, 1.000000000000000000, -0.000000000000000000 ) ) ;
#68207 = AXIS2_PLACEMENT_3D ( 'NONE', #40736, #51313, #14012 ) ;
#68208 = DIRECTION ( 'NONE',  ( -0.000000000000000000, -0.000000000000000000, 1.000000000000000000 ) ) ;
#68209 = ORIENTED_EDGE ( 'NONE', *, *, #60611, .T. ) ;
#68210 = CARTESIAN_POINT ( 'NONE',  ( 197.5334904971816457, 97.00846725096930356, 38.94895049893467842 ) ) ;
#68211 = CARTESIAN_POINT ( 'NONE',  ( 114.6632852039171411, 30.98120524556724575, -76.33079645022053228 ) ) ;
#68212 = VECTOR ( 'NONE', #16084, 1000.000000000000000 ) ;
#68213 = CARTESIAN_POINT ( 'NONE',  ( 182.7686108735401262, 81.77235358504609053, 29.48784566593629108 ) ) ;
#68214 = CARTESIAN_POINT ( 'NONE',  ( 186.6368918226156381, 84.40539020454804131, -92.35556283223742469 ) ) ;
#68215 = CARTESIAN_POINT ( 'NONE',  ( 181.0840389613909736, 80.03940679743416808, -24.38050707541595230 ) ) ;
#68216 = VECTOR ( 'NONE', #66849, 1000.000000000000114 ) ;
#68217 = ORIENTED_EDGE ( 'NONE', *, *, #35755, .F. ) ;
#68218 = CARTESIAN_POINT ( 'NONE',  ( 173.5844030397475706, 72.71952271766126330, 63.34818945125900314 ) ) ;
#68219 = EDGE_CURVE ( 'NONE', #52360, #47781, #51831, .T. ) ;
#68220 = ORIENTED_EDGE ( 'NONE', *, *, #15710, .F. ) ;
#68221 = AXIS2_PLACEMENT_3D ( 'NONE', #45472, #39174, #60959 ) ;
#68222 = CARTESIAN_POINT ( 'NONE',  ( 70.50376765786472788, 15.57629333413343353, 63.66723071467976780 ) ) ;
#68223 = CARTESIAN_POINT ( 'NONE',  ( 140.3784951150909706, 45.50429060678176540, 94.41964330782973036 ) ) ;
#68225 = EDGE_LOOP ( 'NONE', ( #63008, #4472, #42510, #32355 ) ) ;
#68224 = CARTESIAN_POINT ( 'NONE',  ( 156.3797504404255960, 58.07856685387021400, 2.641341998005292790 ) ) ;
#68226 = CARTESIAN_POINT ( 'NONE',  ( -178.7483298110140026, 93.61800926271540391, 33.35710972951046926 ) ) ;
#68227 = ADVANCED_FACE ( 'NONE', ( #23454 ), #1998, .F. ) ;
#68228 = DIRECTION ( 'NONE',  ( 0.000000000000000000, -0.7660444431189770143, 0.6427876096865403621 ) ) ;
#68229 = CARTESIAN_POINT ( 'NONE',  ( 113.4418023215250457, 31.50656691678295473, -50.22257324304041504 ) ) ;
#68230 = ORIENTED_EDGE ( 'NONE', *, *, #47316, .T. ) ;
#68231 = DIRECTION ( 'NONE',  ( -0.000000000000000000, -1.000000000000000000, -0.000000000000000000 ) ) ;
#68232 = CARTESIAN_POINT ( 'NONE',  ( -132.9109786433856470, 51.29129389542020334, 40.78060923209528710 ) ) ;
#68233 = DIRECTION ( 'NONE',  ( 0.000000000000000000, -1.000000000000000000, -0.000000000000000000 ) ) ;
#68234 = ORIENTED_EDGE ( 'NONE', *, *, #28849, .T. ) ;
#68235 = CARTESIAN_POINT ( 'NONE',  ( 79.92842440418705507, 18.29578799637230802, -19.88223195959437817 ) ) ;
#68236 = CARTESIAN_POINT ( 'NONE',  ( -179.2112745835413250, 95.75131705262997173, -91.51719380277768323 ) ) ;
#68237 = CARTESIAN_POINT ( 'NONE',  ( 156.5977259323288422, 56.97512126940428345, 56.29186946110193190 ) ) ;
#68238 = LINE ( 'NONE', #58019, #27124 ) ;
#68239 = B_SPLINE_CURVE_WITH_KNOTS ( 'NONE', 3,
 ( #16045, #10765, #19336, #40792, #35528, #32232, #15704, #46410, #26945, #67889, #56983, #19684, #21666, #62610, #35870, #57325, #52046, #46764, #68232, #42436, #63893, #37154, #10416, #31885, #53315, #54711, #6539, #48722, #1257, #60696, #59983, #49074, #65636, #38191, #17426, #33283, #64937, #28697, #38904, #32915, #6879, #60347, #12512, #66352, #65277, #39252 ),
 .UNSPECIFIED., .F., .F.,
 ( 4, 2, 2, 2, 2, 2, 2, 2, 2, 2, 2, 2, 2, 2, 2, 2, 2, 2, 2, 2, 2, 2, 4 ),
 ( 0.000000000000000000, 0.001615199098318934479, 0.003230398196637868959, 0.004037997745797377615, 0.004845597294956887138, 0.006460796393275913124, 0.007268395942435457342, 0.008075995491595001560, 0.009691194589914039689, 0.01049879413907356569, 0.01130639368823308996, 0.01211399323739261770, 0.01292159278655214197, 0.01453679188487121306, 0.01615199098319028415, 0.01695959053234980321, 0.01776719008150931881, 0.01938238917982828408, 0.02099758827814724935, 0.02180518782730669555, 0.02261278737646613829, 0.02422798647478502376, 0.02584318557310390577 ),
 .UNSPECIFIED. ) ;
#68240 = EDGE_CURVE ( 'NONE', #1408, #13211, #44892, .T. ) ;
#68241 = ORIENTED_EDGE ( 'NONE', *, *, #9966, .T. ) ;
#68242 = CARTESIAN_POINT ( 'NONE',  ( -442.6627218934913230, 399.9999999999997726, 108.5502958579881891 ) ) ;
#68243 = EDGE_LOOP ( 'NONE', ( #28760, #53155, #57869, #54864 ) ) ;
#68244 = ADVANCED_FACE ( 'NONE', ( #6564 ), #28547, .T. ) ;
#68245 = EDGE_CURVE ( 'NONE', #8863, #27270, #22742, .T. ) ;
#68246 = CARTESIAN_POINT ( 'NONE',  ( 152.2924710224605462, 54.98503313872889464, -11.34835473471603251 ) ) ;
#68247 = CARTESIAN_POINT ( 'NONE',  ( -50.89568506533820624, 13.60612807157325932, 85.25567205612109944 ) ) ;
#68248 = CARTESIAN_POINT ( 'NONE',  ( 109.7732660198864352, 29.77277639096405792, 44.61121420573733332 ) ) ;
#68249 = CARTESIAN_POINT ( 'NONE',  ( -3.253130881186330203, 7.643323950922362719, 31.65042780773105591 ) ) ;
#68250 = AXIS2_PLACEMENT_3D ( 'NONE', #48180, #49225, #15844 ) ;
#68251 = CARTESIAN_POINT ( 'NONE',  ( 110.2429982417149574, -170.0000000000000000, 29.61121420573730489 ) ) ;
#68252 = CARTESIAN_POINT ( 'NONE',  ( 184.0001683447904099, 83.06228184427189376, 3.040735668703873795 ) ) ;
#68253 = CARTESIAN_POINT ( 'NONE',  ( 212.1962110267000128, 117.2292732107320745, -44.20259310511458040 ) ) ;
#68254 = CARTESIAN_POINT ( 'NONE',  ( 175.3815143714021190, 73.02838262206998365, 14.84218311195780515 ) ) ;
#68255 = ORIENTED_EDGE ( 'NONE', *, *, #20792, .T. ) ;
#68256 = VECTOR ( 'NONE', #29248, 1000.000000000000000 ) ;
#68257 = DIRECTION ( 'NONE',  ( 0.000000000000000000, 0.000000000000000000, -1.000000000000000000 ) ) ;
#68258 = ORIENTED_EDGE ( 'NONE', *, *, #13961, .T. ) ;
#68259 = CARTESIAN_POINT ( 'NONE',  ( -76.10382222627279702, 22.43453174720079701, 71.81548357156262341 ) ) ;
#68260 = APPLICATION_CONTEXT ( 'automotive_design' ) ;
#68261 = CARTESIAN_POINT ( 'NONE',  ( 56.30171512201000183, 11.21502580416395745, -66.71341671416431041 ) ) ;
#68262 = CARTESIAN_POINT ( 'NONE',  ( 230.9999999999999432, -2.000000000000000000, 380.0000000000000000 ) ) ;
#68263 = CARTESIAN_POINT ( 'NONE',  ( -14.61478091870810836, 7.428644888894361920, 88.10153567374477745 ) ) ;
#68264 = MECHANICAL_DESIGN_GEOMETRIC_PRESENTATION_REPRESENTATION (  '', ( #44660 ), #15482 ) ;
#68265 = CARTESIAN_POINT ( 'NONE',  ( -107.0809603157386789, 36.42942792191065848, -9.887358038569741936 ) ) ;
#68266 = ORIENTED_EDGE ( 'NONE', *, *, #31755, .F. ) ;
#68267 = CARTESIAN_POINT ( 'NONE',  ( -71.17819443284075476, 19.60909329639480703, 65.25372451627271175 ) ) ;
#68268 = CARTESIAN_POINT ( 'NONE',  ( 198.0154285049043779, 97.60753634768724396, -94.07841319457926943 ) ) ;
#68269 = ORIENTED_EDGE ( 'NONE', *, *, #22230, .F. ) ;
#68270 = ORIENTED_EDGE ( 'NONE', *, *, #44479, .T. ) ;
#68271 = CARTESIAN_POINT ( 'NONE',  ( -155.1355020251929488, 69.10372769512069624, 33.23808801693751036 ) ) ;
#68272 = DIRECTION ( 'NONE',  ( -0.000000000000000000, 0.000000000000000000, -1.000000000000000000 ) ) ;
#68273 = CARTESIAN_POINT ( 'NONE',  ( 174.6127059037622757, 72.30368563770913681, -20.71086728071027139 ) ) ;
#68274 = DIRECTION ( 'NONE',  ( 9.109522253334613014E-16, 1.000000000000000000, -3.889846672687432470E-31 ) ) ;
#68275 = AXIS2_PLACEMENT_3D ( 'NONE', #48058, #69512, #36487 ) ;
#68276 = DIRECTION ( 'NONE',  ( -1.000000000000000000, 0.000000000000000000, 0.000000000000000000 ) ) ;
#68277 = ORIENTED_EDGE ( 'NONE', *, *, #38257, .F. ) ;
#68278 = DIRECTION ( 'NONE',  ( 0.4887922226926451064, 0.000000000000000000, -0.8724002309921653486 ) ) ;
#68279 = EDGE_LOOP ( 'NONE', ( #53062, #1945 ) ) ;
#68280 = CARTESIAN_POINT ( 'NONE',  ( 211.7419975634644516, 116.5322580952101816, 7.208722705538775699 ) ) ;
#68281 = PLANE ( 'NONE',  #4627 ) ;
#68282 = CARTESIAN_POINT ( 'NONE',  ( 208.5889601154908632, 111.8333159387241835, 30.28245035469031876 ) ) ;
#68283 = EDGE_CURVE ( 'NONE', #11879, #54755, #45584, .T. ) ;
#68284 = CARTESIAN_POINT ( 'NONE',  ( -20.55634918610408945, -26.11269837220804035, 85.00100000000000477 ) ) ;
#68285 = EDGE_CURVE ( 'NONE', #14749, #61986, #38566, .T. ) ;
#68286 = VERTEX_POINT ( 'NONE', #49453 ) ;
#68287 = VERTEX_POINT ( 'NONE', #55085 ) ;
#68288 = CARTESIAN_POINT ( 'NONE',  ( 114.7439874972685345, -21.94289037477085813, 1.612903297879166642 ) ) ;
#68289 = CARTESIAN_POINT ( 'NONE',  ( -133.3762944804928736, 52.85946325787776345, 92.42369384535366805 ) ) ;
#68290 = CARTESIAN_POINT ( 'NONE',  ( -167.9853834315979384, 81.58767916550895904, -9.881304815344739367 ) ) ;
#68291 = DIRECTION ( 'NONE',  ( 0.000000000000000000, 0.000000000000000000, 1.000000000000000000 ) ) ;
#68292 = CARTESIAN_POINT ( 'NONE',  ( 21.94853621138365440, 6.775987044338161347, 86.91307455820552264 ) ) ;
#68293 = LINE ( 'NONE', #13441, #17591 ) ;
#68294 = VECTOR ( 'NONE', #65257, 1000.000000000000114 ) ;
#68295 = ORIENTED_EDGE ( 'NONE', *, *, #55168, .T. ) ;
#68297 = ADVANCED_FACE ( 'NONE', ( #44176 ), #12897, .T. ) ;
#68296 = DIRECTION ( 'NONE',  ( -2.922263668027335568E-20, -1.000000000000000000, -1.110223024625156294E-16 ) ) ;
#68298 = CARTESIAN_POINT ( 'NONE',  ( -101.8145602049406051, 32.54453702486150490, 72.36362509687884881 ) ) ;
#68299 = VERTEX_POINT ( 'NONE', #28721 ) ;
#68300 = EDGE_CURVE ( 'NONE', #23191, #39369, #27365, .T. ) ;
#68302 = CARTESIAN_POINT ( 'NONE',  ( -86.06016868996614733, 25.27707703029501829, 12.35716539879548392 ) ) ;
#68301 = AXIS2_PLACEMENT_3D ( 'NONE', #26896, #11754, #64886 ) ;
#68303 = ORIENTED_EDGE ( 'NONE', *, *, #20198, .F. ) ;
#68304 = CARTESIAN_POINT ( 'NONE',  ( -59.96408504033276898, 17.10126854471815605, -10.18249688487181004 ) ) ;
#68305 = VERTEX_POINT ( 'NONE', #33657 ) ;
#68306 = EDGE_CURVE ( 'NONE', #23284, #29832, #13241, .T. ) ;
#68307 = ORIENTED_EDGE ( 'NONE', *, *, #25971, .F. ) ;
#68308 = CARTESIAN_POINT ( 'NONE',  ( 8.951900209438534262, 6.378066731449592908, -46.11318404853862063 ) ) ;
#68309 = EDGE_CURVE ( 'NONE', #22785, #8973, #28361, .T. ) ;
#68310 = FACE_OUTER_BOUND ( 'NONE', #35110, .T. ) ;
#68311 = CARTESIAN_POINT ( 'NONE',  ( 132.0440382699655402, 40.34028297386452522, 56.56290485416193548 ) ) ;
#68312 = VERTEX_POINT ( 'NONE', #33998 ) ;
#68313 = CARTESIAN_POINT ( 'NONE',  ( -24.32567406192871573, 8.531457175616735000, 93.80475582042849680 ) ) ;
#68314 = AXIS2_PLACEMENT_3D ( 'NONE', #13406, #66541, #56307 ) ;
#68315 = CARTESIAN_POINT ( 'NONE',  ( 173.5836858989432301, 72.71885240881779566, -70.28283204199895806 ) ) ;
#68316 = DIRECTION ( 'NONE',  ( -0.000000000000000000, -0.000000000000000000, -1.000000000000000000 ) ) ;
#68317 = CARTESIAN_POINT ( 'NONE',  ( 108.3819860115547442, 28.02992728837241287, -50.70304034602167320 ) ) ;
#68318 = ADVANCED_FACE ( 'NONE', ( #49807 ), #1633, .F. ) ;
#68319 = LINE ( 'NONE', #51450, #16336 ) ;
#68320 = DIRECTION ( 'NONE',  ( 0.000000000000000000, 0.000000000000000000, -1.000000000000000000 ) ) ;
#68321 = VERTEX_POINT ( 'NONE', #23791 ) ;
#68322 = ADVANCED_FACE ( 'NONE', ( #50170 ), #18167, .F. ) ;
#68323 = ADVANCED_FACE ( 'NONE', ( #45234 ), #66712, .F. ) ;
#68324 = PLANE ( 'NONE',  #42138 ) ;
#68325 = CARTESIAN_POINT ( 'NONE',  ( -79.14094329813316619, 23.58034730000059653, -76.96000122218161721 ) ) ;
#68326 = DIRECTION ( 'NONE',  ( -1.000000000000000000, 9.109522253334599209E-16, 4.270088556250601699E-16 ) ) ;
#68327 = FACE_OUTER_BOUND ( 'NONE', #2010, .T. ) ;
#68328 = CARTESIAN_POINT ( 'NONE',  ( -55.05276343752909440, 14.68156374112637863, 45.31732777293115788 ) ) ;
#68329 = CARTESIAN_POINT ( 'NONE',  ( 139.3639069815893379, 44.85046254673765986, -92.10545781260216813 ) ) ;
#68330 = CARTESIAN_POINT ( 'NONE',  ( -151.2497169612549044, 65.66843968092749151, 18.72541422205654982 ) ) ;
#68331 = CARTESIAN_POINT ( 'NONE',  ( -118.9668643994983768, 43.27909474462865091, -66.37097778377670920 ) ) ;
#68332 = CARTESIAN_POINT ( 'NONE',  ( 9.962235950564870990, 64.23203137738423152, 133.5802547743875550 ) ) ;
#68333 = CARTESIAN_POINT ( 'NONE',  ( -149.5074843970971301, -170.0000000000000000, -15.46827994102828541 ) ) ;
#68334 = CARTESIAN_POINT ( 'NONE',  ( -104.5730787903383003, 33.96058035148152499, 45.17567448190496293 ) ) ;
#68335 = ORIENTED_EDGE ( 'NONE', *, *, #33142, .F. ) ;
#68336 = CARTESIAN_POINT ( 'NONE',  ( -62.03553610864626222, 17.71631625146951805, 88.69311610642812127 ) ) ;
#68337 = EDGE_LOOP ( 'NONE', ( #28533, #14742, #21814, #55196 ) ) ;
#68338 = CARTESIAN_POINT ( 'NONE',  ( 199.7278513351971299, 99.76879341361770059, -11.34529423773141232 ) ) ;
#68339 = ORIENTED_EDGE ( 'NONE', *, *, #35506, .F. ) ;
#68340 = CARTESIAN_POINT ( 'NONE',  ( 15.78827728214693416, 7.507518794609589818, -77.36349468914950478 ) ) ;
#68341 = DIRECTION ( 'NONE',  ( -1.000000000000000000, 0.000000000000000000, 0.000000000000000000 ) ) ;
#68342 = DIRECTION ( 'NONE',  ( -3.081487911019579554E-32, -1.000000000000000000, -3.469446951953612956E-17 ) ) ;
#68343 = FACE_OUTER_BOUND ( 'NONE', #51947, .T. ) ;
#68344 = CARTESIAN_POINT ( 'NONE',  ( 141.3556389957210513, 47.34429831367556574, -43.22740683371433335 ) ) ;
#68345 = CARTESIAN_POINT ( 'NONE',  ( 205.3776734260163153, 109.0011436241188818, -90.01503221354894890 ) ) ;
#68346 = CARTESIAN_POINT ( 'NONE',  ( 8.287863202055541834, 7.382585476140734571, -42.53069974475695147 ) ) ;
#68347 = LINE ( 'NONE', #32085, #67873 ) ;
#68348 = CARTESIAN_POINT ( 'NONE',  ( 126.9201538765324386, 37.39093565120714402, -40.65955411680997855 ) ) ;
#68349 = EDGE_LOOP ( 'NONE', ( #50446, #57370, #27782, #46919 ) ) ;
#68350 = ORIENTED_EDGE ( 'NONE', *, *, #58743, .F. ) ;
#68351 = AXIS2_PLACEMENT_3D ( 'NONE', #59004, #31944, #52689 ) ;
#68352 = CARTESIAN_POINT ( 'NONE',  ( 23.05216796272351232, -9.986758404123879274, 0.000000000000000000 ) ) ;
#68353 = DIRECTION ( 'NONE',  ( 0.000000000000000000, -0.000000000000000000, -1.000000000000000000 ) ) ;
#68354 = DIRECTION ( 'NONE',  ( -1.000000000000000000, 0.000000000000000000, 0.000000000000000000 ) ) ;
#68355 = AXIS2_PLACEMENT_3D ( 'NONE', #32635, #4181, #63269 ) ;
#68356 = UNCERTAINTY_MEASURE_WITH_UNIT (LENGTH_MEASURE( 1.000000000000000082E-05 ), #36345, 'distance_accuracy_value', 'NONE');
#68357 = CARTESIAN_POINT ( 'NONE',  ( 10.83046137699561839, 6.392429922561260192, 16.31901005528300175 ) ) ;
#68358 = CIRCLE ( 'NONE', #14430, 60.00000000000000000 ) ;
#68359 = CARTESIAN_POINT ( 'NONE',  ( 280.3268469170084245, 21.42428528562853529, -4.999999999999990230 ) ) ;
#68360 = CARTESIAN_POINT ( 'NONE',  ( -74.58602291351357394, -7.967916035252095242, 170.0000000000000000 ) ) ;
#68361 = CARTESIAN_POINT ( 'NONE',  ( 173.7246046907419554, 71.47482343504560731, -69.09541590300931091 ) ) ;
#68362 =( NAMED_UNIT ( * ) PLANE_ANGLE_UNIT ( ) SI_UNIT ( $, .RADIAN. ) );
#68363 = DIRECTION ( 'NONE',  ( -0.000000000000000000, -0.000000000000000000, 1.000000000000000000 ) ) ;
#68364 = CARTESIAN_POINT ( 'NONE',  ( 93.32502112557678231, 21.81526022999039682, -19.89247016698760362 ) ) ;
#68365 = CARTESIAN_POINT ( 'NONE',  ( -25.80443741485379761, 9.749985135376006085, 69.53500943053950323 ) ) ;
#68366 = CARTESIAN_POINT ( 'NONE',  ( 109.3426986656772470, 21.43197803755063902, 4.967354168418953719 ) ) ;
#68367 = DIRECTION ( 'NONE',  ( 2.616877698022258092E-18, -4.379915515250366329E-18, -1.000000000000000000 ) ) ;
#68368 = EDGE_CURVE ( 'NONE', #24023, #40116, #61420, .T. ) ;
#68369 = ORIENTED_EDGE ( 'NONE', *, *, #24640, .F. ) ;
#68370 = CARTESIAN_POINT ( 'NONE',  ( 126.4633682455862385, 38.28837286275647500, 11.45369110127332313 ) ) ;
#68371 = CARTESIAN_POINT ( 'NONE',  ( 133.8566784816069344, 41.42467568809809109, -24.17876034193199786 ) ) ;
#68372 = CARTESIAN_POINT ( 'NONE',  ( -15.55634918610408945, -26.11269837220804035, 85.00100000000000477 ) ) ;
#68373 = CARTESIAN_POINT ( 'NONE',  ( 8.000000000000007105, 249.8719672152120381, 94.99999999999866418 ) ) ;
#68374 = CARTESIAN_POINT ( 'NONE',  ( -49.62489392740900485, 13.29305723289023966, -47.89781638457069590 ) ) ;
#68375 = CARTESIAN_POINT ( 'NONE',  ( -125.8938041572051389, -170.0000000000000000, -15.56915330777026973 ) ) ;
#68376 = LINE ( 'NONE', #35678, #13132 ) ;
#68377 = ORIENTED_EDGE ( 'NONE', *, *, #12315, .F. ) ;
#68379 = EDGE_CURVE ( 'NONE', #54841, #383, #16129, .T. ) ;
#68378 = CARTESIAN_POINT ( 'NONE',  ( 59.72526569420002573, 11.93313563009889045, 17.22574484112362825 ) ) ;
#68380 = CARTESIAN_POINT ( 'NONE',  ( -60.65612136648952912, 16.25551606627059087, 69.67105917315916486 ) ) ;
#68381 = EDGE_LOOP ( 'NONE', ( #19984, #19758, #54507, #27983 ) ) ;
#68382 = EDGE_LOOP ( 'NONE', ( #56032, #35329, #58689, #48226 ) ) ;
#68383 = CYLINDRICAL_SURFACE ( 'NONE', #27424, 65.00000000000000000 ) ;
#68384 = CARTESIAN_POINT ( 'NONE',  ( -173.5394735271662796, 87.59446374803710000, -76.55650775521371543 ) ) ;
#68385 = DIRECTION ( 'NONE',  ( -0.000000000000000000, 1.000000000000000000, -0.000000000000000000 ) ) ;
#68386 = ORIENTED_EDGE ( 'NONE', *, *, #2696, .F. ) ;
#68387 = EDGE_CURVE ( 'NONE', #11547, #34612, #9946, .T. ) ;
#68388 = FACE_OUTER_BOUND ( 'NONE', #30640, .T. ) ;
#68389 = CARTESIAN_POINT ( 'NONE',  ( -4.725257700476000799, 6.708862164351557134, 17.60467424153223348 ) ) ;
#68390 = CARTESIAN_POINT ( 'NONE',  ( -55.15976438495108169, -34.41253982194112382, 170.0000000000000000 ) ) ;
#68391 = EDGE_CURVE ( 'NONE', #18937, #19589, #37021, .T. ) ;
#68392 = CARTESIAN_POINT ( 'NONE',  ( -85.64924756730680144, 26.19583280090851218, 35.16995575340898483 ) ) ;
#68393 = CARTESIAN_POINT ( 'NONE',  ( 149.9611936883170529, 52.04073442100943936, 90.49744601638548147 ) ) ;
#68394 = CARTESIAN_POINT ( 'NONE',  ( 93.92910382125423041, 22.04227458821877761, 38.95172454535422446 ) ) ;
#68395 = VERTEX_POINT ( 'NONE', #47904 ) ;
#68396 = CARTESIAN_POINT ( 'NONE',  ( 133.8566784816069344, 41.42467568809808398, 2.665790248531674678 ) ) ;
#68397 = CARTESIAN_POINT ( 'NONE',  ( -27.70115495247213033, 10.02455692117576369, 44.23695096961487394 ) ) ;
#68398 = CARTESIAN_POINT ( 'NONE',  ( 203.1414537950835211, 105.9225671689748367, 44.05506648896800215 ) ) ;
#68399 = AXIS2_PLACEMENT_3D ( 'NONE', #12931, #33692, #38965 ) ;
#68400 = CARTESIAN_POINT ( 'NONE',  ( -22.50000000000000355, 207.5000000000000284, 1.999999999999998224 ) ) ;
#68402 = VERTEX_POINT ( 'NONE', #20485 ) ;
#68401 = LINE ( 'NONE', #62069, #54524 ) ;
#68403 = CARTESIAN_POINT ( 'NONE',  ( 67.93317348534930034, 14.90531593353391671, 42.99690714744312459 ) ) ;
#68404 = VERTEX_POINT ( 'NONE', #36682 ) ;
#68405 = EDGE_CURVE ( 'NONE', #48270, #30095, #15217, .T. ) ;
#68406 = VECTOR ( 'NONE', #42901, 1000.000000000000000 ) ;
#68407 = VERTEX_POINT ( 'NONE', #69012 ) ;
#68408 = CARTESIAN_POINT ( 'NONE',  ( 117.0069443446175370, 33.26475960880693350, -67.01675685757288647 ) ) ;
#68409 = CARTESIAN_POINT ( 'NONE',  ( -20.00000000000002842, 3.680555555555560243, 4.000000000000000000 ) ) ;
#68410 = CARTESIAN_POINT ( 'NONE',  ( 0.000000000000000000, 0.000000000000000000, 40.00000000000003553 ) ) ;
#68411 = EDGE_CURVE ( 'NONE', #17896, #42033, #4326, .T. ) ;
#68412 = CARTESIAN_POINT ( 'NONE',  ( -33.17493614366368604, 47.98885325116288669, 27.58472369403420643 ) ) ;
#68413 = CARTESIAN_POINT ( 'NONE',  ( -124.1033713525885247, 45.32626312604504903, 72.25125535819661593 ) ) ;
#68414 = CARTESIAN_POINT ( 'NONE',  ( -86.06525741550316866, 26.37048289224655662, -14.51723273906646305 ) ) ;
#68415 = LINE ( 'NONE', #47623, #5020 ) ;
#68416 = CARTESIAN_POINT ( 'NONE',  ( -46.66904755831210139, 6.635317295611287136E-14, 0.000000000000000000 ) ) ;
#68417 = ORIENTED_EDGE ( 'NONE', *, *, #60509, .F. ) ;
#68418 = ORIENTED_EDGE ( 'NONE', *, *, #28463, .T. ) ;
#68419 = CARTESIAN_POINT ( 'NONE',  ( -109.3585523124447576, 37.67345343047318806, 13.70687730902988477 ) ) ;
#68420 = CARTESIAN_POINT ( 'NONE',  ( -86.11230725916330186, 26.39026888680171012, -43.64915368985550259 ) ) ;
#68421 = CARTESIAN_POINT ( 'NONE',  ( 116.5854913516927951, 31.92838880174207716, 86.78310992652015443 ) ) ;
#68422 = CARTESIAN_POINT ( 'NONE',  ( -417.6627218934913230, 179.4906275429376308, 111.5502958579881749 ) ) ;
#68423 = CARTESIAN_POINT ( 'NONE',  ( -30.63688085183209253, 13.36654888745402836, 6.893342933764156300 ) ) ;
#68424 = CARTESIAN_POINT ( 'NONE',  ( 103.0463737467386665, 25.69265572325593538, -95.00000000000133582 ) ) ;
#68425 = CARTESIAN_POINT ( 'NONE',  ( 159.6725804802006223, 59.38339663535509061, -63.28528528614057791 ) ) ;
#68426 = ORIENTED_EDGE ( 'NONE', *, *, #47776, .T. ) ;
#68427 = ORIENTED_EDGE ( 'NONE', *, *, #41457, .F. ) ;
#68428 = ORIENTED_EDGE ( 'NONE', *, *, #8092, .T. ) ;
#68429 = CARTESIAN_POINT ( 'NONE',  ( 38.91512155099543691, 9.360679678889628264, -50.61981746542778637 ) ) ;
#68430 = CARTESIAN_POINT ( 'NONE',  ( 110.0000000000000284, -21.42428528562853529, 5.000000000000004441 ) ) ;
#68431 = CARTESIAN_POINT ( 'NONE',  ( -36.37229078872272936, 11.47648211215766167, -75.33199238139795284 ) ) ;
#68432 = CARTESIAN_POINT ( 'NONE',  ( 433.3728120124416705, 395.0000000000066507, -132.4852380479447618 ) ) ;
#68433 = PRODUCT_RELATED_PRODUCT_CATEGORY ( 'part', '', ( #6321 ) ) ;
#68434 = DIRECTION ( 'NONE',  ( 1.000000000000000000, 0.000000000000000000, 0.000000000000000000 ) ) ;
#68435 = CARTESIAN_POINT ( 'NONE',  ( 8.540853903193184493, 6.376814430361479324, -14.22886706902527898 ) ) ;
#68436 = EDGE_LOOP ( 'NONE', ( #64436, #37288, #29621 ) ) ;
#68437 = CARTESIAN_POINT ( 'NONE',  ( 18.43272992546528855, 7.606837839440252935, 17.69278249756995081 ) ) ;
#68438 = CARTESIAN_POINT ( 'NONE',  ( 188.5645326065591689, 86.51153908883290455, 63.03378560201070258 ) ) ;
#68439 = CARTESIAN_POINT ( 'NONE',  ( -122.8118341587044711, 44.49743491855735300, 4.422630839854232221 ) ) ;
#68440 = DIRECTION ( 'NONE',  ( 1.000000000000000000, 0.000000000000000000, -2.775557561562891844E-16 ) ) ;
#68441 = CARTESIAN_POINT ( 'NONE',  ( 130.7260704202055024, 39.56565398554880630, -23.51021375569008853 ) ) ;
#68443 = ADVANCED_FACE ( 'NONE', ( #35038 ), #31735, .T. ) ;
#68442 = DIRECTION ( 'NONE',  ( -0.000000000000000000, 1.000000000000000000, -0.000000000000000000 ) ) ;
#68444 = CARTESIAN_POINT ( 'NONE',  ( 10.82760985890677397, 7.398654328676832925, 16.31652703457590547 ) ) ;
#68445 = EDGE_CURVE ( 'NONE', #60636, #34560, #4656, .T. ) ;
#68446 = AXIS2_PLACEMENT_3D ( 'NONE', #63797, #68385, #26502 ) ;
#68447 = ORIENTED_EDGE ( 'NONE', *, *, #49203, .F. ) ;
#68448 = CARTESIAN_POINT ( 'NONE',  ( 185.5415406465188823, 83.23025870924406888, 3.913947997146966618 ) ) ;
#68449 = SHAPE_DEFINITION_REPRESENTATION ( #9074, #31639 ) ;
#68450 = DIRECTION ( 'NONE',  ( 1.000000000000000000, 0.000000000000000000, 0.000000000000000000 ) ) ;
#68451 = CARTESIAN_POINT ( 'NONE',  ( -149.5074843970971301, -170.0000000000000000, 57.56537183036274996 ) ) ;
#68452 = CARTESIAN_POINT ( 'NONE',  ( 39.40195752203892710, 8.409560354027375340, -77.46436805589148378 ) ) ;
#68453 = STYLED_ITEM ( 'NONE', ( #9280 ), #65002 ) ;
#68454 = CARTESIAN_POINT ( 'NONE',  ( 188.4365915667138154, 87.87248959723052621, -42.21599812139930918 ) ) ;
#68455 = ORIENTED_EDGE ( 'NONE', *, *, #20966, .F. ) ;
#68456 = ORIENTED_EDGE ( 'NONE', *, *, #69325, .T. ) ;
#68458 = EDGE_CURVE ( 'NONE', #5523, #2888, #8324, .T. ) ;
#68457 = LINE ( 'NONE', #40676, #47101 ) ;
#68459 = CYLINDRICAL_SURFACE ( 'NONE', #36032, 65.00000000000000000 ) ;
#68460 = ORIENTED_EDGE ( 'NONE', *, *, #64362, .T. ) ;
#68461 = EDGE_CURVE ( 'NONE', #59075, #31099, #42634, .T. ) ;
#68462 = CARTESIAN_POINT ( 'NONE',  ( 116.9200705848630548, 32.09536795999726166, 67.40972273578582019 ) ) ;
#68463 = ORIENTED_EDGE ( 'NONE', *, *, #37017, .T. ) ;
#68464 = CARTESIAN_POINT ( 'NONE',  ( 128.4157044224114941, 39.39296260757095780, -75.55268868015734540 ) ) ;
#68465 = CARTESIAN_POINT ( 'NONE',  ( 126.8947007444828046, 37.37669340849689092, 34.20897586740451146 ) ) ;
#68466 = EDGE_CURVE ( 'NONE', #25958, #417, #68674, .T. ) ;
#68467 = DIRECTION ( 'NONE',  ( 0.000000000000000000, -0.000000000000000000, -1.000000000000000000 ) ) ;
#68468 = DIRECTION ( 'NONE',  ( -0.5877852522924802425, 0.8090169943749422332, 5.102127870520019688E-18 ) ) ;
#68469 = CARTESIAN_POINT ( 'NONE',  ( -12.71198166530320606, 21.52685583500265665, 0.000000000000000000 ) ) ;
#68471 = ORIENTED_EDGE ( 'NONE', *, *, #54533, .F. ) ;
#68470 = DIRECTION ( 'NONE',  ( -0.000000000000000000, 1.000000000000000000, -0.000000000000000000 ) ) ;
#68472 = CARTESIAN_POINT ( 'NONE',  ( -37.26544795852028358, 8.987879696173472155, 13.32819299319723605 ) ) ;
#68473 = ORIENTED_EDGE ( 'NONE', *, *, #34942, .F. ) ;
#68474 = ORIENTED_EDGE ( 'NONE', *, *, #62422, .T. ) ;
#68475 = CARTESIAN_POINT ( 'NONE',  ( -172.3127615181936676, 87.73358064377640630, 4.009540804375925305 ) ) ;
#68476 = FACE_OUTER_BOUND ( 'NONE', #13760, .T. ) ;
#68477 = CARTESIAN_POINT ( 'NONE',  ( -146.1201263095600780, 62.66021356509617135, -35.61751423064927735 ) ) ;
#68479 = EDGE_LOOP ( 'NONE', ( #66700, #51436, #63982, #15135, #8250, #45695 ) ) ;
#68478 = CARTESIAN_POINT ( 'NONE',  ( -129.6079169496902068, 50.20899308323962629, 71.48448238020641554 ) ) ;
#68480 = LINE ( 'NONE', #36470, #52179 ) ;
#68481 = VECTOR ( 'NONE', #42616, 1000.000000000000000 ) ;
#68482 = CARTESIAN_POINT ( 'NONE',  ( 0.000000000000000000, 0.000000000000000000, 0.000000000000000000 ) ) ;
#68483 = ORIENTED_EDGE ( 'NONE', *, *, #7661, .F. ) ;
#68484 = DIRECTION ( 'NONE',  ( -0.000000000000000000, -0.000000000000000000, -1.000000000000000000 ) ) ;
#68485 = EDGE_CURVE ( 'NONE', #5635, #68321, #8305, .T. ) ;
#68486 = CARTESIAN_POINT ( 'NONE',  ( -129.4036885357273547, 50.06837984316182144, -62.62615786572060728 ) ) ;
#68487 = CARTESIAN_POINT ( 'NONE',  ( 63.01563776193091826, 12.67277567978495512, -89.40979201309708913 ) ) ;
#68488 = DIRECTION ( 'NONE',  ( 0.000000000000000000, -1.000000000000000000, 0.000000000000000000 ) ) ;
#68489 = CARTESIAN_POINT ( 'NONE',  ( 31.11269837220806522, 4.999999999999936939, 2.000000000000001776 ) ) ;
#68490 = EDGE_LOOP ( 'NONE', ( #23526, #35858, #3198, #36059 ) ) ;
#68491 = CIRCLE ( 'NONE', #40423, 19.99999999999997868 ) ;
#68492 = EDGE_LOOP ( 'NONE', ( #15078, #21150, #47906, #67090 ) ) ;
#68493 = CARTESIAN_POINT ( 'NONE',  ( 182.7789203043889756, 80.33475476315297215, -63.25125628519738541 ) ) ;
#68494 = CARTESIAN_POINT ( 'NONE',  ( -172.3018509397888067, 86.22053936367352378, -34.74525666140065994 ) ) ;
#68495 = LINE ( 'NONE', #20300, #8215 ) ;
#68496 = VECTOR ( 'NONE', #41555, 1000.000000000000227 ) ;
#68497 = CARTESIAN_POINT ( 'NONE',  ( 103.4725384926517222, 26.96797537091727293, -73.50340331479570466 ) ) ;
#68498 = LINE ( 'NONE', #57604, #30944 ) ;
#68499 = CARTESIAN_POINT ( 'NONE',  ( -843.0889760620008246, -561.4220607509099636, 10.00000000000000000 ) ) ;
#68500 = CARTESIAN_POINT ( 'NONE',  ( 67.54641595172913071, 14.80690682047551476, -37.22417361863564622 ) ) ;
#68501 = CARTESIAN_POINT ( 'NONE',  ( -124.1095621208148572, 46.52671329146387791, 45.46233580508904026 ) ) ;
#68502 = CARTESIAN_POINT ( 'NONE',  ( 210.4897348480408255, 114.6382060222044572, 58.78115735310451839 ) ) ;
#68503 = VERTEX_POINT ( 'NONE', #53170 ) ;
#68504 = CARTESIAN_POINT ( 'NONE',  ( -108.6634958860518196, 36.14357436892403541, -11.72466063708648143 ) ) ;
#68505 = ORIENTED_EDGE ( 'NONE', *, *, #67074, .T. ) ;
#68506 = CARTESIAN_POINT ( 'NONE',  ( -38.26732153931115477, 10.81230693396213738, 7.759653135233770982 ) ) ;
#68507 = CARTESIAN_POINT ( 'NONE',  ( 35.38849213634181723, -46.38060988817211694, 27.58472315868180402 ) ) ;
#68508 = CYLINDRICAL_SURFACE ( 'NONE', #57671, 65.00000000000000000 ) ;
#68509 = PLANE ( 'NONE',  #9759 ) ;
#68510 = CARTESIAN_POINT ( 'NONE',  ( 38.91512155099545112, 9.360679678889628264, 3.069283715499573351 ) ) ;
#68511 = CARTESIAN_POINT ( 'NONE',  ( 188.9999999999999432, -57.00000000000007816, -2.000000000000000888 ) ) ;
#68512 = CARTESIAN_POINT ( 'NONE',  ( 39.40195752203892710, 8.409560354027373563, 3.069283715499574683 ) ) ;
#68513 = DIRECTION ( 'NONE',  ( -0.000000000000000000, -0.000000000000000000, -1.000000000000000000 ) ) ;
#68514 = CARTESIAN_POINT ( 'NONE',  ( -37.37206033059243282, 11.66494618096612967, -20.56726544046575000 ) ) ;
#68515 = EDGE_CURVE ( 'NONE', #2626, #50048, #43132, .T. ) ;
#68516 = EDGE_CURVE ( 'NONE', #4373, #38200, #58458, .T. ) ;
#68517 = ORIENTED_EDGE ( 'NONE', *, *, #38675, .T. ) ;
#68518 = FACE_OUTER_BOUND ( 'NONE', #65930, .T. ) ;
#68519 = ORIENTED_EDGE ( 'NONE', *, *, #40356, .T. ) ;
#68520 = FACE_OUTER_BOUND ( 'NONE', #17095, .T. ) ;
#68521 = LINE ( 'NONE', #63248, #28587 ) ;
#68522 = CARTESIAN_POINT ( 'NONE',  ( -190.6985136298602015, 109.1272424661243434, 16.02916387300914280 ) ) ;
#68523 = B_SPLINE_CURVE_WITH_KNOTS ( 'NONE', 3,
 ( #13410, #62285, #34182, #8484, #67244, #2855, #19027, #57017, #44727, #28544, #55618, #7789 ),
 .UNSPECIFIED., .F., .F.,
 ( 4, 2, 2, 2, 2, 4 ),
 ( 0.000000000000000000, 0.002485491944061524097, 0.004970983888123048193, 0.007456475832184572723, 0.008699221804215350601, 0.009941967776246129346 ),
 .UNSPECIFIED. ) ;
#68524 = CARTESIAN_POINT ( 'NONE',  ( -78.66644367742111399, 23.39876645725287219, -50.11545063171791270 ) ) ;
#68526 = EDGE_CURVE ( 'NONE', #18178, #23198, #29754, .T. ) ;
#68525 = CARTESIAN_POINT ( 'NONE',  ( -9.771516655894554759, 7.025139475821121415, -77.02225727686567325 ) ) ;
#68527 = FACE_BOUND ( 'NONE', #45232, .T. ) ;
#68528 = CARTESIAN_POINT ( 'NONE',  ( 152.2924710224605462, 54.98503313872889464, -38.19290532517972281 ) ) ;
#68529 = EDGE_CURVE ( 'NONE', #25377, #64121, #15905, .T. ) ;
#68530 = EDGE_LOOP ( 'NONE', ( #13024, #42235, #30141, #47349, #30632, #13553, #59055, #61296, #39616 ) ) ;
#68531 = EDGE_CURVE ( 'NONE', #14479, #15873, #62288, .T. ) ;
#68532 = DIRECTION ( 'NONE',  ( -0.5802180898069654313, 0.8144611520881498423, 3.098709970130927464E-15 ) ) ;
#68533 = VECTOR ( 'NONE', #48310, 1000.000000000000000 ) ;
#68534 = CARTESIAN_POINT ( 'NONE',  ( 39.40195752203892710, -170.0000000000000000, -16.27526687496408542 ) ) ;
#68535 = CARTESIAN_POINT ( 'NONE',  ( 180.2565361171340612, 79.19912802278402353, -24.34669578964250647 ) ) ;
#68536 = CARTESIAN_POINT ( 'NONE',  ( -108.1180879163843116, 36.99199941971028949, 69.59835785737806191 ) ) ;
#68537 = CARTESIAN_POINT ( 'NONE',  ( -127.4644500646574272, 48.74852676951793029, -49.75091178047936324 ) ) ;
#68538 = VERTEX_POINT ( 'NONE', #9600 ) ;
#68539 = FACE_OUTER_BOUND ( 'NONE', #34154, .T. ) ;
#68540 = CARTESIAN_POINT ( 'NONE',  ( -5.885876544836661672, 6.772369038004089070, -23.32255204279795890 ) ) ;
#68541 = CARTESIAN_POINT ( 'NONE',  ( 204.6977192012829789, 108.0580384837234931, -90.01503221354883522 ) ) ;
#68542 = LINE ( 'NONE', #19659, #22567 ) ;
#68543 = EDGE_CURVE ( 'NONE', #14449, #33323, #68347, .T. ) ;
#68544 = CARTESIAN_POINT ( 'NONE',  ( 141.3403471770513136, 46.13063628128490024, 36.44774808231112218 ) ) ;
#68545 = ORIENTED_EDGE ( 'NONE', *, *, #11819, .T. ) ;
#68546 = CARTESIAN_POINT ( 'NONE',  ( 197.2197025888162045, 96.62026035493821041, 36.04745238432391830 ) ) ;
#68547 = LINE ( 'NONE', #47418, #31693 ) ;
#68548 = ADVANCED_FACE ( 'NONE', ( #40308 ), #14865, .F. ) ;
#68549 = CARTESIAN_POINT ( 'NONE',  ( 187.5246323291926842, 86.86207184872507980, 40.69048242448342734 ) ) ;
#68550 = DIRECTION ( 'NONE',  ( 1.000000000000000000, -0.000000000000000000, -0.000000000000000000 ) ) ;
#68551 = LINE ( 'NONE', #9814, #54330 ) ;
#68552 = VECTOR ( 'NONE', #18815, 1000.000000000000000 ) ;
#68553 = ORIENTED_EDGE ( 'NONE', *, *, #44711, .F. ) ;
#68554 = CARTESIAN_POINT ( 'NONE',  ( 174.9161599490640242, 73.97365196673301568, 59.37798453004636912 ) ) ;
#68555 = ORIENTED_EDGE ( 'NONE', *, *, #23826, .T. ) ;
#68556 = CARTESIAN_POINT ( 'NONE',  ( -108.0980548770427561, 35.83569586822708430, -37.75577146733352407 ) ) ;
#68557 = CARTESIAN_POINT ( 'NONE',  ( 126.4375826614094507, 37.12160219610346701, 89.54261223166750483 ) ) ;
#68558 = CARTESIAN_POINT ( 'NONE',  ( -57.65733424639442717, 15.39521790791522982, 44.85474620224701425 ) ) ;
#68560 = VERTEX_POINT ( 'NONE', #64434 ) ;
#68559 = CARTESIAN_POINT ( 'NONE',  ( 152.8672128926847904, 55.41186463791520111, 4.138895294562964899 ) ) ;
#68561 = CARTESIAN_POINT ( 'NONE',  ( -173.1211646369891071, 87.12891641440859303, 45.82169460664104577 ) ) ;
#68562 = VECTOR ( 'NONE', #49361, 1000.000000000000000 ) ;
#68563 = DIRECTION ( 'NONE',  ( -1.000000000000000000, 0.000000000000000000, 0.000000000000000000 ) ) ;
#68564 = CARTESIAN_POINT ( 'NONE',  ( 117.3145357257065342, 33.41973663092564095, -40.87229264417645425 ) ) ;
#68565 = ORIENTED_EDGE ( 'NONE', *, *, #63242, .T. ) ;
#68566 = B_SPLINE_CURVE_WITH_KNOTS ( 'NONE', 3,
 ( #44580, #1667, #6242, #7297 ),
 .UNSPECIFIED., .F., .F.,
 ( 4, 4 ),
 ( 9.900409499072286585E-07, 0.05658314289920115397 ),
 .UNSPECIFIED. ) ;
#68567 = DIRECTION ( 'NONE',  ( 0.000000000000000000, 0.5000000000000006661, -0.8660254037844382635 ) ) ;
#68568 = DIRECTION ( 'NONE',  ( -0.7071067811865475727, -0.7071067811865475727, 3.925231146709437301E-16 ) ) ;
#68569 = ORIENTED_EDGE ( 'NONE', *, *, #22559, .F. ) ;
#68570 = CARTESIAN_POINT ( 'NONE',  ( 141.3403471770513420, 46.13063628128487181, 63.29229867277483379 ) ) ;
#68571 = CARTESIAN_POINT ( 'NONE',  ( -180.6209674222601791, 97.47999311542514533, 38.15503575396904523 ) ) ;
#68572 = B_SPLINE_CURVE_WITH_KNOTS ( 'NONE', 3,
 ( #3795, #19273, #19982, #31231, #9079, #67825, #41085, #20657, #4487, #51979 ),
 .UNSPECIFIED., .F., .F.,
 ( 4, 2, 2, 2, 4 ),
 ( 0.000000000000000000, 0.002501040261221833608, 0.005002080522443667215, 0.007503120783665500823, 0.01000416104488733443 ),
 .UNSPECIFIED. ) ;
#68573 = CARTESIAN_POINT ( 'NONE',  ( 150.0501577908836737, 52.10460126680128212, 64.87989132378601198 ) ) ;
#68574 = CARTESIAN_POINT ( 'NONE',  ( 93.87111289824409255, 23.09598275302506920, 39.22769905219760744 ) ) ;
#68575 = EDGE_LOOP ( 'NONE', ( #54091, #6535, #34120, #50121 ) ) ;
#68576 = CARTESIAN_POINT ( 'NONE',  ( 45.35146934743634262, 10.27620685439442028, 15.16236855302814490 ) ) ;
#68577 = ORIENTED_EDGE ( 'NONE', *, *, #49365, .T. ) ;
#68578 = AXIS2_PLACEMENT_3D ( 'NONE', #52920, #4745, #25536 ) ;
#68579 = CARTESIAN_POINT ( 'NONE',  ( 153.4509883044095773, 55.84811350575045452, -23.11593860723543870 ) ) ;
#68580 = CARTESIAN_POINT ( 'NONE',  ( 212.0075063341773784, 118.7912820769029594, -18.69025613062296642 ) ) ;
#68581 = CARTESIAN_POINT ( 'NONE',  ( 104.7227067006896419, 27.50728936118535017, 32.01079824686573261 ) ) ;
#68582 = CARTESIAN_POINT ( 'NONE',  ( -155.7433525314458791, 69.65452735858370659, -64.98229209234851567 ) ) ;
#68583 = CARTESIAN_POINT ( 'NONE',  ( -65.00000000000000000, 7.960204194457797252E-15, 85.00000000000000000 ) ) ;
#68584 = CARTESIAN_POINT ( 'NONE',  ( 187.0788993276711949, 86.37277723143233743, 5.450255465685347467 ) ) ;
#68585 = CARTESIAN_POINT ( 'NONE',  ( 210.9747454890631957, 115.3673079504856105, -39.71291949852400194 ) ) ;
#68586 = CARTESIAN_POINT ( 'NONE',  ( 55.61348889666937367, 50.24791103897128863, 41.38025477438755928 ) ) ;
#68587 = ORIENTED_EDGE ( 'NONE', *, *, #33424, .F. ) ;
#68588 = CARTESIAN_POINT ( 'NONE',  ( 39.54205320694412507, -51.58901073076707888, 40.00000000000003553 ) ) ;
#68589 = ORIENTED_EDGE ( 'NONE', *, *, #13575, .F. ) ;
#68590 = CARTESIAN_POINT ( 'NONE',  ( 41.34269507549203126, 9.685203600174693506, -23.53625253713786236 ) ) ;
#68591 = CARTESIAN_POINT ( 'NONE',  ( -78.19460645047368530, 22.14203592077028304, 3.573650549209445249 ) ) ;
#68592 = B_SPLINE_CURVE_WITH_KNOTS ( 'NONE', 3,
 ( #63066, #41610, #19460, #46187 ),
 .UNSPECIFIED., .F., .F.,
 ( 4, 4 ),
 ( 9.900409498985715583E-07, 0.05658314289920115397 ),
 .UNSPECIFIED. ) ;
#68593 = PLANE ( 'NONE',  #10901 ) ;
#68594 = CARTESIAN_POINT ( 'NONE',  ( 20.74561700410410836, 7.717362891868937425, 43.16396733258935825 ) ) ;
#68595 = CARTESIAN_POINT ( 'NONE',  ( -107.2385267828037314, 36.51474259889400997, -21.30232734929181504 ) ) ;
#68596 = ORIENTED_EDGE ( 'NONE', *, *, #31403, .T. ) ;
#68597 = CARTESIAN_POINT ( 'NONE',  ( -71.97434903038468690, 19.88430675376529777, 61.34002548381291575 ) ) ;
#68598 = CARTESIAN_POINT ( 'NONE',  ( -305.1627218934913230, 399.9999999999997726, 1.050295857988214898 ) ) ;
#68599 = ORIENTED_EDGE ( 'NONE', *, *, #6009, .F. ) ;
#68600 = ORIENTED_EDGE ( 'NONE', *, *, #25887, .T. ) ;
#68602 = EDGE_CURVE ( 'NONE', #35856, #8573, #59493, .T. ) ;
#68601 = CARTESIAN_POINT ( 'NONE',  ( -149.5074843970971301, 64.17983161892345834, 30.72082123989904900 ) ) ;
#68603 = CARTESIAN_POINT ( 'NONE',  ( 209.3223706822284100, 18.00000000000002842, 31.44247402469554942 ) ) ;
#68604 = CARTESIAN_POINT ( 'NONE',  ( 39.77028211725815510, -51.87520073220884598, 43.58025477438756212 ) ) ;
#68605 = SURFACE_STYLE_USAGE ( .BOTH. , #3902 ) ;
#68606 = CARTESIAN_POINT ( 'NONE',  ( -144.3945994505580757, 59.96115386701888639, 5.883885038153297664 ) ) ;
#68607 = EDGE_CURVE ( 'NONE', #32425, #44262, #44010, .T. ) ;
#68608 = AXIS2_PLACEMENT_3D ( 'NONE', #62111, #3381, #23463 ) ;
#68609 = ORIENTED_EDGE ( 'NONE', *, *, #24618, .T. ) ;
#68610 = CARTESIAN_POINT ( 'NONE',  ( 4.165045035621076863, -64.88046627338039229, 43.58025477438756923 ) ) ;
#68611 = EDGE_LOOP ( 'NONE', ( #64046, #2581, #56700, #36436 ) ) ;
#68612 = CARTESIAN_POINT ( 'NONE',  ( 209.6525588430077960, 113.3929734759397121, 4.228066349643490263 ) ) ;
#68613 = CARTESIAN_POINT ( 'NONE',  ( -143.4048679855201271, 60.45763799613828837, 42.58799473479032116 ) ) ;
#68614 = PRESENTATION_LAYER_ASSIGNMENT (  '', '', ( #65357 ) ) ;
#68615 = DIRECTION ( 'NONE',  ( -0.000000000000000000, -0.000000000000000000, 1.000000000000000000 ) ) ;
#68616 = CIRCLE ( 'NONE', #30466, 5.000000000000115463 ) ;
#68617 = EDGE_CURVE ( 'NONE', #66303, #18940, #29164, .T. ) ;
#68618 = VERTEX_POINT ( 'NONE', #1462 ) ;
#68619 = ORIENTED_EDGE ( 'NONE', *, *, #18660, .T. ) ;
#68620 = CARTESIAN_POINT ( 'NONE',  ( 114.7429429236411238, -21.94266591301279234, -1.615775360921249959 ) ) ;
#68621 = CARTESIAN_POINT ( 'NONE',  ( -130.4988625216997775, 50.82592816381205125, 85.88177662789409794 ) ) ;
#68622 = CYLINDRICAL_SURFACE ( 'NONE', #8328, 7.500000000000020428 ) ;
#68623 = CARTESIAN_POINT ( 'NONE',  ( 311.9975424824652350, 296.0000000000000000, 529.9060149868646477 ) ) ;
#68624 = CARTESIAN_POINT ( 'NONE',  ( 17.09380310378440981, 6.545254173319234425, 83.78868157438149922 ) ) ;
#68625 = CARTESIAN_POINT ( 'NONE',  ( 10.24659718932696251, 7.392712022583040721, 86.13955876464233086 ) ) ;
#68626 = EDGE_LOOP ( 'NONE', ( #27082, #17882 ) ) ;
#68627 = DIRECTION ( 'NONE',  ( 1.000000000000000000, 0.000000000000000000, 0.000000000000000000 ) ) ;
#68628 = CYLINDRICAL_SURFACE ( 'NONE', #51841, 5.000000000000004441 ) ;
#68629 = ORIENTED_EDGE ( 'NONE', *, *, #61996, .T. ) ;
#68630 = CARTESIAN_POINT ( 'NONE',  ( -79.14678386417813272, 22.50468917936072799, 18.57365054920947145 ) ) ;
#68631 = ORIENTED_EDGE ( 'NONE', *, *, #12613, .T. ) ;
#68632 = LINE ( 'NONE', #13787, #65751 ) ;
#68633 = VERTEX_POINT ( 'NONE', #22918 ) ;
#68634 = ORIENTED_EDGE ( 'NONE', *, *, #8248, .F. ) ;
#68635 = CARTESIAN_POINT ( 'NONE',  ( -119.5563837756079266, 43.64229894412653010, 15.31786711092669329 ) ) ;
#68636 = CARTESIAN_POINT ( 'NONE',  ( -178.0658882571759989, 92.80593104957419825, 59.52230928071593041 ) ) ;
#68637 = CARTESIAN_POINT ( 'NONE',  ( 21.44031696305384926, 6.747195267824408482, 15.62434647642277774 ) ) ;
#68638 = ORIENTED_EDGE ( 'NONE', *, *, #25425, .F. ) ;
#68639 = CARTESIAN_POINT ( 'NONE',  ( -38.19016260632597692, 10.79737009263853587, 88.12259832690817518 ) ) ;
#68640 = CARTESIAN_POINT ( 'NONE',  ( 175.8874477961784635, 74.89984466412603581, -65.14078283235144795 ) ) ;
#68641 = DIRECTION ( 'NONE',  ( -0.000000000000000000, 0.000000000000000000, 1.000000000000000000 ) ) ;
#68642 = CARTESIAN_POINT ( 'NONE',  ( 103.8317086685000135, 26.02720265156212776, -39.52255369601063961 ) ) ;
#68643 = CARTESIAN_POINT ( 'NONE',  ( -23.98903001682803193, 8.486614814224626713, 36.72224464285193335 ) ) ;
#68644 = CARTESIAN_POINT ( 'NONE',  ( -147.7895256390024485, 64.04409735547008609, -61.80240963661621834 ) ) ;
#68645 = ORIENTED_EDGE ( 'NONE', *, *, #13433, .T. ) ;
#68646 = VECTOR ( 'NONE', #8241, 1000.000000000000114 ) ;
#68647 = CARTESIAN_POINT ( 'NONE',  ( 0.000000000000000000, 0.000000000000000000, 5.000000000000000000 ) ) ;
#68648 = CARTESIAN_POINT ( 'NONE',  ( -84.21836162213169530, 25.60181819557221772, -74.52576626856495068 ) ) ;
#68650 = LINE ( 'NONE', #36308, #19213 ) ;
#68649 = AXIS2_PLACEMENT_3D ( 'NONE', #52275, #61452, #57217 ) ;
#68651 = DIRECTION ( 'NONE',  ( -0.000000000000000000, 1.000000000000000000, -0.000000000000000000 ) ) ;
#68652 = EDGE_CURVE ( 'NONE', #51387, #64727, #48235, .T. ) ;
#68653 = DIRECTION ( 'NONE',  ( -2.201526392813400543E-16, -1.184691869787096980E-16, 1.000000000000000000 ) ) ;
#68654 = CARTESIAN_POINT ( 'NONE',  ( 130.3019683985926918, 39.31883119822050077, 3.544598928792382697 ) ) ;
#68655 = CARTESIAN_POINT ( 'NONE',  ( -152.9121563765243650, 67.12206067149024591, 18.06274683814091020 ) ) ;
#68656 = CARTESIAN_POINT ( 'NONE',  ( 26.11269837220812562, 31.11269837220800483, 85.00100000000000477 ) ) ;
#68657 = CARTESIAN_POINT ( 'NONE',  ( 210.0122310839192323, 115.7355030290287914, 42.02281805116941626 ) ) ;
#68658 = CIRCLE ( 'NONE', #16979, 242.4895526022646379 ) ;
#68659 = CARTESIAN_POINT ( 'NONE',  ( 163.2886151008987952, 62.32020850087172192, 5.325560534978804661 ) ) ;
#68660 = CARTESIAN_POINT ( 'NONE',  ( -107.0751323097254755, 35.28386110859232616, 32.23120985814819761 ) ) ;
#68662 = ORIENTED_EDGE ( 'NONE', *, *, #25985, .F. ) ;
#68661 = EDGE_CURVE ( 'NONE', #15138, #38316, #24088, .T. ) ;
#68663 = CARTESIAN_POINT ( 'NONE',  ( -4.337405327941355360, 24.62086340933515416, 0.000000000000000000 ) ) ;
#68664 = VERTEX_POINT ( 'NONE', #33824 ) ;
#68665 = FACE_OUTER_BOUND ( 'NONE', #50871, .T. ) ;
#68666 = VERTEX_POINT ( 'NONE', #1118 ) ;
#68667 = CARTESIAN_POINT ( 'NONE',  ( 16.27775141556968208, 7.523247835309962106, -77.36349468914949057 ) ) ;
#68668 = SURFACE_STYLE_FILL_AREA ( #64085 ) ;
#68669 = CARTESIAN_POINT ( 'NONE',  ( 19.21260320704901403, -55.08522762473832302, 27.58472369377037126 ) ) ;
#68670 = CYLINDRICAL_SURFACE ( 'NONE', #18735, 7.500000000000020428 ) ;
#68671 = DIRECTION ( 'NONE',  ( 0.000000000000000000, -1.000000000000000000, 0.000000000000000000 ) ) ;
#68672 = CARTESIAN_POINT ( 'NONE',  ( -28.13527276074847450, 10.08983026464524002, 4.134317294375541074 ) ) ;
#68673 = CARTESIAN_POINT ( 'NONE',  ( 150.2076397309211586, 52.21780102759851161, -45.51576517098055774 ) ) ;
#68674 = LINE ( 'NONE', #10615, #35274 ) ;
#68675 = DIRECTION ( 'NONE',  ( -0.000000000000000000, 1.000000000000000000, -0.000000000000000000 ) ) ;
#68676 = ORIENTED_EDGE ( 'NONE', *, *, #21801, .F. ) ;
#68677 = EDGE_CURVE ( 'NONE', #24352, #39302, #44363, .T. ) ;
#68678 = ORIENTED_EDGE ( 'NONE', *, *, #67800, .T. ) ;
#68679 = ADVANCED_FACE ( 'NONE', ( #22568 ), #54912, .F. ) ;
#68680 = DIRECTION ( 'NONE',  ( -1.000000000000000000, 0.000000000000000000, 0.000000000000000000 ) ) ;
#68681 = DIRECTION ( 'NONE',  ( -1.000000000000000000, 0.000000000000000000, 0.000000000000000000 ) ) ;
#68682 = CARTESIAN_POINT ( 'NONE',  ( -24.51966494718108081, 5.470267094204372960, 3.061616997868437868E-16 ) ) ;
#68683 = EDGE_CURVE ( 'NONE', #26889, #38519, #42964, .T. ) ;
#68684 = CARTESIAN_POINT ( 'NONE',  ( -9.119248870808011276, 0.000000000000000000, 4.103571619000548232 ) ) ;
#68685 = CARTESIAN_POINT ( 'NONE',  ( 45.76553115525425852, 10.34124506813255095, -73.94115800944651085 ) ) ;
#68686 = DIRECTION ( 'NONE',  ( -1.000000000000000000, 0.000000000000000000, 0.000000000000000000 ) ) ;
#68687 = CARTESIAN_POINT ( 'NONE',  ( 175.5493994043409884, 73.18740965572598611, -65.50213383789414934 ) ) ;
#68688 = CARTESIAN_POINT ( 'NONE',  ( -179.9014775667593540, 95.00669833041663992, -45.42960845675160897 ) ) ;
#68689 = CARTESIAN_POINT ( 'NONE',  ( 91.67571176799447130, 21.20498955963028820, -22.03065998410063386 ) ) ;
#68690 = CARTESIAN_POINT ( 'NONE',  ( -28.81071653159243340, 10.19258396314335080, 71.58963725187859950 ) ) ;
#68691 = CARTESIAN_POINT ( 'NONE',  ( -8.712114576423861223, 23.56346432108866651, 0.000000000000000000 ) ) ;
#68692 = CARTESIAN_POINT ( 'NONE',  ( 162.7963212667074231, 63.21900188423068556, 69.04028839148755026 ) ) ;
#68693 = ADVANCED_FACE ( 'NONE', ( #65487 ), #61, .F. ) ;
#68694 = ORIENTED_EDGE ( 'NONE', *, *, #18763, .T. ) ;
#68695 = CARTESIAN_POINT ( 'NONE',  ( 131.6115093721024607, 41.25402743071399669, 3.006001826248324793 ) ) ;
#68696 = CARTESIAN_POINT ( 'NONE',  ( 417.3372781065086201, 399.9999999999998863, 113.5502958579881891 ) ) ;
#68697 = VECTOR ( 'NONE', #349, 1000.000000000000000 ) ;
#68698 = LINE ( 'NONE', #68372, #15040 ) ;
#68699 = CARTESIAN_POINT ( 'NONE',  ( -107.7677210873466294, 36.80113675102408877, -74.49435489715372682 ) ) ;
#68700 = CARTESIAN_POINT ( 'NONE',  ( -49.11825192196926793, 13.17012322555987680, -38.10387704635710548 ) ) ;
#68701 = EDGE_CURVE ( 'NONE', #10310, #21823, #64787, .T. ) ;
#68702 = ADVANCED_FACE ( 'NONE', ( #32776 ), #6027, .F. ) ;
#68703 = CARTESIAN_POINT ( 'NONE',  ( -0.4228358876318114024, 7.528738343310879877, 92.55318377967873289 ) ) ;
#68704 = AXIS2_PLACEMENT_3D ( 'NONE', #32822, #7497, #54610 ) ;
#68705 = VERTEX_POINT ( 'NONE', #56663 ) ;
#68706 = CARTESIAN_POINT ( 'NONE',  ( -62.15324028806257672, 16.70091357159901335, 67.12728702411425274 ) ) ;
#68707 = VERTEX_POINT ( 'NONE', #14099 ) ;
#68708 = AXIS2_PLACEMENT_3D ( 'NONE', #5921, #11543, #28083 ) ;
#68709 = EDGE_LOOP ( 'NONE', ( #32954, #972, #12882, #35080 ) ) ;
#68710 = CARTESIAN_POINT ( 'NONE',  ( 41.68362887572859421, 9.733053242893493717, 83.95093237084830662 ) ) ;
#68711 = DIRECTION ( 'NONE',  ( 0.000000000000000000, 0.000000000000000000, 1.000000000000000000 ) ) ;
#68712 = DIRECTION ( 'NONE',  ( -0.8118923937861950435, -0.5838071093367415143, 0.000000000000000000 ) ) ;
#68713 = ORIENTED_EDGE ( 'NONE', *, *, #30337, .F. ) ;
#68714 = DIRECTION ( 'NONE',  ( 0.000000000000000000, 0.000000000000000000, -1.000000000000000000 ) ) ;
#68715 = CARTESIAN_POINT ( 'NONE',  ( -13.32397999417976564, -63.99361958670536410, 43.58025477438756212 ) ) ;
#68716 = CARTESIAN_POINT ( 'NONE',  ( 31.95008798096003133, 7.556925044648908241, -15.29275533313533408 ) ) ;
#68717 = LINE ( 'NONE', #59188, #43820 ) ;
#68718 = CARTESIAN_POINT ( 'NONE',  ( -149.9471644042847061, 65.87751327280744817, -76.64767939074971537 ) ) ;
#68719 = CARTESIAN_POINT ( 'NONE',  ( 93.86680996363769225, 22.01878169039502708, 39.19500198369756561 ) ) ;
#68720 = ORIENTED_EDGE ( 'NONE', *, *, #16205, .T. ) ;
#68721 = LINE ( 'NONE', #36382, #40190 ) ;
#68722 = CARTESIAN_POINT ( 'NONE',  ( 12.69192874957004236, 6.421326776602847453, 57.52382708451808213 ) ) ;
#68723 = DIRECTION ( 'NONE',  ( 0.000000000000000000, 0.000000000000000000, -1.000000000000000000 ) ) ;
#68724 = CARTESIAN_POINT ( 'NONE',  ( 198.7129816317746531, 100.1061386900356069, 41.23588947464686072 ) ) ;
#68725 = CARTESIAN_POINT ( 'NONE',  ( 0.000000000000000000, 0.000000000000000000, 5.000000000000000000 ) ) ;
#68727 = EDGE_LOOP ( 'NONE', ( #42515, #15683, #7673, #6653 ) ) ;
#68726 = CARTESIAN_POINT ( 'NONE',  ( 1.118033988749894458, 2.877919977996280320E-15, -23.50000000000000000 ) ) ;
#68728 = ORIENTED_EDGE ( 'NONE', *, *, #11964, .F. ) ;
#68729 = VERTEX_POINT ( 'NONE', #29242 ) ;
#68730 = CARTESIAN_POINT ( 'NONE',  ( -4.000000000000013323, 6.928203230275504332, -9.500000000000000000 ) ) ;
#68731 = ADVANCED_FACE ( 'NONE', ( #66546 ), #23961, .F. ) ;
#68732 = CARTESIAN_POINT ( 'NONE',  ( 198.8687991397275425, 98.67887821384410074, -75.39677907356383457 ) ) ;
#68733 = DIRECTION ( 'NONE',  ( -0.000000000000000000, -0.000000000000000000, -1.000000000000000000 ) ) ;
#68734 = DIRECTION ( 'NONE',  ( -0.000000000000000000, -0.000000000000000000, -1.000000000000000000 ) ) ;
#68735 = DIRECTION ( 'NONE',  ( -0.000000000000000000, -0.000000000000000000, -1.000000000000000000 ) ) ;
#68736 = CARTESIAN_POINT ( 'NONE',  ( -20.63749999999999929, 0.000000000000000000, 0.000000000000000000 ) ) ;
#68737 = EDGE_CURVE ( 'NONE', #54877, #17632, #36429, .T. ) ;
#68738 = CARTESIAN_POINT ( 'NONE',  ( -156.0300823189602397, 69.91528270335483342, -46.05349014652669126 ) ) ;
#68739 = EDGE_LOOP ( 'NONE', ( #20681, #58099, #9514, #59150 ) ) ;
#68740 =( REPRESENTATION_RELATIONSHIP ('NONE','NONE', #40274, #64096 ) REPRESENTATION_RELATIONSHIP_WITH_TRANSFORMATION ( #44917 )SHAPE_REPRESENTATION_RELATIONSHIP( ) );
#68741 = EDGE_LOOP ( 'NONE', ( #810, #21523, #27785, #57998, #58085, #59737, #26700 ) ) ;
#68742 = DIRECTION ( 'NONE',  ( -0.000000000000000000, -0.000000000000000000, -1.000000000000000000 ) ) ;
#68743 = CARTESIAN_POINT ( 'NONE',  ( -84.53753601793928851, 25.73343139558517478, -47.30913981394891721 ) ) ;
#68744 = CARTESIAN_POINT ( 'NONE',  ( 103.0087611945305923, 25.67668113601890667, 92.80995230241677518 ) ) ;
#68745 = CARTESIAN_POINT ( 'NONE',  ( -155.2836587093739240, 70.59655508952972980, 6.585747873642095129 ) ) ;
#68746 = AXIS2_PLACEMENT_3D ( 'NONE', #21822, #1421, #11267 ) ;
#68747 = CARTESIAN_POINT ( 'NONE',  ( -23.14886993799584047, 9.760512885996790899, 3.061616997868437868E-16 ) ) ;
#68748 = DIRECTION ( 'NONE',  ( 0.000000000000000000, 0.000000000000000000, 1.000000000000000000 ) ) ;
#68749 = CARTESIAN_POINT ( 'NONE',  ( -153.2251259997642023, 68.74288695996825993, 85.39013094563341610 ) ) ;
#68750 = ORIENTED_EDGE ( 'NONE', *, *, #1909, .F. ) ;
#68751 = ADVANCED_FACE ( 'NONE', ( #61925 ), #39443, .F. ) ;
#68752 = ORIENTED_EDGE ( 'NONE', *, *, #36534, .T. ) ;
#68753 = EDGE_CURVE ( 'NONE', #61903, #34081, #50691, .T. ) ;
#68754 = ORIENTED_EDGE ( 'NONE', *, *, #14057, .F. ) ;
#68755 = VECTOR ( 'NONE', #51318, 1000.000000000000000 ) ;
#68756 = VECTOR ( 'NONE', #30918, 1000.000000000000000 ) ;
#68757 = ADVANCED_FACE ( 'NONE', ( #35559 ), #45412, .F. ) ;
#68758 = CARTESIAN_POINT ( 'NONE',  ( 175.0129209324024089, 72.68029375226022637, -93.00527503831655451 ) ) ;
#68759 = CARTESIAN_POINT ( 'NONE',  ( 105.0002060648038480, -21.99995316709852489, 0.3345430166890353552 ) ) ;
#68760 = EDGE_CURVE ( 'NONE', #31066, #27441, #68523, .T. ) ;
#68761 = VECTOR ( 'NONE', #14999, 1000.000000000000000 ) ;
#68762 = LINE ( 'NONE', #51570, #45021 ) ;
#68763 = CARTESIAN_POINT ( 'NONE',  ( -60.00000000000000000, 0.000000000000000000, -5.000000000000000000 ) ) ;
#68764 = CARTESIAN_POINT ( 'NONE',  ( 32.14349651933086705, 7.576119504381656711, 62.30723258595453729 ) ) ;
#68765 = CARTESIAN_POINT ( 'NONE',  ( 12.69192874957004769, 6.421326776602847453, -23.00982468687297100 ) ) ;
#68766 = CARTESIAN_POINT ( 'NONE',  ( 21.43750346857337874, 7.754771113113080538, 15.62753494944939625 ) ) ;
#68767 = CARTESIAN_POINT ( 'NONE',  ( 185.5415406465189960, 83.23025870924408309, 57.60304917807435743 ) ) ;
#68768 = CARTESIAN_POINT ( 'NONE',  ( -118.6157340058430236, 41.88485941274770141, 13.10580239523996049 ) ) ;
#68769 = PLANE ( 'NONE',  #24143 ) ;
#68770 = LINE ( 'NONE', #20585, #60001 ) ;
#68771 = CARTESIAN_POINT ( 'NONE',  ( 21.74799039132243905, 7.772294950329606600, -11.59454531415493861 ) ) ;
#68772 = CARTESIAN_POINT ( 'NONE',  ( 199.7255144154429161, 99.76581417577203581, 57.91832127983512635 ) ) ;
#68773 = VERTEX_POINT ( 'NONE', #34873 ) ;
#68774 = CARTESIAN_POINT ( 'NONE',  ( 188.5843222076478867, 86.53342480589847696, 10.26064979393518684 ) ) ;
#68775 = SHAPE_DEFINITION_REPRESENTATION ( #56956, #36174 ) ;
#68776 = CARTESIAN_POINT ( 'NONE',  ( 178.4027079424739384, 75.93756746109792743, 43.81623254374778753 ) ) ;
#68777 = DIRECTION ( 'NONE',  ( 0.000000000000000000, 0.000000000000000000, 1.000000000000000000 ) ) ;
#68778 = ADVANCED_FACE ( 'NONE', ( #49992 ), #18332, .F. ) ;
#68779 = CARTESIAN_POINT ( 'NONE',  ( -102.7494334820056707, 34.14986869751098908, -35.01457726497590528 ) ) ;
#68780 = EDGE_CURVE ( 'NONE', #18030, #18889, #8133, .T. ) ;
#68781 = CARTESIAN_POINT ( 'NONE',  ( 188.5651904823862708, 88.01586411309102687, -43.11409047739251577 ) ) ;
#68782 = ORIENTED_EDGE ( 'NONE', *, *, #5904, .F. ) ;
#68783 = VERTEX_POINT ( 'NONE', #66206 ) ;
#68784 = EDGE_CURVE ( 'NONE', #2078, #35908, #51398, .T. ) ;
#68785 = CARTESIAN_POINT ( 'NONE',  ( -28.35330809568271704, 9.105138953156455273, -9.132531776435367732 ) ) ;
#68786 = CARTESIAN_POINT ( 'NONE',  ( 173.7926097690033771, 71.53801684183484610, 92.29874427387952096 ) ) ;
#68787 = VERTEX_POINT ( 'NONE', #7447 ) ;
#68788 = DIRECTION ( 'NONE',  ( 1.000000000000000000, 0.000000000000000000, 0.000000000000000000 ) ) ;
#68789 = ORIENTED_EDGE ( 'NONE', *, *, #20192, .F. ) ;
#68790 = CARTESIAN_POINT ( 'NONE',  ( 117.0069443446175370, 33.26475960880692639, 67.20599609474545844 ) ) ;
#68791 = DIRECTION ( 'NONE',  ( 0.000000000000000000, 1.000000000000000000, 0.000000000000000000 ) ) ;
#68792 = LINE ( 'NONE', #36113, #45462 ) ;
#68793 = AXIS2_PLACEMENT_3D ( 'NONE', #19062, #61285, #29275 ) ;
#68794 = DIRECTION ( 'NONE',  ( -1.000000000000000000, 0.000000000000000000, 0.000000000000000000 ) ) ;
#68795 = FACE_OUTER_BOUND ( 'NONE', #36246, .T. ) ;
#68796 = VECTOR ( 'NONE', #31302, 1000.000000000000114 ) ;
#68798 = VERTEX_POINT ( 'NONE', #45768 ) ;
#68797 = LINE ( 'NONE', #52960, #25242 ) ;
#68799 = CARTESIAN_POINT ( 'NONE',  ( 64.52696037203369883, -10.43950074664763683, 41.38025477438755928 ) ) ;
#68800 = VERTEX_POINT ( 'NONE', #46101 ) ;
#68801 = CIRCLE ( 'NONE', #46367, 10.00000000000000000 ) ;
#68802 = VERTEX_POINT ( 'NONE', #35208 ) ;
#68803 = CARTESIAN_POINT ( 'NONE',  ( -120.4816138481824908, 43.03185659245512085, -20.78403245137389987 ) ) ;
#68804 = CARTESIAN_POINT ( 'NONE',  ( 63.74253542338254164, 39.54050679744534591, 170.0000000000000000 ) ) ;
#68805 = CARTESIAN_POINT ( 'NONE',  ( -180.3153482337535820, 95.51031295027645740, -13.22612429021853409 ) ) ;
#68807 = ORIENTED_EDGE ( 'NONE', *, *, #5489, .F. ) ;
#68806 = CARTESIAN_POINT ( 'NONE',  ( 22.07550062443499428, -11.73338281062043364, 0.000000000000000000 ) ) ;
#68808 = CARTESIAN_POINT ( 'NONE',  ( -109.7839076876610562, 37.90938796091269580, 91.47912654843170799 ) ) ;
#68809 = VECTOR ( 'NONE', #43466, 1000.000000000000000 ) ;
#68810 = LINE ( 'NONE', #48628, #59798 ) ;
#68811 = ORIENTED_EDGE ( 'NONE', *, *, #65655, .T. ) ;
#68812 = CARTESIAN_POINT ( 'NONE',  ( -59.94781924509481286, 16.04872117907065743, -10.18417756321730039 ) ) ;
#68813 = CARTESIAN_POINT ( 'NONE',  ( -133.3944793432480367, 52.87251459353621641, -69.00333076711490321 ) ) ;
#68814 = EDGE_CURVE ( 'NONE', #56977, #44262, #28902, .T. ) ;
#68815 = CYLINDRICAL_SURFACE ( 'NONE', #34836, 74.99999999999998579 ) ;
#68816 = DIRECTION ( 'NONE',  ( -0.8345732537213078617, 0.5508969814520945363, 0.000000000000000000 ) ) ;
#68817 = CARTESIAN_POINT ( 'NONE',  ( -96.02415295709707266, 29.71480036090586196, -73.50342397880682199 ) ) ;
#68818 = ORIENTED_EDGE ( 'NONE', *, *, #26883, .F. ) ;
#68819 = ORIENTED_EDGE ( 'NONE', *, *, #53901, .F. ) ;
#68820 = CARTESIAN_POINT ( 'NONE',  ( 185.5572090022886016, 83.24697331286186852, -64.53146504295692409 ) ) ;
#68821 = CARTESIAN_POINT ( 'NONE',  ( -166.9982296371934467, 80.56207291422407479, -46.55132158310039614 ) ) ;
#68822 = CARTESIAN_POINT ( 'NONE',  ( 0.000000000000000000, 26.99999999999999645, 12.00000000000000000 ) ) ;
#68823 = CARTESIAN_POINT ( 'NONE',  ( 106.6181401479172308, 28.34160787025143335, -63.69676998527926060 ) ) ;
#68824 = CARTESIAN_POINT ( 'NONE',  ( -77.71490760329791669, 23.03637365463981723, 30.46362590998626985 ) ) ;
#68825 = CARTESIAN_POINT ( 'NONE',  ( 79.38020582286196714, 17.07365509555548755, 35.22343465671548302 ) ) ;
#68826 = CARTESIAN_POINT ( 'NONE',  ( 63.50537371531939357, 13.81987663608981798, -35.72069083216972274 ) ) ;
#68827 = LINE ( 'NONE', #35807, #12643 ) ;
#68828 = CARTESIAN_POINT ( 'NONE',  ( -84.49322488516129681, 0.000000000000000000, 43.58025477438756212 ) ) ;
#68829 = EDGE_CURVE ( 'NONE', #48794, #5387, #39794, .T. ) ;
#68830 = ORIENTED_EDGE ( 'NONE', *, *, #43108, .T. ) ;
#68831 = CARTESIAN_POINT ( 'NONE',  ( -105.8879439778144871, 34.65133284149108306, -22.26253636860239027 ) ) ;
#68832 = ORIENTED_EDGE ( 'NONE', *, *, #68898, .T. ) ;
#68833 = CARTESIAN_POINT ( 'NONE',  ( -35.99019277275120743, 10.38248800679342310, 16.85316403250221740 ) ) ;
#68834 = CARTESIAN_POINT ( 'NONE',  ( 79.91920957766411959, 18.29292522273511068, 67.44459320285845649 ) ) ;
#68835 = EDGE_CURVE ( 'NONE', #39142, #40691, #64395, .T. ) ;
#68836 = CARTESIAN_POINT ( 'NONE',  ( 19.62566184736102315, -15.48655536434847413, 0.000000000000000000 ) ) ;
#68837 = DIRECTION ( 'NONE',  ( -1.000000000000000000, 0.000000000000000000, 0.000000000000000000 ) ) ;
#68838 = DIRECTION ( 'NONE',  ( 0.000000000000000000, 0.000000000000000000, 1.000000000000000000 ) ) ;
#68839 = EDGE_CURVE ( 'NONE', #37709, #38638, #41525, .T. ) ;
#68840 = CARTESIAN_POINT ( 'NONE',  ( 0.000000000000000000, 0.000000000000000000, 0.000000000000000000 ) ) ;
#68841 = CARTESIAN_POINT ( 'NONE',  ( 34.83825437341838693, 7.859462995505729133, -75.93605119989038599 ) ) ;
#68842 = CARTESIAN_POINT ( 'NONE',  ( -98.68609963468202295, 32.11186931716879656, -62.75914624374382100 ) ) ;
#68843 = CIRCLE ( 'NONE', #19445, 65.36598343705435354 ) ;
#68844 = CARTESIAN_POINT ( 'NONE',  ( -36.00304714721387711, 11.40794940913596456, -10.00091909768606335 ) ) ;
#68845 = ORIENTED_EDGE ( 'NONE', *, *, #3843, .T. ) ;
#68846 = VECTOR ( 'NONE', #11124, 1000.000000000000114 ) ;
#68847 = DIRECTION ( 'NONE',  ( 1.000000000000000000, 0.000000000000000000, -0.000000000000000000 ) ) ;
#68848 = ORIENTED_EDGE ( 'NONE', *, *, #23983, .F. ) ;
#68849 = CARTESIAN_POINT ( 'NONE',  ( 59.30258796551119360, 12.87111270082601600, 57.62249339133282433 ) ) ;
#68850 = CARTESIAN_POINT ( 'NONE',  ( -25.98312968277007329, 8.759224980175261521, 5.719980934363178449 ) ) ;
#68851 = DIRECTION ( 'NONE',  ( 0.000000000000000000, 0.000000000000000000, -1.000000000000000000 ) ) ;
#68852 = CARTESIAN_POINT ( 'NONE',  ( 44.99999999999995737, -22.99999999999998579, 0.000000000000000000 ) ) ;
#68853 = CARTESIAN_POINT ( 'NONE',  ( 0.000000000000000000, 0.000000000000000000, 40.00000000000003553 ) ) ;
#68854 = AXIS2_PLACEMENT_3D ( 'NONE', #18953, #40399, #61845 ) ;
#68855 = CARTESIAN_POINT ( 'NONE',  ( 152.1381498073141074, 54.87048121475569928, -48.92046709163152229 ) ) ;
#68856 = VERTEX_POINT ( 'NONE', #62977 ) ;
#68858 = AXIS2_PLACEMENT_3D ( 'NONE', #18160, #55081, #33994 ) ;
#68857 = DIRECTION ( 'NONE',  ( 9.939659282862092686E-15, -1.000000000000000000, -4.041333507787477774E-15 ) ) ;
#68859 = CARTESIAN_POINT ( 'NONE',  ( -154.8006992380339000, 70.15733562427990933, 70.40004192881569622 ) ) ;
#68860 = CARTESIAN_POINT ( 'NONE',  ( 173.6700117628886630, 72.79957362875114768, -15.71003057700986716 ) ) ;
#68861 = CARTESIAN_POINT ( 'NONE',  ( 15.55634918610406103, 15.55634918610400241, 85.00100000000000477 ) ) ;
#68862 = CARTESIAN_POINT ( 'NONE',  ( -128.9843070188472893, 49.78011598923034597, -49.26255782700048513 ) ) ;
#68863 = ORIENTED_EDGE ( 'NONE', *, *, #52250, .T. ) ;
#68864 = CARTESIAN_POINT ( 'NONE',  ( -20.16272189348855903, 400.0000000000064801, 321.0502958579853043 ) ) ;
#68865 = CARTESIAN_POINT ( 'NONE',  ( -6.851003965218993130, 6.829052369041586523, -23.52622361473696699 ) ) ;
#68866 = EDGE_CURVE ( 'NONE', #51645, #39831, #62642, .T. ) ;
#68867 = CARTESIAN_POINT ( 'NONE',  ( 198.7123879174244223, 100.1053816708572555, -21.50880716110014035 ) ) ;
#68868 = CARTESIAN_POINT ( 'NONE',  ( -151.7300473889874581, 66.08683396307566227, 84.72635355681168789 ) ) ;
#68869 = CARTESIAN_POINT ( 'NONE',  ( 136.1310312718401860, 42.81430973242785853, 44.17212115549305906 ) ) ;
#68870 = ORIENTED_EDGE ( 'NONE', *, *, #59283, .T. ) ;
#68871 = CARTESIAN_POINT ( 'NONE',  ( 197.3685896092616190, 96.80423329231987850, 35.08436879187444646 ) ) ;
#68872 = CARTESIAN_POINT ( 'NONE',  ( 69.77839676787858991, 27.52340539440040956, 170.0000000000000000 ) ) ;
#68873 = CARTESIAN_POINT ( 'NONE',  ( 184.3966782763551464, 83.48172388049827930, 30.06520294631881285 ) ) ;
#68874 = CARTESIAN_POINT ( 'NONE',  ( 16.78635691501517613, 6.000000000000000000, -41.68900338898716740 ) ) ;
#68875 = CARTESIAN_POINT ( 'NONE',  ( -102.2801239173131194, 33.91021738430207932, 45.51907450641513009 ) ) ;
#68876 = VERTEX_POINT ( 'NONE', #14784 ) ;
#68877 = B_SPLINE_CURVE_WITH_KNOTS ( 'NONE', 3,
 ( #2669, #68088, #19888, #9328, #30789, #52234 ),
 .UNSPECIFIED., .F., .F.,
 ( 4, 2, 4 ),
 ( 0.01291313371729459550, 0.01525081363757311605, 0.01758849355785163660 ),
 .UNSPECIFIED. ) ;
#68878 = DIRECTION ( 'NONE',  ( 0.000000000000000000, 0.000000000000000000, 1.000000000000000000 ) ) ;
#68879 = ORIENTED_EDGE ( 'NONE', *, *, #22647, .F. ) ;
#68880 = CARTESIAN_POINT ( 'NONE',  ( -71.97434903038468690, 19.88430675376528711, -19.19362628757813027 ) ) ;
#68881 = PLANE ( 'NONE',  #65717 ) ;
#68882 = VECTOR ( 'NONE', #14203, 1000.000000000000000 ) ;
#68883 = CARTESIAN_POINT ( 'NONE',  ( -55.54058841405665703, 14.81234591756537888, 45.31732777293116499 ) ) ;
#68885 = ORIENTED_EDGE ( 'NONE', *, *, #4289, .F. ) ;
#68884 = CARTESIAN_POINT ( 'NONE',  ( 44.01696072966022655, -47.84694004974146253, 170.0000000000000000 ) ) ;
#68886 = CARTESIAN_POINT ( 'NONE',  ( -180.6213815675304772, 95.88446356933845038, 38.01213868508001781 ) ) ;
#68887 = DIRECTION ( 'NONE',  ( 0.000000000000000000, 0.000000000000000000, 1.000000000000000000 ) ) ;
#68888 = LINE ( 'NONE', #14747, #37309 ) ;
#68889 = VECTOR ( 'NONE', #18169, 1000.000000000000114 ) ;
#68890 = ORIENTED_EDGE ( 'NONE', *, *, #3440, .T. ) ;
#68891 = CARTESIAN_POINT ( 'NONE',  ( -173.1211646369891355, -170.0000000000000000, -95.90105834567735599 ) ) ;
#68893 = EDGE_CURVE ( 'NONE', #41788, #66440, #7370, .T. ) ;
#68892 = AXIS2_PLACEMENT_3D ( 'NONE', #50344, #61915, #66194 ) ;
#68894 = EDGE_CURVE ( 'NONE', #29891, #59106, #36597, .T. ) ;
#68895 = VECTOR ( 'NONE', #51242, 1000.000000000000000 ) ;
#68896 = CARTESIAN_POINT ( 'NONE',  ( 86.62931800182293784, 20.48449268398422518, -23.97701360844805407 ) ) ;
#68897 = CARTESIAN_POINT ( 'NONE',  ( 141.2366329129481244, 46.06278879703609874, 62.49230329047843213 ) ) ;
#68898 = EDGE_CURVE ( 'NONE', #38050, #38689, #20704, .T. ) ;
#68899 = CARTESIAN_POINT ( 'NONE',  ( -171.4814970982680222, 85.32124710276291069, 45.65206851958718914 ) ) ;
#68900 = AXIS2_PLACEMENT_3D ( 'NONE', #91, #43687, #21892 ) ;
#68901 = CARTESIAN_POINT ( 'NONE',  ( 153.2282895792479565, 54.42637815496158993, 57.56435675519129802 ) ) ;
#68902 = CARTESIAN_POINT ( 'NONE',  ( -31.11269837220806878, 5.594483210025202879E-14, 2.000000000000001776 ) ) ;
#68903 = ORIENTED_EDGE ( 'NONE', *, *, #10397, .F. ) ;
#68904 = CARTESIAN_POINT ( 'NONE',  ( 46.80475532923159676, 10.50744084852537163, 9.340717336282994054 ) ) ;
#68905 = VERTEX_POINT ( 'NONE', #63673 ) ;
#68906 = VECTOR ( 'NONE', #59318, 1000.000000000000000 ) ;
#68907 = CARTESIAN_POINT ( 'NONE',  ( 151.1827182658834090, 54.16800928478855326, -20.89999102867709269 ) ) ;
#68908 = CARTESIAN_POINT ( 'NONE',  ( -59.24627258934994245, 15.84537569346437458, 85.25633480741510084 ) ) ;
#68909 = CARTESIAN_POINT ( 'NONE',  ( 103.1695711638930817, 26.83837309506527546, 34.56746450366944146 ) ) ;
#68910 = DIRECTION ( 'NONE',  ( 0.000000000000000000, 0.000000000000000000, 1.000000000000000000 ) ) ;
#68911 = CARTESIAN_POINT ( 'NONE',  ( -9.964117946888970678, -64.24592483216726180, 3.061616997868437868E-16 ) ) ;
#68912 = CARTESIAN_POINT ( 'NONE',  ( 188.5838389098763344, 88.03667982118683710, 10.27324879826098503 ) ) ;
#68913 = FACE_OUTER_BOUND ( 'NONE', #39653, .T. ) ;
#68914 = DIRECTION ( 'NONE',  ( 0.000000000000000000, 0.000000000000000000, 1.000000000000000000 ) ) ;
#68916 = ORIENTED_EDGE ( 'NONE', *, *, #30667, .F. ) ;
#68915 = B_SPLINE_CURVE_WITH_KNOTS ( 'NONE', 3,
 ( #55313, #65898, #11704, #38448, #7132, #18041, #65537, #43703, #2215, #17330, #6782, #44056, #49678, #33871, #12066, #22969, #44415, #54965, #23665, #820, #28950, #33178, #38805, #39493, #44773, #54611, #59885, #60598, #23329, #66250, #6442, #28228, #60248, #1873, #22269, #34223, #28593, #50046, #55667, #60944, #65181, #12763, #16975, #49329 ),
 .UNSPECIFIED., .F., .F.,
 ( 4, 2, 2, 2, 2, 2, 2, 2, 2, 2, 2, 2, 2, 2, 2, 2, 2, 2, 2, 2, 2, 4 ),
 ( 1.398578778534940505E-17, 0.001487235713946735011, 0.002230853570920115960, 0.002974471427893496910, 0.004461707141840256206, 0.005948942855787015503, 0.007436178569733774800, 0.008179796426707155316, 0.008923414283680533229, 0.01041064999762730467, 0.01189788571157407611, 0.01264150356854745749, 0.01338512142552083888, 0.01487235713946760164, 0.01561597499644099343, 0.01635959285341438349, 0.01784682856736116360, 0.01933406428130794372, 0.02007768213828133724, 0.02082129999525472730, 0.02230853570920151435, 0.02379577142314830140 ),
 .UNSPECIFIED. ) ;
#68917 = CARTESIAN_POINT ( 'NONE',  ( 112.3013380801408658, 395.0000000000065938, -123.9497041420121235 ) ) ;
#68918 = ORIENTED_EDGE ( 'NONE', *, *, #68701, .F. ) ;
#68919 = CARTESIAN_POINT ( 'NONE',  ( -75.43271753227890031, 22.18711452892411273, 71.54694186117023946 ) ) ;
#68920 = EDGE_CURVE ( 'NONE', #22014, #56285, #68929, .T. ) ;
#68921 = CARTESIAN_POINT ( 'NONE',  ( 0.3157512944565082358, -3.097794232830076044, 8.000000000000000000 ) ) ;
#68922 = CARTESIAN_POINT ( 'NONE',  ( 59.72897338775215559, 11.93428797217974591, -76.81118384515825426 ) ) ;
#68923 = EDGE_CURVE ( 'NONE', #56044, #13483, #58379, .T. ) ;
#68924 = DIRECTION ( 'NONE',  ( 0.000000000000000000, 0.000000000000000000, 1.000000000000000000 ) ) ;
#68925 = CARTESIAN_POINT ( 'NONE',  ( 6.564829507346455983, -24.24955267099640110, 0.000000000000000000 ) ) ;
#68926 = CARTESIAN_POINT ( 'NONE',  ( 20.74185656603722450, 7.717159106492252896, 31.86164482231723127 ) ) ;
#68927 = CARTESIAN_POINT ( 'NONE',  ( 158.3636111008086687, 59.62671916656143623, -62.96873488960133614 ) ) ;
#68928 = ORIENTED_EDGE ( 'NONE', *, *, #49402, .T. ) ;
#68929 = LINE ( 'NONE', #20753, #13982 ) ;
#68930 = PLANE ( 'NONE',  #46469 ) ;
#68931 = ORIENTED_EDGE ( 'NONE', *, *, #58076, .F. ) ;
#68932 = VERTEX_POINT ( 'NONE', #686 ) ;
#68933 = CARTESIAN_POINT ( 'NONE',  ( -155.1302201283146189, 69.09929365814133462, 43.19023084304400584 ) ) ;
#68934 = CARTESIAN_POINT ( 'NONE',  ( 55.56474667084417263, 11.06706367715628581, -42.22808952694573037 ) ) ;
#68935 = LINE ( 'NONE', #49108, #14324 ) ;
#68936 = DIRECTION ( 'NONE',  ( -1.000000000000000000, 9.109522253334613014E-16, 0.000000000000000000 ) ) ;
#68937 = VECTOR ( 'NONE', #18705, 1000.000000000000000 ) ;
#68938 = CARTESIAN_POINT ( 'NONE',  ( -145.3279998500303520, 60.71393190715791377, 5.144276485782331321 ) ) ;
#68939 = VERTEX_POINT ( 'NONE', #64347 ) ;
#68940 = CARTESIAN_POINT ( 'NONE',  ( -132.4896623150434039, 52.22616402022728721, 41.69918907009083142 ) ) ;
#68941 = ORIENTED_EDGE ( 'NONE', *, *, #18062, .F. ) ;
#68942 = CARTESIAN_POINT ( 'NONE',  ( 204.6977192012829789, 106.3443248447423599, 2.363170148305747009 ) ) ;
#68943 = LINE ( 'NONE', #16175, #36077 ) ;
#68944 = VECTOR ( 'NONE', #61606, 1000.000000000000000 ) ;
#68945 = CARTESIAN_POINT ( 'NONE',  ( 210.1954643503416094, 114.1986276268024056, 41.81508267376618448 ) ) ;
#68946 = CARTESIAN_POINT ( 'NONE',  ( -7.825402957745085430, 7.899365992529246761, 71.96013162991091860 ) ) ;
#68947 = VECTOR ( 'NONE', #63413, 1000.000000000000000 ) ;
#68948 = CIRCLE ( 'NONE', #12787, 25.12245591505646303 ) ;
#68949 = AXIS2_PLACEMENT_3D ( 'NONE', #24616, #57655, #66844 ) ;
#68950 = EDGE_LOOP ( 'NONE', ( #41761, #3927, #18584 ) ) ;
#68951 = EDGE_LOOP ( 'NONE', ( #27703, #16417, #26920, #25895, #56302, #29163, #28197, #39959, #59204, #55955, #491, #57450 ) ) ;
#68952 = CARTESIAN_POINT ( 'NONE',  ( 110.6590877922806015, -21.43203852822544064, -4.967093445758837156 ) ) ;
#68953 = CARTESIAN_POINT ( 'NONE',  ( 0.000000000000000000, 0.000000000000000000, 0.000000000000000000 ) ) ;
#68954 = AXIS2_PLACEMENT_3D ( 'NONE', #16511, #6652, #54475 ) ;
#68955 = CARTESIAN_POINT ( 'NONE',  ( 36.30999198706539488, 9.040534725358943646, -63.12703590951987564 ) ) ;
#68956 = PLANE ( 'NONE',  #46758 ) ;
#68957 = PLANE ( 'NONE',  #9426 ) ;
#68958 = CARTESIAN_POINT ( 'NONE',  ( 12.60448962010195473, 7.425467749510118232, 84.38144641662934475 ) ) ;
#68959 = ORIENTED_EDGE ( 'NONE', *, *, #28369, .T. ) ;
#68960 = DIRECTION ( 'NONE',  ( -0.000000000000000000, 1.000000000000000000, -0.000000000000000000 ) ) ;
#68961 = DIRECTION ( 'NONE',  ( 0.000000000000000000, 0.000000000000000000, -1.000000000000000000 ) ) ;
#68962 = ORIENTED_EDGE ( 'NONE', *, *, #13379, .F. ) ;
#68963 = CARTESIAN_POINT ( 'NONE',  ( -86.06489347855098515, 25.27905598459106784, 9.817369700168111279 ) ) ;
#68964 = EDGE_LOOP ( 'NONE', ( #34955, #40727, #49500, #38039 ) ) ;
#68965 = VERTEX_POINT ( 'NONE', #37968 ) ;
#68966 = EDGE_LOOP ( 'NONE', ( #65710, #19385, #22686, #38251 ) ) ;
#68967 = CARTESIAN_POINT ( 'NONE',  ( -123.0348077379026819, 45.83489305753315790, 18.21289688529726192 ) ) ;
#68968 = CARTESIAN_POINT ( 'NONE',  ( 185.0000000000000000, 0.000000000000000000, 2.499999999999999556 ) ) ;
#68969 = ADVANCED_FACE ( 'NONE', ( #48840 ), #34185, .T. ) ;
#68970 = CARTESIAN_POINT ( 'NONE',  ( 126.9201538765324671, 37.39093565120717244, 66.71864824504474711 ) ) ;
#68971 = VERTEX_POINT ( 'NONE', #17191 ) ;
#68972 = ADVANCED_FACE ( 'NONE', ( #16160 ), #11223, .F. ) ;
#68973 = CARTESIAN_POINT ( 'NONE',  ( -38.80050246754539245, 10.91612181589391284, 92.87695660739120740 ) ) ;
#68974 = CARTESIAN_POINT ( 'NONE',  ( 152.1327777395850376, 53.61712543276775733, 42.18410997051201861 ) ) ;
#68975 = VECTOR ( 'NONE', #12334, 1000.000000000000000 ) ;
#68976 = EDGE_CURVE ( 'NONE', #48814, #14060, #4980, .T. ) ;
#68977 = LINE ( 'NONE', #42602, #46019 ) ;
#68978 = CARTESIAN_POINT ( 'NONE',  ( 107.0477776024379182, 27.43148174916615645, -50.21201981945658588 ) ) ;
#68979 = CARTESIAN_POINT ( 'NONE',  ( 135.6647932137617545, 43.70902528961477884, -63.07493546931258521 ) ) ;
#68980 = CARTESIAN_POINT ( 'NONE',  ( -10.27459169636330749, -50.63337651310006038, 26.66469066592268788 ) ) ;
#68981 = ORIENTED_EDGE ( 'NONE', *, *, #45566, .F. ) ;
#68982 = VECTOR ( 'NONE', #19639, 1000.000000000000000 ) ;
#68983 = EDGE_CURVE ( 'NONE', #63892, #32531, #11562, .T. ) ;
#68984 = CARTESIAN_POINT ( 'NONE',  ( 74.39890044415633952, 7.951074708187157114, 170.0000000000000000 ) ) ;
#68985 = VECTOR ( 'NONE', #17387, 1000.000000000000000 ) ;
#68986 = CARTESIAN_POINT ( 'NONE',  ( -4.000000000000013323, 6.928203230275504332, -9.500000000000000000 ) ) ;
#68987 = DIRECTION ( 'NONE',  ( 0.000000000000000000, 0.000000000000000000, -1.000000000000000000 ) ) ;
#68988 = FACE_OUTER_BOUND ( 'NONE', #25643, .T. ) ;
#68989 = DIRECTION ( 'NONE',  ( 1.000000000000000000, 0.000000000000000000, 0.000000000000000000 ) ) ;
#68990 = CARTESIAN_POINT ( 'NONE',  ( 136.8102763416569303, 43.23640610422827280, -90.30779350402794137 ) ) ;
#68991 = CARTESIAN_POINT ( 'NONE',  ( -156.6692143066620417, 70.50016761530885390, 9.132081936590415339 ) ) ;
#68992 = DIRECTION ( 'NONE',  ( -0.8118923937861950435, -0.5838071093367415143, 0.000000000000000000 ) ) ;
#68993 = AXIS2_PLACEMENT_3D ( 'NONE', #99, #21555, #64473 ) ;
#68994 = CARTESIAN_POINT ( 'NONE',  ( 65.62848231372478836, 13.29388722724789140, 3.434105544353177830 ) ) ;
#68995 = CARTESIAN_POINT ( 'NONE',  ( 164.7167608259061922, 63.51199216609074227, 8.111511345676536422 ) ) ;
#68996 = CARTESIAN_POINT ( 'NONE',  ( -7.825402957745087207, -170.0000000000000000, -35.41807073194381417 ) ) ;
#68997 = ORIENTED_EDGE ( 'NONE', *, *, #48734, .F. ) ;
#68999 = AXIS2_PLACEMENT_3D ( 'NONE', #47942, #69413, #68050 ) ;
#68998 = CONTEXT_DEPENDENT_SHAPE_REPRESENTATION ( #8985, #46264 ) ;
#69000 = CARTESIAN_POINT ( 'NONE',  ( -60.66790124542881557, 17.30811205907484762, 86.52422518474469371 ) ) ;
#69001 = ORIENTED_EDGE ( 'NONE', *, *, #14306, .T. ) ;
#69002 = LINE ( 'NONE', #58121, #5971 ) ;
#69003 = ORIENTED_EDGE ( 'NONE', *, *, #30480, .F. ) ;
#69004 = EDGE_CURVE ( 'NONE', #68787, #67311, #27402, .T. ) ;
#69005 = CARTESIAN_POINT ( 'NONE',  ( 23.24047374271773947, 7.861801299833796719, -68.88436191109398976 ) ) ;
#69006 = CARTESIAN_POINT ( 'NONE',  ( 116.4569059613810680, 32.98885890446639735, 94.99999999999866418 ) ) ;
#69007 = CARTESIAN_POINT ( 'NONE',  ( 14.07802376132189970, -39.28261699430611742, 13.79046412305352121 ) ) ;
#69008 = PLANE ( 'NONE',  #756 ) ;
#69009 = CARTESIAN_POINT ( 'NONE',  ( 136.1037846510192821, 43.98155406734451844, -36.35297218151394105 ) ) ;
#69010 = CARTESIAN_POINT ( 'NONE',  ( 210.9029460956748210, 117.0873171135434774, -93.27756825301547394 ) ) ;
#69011 = CARTESIAN_POINT ( 'NONE',  ( -2.113472939309121834, -74.92159864268212743, 41.38025477438755928 ) ) ;
#69012 = CARTESIAN_POINT ( 'NONE',  ( 18.07314801315404296, -17.44990292519077002, 0.000000000000000000 ) ) ;
#69013 = CARTESIAN_POINT ( 'NONE',  ( -15.24379698450855436, -38.84509498579587472, 13.79046412320005288 ) ) ;
#69014 = VERTEX_POINT ( 'NONE', #54474 ) ;
#69015 = ORIENTED_EDGE ( 'NONE', *, *, #60126, .F. ) ;
#69016 = DIRECTION ( 'NONE',  ( -1.000000000000000000, 0.000000000000000000, 0.000000000000000000 ) ) ;
#69017 = PLANE ( 'NONE',  #35266 ) ;
#69018 = LINE ( 'NONE', #42642, #12778 ) ;
#69019 = UNCERTAINTY_MEASURE_WITH_UNIT (LENGTH_MEASURE( 1.000000000000000082E-05 ), #8331, 'distance_accuracy_value', 'NONE');
#69020 = CARTESIAN_POINT ( 'NONE',  ( 66.35539324779723813, 14.50870466687347360, -90.19136351260330287 ) ) ;
#69021 = DIRECTION ( 'NONE',  ( 0.000000000000000000, 0.000000000000000000, -1.000000000000000000 ) ) ;
#69022 = CARTESIAN_POINT ( 'NONE',  ( 183.9887307715836755, 83.05100282186906213, -9.962353762427376580 ) ) ;
#69023 = CARTESIAN_POINT ( 'NONE',  ( 173.6710158776851074, 71.42507420636738402, -71.74642395748696799 ) ) ;
#69024 = CARTESIAN_POINT ( 'NONE',  ( 51.39999999999999858, 5.109226446042757607E-16, -4.171999999999999709 ) ) ;
#69025 = CARTESIAN_POINT ( 'NONE',  ( 87.11228333101212229, 19.58587579906928156, -8.977013608448025650 ) ) ;
#69026 = DIRECTION ( 'NONE',  ( -0.000000000000000000, 1.000000000000000000, -0.000000000000000000 ) ) ;
#69027 = CARTESIAN_POINT ( 'NONE',  ( -36.84489839129265931, -53.54860840895233309, 40.00000000000003553 ) ) ;
#69028 = VECTOR ( 'NONE', #64238, 1000.000000000000000 ) ;
#69029 = VERTEX_POINT ( 'NONE', #59411 ) ;
#69030 = CARTESIAN_POINT ( 'NONE',  ( -123.6619986853278164, 45.04188181212060016, -35.24979993431918501 ) ) ;
#69031 = DIRECTION ( 'NONE',  ( 0.000000000000000000, 0.000000000000000000, -1.000000000000000000 ) ) ;
#69032 = CARTESIAN_POINT ( 'NONE',  ( 15.55634918610400241, -15.55634918610406103, 2.000000000000001776 ) ) ;
#69033 = LINE ( 'NONE', #48603, #33214 ) ;
#69034 = CARTESIAN_POINT ( 'NONE',  ( 150.9184679586218749, 52.73111408630720831, 13.72417758240726293 ) ) ;
#69035 = CARTESIAN_POINT ( 'NONE',  ( -0.6787582498729884950, 7.537756487205481193, 89.00659339660666092 ) ) ;
#69036 = VECTOR ( 'NONE', #43678, 1000.000000000000000 ) ;
#69037 = ADVANCED_FACE ( 'NONE', ( #16510 ), #65759, .F. ) ;
#69038 = ORIENTED_EDGE ( 'NONE', *, *, #59771, .T. ) ;
#69039 = AXIS2_PLACEMENT_3D ( 'NONE', #21700, #241, #22402 ) ;
#69040 = DIRECTION ( 'NONE',  ( 0.3978782902816504485, 0.9174375763581197329, -0.001076851285082543923 ) ) ;
#69041 = VECTOR ( 'NONE', #57055, 1000.000000000000114 ) ;
#69042 = DIRECTION ( 'NONE',  ( 0.000000000000000000, 0.000000000000000000, 1.000000000000000000 ) ) ;
#69043 = ORIENTED_EDGE ( 'NONE', *, *, #3173, .F. ) ;
#69044 = ORIENTED_EDGE ( 'NONE', *, *, #60985, .F. ) ;
#69045 = CIRCLE ( 'NONE', #48849, 65.36598343705435354 ) ;
#69046 = CARTESIAN_POINT ( 'NONE',  ( 32.82008564316742394, 8.655929161490991675, 94.71415288098671681 ) ) ;
#69047 = CARTESIAN_POINT ( 'NONE',  ( -34.96012151086435438, -55.23134702900938464, 3.125053320693577513E-16 ) ) ;
#69048 = CARTESIAN_POINT ( 'NONE',  ( 136.4481901104277597, 44.19676283245976833, -90.17176020796104297 ) ) ;
#69049 = ORIENTED_EDGE ( 'NONE', *, *, #63212, .T. ) ;
#69050 = CARTESIAN_POINT ( 'NONE',  ( 0.000000000000000000, 0.000000000000000000, 378.0000000000000000 ) ) ;
#69051 = CARTESIAN_POINT ( 'NONE',  ( 57.30278335769613562, -48.40406511297320691, 43.58025477438756923 ) ) ;
#69052 = CARTESIAN_POINT ( 'NONE',  ( -1.096061481932294690, 7.553048580900439291, 7.450378931708088182 ) ) ;
#69053 = DIRECTION ( 'NONE',  ( -1.000000000000000000, 0.000000000000000000, 0.000000000000000000 ) ) ;
#69054 = CARTESIAN_POINT ( 'NONE',  ( -155.1204242627069902, 70.44799358128196332, -74.13786203925820928 ) ) ;
#69055 = DIRECTION ( 'NONE',  ( -0.5508969814521065267, 0.8345732537212999791, 0.000000000000000000 ) ) ;
#69056 = ORIENTED_EDGE ( 'NONE', *, *, #53261, .F. ) ;
#69057 = EDGE_CURVE ( 'NONE', #32425, #56977, #26726, .T. ) ;
#69058 = CARTESIAN_POINT ( 'NONE',  ( 103.5849290181278803, 27.01613348792538716, -20.03964120650123348 ) ) ;
#69059 = DIRECTION ( 'NONE',  ( 0.000000000000000000, 0.000000000000000000, 1.000000000000000000 ) ) ;
#69060 = CARTESIAN_POINT ( 'NONE',  ( 8.287863202055540057, 7.382585476140733682, 38.00295202663408389 ) ) ;
#69061 = DIRECTION ( 'NONE',  ( -1.000000000000000000, 0.000000000000000000, 0.000000000000000000 ) ) ;
#69062 = DIRECTION ( 'NONE',  ( -1.000000000000000000, 0.000000000000000000, 0.000000000000000000 ) ) ;
#69064 = ORIENTED_EDGE ( 'NONE', *, *, #55000, .F. ) ;
#69063 = DIRECTION ( 'NONE',  ( 0.000000000000000000, 0.000000000000000000, -1.000000000000000000 ) ) ;
#69065 = ORIENTED_EDGE ( 'NONE', *, *, #56144, .T. ) ;
#69066 = EDGE_CURVE ( 'NONE', #39519, #11058, #37516, .T. ) ;
#69067 = VERTEX_POINT ( 'NONE', #27753 ) ;
#69068 = DIRECTION ( 'NONE',  ( 1.000000000000000000, 0.000000000000000000, -0.000000000000000000 ) ) ;
#69069 = PLANE ( 'NONE',  #49101 ) ;
#69070 = CARTESIAN_POINT ( 'NONE',  ( 201.6034029841261770, 102.1956603101140644, -63.82502672031729674 ) ) ;
#69071 = CARTESIAN_POINT ( 'NONE',  ( -42.32797523529131922, 61.85511477251419166, 41.38025477438755928 ) ) ;
#69072 = CARTESIAN_POINT ( 'NONE',  ( -10.24974837193994759, 8.069704751038640822, -8.959403934766353217 ) ) ;
#69073 = CARTESIAN_POINT ( 'NONE',  ( 150.4544126017351005, 52.39556706174411005, -73.13320268118599188 ) ) ;
#69074 = CARTESIAN_POINT ( 'NONE',  ( -59.94154301275570873, 45.09516516490385385, 170.0000000000000000 ) ) ;
#69075 = AXIS2_PLACEMENT_3D ( 'NONE', #29367, #14572, #13542 ) ;
#69076 = LINE ( 'NONE', #68416, #60992 ) ;
#69077 = ORIENTED_EDGE ( 'NONE', *, *, #61875, .T. ) ;
#69079 = ORIENTED_EDGE ( 'NONE', *, *, #19048, .T. ) ;
#69078 = B_SPLINE_CURVE_WITH_KNOTS ( 'NONE', 3,
 ( #6701, #55943, #50655, #44326, #7050, #2475, #44690, #66509, #67208, #40449, #45026, #12680, #39072, #18301, #13042, #35172, #49594, #66170, #17960, #34503, #45731, #40109, #1426, #34842, #18656, #23930, #45380, #66858, #49953, #1789, #34146, #61565, #61894, #13381, #56277, #28147, #8094, #22883, #7415, #51012, #23246, #18997, #39409, #60857, #55581, #67540, #30251, #25326, #3508, #3861, #53669, #26606, #3174, #58599, #46069, #14062, #5146, #64585 ),
 .UNSPECIFIED., .F., .F.,
 ( 4, 2, 2, 2, 2, 2, 2, 2, 2, 2, 2, 2, 2, 2, 2, 2, 2, 2, 2, 2, 2, 2, 2, 2, 2, 2, 2, 2, 4 ),
 ( 0.000000000000000000, 0.002011591002436438277, 0.003017386503654637901, 0.004023182004872837524, 0.005028977506091036713, 0.006034773007309235902, 0.007040568508527436827, 0.008046364009745635149, 0.009052159510963836073, 0.01005795501218203526, 0.01206954601461843364, 0.01307534151583663630, 0.01408113701705483722, 0.01508693251827303815, 0.01609272801949123907, 0.01709852352070944173, 0.01810431902192764092, 0.02011591002436405665, 0.02112170552558225237, 0.02212750102680045156, 0.02313329652801864728, 0.02413909202923684647, 0.02514488753045504565, 0.02615068303167324484, 0.02715647853289144056, 0.02816227403410963975, 0.03017386503654603466, 0.03117966053776423385, 0.03218545603898243651 ),
 .UNSPECIFIED. ) ;
#69080 = ADVANCED_FACE ( 'NONE', ( #11929 ), #54830, .F. ) ;
#69081 = CARTESIAN_POINT ( 'NONE',  ( 70.51522979775972999, 15.57935281015687146, -15.87393280675930285 ) ) ;
#69082 = VECTOR ( 'NONE', #10347, 1000.000000000000000 ) ;
#69083 = CARTESIAN_POINT ( 'NONE',  ( -86.10360257264196093, 26.38663017581290404, -41.61327775500715376 ) ) ;
#69084 = CARTESIAN_POINT ( 'NONE',  ( 104.0890294065521289, 26.13727058016808513, 86.45864299650676799 ) ) ;
#69086 = EDGE_CURVE ( 'NONE', #48274, #31799, #6301, .T. ) ;
#69085 = CARTESIAN_POINT ( 'NONE',  ( -149.9475539515598541, 65.87716206616008208, 18.87627064943539423 ) ) ;
#69087 = EDGE_CURVE ( 'NONE', #18908, #4486, #5600, .T. ) ;
#69088 = AXIS2_PLACEMENT_3D ( 'NONE', #14277, #45587, #62462 ) ;
#69089 = VECTOR ( 'NONE', #18794, 1000.000000000000000 ) ;
#69090 = CARTESIAN_POINT ( 'NONE',  ( 188.2988323915788271, 86.21831227955479449, -41.65539209327070580 ) ) ;
#69091 = CARTESIAN_POINT ( 'NONE',  ( 48.39383208188444030, -43.94028683479018582, 43.58025477438756212 ) ) ;
#69092 = AXIS2_PLACEMENT_3D ( 'NONE', #23717, #66639, #45160 ) ;
#69093 = DIRECTION ( 'NONE',  ( 0.000000000000000000, 1.000000000000000000, 0.000000000000000000 ) ) ;
#69094 = EDGE_LOOP ( 'NONE', ( #8059, #41445, #29382, #541, #13565, #20029, #29493, #35243, #2702 ) ) ;
#69095 = ORIENTED_EDGE ( 'NONE', *, *, #32463, .T. ) ;
#69096 = VECTOR ( 'NONE', #30936, 1000.000000000000000 ) ;
#69097 = EDGE_LOOP ( 'NONE', ( #12754, #28620, #56158, #8625 ) ) ;
#69098 = AXIS2_PLACEMENT_3D ( 'NONE', #7936, #23769, #61735 ) ;
#69099 = FACE_OUTER_BOUND ( 'NONE', #7976, .T. ) ;
#69100 = CARTESIAN_POINT ( 'NONE',  ( 92.30447928123513179, 22.50875695451826530, -92.09038778501471256 ) ) ;
#69101 = CARTESIAN_POINT ( 'NONE',  ( 108.8631335077135418, -21.45382118812038641, 4.871821213770127557 ) ) ;
#69102 = B_SPLINE_CURVE_WITH_KNOTS ( 'NONE', 3,
 ( #33635, #917, #55064, #22366, #6882, #44524, #39597, #28337, #6183, #65999, #49783, #53061, #10164, #17799, #39255, #60700, #31626, #47793, #69254, #54355, #7599, #18835, #3010, #45562, #46245, #30427, #2318, #67044, #7934, #56824, #40291, #18487, #29733, #29386, #51876, #61734, #24120, #3687, #23768, #8638, #24471, #67382, #45214, #51544 ),
 .UNSPECIFIED., .F., .F.,
 ( 4, 2, 2, 2, 2, 2, 2, 2, 2, 2, 2, 2, 2, 2, 2, 2, 2, 2, 2, 2, 2, 4 ),
 ( 0.02814986980477066775, 0.02995274102020804158, 0.03085417662792674237, 0.03175561223564544316, 0.03355848345108281700, 0.03536135466652019083, 0.03716422588195756466, 0.03896709709739493849, 0.03986853270511362540, 0.04076996831283231232, 0.04167140392055099923, 0.04257283952826968615, 0.04347427513598837306, 0.04437571074370705304, 0.04527714635142573996, 0.04617858195914442687, 0.04798145317458180070, 0.04978432439001917453, 0.05158719560545654836, 0.05339006682089392219, 0.05519293803633129603, 0.05699580925176866986 ),
 .UNSPECIFIED. ) ;
#69103 = CARTESIAN_POINT ( 'NONE',  ( -452.6627218934913230, 399.9999999999997726, 113.5502958579881891 ) ) ;
#69104 = FACE_OUTER_BOUND ( 'NONE', #66417, .T. ) ;
#69105 = VERTEX_POINT ( 'NONE', #48489 ) ;
#69106 = DIRECTION ( 'NONE',  ( -0.000000000000000000, -0.000000000000000000, -1.000000000000000000 ) ) ;
#69107 = CARTESIAN_POINT ( 'NONE',  ( 14.80205238535216949, 6.470775952815779775, -23.62538962562426192 ) ) ;
#69108 = CARTESIAN_POINT ( 'NONE',  ( -7.825402957745085430, 7.899365992529248537, -35.41807073194381417 ) ) ;
#69109 = CARTESIAN_POINT ( 'NONE',  ( 36.61292551086603453, 65.40035471292272007, 41.38025477438755928 ) ) ;
#69110 = CARTESIAN_POINT ( 'NONE',  ( -65.36598343705435354, 0.000000000000000000, 41.38025477438755928 ) ) ;
#69111 = LINE ( 'NONE', #53955, #7055 ) ;
#69112 = CARTESIAN_POINT ( 'NONE',  ( 19.54475376904846939, 6.649964688461122542, 70.85535027690984577 ) ) ;
#69113 = CARTESIAN_POINT ( 'NONE',  ( 0.000000000000000000, 2.449293598294705330E-15, -19.99999999999998934 ) ) ;
#69114 = CARTESIAN_POINT ( 'NONE',  ( 9.280894575734579988, 7.385644305345134164, 6.909217225878244051 ) ) ;
#69115 = B_SPLINE_CURVE_WITH_KNOTS ( 'NONE', 3,
 ( #13160, #55714, #7540, #28996, #23708, #45149 ),
 .UNSPECIFIED., .F., .F.,
 ( 4, 2, 4 ),
 ( 0.03218937259408886919, 0.06469834484649494843, 0.09720731709890104155 ),
 .UNSPECIFIED. ) ;
#69116 = ORIENTED_EDGE ( 'NONE', *, *, #22312, .T. ) ;
#69117 = CARTESIAN_POINT ( 'NONE',  ( 184.0013086981203969, 81.60415045669147105, 16.88678854673017327 ) ) ;
#69118 = PRODUCT_CONTEXT ( 'NONE', #51611, 'mechanical' ) ;
#69119 = CARTESIAN_POINT ( 'NONE',  ( -15.47041015649555185, -73.39774458108232125, 170.0000000000000000 ) ) ;
#69120 = CARTESIAN_POINT ( 'NONE',  ( 6.400000000000000355, -9.237604307034033013, -1.753283555911559014E-16 ) ) ;
#69121 = DIRECTION ( 'NONE',  ( -0.000000000000000000, -1.000000000000000000, -0.000000000000000000 ) ) ;
#69122 = CARTESIAN_POINT ( 'NONE',  ( 58.09877917144280701, 12.61383386832654452, -75.74971096422066807 ) ) ;
#69123 = VERTEX_POINT ( 'NONE', #1376 ) ;
#69124 = ADVANCED_FACE ( 'NONE', ( #21778 ), #43226, .F. ) ;
#69125 = ORIENTED_EDGE ( 'NONE', *, *, #297, .T. ) ;
#69126 = CARTESIAN_POINT ( 'NONE',  ( -24.70354720400823112, 8.582324684301857687, -12.63687245714519136 ) ) ;
#69127 = CARTESIAN_POINT ( 'NONE',  ( 198.8732368717152212, 100.3103976497391301, 14.59490042447026603 ) ) ;
#69128 = VERTEX_POINT ( 'NONE', #1033 ) ;
#69129 = ADVANCED_FACE ( 'NONE', ( #22483 ), #43920, .T. ) ;
#69130 = AXIS2_PLACEMENT_3D ( 'NONE', #30087, #19520, #67722 ) ;
#69131 = B_SPLINE_CURVE_WITH_KNOTS ( 'NONE', 3,
 ( #31003, #52450, #35235, #56690, #4267, #25730 ),
 .UNSPECIFIED., .F., .F.,
 ( 4, 2, 4 ),
 ( 1.095770181103599004E-06, 0.03239442681617710207, 0.06478775786217309818 ),
 .UNSPECIFIED. ) ;
#69132 = CARTESIAN_POINT ( 'NONE',  ( 110.2429982417149432, 28.88204397445228722, 71.45576479620103783 ) ) ;
#69133 = ORIENTED_EDGE ( 'NONE', *, *, #48469, .F. ) ;
#69134 = CARTESIAN_POINT ( 'NONE',  ( -417.6627218934913230, 399.9999999999998295, 78.55029585798814651 ) ) ;
#69135 = CARTESIAN_POINT ( 'NONE',  ( 130.3019683985926349, 39.31883119822051498, 30.38914951925604413 ) ) ;
#69136 = VECTOR ( 'NONE', #34255, 1000.000000000000000 ) ;
#69137 = LINE ( 'NONE', #47334, #16234 ) ;
#69138 = CARTESIAN_POINT ( 'NONE',  ( 159.9864727992238329, 59.63397373978884275, -90.23824594202466187 ) ) ;
#69139 = AXIS2_PLACEMENT_3D ( 'NONE', #26220, #10373, #47659 ) ;
#69141 = CARTESIAN_POINT ( 'NONE',  ( 89.21005684773504640, 20.31770592753387561, -50.36762118906799657 ) ) ;
#69140 = VECTOR ( 'NONE', #57732, 1000.000000000000000 ) ;
#69143 = ORIENTED_EDGE ( 'NONE', *, *, #5076, .F. ) ;
#69142 = CARTESIAN_POINT ( 'NONE',  ( -25.00000000000000000, 65.13282190615278466, 5.000000000000000000 ) ) ;
#69144 = EDGE_CURVE ( 'NONE', #69403, #66426, #53436, .T. ) ;
#69145 = CARTESIAN_POINT ( 'NONE',  ( 51.85299110299497016, -39.21848821248376282, 41.38025477438755928 ) ) ;
#69146 = AXIS2_PLACEMENT_3D ( 'NONE', #4714, #47610, #63811 ) ;
#69147 = ORIENTED_EDGE ( 'NONE', *, *, #54944, .F. ) ;
#69149 = ORIENTED_EDGE ( 'NONE', *, *, #5851, .T. ) ;
#69148 = EDGE_CURVE ( 'NONE', #59809, #68503, #23192, .T. ) ;
#69150 = CARTESIAN_POINT ( 'NONE',  ( -118.9468627709229054, 42.08677365399180559, -12.73045928823215078 ) ) ;
#69151 = CIRCLE ( 'NONE', #64690, 65.36598343705435354 ) ;
#69152 = DIRECTION ( 'NONE',  ( 0.000000000000000000, 0.000000000000000000, 1.000000000000000000 ) ) ;
#69153 =( REPRESENTATION_RELATIONSHIP ('NONE','NONE', #40274, #5548 ) REPRESENTATION_RELATIONSHIP_WITH_TRANSFORMATION ( #37005 )SHAPE_REPRESENTATION_RELATIONSHIP( ) );
#69154 = CARTESIAN_POINT ( 'NONE',  ( -179.9014775667593256, 95.00669833041662571, -18.58505786628793288 ) ) ;
#69155 = EDGE_CURVE ( 'NONE', #62318, #28106, #50607, .T. ) ;
#69156 = CARTESIAN_POINT ( 'NONE',  ( 10.00000000000000178, 35.26862320190615208, -5.000000000000000000 ) ) ;
#69158 = EDGE_LOOP ( 'NONE', ( #1605, #65575, #4312, #19029 ) ) ;
#69157 = CARTESIAN_POINT ( 'NONE',  ( -143.8794621588509131, 59.54894433207191895, -47.27635651071666700 ) ) ;
#69159 = CARTESIAN_POINT ( 'NONE',  ( -105.2272522001715203, 35.43984897390651412, 84.78553490936539561 ) ) ;
#69160 = ADVANCED_FACE ( 'NONE', ( #61166 ), #29849, .T. ) ;
#69161 = ORIENTED_EDGE ( 'NONE', *, *, #8569, .F. ) ;
#69162 = CARTESIAN_POINT ( 'NONE',  ( -62.53989795537026453, 16.81768094534200486, -15.36652373032253571 ) ) ;
#69163 = CARTESIAN_POINT ( 'NONE',  ( -95.52093927227220149, 30.58993121475389287, 68.12384946097193961 ) ) ;
#69164 = LINE ( 'NONE', #31888, #69028 ) ;
#69165 = CARTESIAN_POINT ( 'NONE',  ( 59.13912479700537261, 11.80663573504270580, -90.47641827390418712 ) ) ;
#69166 = CARTESIAN_POINT ( 'NONE',  ( -95.05546640093039912, 29.25972325950978359, 9.094772062743739838 ) ) ;
#69167 = CARTESIAN_POINT ( 'NONE',  ( -151.1146011326114262, 65.55487790163387274, -88.67329123693549775 ) ) ;
#69168 = EDGE_LOOP ( 'NONE', ( #12832, #44276, #13215, #54951, #892, #15054, #64663, #64044, #32936, #25399, #28140, #9530, #20823, #66372, #49828, #21220, #10082, #46075 ) ) ;
#69169 = ORIENTED_EDGE ( 'NONE', *, *, #12497, .T. ) ;
#69170 = FACE_OUTER_BOUND ( 'NONE', #46647, .T. ) ;
#69171 = CARTESIAN_POINT ( 'NONE',  ( -166.5686015187718283, 80.11916873959171426, -38.55272842176326265 ) ) ;
#69173 = EDGE_CURVE ( 'NONE', #15418, #60845, #60806, .T. ) ;
#69172 = CARTESIAN_POINT ( 'NONE',  ( 29.69502258243350923, 57.82046033912877903, 170.0000000000000000 ) ) ;
#69174 = EDGE_CURVE ( 'NONE', #45231, #35894, #12330, .T. ) ;
#69175 = DIRECTION ( 'NONE',  ( 0.000000000000000000, 0.000000000000000000, -1.000000000000000000 ) ) ;
#69176 = CARTESIAN_POINT ( 'NONE',  ( -12.50012419267789632, 0.000000000000000000, -27.27172336262651697 ) ) ;
#69177 = CARTESIAN_POINT ( 'NONE',  ( 79.22946426532585917, 17.02750615740071538, 35.96478783741785890 ) ) ;
#69178 = EDGE_CURVE ( 'NONE', #45327, #44398, #518, .T. ) ;
#69179 = DIRECTION ( 'NONE',  ( -1.850371928290090422E-16, 1.000000000000000000, 1.110223024625156171E-16 ) ) ;
#69180 = CARTESIAN_POINT ( 'NONE',  ( 41.80869235728137312, 9.750404582811613707, -50.24005329498232442 ) ) ;
#69181 = CARTESIAN_POINT ( 'NONE',  ( 209.5118425285947978, 113.1852661712287187, 69.30774190640538279 ) ) ;
#69182 = ORIENTED_EDGE ( 'NONE', *, *, #3333, .T. ) ;
#69183 = DIRECTION ( 'NONE',  ( 0.5407162030609372616, -0.6444004775717707689, 0.5407162030609374836 ) ) ;
#69184 = ORIENTED_EDGE ( 'NONE', *, *, #43567, .F. ) ;
#69185 = VECTOR ( 'NONE', #62623, 1000.000000000000000 ) ;
#69186 = CARTESIAN_POINT ( 'NONE',  ( -14.92903005859421306, 7.458185427130750611, -40.49964561733013113 ) ) ;
#69187 = CARTESIAN_POINT ( 'NONE',  ( 86.62931800182293784, 20.48449268398422163, 71.55663816294304524 ) ) ;
#69188 = CARTESIAN_POINT ( 'NONE',  ( 93.43270425363546394, 22.93046121381055613, 60.89014534178737392 ) ) ;
#69189 = CARTESIAN_POINT ( 'NONE',  ( 155.7262569076171417, 56.30477153194512141, -9.429534158704324653 ) ) ;
#69190 = CARTESIAN_POINT ( 'NONE',  ( 14.83727810650406731, 400.0000000000001137, -353.9497041420119672 ) ) ;
#69192 = CARTESIAN_POINT ( 'NONE',  ( 0.000000000000000000, 0.000000000000000000, 0.000000000000000000 ) ) ;
#69191 = CIRCLE ( 'NONE', #11898, 24.69999999999999929 ) ;
#69193 = CARTESIAN_POINT ( 'NONE',  ( 37.70762885381311236, 8.195134395012283690, -62.65420549904246172 ) ) ;
#69194 = CARTESIAN_POINT ( 'NONE',  ( -452.6627218934918346, 365.0000000000064233, -146.4497041420121377 ) ) ;
#69195 = CARTESIAN_POINT ( 'NONE',  ( -34.06637338149494809, 11.05895377318623574, -23.00161039628460458 ) ) ;
#69196 = VECTOR ( 'NONE', #100, 1000.000000000000000 ) ;
#69197 = EDGE_LOOP ( 'NONE', ( #44655, #59446 ) ) ;
#69198 = CARTESIAN_POINT ( 'NONE',  ( -20.63749999999999929, 0.000000000000000000, 0.000000000000000000 ) ) ;
#69199 = ORIENTED_EDGE ( 'NONE', *, *, #54505, .T. ) ;
#69200 = PRODUCT_DEFINITION_FORMATION_WITH_SPECIFIED_SOURCE ( 'ANY', '', #25383, .NOT_KNOWN. ) ;
#69201 = DIRECTION ( 'NONE',  ( 1.000000000000000000, 0.000000000000000000, 0.000000000000000000 ) ) ;
#69202 = CARTESIAN_POINT ( 'NONE',  ( 13.37708032728285268, 7.441924986912759721, -76.96957816635067218 ) ) ;
#69203 = CARTESIAN_POINT ( 'NONE',  ( -189.8071159312682994, 107.8771087123619736, 8.698159761132112422 ) ) ;
#69204 = CYLINDRICAL_SURFACE ( 'NONE', #9755, 65.00000000000000000 ) ;
#69205 = CIRCLE ( 'NONE', #25397, 65.00000000000000000 ) ;
#69206 = CARTESIAN_POINT ( 'NONE',  ( -7.336760511143403107, 6.859209474528212169, 30.11558103944718923 ) ) ;
#69207 = DIRECTION ( 'NONE',  ( 0.6579387259397138088, -0.7530714660036099684, 0.000000000000000000 ) ) ;
#69208 = CARTESIAN_POINT ( 'NONE',  ( 151.8005253678161921, 54.62151558044534028, -48.56025122383216086 ) ) ;
#69209 = AXIS2_PLACEMENT_3D ( 'NONE', #27400, #21776, #21434 ) ;
#69210 = VERTEX_POINT ( 'NONE', #45328 ) ;
#69211 = CARTESIAN_POINT ( 'NONE',  ( -162.5100517536593827, 306.5915846175126376, 486.5068267248761344 ) ) ;
#69212 = CARTESIAN_POINT ( 'NONE',  ( -189.5329886872043232, 107.4958891766010680, -17.39794636820806417 ) ) ;
#69213 = CARTESIAN_POINT ( 'NONE',  ( 179.0091171455097765, 77.94933395983136393, -24.10062151846888412 ) ) ;
#69214 = CARTESIAN_POINT ( 'NONE',  ( -107.7677210873466578, 36.80113675102408877, 59.72839805516473888 ) ) ;
#69215 = FACE_OUTER_BOUND ( 'NONE', #19454, .T. ) ;
#69216 = VERTEX_POINT ( 'NONE', #12633 ) ;
#69217 = DIRECTION ( 'NONE',  ( 0.000000000000000000, 0.000000000000000000, 1.000000000000000000 ) ) ;
#69218 = CARTESIAN_POINT ( 'NONE',  ( -0.3747453031323926265, 6.520267647591904137, -17.06192658141792862 ) ) ;
#69219 = CARTESIAN_POINT ( 'NONE',  ( -44.00727179482577611, 47.83680621839560132, 170.0000000000000000 ) ) ;
#69220 = CARTESIAN_POINT ( 'NONE',  ( -153.7071867110339838, 67.82509357424204666, 85.68967940371055647 ) ) ;
#69221 = ADVANCED_FACE ( 'NONE', ( #51316, #7363 ), #2090, .F. ) ;
#69222 = CARTESIAN_POINT ( 'NONE',  ( 136.3292018078239494, 42.93753790426546146, 29.92580818695415701 ) ) ;
#69223 = VERTEX_POINT ( 'NONE', #56579 ) ;
#69224 = CARTESIAN_POINT ( 'NONE',  ( 447.3372781065085633, 177.8591479523844612, -111.4497041420119388 ) ) ;
#69225 = CARTESIAN_POINT ( 'NONE',  ( 81.76212856587196143, 18.87332718082996763, 4.656136250459809389 ) ) ;
#69226 = CARTESIAN_POINT ( 'NONE',  ( 164.6561571795775194, 64.77723933022093661, 12.28447893835758542 ) ) ;
#69227 = CARTESIAN_POINT ( 'NONE',  ( 0.000000000000000000, 0.000000000000000000, 73.58025477438756923 ) ) ;
#69228 = ORIENTED_EDGE ( 'NONE', *, *, #68145, .F. ) ;
#69229 = EDGE_CURVE ( 'NONE', #27445, #27319, #39711, .T. ) ;
#69230 = CARTESIAN_POINT ( 'NONE',  ( 173.7225111622554437, 72.84868911716897344, 65.11675756556223860 ) ) ;
#69231 = VERTEX_POINT ( 'NONE', #67161 ) ;
#69232 = AXIS2_PLACEMENT_3D ( 'NONE', #56206, #30871, #25253 ) ;
#69233 = CARTESIAN_POINT ( 'NONE',  ( -102.2801239173131194, 32.78103895658057354, -35.01457726497591239 ) ) ;
#69234 = DIRECTION ( 'NONE',  ( -0.000000000000000000, -1.000000000000000000, -0.000000000000000000 ) ) ;
#69235 = EDGE_CURVE ( 'NONE', #7387, #12094, #61514, .T. ) ;
#69236 = DIRECTION ( 'NONE',  ( 0.000000000000000000, 0.000000000000000000, 1.000000000000000000 ) ) ;
#69237 = EDGE_CURVE ( 'NONE', #17852, #29447, #56228, .T. ) ;
#69238 = VECTOR ( 'NONE', #41186, 1000.000000000000000 ) ;
#69240 = ORIENTED_EDGE ( 'NONE', *, *, #44865, .F. ) ;
#69239 = CYLINDRICAL_SURFACE ( 'NONE', #45516, 7.500000000000013323 ) ;
#69241 = CARTESIAN_POINT ( 'NONE',  ( -179.6470915626257465, 94.69856161161348496, 34.61518667817517070 ) ) ;
#69242 = LINE ( 'NONE', #3856, #40652 ) ;
#69243 = EDGE_CURVE ( 'NONE', #48350, #25214, #39839, .T. ) ;
#69244 = CARTESIAN_POINT ( 'NONE',  ( 115.0485321076020284, 32.28990710985444679, -37.64332603850842673 ) ) ;
#69245 = VECTOR ( 'NONE', #1145, 1000.000000000000114 ) ;
#69246 = ORIENTED_EDGE ( 'NONE', *, *, #51299, .T. ) ;
#69247 = ORIENTED_EDGE ( 'NONE', *, *, #52411, .T. ) ;
#69248 = DIRECTION ( 'NONE',  ( 0.000000000000000000, 0.000000000000000000, -1.000000000000000000 ) ) ;
#69249 = ADVANCED_BREP_SHAPE_REPRESENTATION ( '', ( #63029, #66832 ), #32049 ) ;
#69250 = AXIS2_PLACEMENT_3D ( 'NONE', #31209, #63555, #52975 ) ;
#69251 = CARTESIAN_POINT ( 'NONE',  ( 134.3172730033263633, 41.70277427218489663, 71.35489142945908725 ) ) ;
#69252 = CARTESIAN_POINT ( 'NONE',  ( -166.9969673948021409, 80.56076768517783648, 42.65932412964239973 ) ) ;
#69253 = CARTESIAN_POINT ( 'NONE',  ( 127.4992165631961285, 38.87141012667725448, 59.84453210894926656 ) ) ;
#69254 = CARTESIAN_POINT ( 'NONE',  ( 188.2950202724320832, 86.21411212788221690, -18.96334599335139259 ) ) ;
#69255 = B_SPLINE_CURVE_WITH_KNOTS ( 'NONE', 3,
 ( #23682, #66606, #61311, #45125, #18396, #39853 ),
 .UNSPECIFIED., .F., .F.,
 ( 4, 2, 4 ),
 ( 2.380731631042988191E-07, 0.002336973833157624057, 0.004673709593152144438 ),
 .UNSPECIFIED. ) ;
#69256 = ORIENTED_EDGE ( 'NONE', *, *, #31936, .F. ) ;
#69257 = CARTESIAN_POINT ( 'NONE',  ( -8.320534640989473374, 7.931748412542462212, 71.96013162991094703 ) ) ;
#69258 = ORIENTED_EDGE ( 'NONE', *, *, #39782, .F. ) ;
#69259 = VERTEX_POINT ( 'NONE', #14015 ) ;
#69261 = EDGE_CURVE ( 'NONE', #58577, #48517, #25625, .T. ) ;
#69260 = CARTESIAN_POINT ( 'NONE',  ( -452.6627218934859798, 400.0000000000066507, -146.4497041420121377 ) ) ;
#69262 = CARTESIAN_POINT ( 'NONE',  ( -62.48811917300399443, 16.80201428380103934, 92.54160460740271787 ) ) ;
#69263 = SURFACE_STYLE_FILL_AREA ( #54808 ) ;
#69264 = DIRECTION ( 'NONE',  ( 2.377681859532301304E-16, -7.725556675377196710E-17, 1.000000000000000000 ) ) ;
#69265 = CARTESIAN_POINT ( 'NONE',  ( -109.4660948262506537, 36.58364455021701644, 89.53602648964154298 ) ) ;
#69266 = ADVANCED_FACE ( 'NONE', ( #36858 ), #47389, .F. ) ;
#69267 = CARTESIAN_POINT ( 'NONE',  ( 187.2384682876462136, 86.54721710842893856, 14.27990392942774633 ) ) ;
#69268 = CARTESIAN_POINT ( 'NONE',  ( 313.9975424824652350, 295.6904194069557548, 539.5330678552892323 ) ) ;
#69269 = B_SPLINE_CURVE_WITH_KNOTS ( 'NONE', 3,
 ( #16617, #27515, #64463, #53549, #798, #37045, #22250, #53890, #5381, #16275, #65163, #16956, #26836, #31768, #59870, #69034, #21545, #53198, #11686, #5026, #52856, #4682, #26147, #47579, #42992, #26492, #47927, #69398, #21217, #42662, #64119, #15930, #37376, #58833, #18363, #28930, #45439, #44035, #66231, #33852, #33517, #54945, #6763, #55643, #7480, #50716, #23647 ),
 .UNSPECIFIED., .F., .F.,
 ( 4, 2, 2, 2, 2, 2, 2, 2, 2, 2, 2, 1, 2, 2, 2, 2, 2, 2, 2, 2, 2, 2, 2, 4 ),
 ( 0.000000000000000000, 0.003297771944418890870, 0.004122214930523575641, 0.004946657916628260411, 0.006595543888837629085, 0.007419986874942339876, 0.008244429861047052402, 0.009068872847151762326, 0.009893315833256473985, 0.01154220180546592679, 0.01236664479157065580, 0.01319108777767538133, 0.01401553076378011034, 0.01483997374988483761, 0.01566441673598956835, 0.01648885972209429562, 0.01813774569430378139, 0.01896218868040854336, 0.01978663166651330532, 0.02061107465261806729, 0.02143551763872282578, 0.02308440361093234625, 0.02473328958314187018, 0.02638217555535139064 ),
 .UNSPECIFIED. ) ;
#69270 = CARTESIAN_POINT ( 'NONE',  ( -31.11269837220801193, 31.11269837220812207, 85.00100000000000477 ) ) ;
#69271 = ORIENTED_EDGE ( 'NONE', *, *, #22627, .T. ) ;
#69272 = CARTESIAN_POINT ( 'NONE',  ( -97.21566814336060247, 31.39773419228200524, -90.65435922756391562 ) ) ;
#69273 = ORIENTED_EDGE ( 'NONE', *, *, #35169, .T. ) ;
#69274 = CARTESIAN_POINT ( 'NONE',  ( -71.27103490383373696, 20.70545763375147530, 66.03643395433377350 ) ) ;
#69275 = DIRECTION ( 'NONE',  ( 0.000000000000000000, 0.000000000000000000, 1.000000000000000000 ) ) ;
#69276 = CARTESIAN_POINT ( 'NONE',  ( 62.53328835682431475, 12.56090025569836754, -77.56524142263340593 ) ) ;
#69277 = CARTESIAN_POINT ( 'NONE',  ( -77.72491324796696688, 21.96482567905608008, 3.617778172024071370 ) ) ;
#69278 = CARTESIAN_POINT ( 'NONE',  ( -120.6739978760425913, 44.33795494230366785, 70.35544155365153074 ) ) ;
#69279 = CARTESIAN_POINT ( 'NONE',  ( -55.05276343752910151, 14.68156374112636620, 3.472777182467474244 ) ) ;
#69280 = CARTESIAN_POINT ( 'NONE',  ( 197.2510943223972504, 96.65903929707269526, 89.47520902944462762 ) ) ;
#69281 = CARTESIAN_POINT ( 'NONE',  ( 164.6598737201887559, 64.78038692612514637, -72.67496918674851258 ) ) ;
#69282 = ORIENTED_EDGE ( 'NONE', *, *, #53288, .F. ) ;
#69283 = CARTESIAN_POINT ( 'NONE',  ( -71.26675986148644881, 19.63956187826082811, 66.01101777128145898 ) ) ;
#69284 = DIRECTION ( 'NONE',  ( -3.049318610115480619E-20, -1.000000000000000000, -6.106226635438359986E-16 ) ) ;
#69285 = ORIENTED_EDGE ( 'NONE', *, *, #15489, .F. ) ;
#69286 = EDGE_LOOP ( 'NONE', ( #14048, #55980, #63839 ) ) ;
#69287 = CARTESIAN_POINT ( 'NONE',  ( -156.7487895666417046, 70.57327586518567841, 36.24776524068245465 ) ) ;
#69288 = CARTESIAN_POINT ( 'NONE',  ( 59.29597493004737174, 11.84030339376940510, -36.68987112816819973 ) ) ;
#69289 = CARTESIAN_POINT ( 'NONE',  ( 57.25833571151937207, -48.36523237396138342, 41.38025477438755928 ) ) ;
#69290 = AXIS2_PLACEMENT_3D ( 'NONE', #49277, #10964, #27483 ) ;
#69291 = PLANE ( 'NONE',  #8068 ) ;
#69292 = CARTESIAN_POINT ( 'NONE',  ( 56.74421265833558436, 32.44697398030905333, 43.58025477438756212 ) ) ;
#69293 = VECTOR ( 'NONE', #58992, 1000.000000000000000 ) ;
#69294 = ORIENTED_EDGE ( 'NONE', *, *, #8361, .F. ) ;
#69295 = ORIENTED_EDGE ( 'NONE', *, *, #54131, .F. ) ;
#69296 = CARTESIAN_POINT ( 'NONE',  ( -133.2787743207940991, 52.78950725740543959, 39.45582838502271272 ) ) ;
#69297 = CIRCLE ( 'NONE', #23230, 4.999999999999997335 ) ;
#69298 = ORIENTED_EDGE ( 'NONE', *, *, #34802, .F. ) ;
#69299 = DIRECTION ( 'NONE',  ( -1.387778780781445429E-16, 1.000000000000000000, 3.081487911019577365E-33 ) ) ;
#69300 = CARTESIAN_POINT ( 'NONE',  ( 0.000000000000000000, 0.000000000000000000, 0.000000000000000000 ) ) ;
#69301 = CARTESIAN_POINT ( 'NONE',  ( 207.8675797643809631, 110.7908513421272119, 43.51807350428817500 ) ) ;
#69302 = FACE_BOUND ( 'NONE', #30784, .T. ) ;
#69303 = CYLINDRICAL_SURFACE ( 'NONE', #274, 7.500000000000013323 ) ;
#69304 = AXIS2_PLACEMENT_3D ( 'NONE', #57700, #47129, #25359 ) ;
#69305 = ADVANCED_FACE ( 'NONE', ( #20670 ), #56936, .F. ) ;
#69306 = SURFACE_STYLE_FILL_AREA ( #16870 ) ;
#69307 = VECTOR ( 'NONE', #67380, 1000.000000000000000 ) ;
#69308 = EDGE_CURVE ( 'NONE', #42408, #1617, #26306, .T. ) ;
#69309 = VERTEX_POINT ( 'NONE', #30541 ) ;
#69310 = ORIENTED_EDGE ( 'NONE', *, *, #32658, .T. ) ;
#69311 = DIRECTION ( 'NONE',  ( 1.000000000000000000, 6.405132834375897126E-16, 4.102572662600025274E-31 ) ) ;
#69312 = DIRECTION ( 'NONE',  ( 0.000000000000000000, -3.469446951953614805E-17, 1.000000000000000000 ) ) ;
#69313 = CARTESIAN_POINT ( 'NONE',  ( -165.6212796729685124, 79.15047440262053158, -15.67432408031424806 ) ) ;
#69314 = CARTESIAN_POINT ( 'NONE',  ( 133.8566784816069060, 41.42467568809810530, -77.86786152285937135 ) ) ;
#69315 = DIRECTION ( 'NONE',  ( 0.000000000000000000, 0.000000000000000000, -1.000000000000000000 ) ) ;
#69316 = CARTESIAN_POINT ( 'NONE',  ( -189.9638655956219679, 108.0957249433520246, -72.18686446978868787 ) ) ;
#69317 = ORIENTED_EDGE ( 'NONE', *, *, #38668, .T. ) ;
#69318 = CARTESIAN_POINT ( 'NONE',  ( -4.999999999999971578, 15.55634918610403084, 0.000000000000000000 ) ) ;
#69319 = ADVANCED_FACE ( 'NONE', ( #68518 ), #19993, .F. ) ;
#69320 = CARTESIAN_POINT ( 'NONE',  ( -99.31850058233797540, 31.30166762705807670, 71.75812556856945434 ) ) ;
#69321 = ORIENTED_EDGE ( 'NONE', *, *, #32971, .T. ) ;
#69322 = DIRECTION ( 'NONE',  ( -0.000000000000000000, 1.000000000000000000, -0.000000000000000000 ) ) ;
#69323 = VERTEX_POINT ( 'NONE', #4160 ) ;
#69324 = EDGE_CURVE ( 'NONE', #6967, #13968, #26388, .T. ) ;
#69325 = EDGE_CURVE ( 'NONE', #53557, #42385, #24924, .T. ) ;
#69326 = B_SPLINE_CURVE_WITH_KNOTS ( 'NONE', 3,
 ( #8048, #23546, #18256, #61518, #29161, #56232, #30208, #7713, #3466, #14018, #9095, #45688, #56939, #67165, #40745, #46025, #29852, #50963, #39715, #35126, #51319, #45332, #61170, #57282, #2775, #41102, #13337, #35478, #62561, #55895, #12995, #56582, #18954, #2429, #40400, #61846, #51658, #35829, #67492, #30544, #24927, #46360, #23886, #67842 ),
 .UNSPECIFIED., .F., .F.,
 ( 4, 2, 2, 2, 2, 2, 2, 2, 2, 2, 2, 2, 1, 2, 2, 2, 2, 2, 2, 1, 2, 2, 4 ),
 ( 0.02381751147647563627, 0.02531129726520768564, 0.02605819015957370685, 0.02680508305393972807, 0.02829886884267176356, 0.02979265463140379558, 0.03053954752576982720, 0.03128644042013585536, 0.03278022620886791860, 0.03427401199759996103, 0.03576779778633200346, 0.03651469068069800039, 0.03726158357506400426, 0.03800847646943000119, 0.03875536936379600506, 0.04024915515252804055, 0.04174294094126008298, 0.04323672672999212541, 0.04398361962435815009, 0.04473051251872417478, 0.04547740541309019946, 0.04622429830745622414, 0.04771808409618829433 ),
 .UNSPECIFIED. ) ;
#69327 = VERTEX_POINT ( 'NONE', #62900 ) ;
#69328 = CARTESIAN_POINT ( 'NONE',  ( -118.8691191306315034, 43.21907118237573542, 13.91607852633928566 ) ) ;
#69329 = CARTESIAN_POINT ( 'NONE',  ( -177.1539090641757355, 91.73101548694627638, 71.50528903873359354 ) ) ;
#69330 = CARTESIAN_POINT ( 'NONE',  ( 16.28371206594635368, 6.516665886438622657, 18.17015708224157322 ) ) ;
#69331 = ORIENTED_EDGE ( 'NONE', *, *, #64112, .T. ) ;
#69332 = VECTOR ( 'NONE', #12391, 1000.000000000000114 ) ;
#69333 = CARTESIAN_POINT ( 'NONE',  ( -443.8104064242511981, 394.8690347851185152, 98.47546630130500489 ) ) ;
#69334 = CIRCLE ( 'NONE', #61524, 242.4895526022646379 ) ;
#69335 = CARTESIAN_POINT ( 'NONE',  ( 154.6667526376336923, 55.50347409140649546, 43.86940883944475189 ) ) ;
#69336 = LINE ( 'NONE', #20804, #48195 ) ;
#69337 = CYLINDRICAL_SURFACE ( 'NONE', #32759, 7.500000000000020428 ) ;
#69338 = CARTESIAN_POINT ( 'NONE',  ( -24.19091603582231542, 8.513464105188679909, 39.65939032213886861 ) ) ;
#69339 = VECTOR ( 'NONE', #33415, 1000.000000000000000 ) ;
#69340 = DIRECTION ( 'NONE',  ( 0.000000000000000000, 1.000000000000000000, 0.000000000000000000 ) ) ;
#69341 = ORIENTED_EDGE ( 'NONE', *, *, #30555, .T. ) ;
#69342 = FACE_BOUND ( 'NONE', #21452, .T. ) ;
#69343 = AXIS2_PLACEMENT_3D ( 'NONE', #49066, #38530, #44140 ) ;
#69344 = CARTESIAN_POINT ( 'NONE',  ( 24.46491470961352732, 5.710143558203322200, 3.061616997868437868E-16 ) ) ;
#69345 = CARTESIAN_POINT ( 'NONE',  ( -42.36049017605873956, -61.90437280228297112, 43.58025477438756212 ) ) ;
#69346 = CARTESIAN_POINT ( 'NONE',  ( 117.1658080721356470, 32.21846976819855257, -94.19636932247044570 ) ) ;
#69347 = CARTESIAN_POINT ( 'NONE',  ( -119.2804658695888378, 43.47213805166353495, -45.96062334567895391 ) ) ;
#69348 = DIRECTION ( 'NONE',  ( -1.000000000000000000, 0.000000000000000000, 0.000000000000000000 ) ) ;
#69349 = AXIS2_PLACEMENT_3D ( 'NONE', #34846, #23592, #17964 ) ;
#69350 = CARTESIAN_POINT ( 'NONE',  ( 0.000000000000000000, 0.000000000000000000, 40.00000000000003553 ) ) ;
#69351 = ADVANCED_FACE ( 'NONE', ( #57962 ), #10116, .F. ) ;
#69352 = CARTESIAN_POINT ( 'NONE',  ( -154.0775378574014383, 68.15437918458555089, 17.34221547010214692 ) ) ;
#69353 = CARTESIAN_POINT ( 'NONE',  ( -125.8938041572051389, 47.69968343338780414, -61.75825448869760237 ) ) ;
#69354 = CARTESIAN_POINT ( 'NONE',  ( 67.92995549349548412, 13.86623459444478534, 4.781840506428621573 ) ) ;
#69355 = FACE_OUTER_BOUND ( 'NONE', #6656, .T. ) ;
#69356 = CARTESIAN_POINT ( 'NONE',  ( 88.52077179907882964, 21.14145351760141267, -9.215479869664170209 ) ) ;
#69357 = ORIENTED_EDGE ( 'NONE', *, *, #24669, .F. ) ;
#69358 = CONTEXT_DEPENDENT_SHAPE_REPRESENTATION ( #13905, #50737 ) ;
#69359 = ORIENTED_EDGE ( 'NONE', *, *, #13414, .T. ) ;
#69360 = CARTESIAN_POINT ( 'NONE',  ( -65.00000000000000000, 0.000000000000000000, 170.0000000000000000 ) ) ;
#69361 = VERTEX_POINT ( 'NONE', #3463 ) ;
#69362 = CARTESIAN_POINT ( 'NONE',  ( 110.2429982417149574, 29.99119854320843714, -9.077886975189997543 ) ) ;
#69363 =( LENGTH_UNIT ( ) NAMED_UNIT ( * ) SI_UNIT ( .MILLI., .METRE. ) );
#69364 = CARTESIAN_POINT ( 'NONE',  ( -142.5042386072304055, 59.74110826975218203, 62.32831377680863483 ) ) ;
#69365 = CARTESIAN_POINT ( 'NONE',  ( 8.000000000000007105, 249.8719672152120381, -95.00000000000133582 ) ) ;
#69366 = LINE ( 'NONE', #20833, #265 ) ;
#69367 = CARTESIAN_POINT ( 'NONE',  ( 208.9325386374517279, 114.1236747564815772, -91.31446213177319748 ) ) ;
#69368 = CARTESIAN_POINT ( 'NONE',  ( 410.0000000000000000, 190.0000000000000000, 2.000000000000000000 ) ) ;
#69369 = CARTESIAN_POINT ( 'NONE',  ( 22.07550062443481664, 11.73338281062075872, 0.000000000000000000 ) ) ;
#69370 = VERTEX_POINT ( 'NONE', #20324 ) ;
#69371 = VERTEX_POINT ( 'NONE', #31574 ) ;
#69372 = CARTESIAN_POINT ( 'NONE',  ( 70.02892116572942882, 14.40944430928136732, -40.55127576682969703 ) ) ;
#69373 = CARTESIAN_POINT ( 'NONE',  ( 181.8106359728740529, 80.78261033454286633, 83.02753339407779265 ) ) ;
#69374 = CARTESIAN_POINT ( 'NONE',  ( 0.000000000000000000, 0.000000000000000000, 0.000000000000000000 ) ) ;
#69375 = LINE ( 'NONE', #20843, #19551 ) ;
#69376 = LINE ( 'NONE', #68684, #67880 ) ;
#69377 = EDGE_CURVE ( 'NONE', #19968, #6351, #9849, .T. ) ;
#69378 = DIRECTION ( 'NONE',  ( 0.000000000000000000, 1.000000000000000000, -0.000000000000000000 ) ) ;
#69379 = CARTESIAN_POINT ( 'NONE',  ( 181.0840389613909736, 80.03940679743416808, -24.38050707541595230 ) ) ;
#69380 = CARTESIAN_POINT ( 'NONE',  ( -85.90441187606242579, 25.21188850826091254, -13.74108820849124335 ) ) ;
#69381 =( LENGTH_UNIT ( ) NAMED_UNIT ( * ) SI_UNIT ( .MILLI., .METRE. ) );
#69382 = AXIS2_PLACEMENT_3D ( 'NONE', #30400, #3324, #46224 ) ;
#69383 = CARTESIAN_POINT ( 'NONE',  ( 50.97490815085634352, 6.000000000000000000, -36.68900338898716740 ) ) ;
#69384 = CARTESIAN_POINT ( 'NONE',  ( 42.03492317486908547, 8.766487167902370814, -23.30212316240421444 ) ) ;
#69385 = LINE ( 'NONE', #32105, #43223 ) ;
#69386 = PLANE ( 'NONE',  #59861 ) ;
#69387 = ADVANCED_FACE ( 'NONE', ( #36508 ), #9781, .F. ) ;
#69388 = FACE_OUTER_BOUND ( 'NONE', #67151, .T. ) ;
#69389 = ADVANCED_FACE ( 'NONE', ( #54037 ), #27670, .F. ) ;
#69390 = EDGE_CURVE ( 'NONE', #32243, #28546, #21023, .T. ) ;
#69391 = ORIENTED_EDGE ( 'NONE', *, *, #46065, .F. ) ;
#69392 = VECTOR ( 'NONE', #23399, 1000.000000000000000 ) ;
#69393 = CARTESIAN_POINT ( 'NONE',  ( -90.13282190615392153, -1.844136286507718230E-12, -9.999999999999998224 ) ) ;
#69394 = CARTESIAN_POINT ( 'NONE',  ( 87.11239765416378589, 20.65008247340817249, -35.82156419891170884 ) ) ;
#69395 = EDGE_CURVE ( 'NONE', #36317, #39465, #27318, .T. ) ;
#69396 = CARTESIAN_POINT ( 'NONE',  ( 409.0783954480986608, -1.426547569622074412E-15, 174.7010307253933377 ) ) ;
#69397 = FACE_OUTER_BOUND ( 'NONE', #52299, .T. ) ;
#69398 = CARTESIAN_POINT ( 'NONE',  ( 150.2809931605061990, 52.27058242113234598, 7.911800210953336077 ) ) ;
#69399 = CARTESIAN_POINT ( 'NONE',  ( -14.46498759803290746, 8.425214076810821240, 87.80158803776117793 ) ) ;
#69400 = ORIENTED_EDGE ( 'NONE', *, *, #901, .T. ) ;
#69401 = LINE ( 'NONE', #21221, #33665 ) ;
#69402 = LINE ( 'NONE', #20516, #2393 ) ;
#69403 = VERTEX_POINT ( 'NONE', #5525 ) ;
#69404 = B_SPLINE_CURVE_WITH_KNOTS ( 'NONE', 3,
 ( #20422, #48171, #10900, #53108, #42900, #32371 ),
 .UNSPECIFIED., .F., .F.,
 ( 4, 2, 4 ),
 ( 1.095770181124384134E-06, 0.03239442681617711595, 0.06478775786217309818 ),
 .UNSPECIFIED. ) ;
#69405 = VECTOR ( 'NONE', #25251, 1000.000000000000114 ) ;
#69406 = ORIENTED_EDGE ( 'NONE', *, *, #1209, .T. ) ;
#69407 = CARTESIAN_POINT ( 'NONE',  ( 45.20784367118678659, 10.25355619695782927, 86.30875473536740117 ) ) ;
#69408 = CARTESIAN_POINT ( 'NONE',  ( 31.11269837220806522, 4.999999999999936939, 85.00100000000000477 ) ) ;
#69409 = CARTESIAN_POINT ( 'NONE',  ( -15.55634918610411077, -41.66904755831209428, 0.000000000000000000 ) ) ;
#69410 = EDGE_CURVE ( 'NONE', #7619, #8543, #31925, .T. ) ;
#69411 = VERTEX_POINT ( 'NONE', #10803 ) ;
#69412 = CARTESIAN_POINT ( 'NONE',  ( 67.54641595172914492, 14.80690682047551121, 70.15402874321907234 ) ) ;
#69413 = DIRECTION ( 'NONE',  ( -0.7660444431189771253, 0.6427876096865404731, -2.989969378020156799E-16 ) ) ;
#69414 = CARTESIAN_POINT ( 'NONE',  ( 37.47081272996201307, 8.166145978397521432, -9.024001403194343851 ) ) ;
#69415 = CARTESIAN_POINT ( 'NONE',  ( 160.2883311361769358, 61.16711613734477027, 43.86358491700874396 ) ) ;
#69416 = CARTESIAN_POINT ( 'NONE',  ( 163.9335029509016692, 62.85601444701051577, 94.42016238087119007 ) ) ;
#69417 = CARTESIAN_POINT ( 'NONE',  ( 88.28780346671267409, 19.99350429399659745, 29.89382215203381676 ) ) ;
#69418 = EDGE_LOOP ( 'NONE', ( #50154, #35827 ) ) ;
#69419 = CARTESIAN_POINT ( 'NONE',  ( 105.4376736768159049, 27.81988511842610023, -22.34144044879345969 ) ) ;
#69420 = DIRECTION ( 'NONE',  ( -0.000000000000000000, 1.000000000000000000, -0.000000000000000000 ) ) ;
#69421 = CARTESIAN_POINT ( 'NONE',  ( -30.95341298663138119, 10.53108683215057084, 30.21645440618916112 ) ) ;
#69422 = CARTESIAN_POINT ( 'NONE',  ( 197.5344433744249102, 98.61756151884685551, 38.95244195491510908 ) ) ;
#69423 = DIRECTION ( 'NONE',  ( 1.000000000000000000, 0.000000000000000000, 0.000000000000000000 ) ) ;
#69425 = VERTEX_POINT ( 'NONE', #597 ) ;
#69424 = LINE ( 'NONE', #53229, #44456 ) ;
#69426 = ORIENTED_EDGE ( 'NONE', *, *, #63160, .F. ) ;
#69427 = ORIENTED_EDGE ( 'NONE', *, *, #36076, .F. ) ;
#69428 = CARTESIAN_POINT ( 'NONE',  ( -51.66904755831212981, -15.55634918610397222, 2.000000000000000000 ) ) ;
#69429 = FACE_OUTER_BOUND ( 'NONE', #38678, .T. ) ;
#69430 = CARTESIAN_POINT ( 'NONE',  ( -55.05276343752908730, 15.72344139423348430, 72.16187836339486239 ) ) ;
#69431 = CARTESIAN_POINT ( 'NONE',  ( -35.99414836699283882, 11.40630460607619945, 58.58236999211133877 ) ) ;
#69432 = CARTESIAN_POINT ( 'NONE',  ( 0.000000000000000000, 70.00000000000000000, 0.000000000000000000 ) ) ;
#69433 = CARTESIAN_POINT ( 'NONE',  ( 150.8925291903903201, 52.71218673668931842, -74.11121607790209964 ) ) ;
#69434 = DIRECTION ( 'NONE',  ( -0.000000000000000000, 1.000000000000000000, -0.000000000000000000 ) ) ;
#69435 = CARTESIAN_POINT ( 'NONE',  ( 46.66904755831210139, 4.999999999999909406, 2.000000000000001776 ) ) ;
#69436 = EDGE_LOOP ( 'NONE', ( #54487, #54999, #33950, #31977 ) ) ;
#69437 = ORIENTED_EDGE ( 'NONE', *, *, #18818, .T. ) ;
#69438 = AXIS2_PLACEMENT_3D ( 'NONE', #12307, #38335, #28840 ) ;
#69439 = CARTESIAN_POINT ( 'NONE',  ( 66.30636076182547356, 14.49616748423541068, -9.619026385704664506 ) ) ;
#69440 = CARTESIAN_POINT ( 'NONE',  ( 0.000000000000000000, 0.000000000000000000, 0.000000000000000000 ) ) ;
#69441 = CARTESIAN_POINT ( 'NONE',  ( 104.5164129159900170, 26.32100697179284765, 85.91093688393655725 ) ) ;
#69442 = CARTESIAN_POINT ( 'NONE',  ( -156.8773151811562911, 72.06122063279302381, 12.79581229564695022 ) ) ;
#69443 = VECTOR ( 'NONE', #51361, 1000.000000000000227 ) ;
#69444 = ADVANCED_FACE ( 'NONE', ( #63929 ), #6573, .F. ) ;
#69445 = CARTESIAN_POINT ( 'NONE',  ( -2.113472939310175658, 74.92159864268209901, 41.38025477438755928 ) ) ;
#69446 = CARTESIAN_POINT ( 'NONE',  ( 0.000000000000000000, 0.000000000000000000, 40.00000000000003553 ) ) ;
#69447 = CARTESIAN_POINT ( 'NONE',  ( 0.000000000000000000, 0.000000000000000000, 0.000000000000000000 ) ) ;
#69448 = ORIENTED_EDGE ( 'NONE', *, *, #34877, .F. ) ;
#69449 = ORIENTED_EDGE ( 'NONE', *, *, #47864, .T. ) ;
#69450 = VERTEX_POINT ( 'NONE', #26645 ) ;
#69451 = CARTESIAN_POINT ( 'NONE',  ( -155.1359377029286009, 70.46175948311802983, -10.48588441764089474 ) ) ;
#69452 = CARTESIAN_POINT ( 'NONE',  ( 33.44035656425387515, 8.720466003183664938, -38.54271289854762017 ) ) ;
#69453 = CARTESIAN_POINT ( 'NONE',  ( -37.38781680082738745, 10.64362327909142714, 59.96723102333222499 ) ) ;
#69454 = CARTESIAN_POINT ( 'NONE',  ( 204.3129818922372749, 107.5244029525888863, 56.05227132923313604 ) ) ;
#69455 = ORIENTED_EDGE ( 'NONE', *, *, #10170, .T. ) ;
#69456 = FACE_BOUND ( 'NONE', #27876, .T. ) ;
#69457 = CARTESIAN_POINT ( 'NONE',  ( -156.4960819023051215, 70.34114605623869920, 67.83986282103712995 ) ) ;
#69458 =( NAMED_UNIT ( * ) SI_UNIT ( $, .STERADIAN. ) SOLID_ANGLE_UNIT ( ) );
#69459 = CARTESIAN_POINT ( 'NONE',  ( -6.843910203392213454, 7.836697961436720483, -35.46655999132715209 ) ) ;
#69460 = CARTESIAN_POINT ( 'NONE',  ( 187.5325688887159004, 85.37769363979911930, 67.52131414333028658 ) ) ;
#69461 = DIRECTION ( 'NONE',  ( 1.387778780781445922E-16, -1.000000000000000000, -1.232595164407830946E-32 ) ) ;
#69462 = CARTESIAN_POINT ( 'NONE',  ( -86.09999398724994535, 25.29376521564874380, -41.58702898857048069 ) ) ;
#69463 = FACE_OUTER_BOUND ( 'NONE', #19314, .T. ) ;
#69464 = CARTESIAN_POINT ( 'NONE',  ( 63.01563776193090405, 13.70579113808097382, -62.56524142263340593 ) ) ;
#69465 = CARTESIAN_POINT ( 'NONE',  ( 13.37820144534469158, 6.435512790162279728, -62.75700969552578101 ) ) ;
#69466 = EDGE_CURVE ( 'NONE', #66593, #63326, #65711, .T. ) ;
#69467 = ORIENTED_EDGE ( 'NONE', *, *, #27350, .F. ) ;
#69468 = LINE ( 'NONE', #58560, #152 ) ;
#69469 = PRODUCT_CONTEXT ( 'NONE', #17920, 'mechanical' ) ;
#69470 = ADVANCED_FACE ( 'NONE', ( #43841 ), #64973, .T. ) ;
#69471 = CARTESIAN_POINT ( 'NONE',  ( 173.6710158776851358, 71.42507420636738402, 35.63177840436776478 ) ) ;
#69472 = CARTESIAN_POINT ( 'NONE',  ( -128.1384526288949814, 47.98891607499718504, -49.58460275042809684 ) ) ;
#69473 = CARTESIAN_POINT ( 'NONE',  ( 39.88971011078922402, 8.472992116645418292, -77.46436805589146957 ) ) ;
#69474 = CARTESIAN_POINT ( 'NONE',  ( 63.01563776193091826, 13.70579113808094718, -77.56524142263344856 ) ) ;
#69475 = ORIENTED_EDGE ( 'NONE', *, *, #26188, .F. ) ;
#69476 = VERTEX_POINT ( 'NONE', #17105 ) ;
#69477 = CARTESIAN_POINT ( 'NONE',  ( -24.93568128341082968, 8.613819379861704206, -12.20478168535062835 ) ) ;
#69478 = CARTESIAN_POINT ( 'NONE',  ( 174.4960269704457119, 72.19444789407123153, 86.89327852742059122 ) ) ;
#69479 = EDGE_LOOP ( 'NONE', ( #35035, #57558, #31065, #26952 ) ) ;
#69480 = CARTESIAN_POINT ( 'NONE',  ( 117.4830770399668012, 32.37795270233551292, 65.97967136513133823 ) ) ;
#69481 = ADVANCED_FACE ( 'NONE', ( #42468 ), #38578, .F. ) ;
#69482 = ORIENTED_EDGE ( 'NONE', *, *, #34499, .F. ) ;
#69483 = CARTESIAN_POINT ( 'NONE',  ( 128.3889472838589256, 39.37765603157609462, -65.21099523326392955 ) ) ;
#69484 = CARTESIAN_POINT ( 'NONE',  ( -190.6985136298601731, 109.1272424661242582, -95.00000000000133582 ) ) ;
#69485 = AXIS2_PLACEMENT_3D ( 'NONE', #66058, #50204, #5886 ) ;
#69486 = DIRECTION ( 'NONE',  ( -0.000000000000000000, 1.000000000000000000, -0.000000000000000000 ) ) ;
#69487 = CARTESIAN_POINT ( 'NONE',  ( 85.83240444548572157, 19.15035268578635907, -89.54263933694141997 ) ) ;
#69488 = AXIS2_PLACEMENT_3D ( 'NONE', #16826, #21415, #15800 ) ;
#69489 = DIRECTION ( 'NONE',  ( 0.9009688679024155933, 0.4338837391175656699, 0.000000000000000000 ) ) ;
#69490 = LINE ( 'NONE', #15351, #53318 ) ;
#69491 = ORIENTED_EDGE ( 'NONE', *, *, #7857, .T. ) ;
#69492 = ORIENTED_EDGE ( 'NONE', *, *, #35651, .F. ) ;
#69493 = CARTESIAN_POINT ( 'NONE',  ( -120.4586945679390482, 43.01762219615311977, -10.37801267066958388 ) ) ;
#69494 = FACE_BOUND ( 'NONE', #58854, .T. ) ;
#69495 = CARTESIAN_POINT ( 'NONE',  ( -173.1211646369891071, 87.12891641440859303, -22.86740657428632773 ) ) ;
#69496 = CARTESIAN_POINT ( 'NONE',  ( -173.1211646369891071, 88.63826465341152527, -61.55650775521367279 ) ) ;
#69498 = VERTEX_POINT ( 'NONE', #37889 ) ;
#69497 = CARTESIAN_POINT ( 'NONE',  ( -144.9439644317224065, 60.40328483334192100, -48.26935030906360424 ) ) ;
#69499 = DIRECTION ( 'NONE',  ( 0.000000000000000000, 1.000000000000000000, 0.000000000000000000 ) ) ;
#69500 = VERTEX_POINT ( 'NONE', #15740 ) ;
#69501 = CARTESIAN_POINT ( 'NONE',  ( 433.3728120124415568, 400.0000000000067075, -132.4852380479447902 ) ) ;
#69502 = DIRECTION ( 'NONE',  ( 1.000000000000000000, 0.000000000000000000, 0.000000000000000000 ) ) ;
#69503 = CARTESIAN_POINT ( 'NONE',  ( 79.93126905972559371, 17.24332478304278382, -19.86064041717387241 ) ) ;
#69504 = CARTESIAN_POINT ( 'NONE',  ( -131.6399667378751701, 51.62465701391632678, -64.41211764283146124 ) ) ;
#69505 = CARTESIAN_POINT ( 'NONE',  ( 59.67833965117457495, 11.92331751763832237, -90.19013027095671475 ) ) ;
#69506 = CARTESIAN_POINT ( 'NONE',  ( -29.70166638324878150, -57.83280658984300970, 41.38025477438755928 ) ) ;
#69507 = CARTESIAN_POINT ( 'NONE',  ( -95.52163045714284806, 29.47808868198297105, -72.62058247320986482 ) ) ;
#69508 = ORIENTED_EDGE ( 'NONE', *, *, #12189, .F. ) ;
#69509 = ORIENTED_EDGE ( 'NONE', *, *, #50654, .T. ) ;
#69510 = CARTESIAN_POINT ( 'NONE',  ( 183.9986899696430953, 81.60141257362811018, -77.49343821721251402 ) ) ;
#69511 = DIRECTION ( 'NONE',  ( -0.000000000000000000, -1.000000000000000000, -0.000000000000000000 ) ) ;
#69512 = DIRECTION ( 'NONE',  ( 0.000000000000000000, 0.000000000000000000, 1.000000000000000000 ) ) ;
#69513 = DIRECTION ( 'NONE',  ( 4.258099457802021297E-18, 2.810746842852143592E-18, -1.000000000000000000 ) ) ;
#69514 = CARTESIAN_POINT ( 'NONE',  ( 110.2429982417149574, 29.99119854320845846, -77.76698815611739235 ) ) ;
#69515 = CARTESIAN_POINT ( 'NONE',  ( -71.15374617000811952, 20.66492714610676273, 37.92836382045980770 ) ) ;
#69516 = EDGE_CURVE ( 'NONE', #45282, #29497, #29748, .T. ) ;
#69517 = CARTESIAN_POINT ( 'NONE',  ( -1.683356153842345604, -65.34430428700412108, 43.58025477438756212 ) ) ;
#69518 = CARTESIAN_POINT ( 'NONE',  ( 29.69502258243432635, -57.82046033912835270, 40.00000000000003553 ) ) ;
#69519 = CARTESIAN_POINT ( 'NONE',  ( 46.80475532923158255, 10.50744084852537163, -44.34838384464438832 ) ) ;
#69520 = FACE_BOUND ( 'NONE', #24254, .T. ) ;
#69521 = ORIENTED_EDGE ( 'NONE', *, *, #55662, .F. ) ;
#69522 = CARTESIAN_POINT ( 'NONE',  ( -102.7502407665687372, 33.01985383847078026, -8.170026674512229192 ) ) ;
#69524 = ORIENTED_EDGE ( 'NONE', *, *, #21752, .F. ) ;
#69523 = B_SPLINE_CURVE_WITH_KNOTS ( 'NONE', 3,
 ( #49022, #69454, #21274, #26210, #47647, #15312, #862, #42384, #42039, #42721, #63499, #58894, #64178, #53948, #10710, #37795, #36773, #53614, #10033, #48321, #31488, #52921, #32518, #4746, #49378, #1208, #12460, #1924, #65226, #13163, #7184, #29331, #50095, #29002, #50445, #17746, #66302, #23382, #38490, #44821, #34272, #18089, #11751, #22315, #23712, #55719, #39884, #7543, #44468, #65949 ),
 .UNSPECIFIED., .F., .F.,
 ( 4, 2, 2, 2, 2, 2, 2, 2, 2, 2, 2, 2, 2, 2, 2, 2, 2, 2, 2, 2, 2, 2, 2, 2, 4 ),
 ( 0.03296461860586798881, 0.03492857779726591533, 0.03689253698866384878, 0.03885649618006177530, 0.04082045537145970182, 0.04278441456285763528, 0.04376639415855656384, 0.04474837375425549241, 0.04573035334995442097, 0.04671233294565334954, 0.04720332274350281382, 0.04769431254135228504, 0.04867629213705121360, 0.04965827173275014217, 0.05064025132844907073, 0.05162223092414799930, 0.05260421051984692786, 0.05358619011554585643, 0.05456816971124478499, 0.05555014930694372050, 0.05653212890264264906, 0.05849608809404049925, 0.06046004728543834250, 0.06242400647683619269, 0.06438796566823404288 ),
 .UNSPECIFIED. ) ;
#69525 = EDGE_CURVE ( 'NONE', #24447, #47168, #3134, .T. ) ;
#69526 = CARTESIAN_POINT ( 'NONE',  ( -14.19493007850031141, 7.389842975086041044, -46.88529827066894029 ) ) ;
#69527 = CYLINDRICAL_SURFACE ( 'NONE', #29585, 7.500000000000013323 ) ;
#69528 = CARTESIAN_POINT ( 'NONE',  ( 94.02861641584118502, 23.15570573563316614, 62.80575613031886917 ) ) ;
#69529 = CARTESIAN_POINT ( 'NONE',  ( 154.6667526376337491, 55.50347409140650257, -9.819692341482584297 ) ) ;
#69530 = CARTESIAN_POINT ( 'NONE',  ( 38.42095780754792855, 9.297684251045552628, 18.02115975282741189 ) ) ;
#69531 = LINE ( 'NONE', #59928, #54683 ) ;
#69532 = CARTESIAN_POINT ( 'NONE',  ( -31.11269837220809364, -10.55634918610397932, 85.00100000000000477 ) ) ;
#69533 = CARTESIAN_POINT ( 'NONE',  ( 111.9975424824652634, 22.00669820036272384, 401.6295345748407613 ) ) ;
#69534 = VECTOR ( 'NONE', #39994, 1000.000000000000000 ) ;
#69535 = EDGE_LOOP ( 'NONE', ( #59069, #12258, #6831, #56180 ) ) ;
#69536 = CARTESIAN_POINT ( 'NONE',  ( 149.0250918491436494, 6.000000000000000000, -41.68900338898718871 ) ) ;
#69537 = ORIENTED_EDGE ( 'NONE', *, *, #65358, .T. ) ;
#69538 = CARTESIAN_POINT ( 'NONE',  ( 57.09527843067915143, 12.40436368789087318, 59.54664166497151712 ) ) ;
#69539 = CARTESIAN_POINT ( 'NONE',  ( -45.14452675491352096, -49.02628165194661847, 34.48241824012613677 ) ) ;
#69540 = CARTESIAN_POINT ( 'NONE',  ( -40.13282190614798850, -1.847197903505587038E-12, 5.000000000000000000 ) ) ;
#69541 = EDGE_CURVE ( 'NONE', #45468, #21445, #16432, .T. ) ;
#69542 = DIRECTION ( 'NONE',  ( 0.000000000000000000, 0.000000000000000000, 1.000000000000000000 ) ) ;
#69543 = CARTESIAN_POINT ( 'NONE',  ( -61.90200967450776659, 16.62550425046104863, -93.31852439468944738 ) ) ;
#69544 = CARTESIAN_POINT ( 'NONE',  ( -96.00016893459647349, 29.70347032303887147, -11.56214555964269941 ) ) ;
#69545 = EDGE_CURVE ( 'NONE', #14540, #59876, #64270, .T. ) ;
#69546 = CARTESIAN_POINT ( 'NONE',  ( 79.43281949162772548, 18.14250680856633480, 88.76187498690042332 ) ) ;
#69547 = EDGE_CURVE ( 'NONE', #6104, #34219, #32953, .T. ) ;
#69548 = ORIENTED_EDGE ( 'NONE', *, *, #18928, .F. ) ;
#69549 = DIRECTION ( 'NONE',  ( -0.7952297978268511036, -5.486401878248946344E-15, -0.6063081466121542640 ) ) ;
#69550 = EDGE_CURVE ( 'NONE', #64521, #68286, #56714, .T. ) ;
#69551 = DIRECTION ( 'NONE',  ( -0.000000000000000000, 1.000000000000000000, -0.000000000000000000 ) ) ;
#69552 = CARTESIAN_POINT ( 'NONE',  ( -132.4819073909166036, 50.98736898418874119, 14.89792975520157547 ) ) ;
#69553 = CARTESIAN_POINT ( 'NONE',  ( -106.4728934171454284, 36.10295170132725673, 58.64049600876298740 ) ) ;
#69554 = ITEM_DEFINED_TRANSFORMATION ( 'NONE', 'NONE', #664,  #66832 ) ;
#69555 = CARTESIAN_POINT ( 'NONE',  ( -180.1361238728360377, 95.29182030496930622, 94.68613861460413261 ) ) ;
#69556 = ORIENTED_EDGE ( 'NONE', *, *, #55168, .F. ) ;
#69557 = LINE ( 'NONE', #47756, #55998 ) ;
#69558 = CARTESIAN_POINT ( 'NONE',  ( 94.12988949694079110, 22.11811104795075522, 64.29232835590543971 ) ) ;
#69559 = CARTESIAN_POINT ( 'NONE',  ( -156.8975660802013010, 70.71010336351562842, 90.58301405942083306 ) ) ;
#69560 = CARTESIAN_POINT ( 'NONE',  ( 141.9165763529819344, 192.0000000000000000, 129.0000000000000000 ) ) ;
#69561 = ADVANCED_FACE ( 'NONE', ( #59333 ), #11146, .T. ) ;
#69562 = VERTEX_POINT ( 'NONE', #1643 ) ;
#69563 = CYLINDRICAL_SURFACE ( 'NONE', #53652, 7.500000000000013323 ) ;
#69564 = CARTESIAN_POINT ( 'NONE',  ( -20.55634918610405748, -15.55634918610400774, 85.00100000000000477 ) ) ;
#69565 = LINE ( 'NONE', #59016, #65865 ) ;
#69566 = DIRECTION ( 'NONE',  ( 0.000000000000000000, 0.000000000000000000, 1.000000000000000000 ) ) ;
#69567 = EDGE_CURVE ( 'NONE', #35709, #7827, #17829, .T. ) ;
#69568 = EDGE_CURVE ( 'NONE', #24108, #51034, #60389, .T. ) ;
#69569 = EDGE_CURVE ( 'NONE', #27634, #55170, #65675, .T. ) ;
#69570 = EDGE_LOOP ( 'NONE', ( #44404, #37098, #41183, #14296 ) ) ;
#69571 = FILL_AREA_STYLE_COLOUR ( '', #38382 ) ;
#69572 = NEXT_ASSEMBLY_USAGE_OCCURRENCE ( 'NAUO1', ' ', ' ', #2684, #46499, $ ) ;
#69573 = NEXT_ASSEMBLY_USAGE_OCCURRENCE ( 'NAUO2', ' ', ' ', #2684, #3950, $ ) ;
#69574 = NEXT_ASSEMBLY_USAGE_OCCURRENCE ( 'NAUO3', ' ', ' ', #2684, #58101, $ ) ;
#69575 = NEXT_ASSEMBLY_USAGE_OCCURRENCE ( 'NAUO4', ' ', ' ', #2684, #43475, $ ) ;
#69576 = NEXT_ASSEMBLY_USAGE_OCCURRENCE ( 'NAUO5', ' ', ' ', #2684, #28900, $ ) ;
#69577 = NEXT_ASSEMBLY_USAGE_OCCURRENCE ( 'NAUO6', ' ', ' ', #2684, #28900, $ ) ;
#69578 = NEXT_ASSEMBLY_USAGE_OCCURRENCE ( 'NAUO7', ' ', ' ', #2684, #38320, $ ) ;
#69579 = NEXT_ASSEMBLY_USAGE_OCCURRENCE ( 'NAUO8', ' ', ' ', #2684, #38320, $ ) ;
#69580 = NEXT_ASSEMBLY_USAGE_OCCURRENCE ( 'NAUO9', ' ', ' ', #2684, #38320, $ ) ;
#69581 = NEXT_ASSEMBLY_USAGE_OCCURRENCE ( 'NAUO10', ' ', ' ', #2684, #38320, $ ) ;
#69582 = NEXT_ASSEMBLY_USAGE_OCCURRENCE ( 'NAUO11', ' ', ' ', #2684, #58964, $ ) ;
#69583 = NEXT_ASSEMBLY_USAGE_OCCURRENCE ( 'NAUO12', ' ', ' ', #2684, #58964, $ ) ;
#69584 = NEXT_ASSEMBLY_USAGE_OCCURRENCE ( 'NAUO13', ' ', ' ', #2684, #58964, $ ) ;
#69585 = NEXT_ASSEMBLY_USAGE_OCCURRENCE ( 'NAUO14', ' ', ' ', #2684, #63276, $ ) ;
#69586 = NEXT_ASSEMBLY_USAGE_OCCURRENCE ( 'NAUO15', ' ', ' ', #2684, #23342, $ ) ;
#69587 = NEXT_ASSEMBLY_USAGE_OCCURRENCE ( 'NAUO16', ' ', ' ', #2684, #57716, $ ) ;
#69588 = NEXT_ASSEMBLY_USAGE_OCCURRENCE ( 'NAUO17', ' ', ' ', #2684, #46114, $ ) ;
#69589 = NEXT_ASSEMBLY_USAGE_OCCURRENCE ( 'NAUO18', ' ', ' ', #2684, #46114, $ ) ;
#69590 = NEXT_ASSEMBLY_USAGE_OCCURRENCE ( 'NAUO19', ' ', ' ', #2684, #46114, $ ) ;
#69591 = NEXT_ASSEMBLY_USAGE_OCCURRENCE ( 'NAUO20', ' ', ' ', #2684, #46114, $ ) ;
#69592 = NEXT_ASSEMBLY_USAGE_OCCURRENCE ( 'NAUO21', ' ', ' ', #2684, #46114, $ ) ;
#69593 = NEXT_ASSEMBLY_USAGE_OCCURRENCE ( 'NAUO22', ' ', ' ', #2684, #46114, $ ) ;
#69594 = NEXT_ASSEMBLY_USAGE_OCCURRENCE ( 'NAUO23', ' ', ' ', #2684, #46114, $ ) ;
#69595 = NEXT_ASSEMBLY_USAGE_OCCURRENCE ( 'NAUO24', ' ', ' ', #2684, #46114, $ ) ;
#69596 = NEXT_ASSEMBLY_USAGE_OCCURRENCE ( 'NAUO25', ' ', ' ', #2684, #9991, $ ) ;
#69597 = NEXT_ASSEMBLY_USAGE_OCCURRENCE ( 'NAUO26', ' ', ' ', #2684, #9991, $ ) ;
#69598 = NEXT_ASSEMBLY_USAGE_OCCURRENCE ( 'NAUO27', ' ', ' ', #2684, #9991, $ ) ;
#69599 = NEXT_ASSEMBLY_USAGE_OCCURRENCE ( 'NAUO28', ' ', ' ', #2684, #9991, $ ) ;
#69600 = NEXT_ASSEMBLY_USAGE_OCCURRENCE ( 'NAUO29', ' ', ' ', #2684, #9991, $ ) ;
#69601 = NEXT_ASSEMBLY_USAGE_OCCURRENCE ( 'NAUO30', ' ', ' ', #2684, #9991, $ ) ;
#69602 = NEXT_ASSEMBLY_USAGE_OCCURRENCE ( 'NAUO31', ' ', ' ', #2684, #9991, $ ) ;
#69603 = NEXT_ASSEMBLY_USAGE_OCCURRENCE ( 'NAUO32', ' ', ' ', #2684, #9991, $ ) ;
#69604 = NEXT_ASSEMBLY_USAGE_OCCURRENCE ( 'NAUO33', ' ', ' ', #2684, #56848, $ ) ;
#69605 = NEXT_ASSEMBLY_USAGE_OCCURRENCE ( 'NAUO34', ' ', ' ', #2684, #56848, $ ) ;
#69606 = NEXT_ASSEMBLY_USAGE_OCCURRENCE ( 'NAUO35', ' ', ' ', #2684, #54682, $ ) ;
#69607 = NEXT_ASSEMBLY_USAGE_OCCURRENCE ( 'NAUO36', ' ', ' ', #2684, #13877, $ ) ;
#69608 = NEXT_ASSEMBLY_USAGE_OCCURRENCE ( 'NAUO37', ' ', ' ', #2684, #58568, $ ) ;
#69609 = NEXT_ASSEMBLY_USAGE_OCCURRENCE ( 'NAUO38', ' ', ' ', #2684, #16010, $ ) ;
#69610 = NEXT_ASSEMBLY_USAGE_OCCURRENCE ( 'NAUO39', ' ', ' ', #2684, #16010, $ ) ;
#69611 = NEXT_ASSEMBLY_USAGE_OCCURRENCE ( 'NAUO40', ' ', ' ', #2684, #8730, $ ) ;
#69612 = NEXT_ASSEMBLY_USAGE_OCCURRENCE ( 'NAUO41', ' ', ' ', #2684, #8730, $ ) ;
#69613 = NEXT_ASSEMBLY_USAGE_OCCURRENCE ( 'NAUO42', ' ', ' ', #2684, #8730, $ ) ;
#69614 = NEXT_ASSEMBLY_USAGE_OCCURRENCE ( 'NAUO43', ' ', ' ', #2684, #8730, $ ) ;
#69615 = NEXT_ASSEMBLY_USAGE_OCCURRENCE ( 'NAUO44', ' ', ' ', #2684, #67192, $ ) ;
#69616 = NEXT_ASSEMBLY_USAGE_OCCURRENCE ( 'NAUO45', ' ', ' ', #2684, #67192, $ ) ;
#69617 = NEXT_ASSEMBLY_USAGE_OCCURRENCE ( 'NAUO46', ' ', ' ', #2684, #67192, $ ) ;
#69618 = NEXT_ASSEMBLY_USAGE_OCCURRENCE ( 'NAUO47', ' ', ' ', #2684, #67192, $ ) ;
#69619 = NEXT_ASSEMBLY_USAGE_OCCURRENCE ( 'NAUO48', ' ', ' ', #2684, #67192, $ ) ;
#69620 = NEXT_ASSEMBLY_USAGE_OCCURRENCE ( 'NAUO49', ' ', ' ', #2684, #67192, $ ) ;
#69621 = NEXT_ASSEMBLY_USAGE_OCCURRENCE ( 'NAUO50', ' ', ' ', #2684, #67192, $ ) ;
#69622 = NEXT_ASSEMBLY_USAGE_OCCURRENCE ( 'NAUO51', ' ', ' ', #2684, #67192, $ ) ;
#69623 = NEXT_ASSEMBLY_USAGE_OCCURRENCE ( 'NAUO52', ' ', ' ', #2684, #67192, $ ) ;
#69624 = NEXT_ASSEMBLY_USAGE_OCCURRENCE ( 'NAUO53', ' ', ' ', #2684, #67192, $ ) ;
#69625 = NEXT_ASSEMBLY_USAGE_OCCURRENCE ( 'NAUO54', ' ', ' ', #2684, #67192, $ ) ;
#69626 = NEXT_ASSEMBLY_USAGE_OCCURRENCE ( 'NAUO55', ' ', ' ', #2684, #67192, $ ) ;
#69627 = NEXT_ASSEMBLY_USAGE_OCCURRENCE ( 'NAUO56', ' ', ' ', #2684, #67192, $ ) ;
#69628 = NEXT_ASSEMBLY_USAGE_OCCURRENCE ( 'NAUO57', ' ', ' ', #2684, #67192, $ ) ;
#69629 = NEXT_ASSEMBLY_USAGE_OCCURRENCE ( 'NAUO58', ' ', ' ', #2684, #67192, $ ) ;
#69630 = NEXT_ASSEMBLY_USAGE_OCCURRENCE ( 'NAUO59', ' ', ' ', #2684, #67192, $ ) ;
#69631 = NEXT_ASSEMBLY_USAGE_OCCURRENCE ( 'NAUO60', ' ', ' ', #2684, #65913, $ ) ;
#69632 = NEXT_ASSEMBLY_USAGE_OCCURRENCE ( 'NAUO61', ' ', ' ', #23342, #16408, $ ) ;
#69633 = NEXT_ASSEMBLY_USAGE_OCCURRENCE ( 'NAUO62', ' ', ' ', #23342, #39219, $ ) ;
#69634 = NEXT_ASSEMBLY_USAGE_OCCURRENCE ( 'NAUO63', ' ', ' ', #23342, #53790, $ ) ;
#69635 = NEXT_ASSEMBLY_USAGE_OCCURRENCE ( 'NAUO64', ' ', ' ', #23342, #45241, $ ) ;
#69636 = NEXT_ASSEMBLY_USAGE_OCCURRENCE ( 'NAUO65', ' ', ' ', #23342, #43080, $ ) ;
#69637 = NEXT_ASSEMBLY_USAGE_OCCURRENCE ( 'NAUO66', ' ', ' ', #23342, #55565, $ ) ;
ENDSEC;
END-ISO-10303-21;
